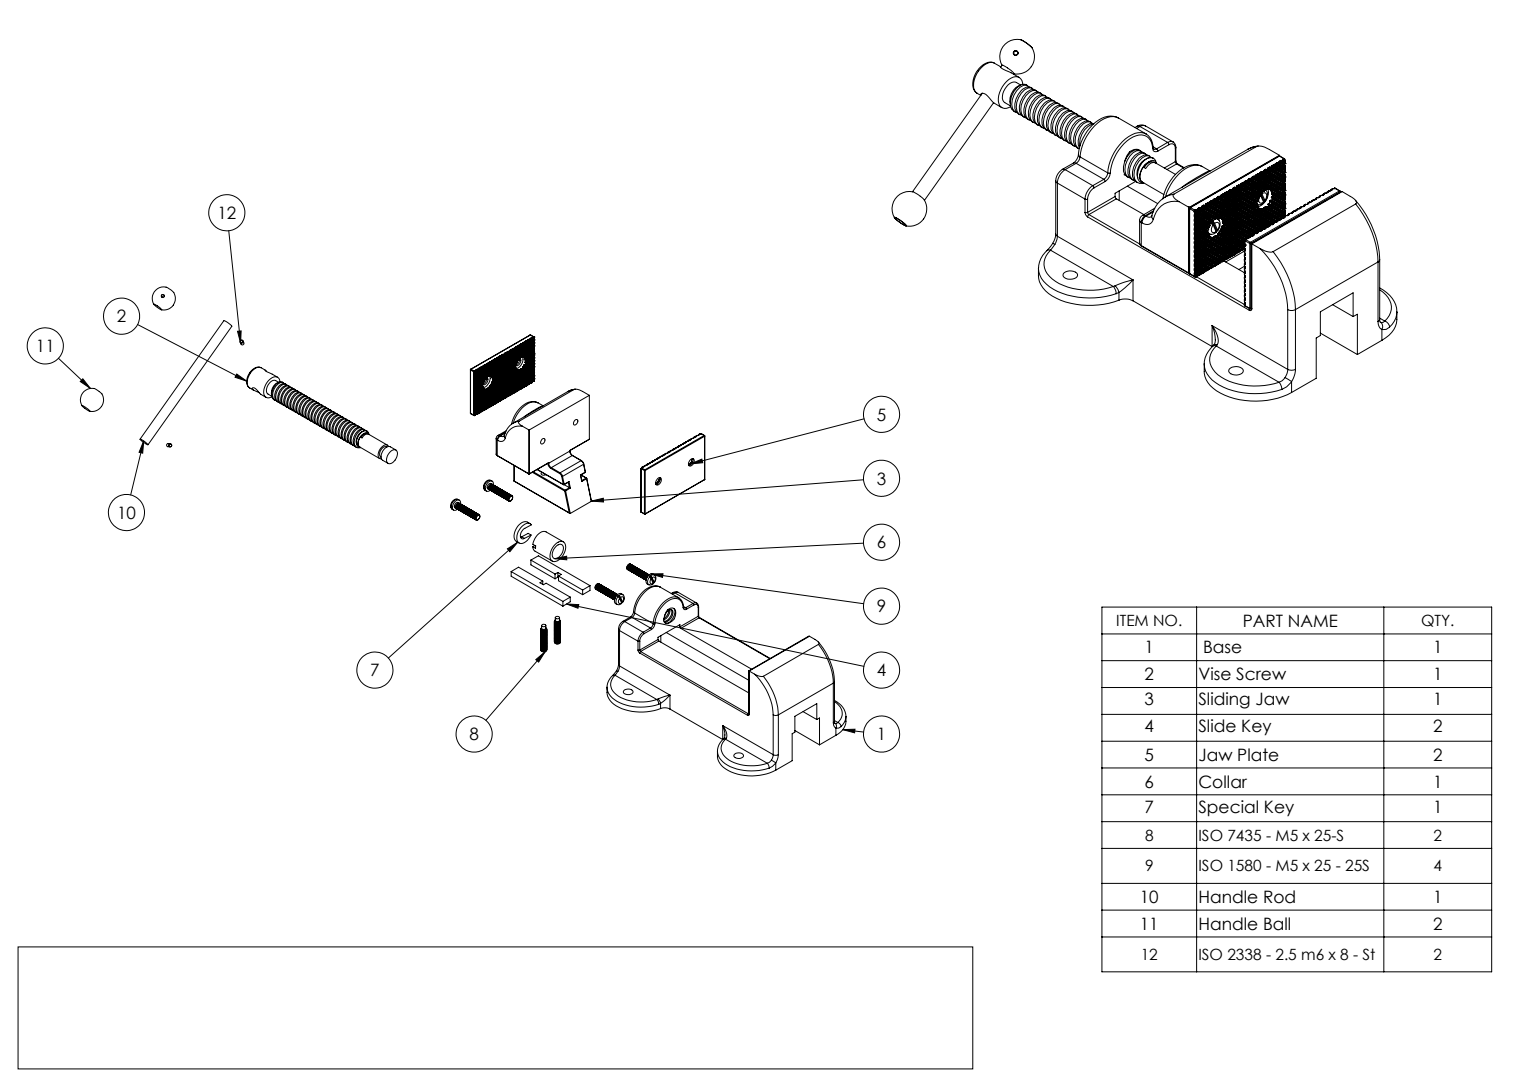
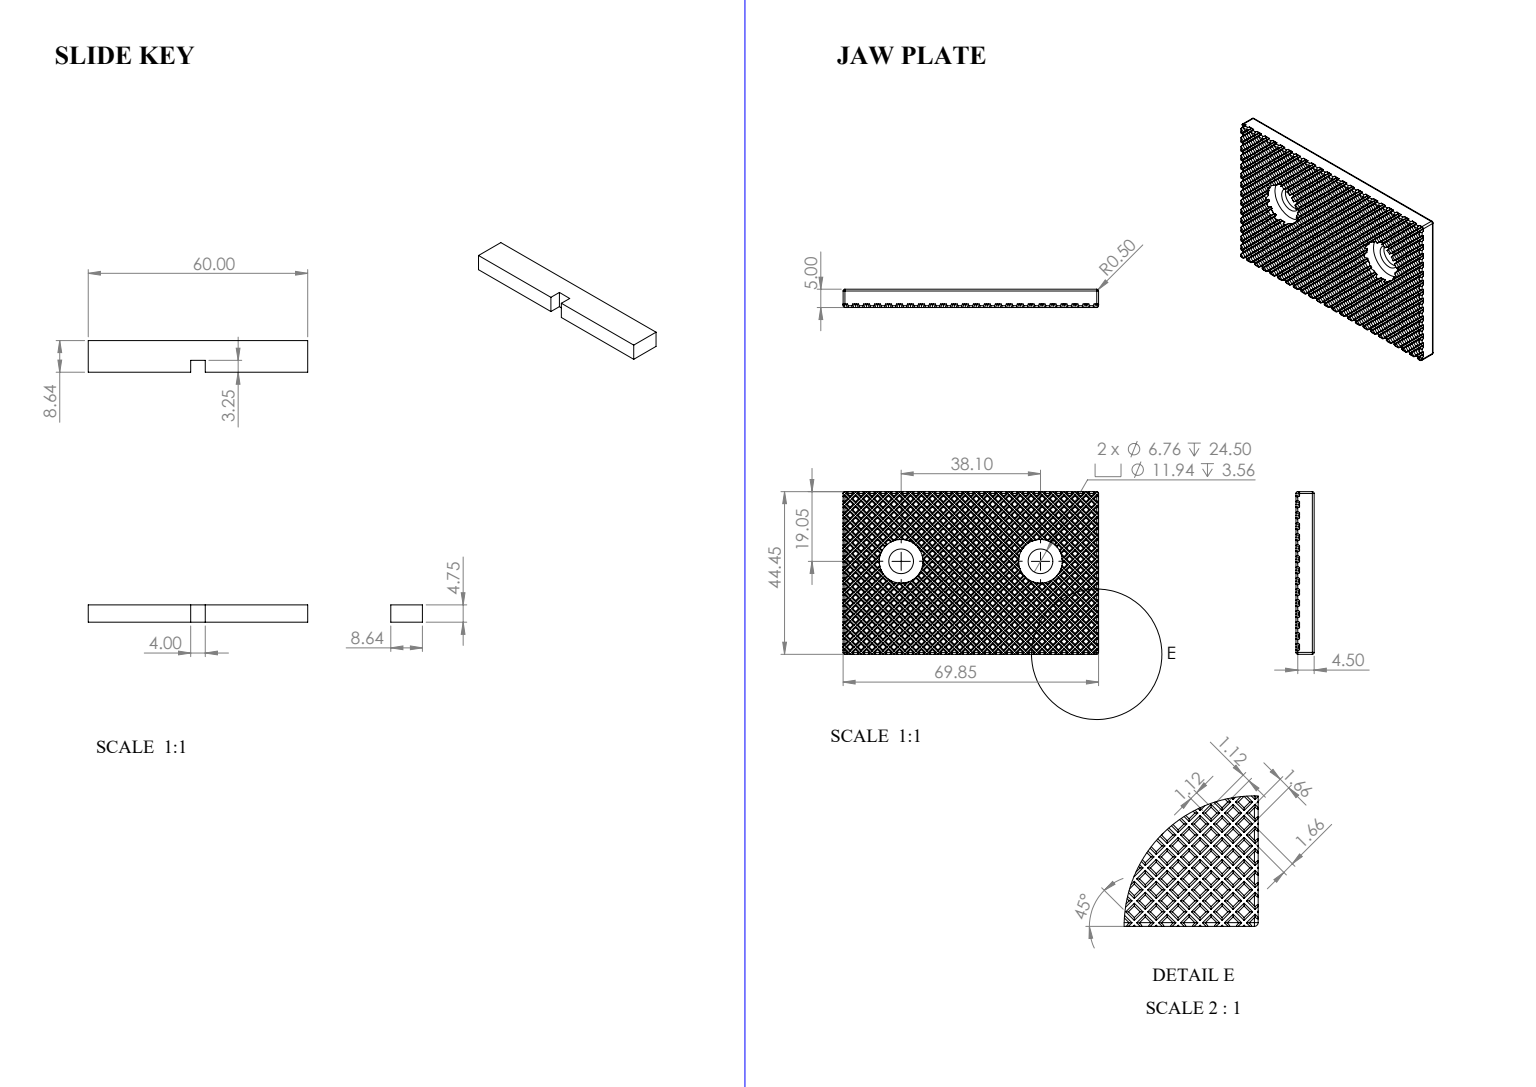
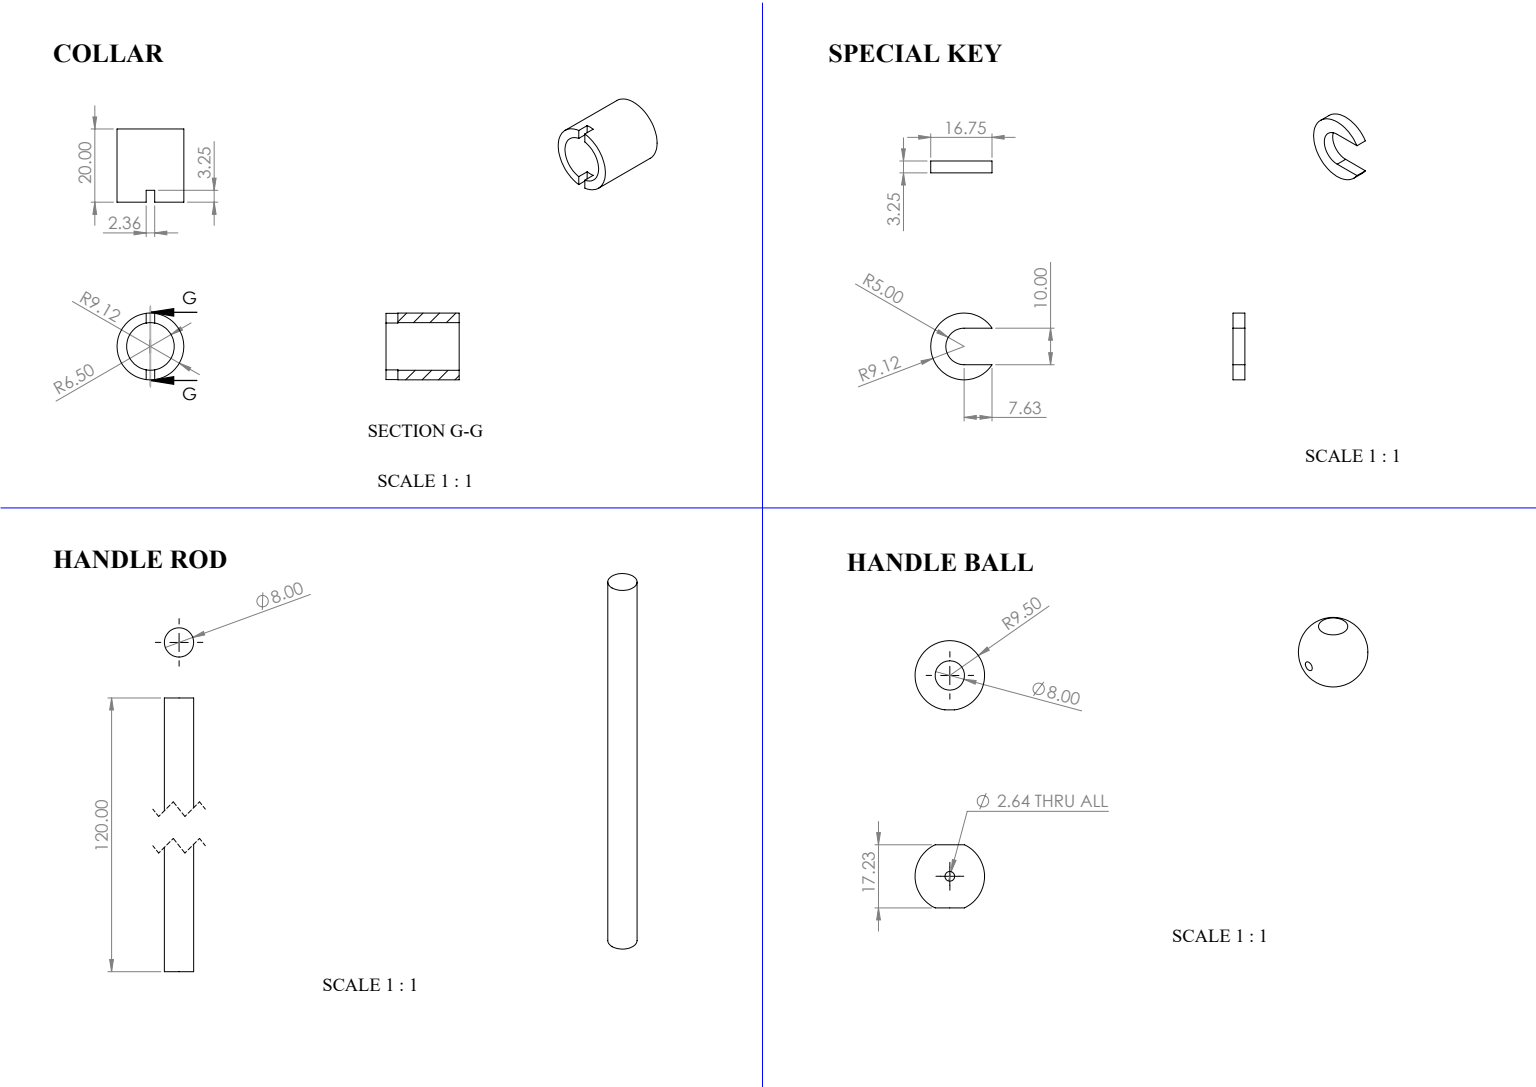
ISO-10303-21;
HEADER;
FILE_DESCRIPTION (('STEP AP214'),
    '1' );
FILE_NAME ('MAS-695',
    '2026-10-06T08:51:13',
    ( '' ),
    ( '' ),
    'SwSTEP 2.0',
    'SolidWorks 2021',
    '' );
FILE_SCHEMA (( 'AUTOMOTIVE_DESIGN' ));
ENDSEC;

DATA;
#1 = DIRECTION ( 'NONE',  ( 0.000000000000000000, 0.000000000000000000, 1.000000000000000000 ) ) ;
#2 = DIRECTION ( 'NONE',  ( 0.000000000000000000, 0.000000000000000000, -1.000000000000000000 ) ) ;
#3 = ADVANCED_FACE ( 'NONE', ( #5101 ), #71138, .F. ) ;
#4 = CARTESIAN_POINT ( 'NONE',  ( 156.1499999999997783, -49.14999999999999147, -40.92499999999998295 ) ) ;
#5 = VECTOR ( 'NONE', #78980, 1000.000000000000227 ) ;
#6 = CARTESIAN_POINT ( 'NONE',  ( 116.7245968585647660, -1.637169565754160949, 6.109999999999997655 ) ) ;
#7 = ORIENTED_EDGE ( 'NONE', *, *, #104399, .F. ) ;
#8 = EDGE_LOOP ( 'NONE', ( #83544, #1856, #131189, #37000 ) ) ;
#9 = FACE_OUTER_BOUND ( 'NONE', #81012, .T. ) ;
#10 = VECTOR ( 'NONE', #93764, 1000.000000000000000 ) ;
#11 = AXIS2_PLACEMENT_3D ( 'NONE', #21199, #109633, #54568 ) ;
#12 = VECTOR ( 'NONE', #112321, 1000.000000000000000 ) ;
#13 =( BOUNDED_CURVE ( )  B_SPLINE_CURVE ( 3, ( #128504, #27742, #103166, #38633 ),
 .UNSPECIFIED., .F., .T. ) 
 B_SPLINE_CURVE_WITH_KNOTS ( ( 4, 4 ),
 ( 5.143245962375963209, 6.645403452391246191 ),
 .UNSPECIFIED. ) 
 CURVE ( )  GEOMETRIC_REPRESENTATION_ITEM ( )  RATIONAL_B_SPLINE_CURVE ( ( 1.000000000000000000, 0.8206354192515237234, 0.8206354192515237234, 1.000000000000000000 ) ) 
 REPRESENTATION_ITEM ( '' )  );
#14 = COLOUR_RGB ( '', 0.08235294, 0.09019608, 0.10196078) ;
#15 = ORIENTED_EDGE ( 'NONE', *, *, #47014, .F. ) ;
#16 = VERTEX_POINT ( 'NONE', #58144 ) ;
#17 = CARTESIAN_POINT ( 'NONE',  ( 37.77126352523144703, 4.472830434245839371, 4.472830434245842035 ) ) ;
#18 = ORIENTED_EDGE ( 'NONE', *, *, #122540, .F. ) ;
#19 = CARTESIAN_POINT ( 'NONE',  ( -20.20710678118640402, -14.24070752338413826, 5.000000000000000000 ) ) ;
#20 = DIRECTION ( 'NONE',  ( -1.000000000000000000, -0.000000000000000000, -0.000000000000000000 ) ) ;
#21 = CYLINDRICAL_SURFACE ( 'NONE', #62371, 5.999999999999998224 ) ;
#22 = AXIS2_PLACEMENT_3D ( 'NONE', #116807, #105905, #95043 ) ;
#23 = CARTESIAN_POINT ( 'NONE',  ( 26.89126352523144092, -4.472830434245839371, -4.472830434245839371 ) ) ;
#24 = ORIENTED_EDGE ( 'NONE', *, *, #19090, .F. ) ;
#25 = LINE ( 'NONE', #44323, #82672 ) ;
#26 = ORIENTED_EDGE ( 'NONE', *, *, #3909, .F. ) ;
#27 = ORIENTED_EDGE ( 'NONE', *, *, #125600, .F. ) ;
#28 = AXIS2_PLACEMENT_3D ( 'NONE', #83260, #28167, #72429 ) ;
#29 = ORIENTED_EDGE ( 'NONE', *, *, #119403, .F. ) ;
#30 = VECTOR ( 'NONE', #87246, 1000.000000000000000 ) ;
#32 = PLANE ( 'NONE',  #68433 ) ;
#31 = VECTOR ( 'NONE', #125646, 1000.000000000000227 ) ;
#33 = CARTESIAN_POINT ( 'NONE',  ( -1.180000000000000604, 10.00000000000000178, 6.750000000000000888 ) ) ;
#34 = ORIENTED_EDGE ( 'NONE', *, *, #95665, .T. ) ;
#35 = FACE_OUTER_BOUND ( 'NONE', #136835, .T. ) ;
#36 = LINE ( 'NONE', #90690, #18133 ) ;
#37 = PLANE ( 'NONE',  #65195 ) ;
#38 = ADVANCED_FACE ( 'NONE', ( #115284 ), #3675, .F. ) ;
#39 = FACE_BOUND ( 'NONE', #50173, .T. ) ;
#40 = ORIENTED_EDGE ( 'NONE', *, *, #20313, .F. ) ;
#41 = CARTESIAN_POINT ( 'NONE',  ( -29.99451991528749417, 28.92564299267958816, 4.000000000000000000 ) ) ;
#42 = EDGE_CURVE ( 'NONE', #25059, #21205, #27594, .T. ) ;
#43 = EDGE_CURVE ( 'NONE', #65963, #18880, #92855, .T. ) ;
#44 = AXIS2_PLACEMENT_3D ( 'NONE', #3347, #93234, #125883 ) ;
#45 = DIRECTION ( 'NONE',  ( 0.3543493200069162685, -0.000000000000000000, -0.9351131265310288487 ) ) ;
#46 = DIRECTION ( 'NONE',  ( 1.000000000000000000, 0.000000000000000000, -0.000000000000000000 ) ) ;
#47 = ORIENTED_EDGE ( 'NONE', *, *, #35015, .F. ) ;
#48 = LINE ( 'NONE', #77678, #78225 ) ;
#49 = EDGE_LOOP ( 'NONE', ( #96646, #108093, #78224, #23588 ) ) ;
#50 = ORIENTED_EDGE ( 'NONE', *, *, #36159, .F. ) ;
#51 = LINE ( 'NONE', #32014, #142062 ) ;
#52 = ORIENTED_EDGE ( 'NONE', *, *, #60548, .T. ) ;
#53 = EDGE_CURVE ( 'NONE', #25081, #19559, #82032, .T. ) ;
#54 = EDGE_CURVE ( 'NONE', #25745, #125467, #104441, .T. ) ;
#55 = CARTESIAN_POINT ( 'NONE',  ( 47.30793019189811588, -6.109999999999998543, 1.637169565754158507 ) ) ;
#56 = ORIENTED_EDGE ( 'NONE', *, *, #91353, .F. ) ;
#57 = AXIS2_PLACEMENT_3D ( 'NONE', #43785, #22010, #66260 ) ;
#58 = DIRECTION ( 'NONE',  ( -0.7071067811865486830, -0.7071067811865464625, 0.000000000000000000 ) ) ;
#59 = CARTESIAN_POINT ( 'NONE',  ( -12.69999999999999929, -60.26999999999998892, -39.50000000000000000 ) ) ;
#60 = ADVANCED_FACE ( 'NONE', ( #80585 ), #50094, .F. ) ;
#61 = CARTESIAN_POINT ( 'NONE',  ( 68.99451991528748351, 28.92564299267986172, 4.000000000000000000 ) ) ;
#62 = EDGE_LOOP ( 'NONE', ( #94258, #115607, #50312, #53192 ) ) ;
#64 = CARTESIAN_POINT ( 'NONE',  ( 34.92499999999998295, -21.72500000000000142, 5.000000000000000000 ) ) ;
#63 = AXIS2_PLACEMENT_3D ( 'NONE', #104309, #85415, #117326 ) ;
#65 = EDGE_CURVE ( 'NONE', #58716, #118828, #49403, .T. ) ;
#66 = FILL_AREA_STYLE ('',( #56690 ) ) ;
#67 = DIRECTION ( 'NONE',  ( -0.7071067811865486830, -0.7071067811865464625, 0.000000000000000000 ) ) ;
#68 = DIRECTION ( 'NONE',  ( 0.000000000000000000, 0.000000000000000000, 1.000000000000000000 ) ) ;
#69 = LINE ( 'NONE', #66808, #128074 ) ;
#70 = DIRECTION ( 'NONE',  ( -0.7071067811865486830, -0.7071067811865464625, 0.000000000000000000 ) ) ;
#71 = ORIENTED_EDGE ( 'NONE', *, *, #64035, .T. ) ;
#72 = ORIENTED_EDGE ( 'NONE', *, *, #68229, .T. ) ;
#73 = VECTOR ( 'NONE', #82018, 1000.000000000000114 ) ;
#74 = EDGE_LOOP ( 'NONE', ( #63334, #111913, #607, #124092 ) ) ;
#75 = FACE_OUTER_BOUND ( 'NONE', #77019, .T. ) ;
#76 = EDGE_CURVE ( 'NONE', #54574, #78177, #14595, .T. ) ;
#77 = DIRECTION ( 'NONE',  ( 0.3543493200069162685, -0.000000000000000000, -0.9351131265310288487 ) ) ;
#78 = ORIENTED_EDGE ( 'NONE', *, *, #62615, .T. ) ;
#79 = ORIENTED_EDGE ( 'NONE', *, *, #43969, .T. ) ;
#80 = CARTESIAN_POINT ( 'NONE',  ( 166.6274442290528555, 26.96999999999994202, -32.76433874914447131 ) ) ;
#81 = DIRECTION ( 'NONE',  ( 1.000000000000000000, 0.000000000000000000, 0.000000000000000000 ) ) ;
#82 = CARTESIAN_POINT ( 'NONE',  ( 0.000000000000000000, 0.000000000000000000, 5.000000000000000000 ) ) ;
#83 = ORIENTED_EDGE ( 'NONE', *, *, #34651, .F. ) ;
#84 = DIRECTION ( 'NONE',  ( 0.3543493200069162685, -0.000000000000000000, -0.9351131265310288487 ) ) ;
#85 = EDGE_CURVE ( 'NONE', #114150, #6491, #116025, .T. ) ;
#86 = VECTOR ( 'NONE', #59606, 1000.000000000000000 ) ;
#87 = CARTESIAN_POINT ( 'NONE',  ( -9.489213562373095101, -27.52281430457062328, 5.000000000000000000 ) ) ;
#88 = CARTESIAN_POINT ( 'NONE',  ( 23.54623647476855552, -7.934999999999990727, 4.858786175617117713E-16 ) ) ;
#89 = CARTESIAN_POINT ( 'NONE',  ( 14.99999999999989519, -2.904428200921294057, -6.989807076074975534 ) ) ;
#90 = ORIENTED_EDGE ( 'NONE', *, *, #118546, .F. ) ;
#91 = CARTESIAN_POINT ( 'NONE',  ( 109.2870968585647944, 3.054999999999997939, 5.291415217122920289 ) ) ;
#92 = CARTESIAN_POINT ( 'NONE',  ( -19.83905809817562016, 22.22500000000000142, 10.71662732872346169 ) ) ;
#93 = EDGE_CURVE ( 'NONE', #95062, #84583, #91456, .T. ) ;
#94 = DIRECTION ( 'NONE',  ( -0.6830127018922180770, -0.6830127018922204085, -0.2588190451025213501 ) ) ;
#96 = ORIENTED_EDGE ( 'NONE', *, *, #90476, .F. ) ;
#95 = CARTESIAN_POINT ( 'NONE',  ( 20.99999999999985079, 12.25461709320622639, -10.07315571508692464 ) ) ;
#97 = DIRECTION ( 'NONE',  ( -0.000000000000000000, 0.000000000000000000, 1.000000000000000000 ) ) ;
#98 = ORIENTED_EDGE ( 'NONE', *, *, #70389, .T. ) ;
#99 = DIRECTION ( 'NONE',  ( -0.7071067811865486830, 0.7071067811865464625, 0.000000000000000000 ) ) ;
#100 = VECTOR ( 'NONE', #124280, 1000.000000000000000 ) ;
#101 = CARTESIAN_POINT ( 'NONE',  ( 3.489213562373097322, -27.52281430457057709, 5.000000000000000000 ) ) ;
#102 = DIRECTION ( 'NONE',  ( 1.201410254241279878E-16, -1.000000000000000000, 8.881784197001252323E-16 ) ) ;
#103 = ORIENTED_EDGE ( 'NONE', *, *, #12795, .T. ) ;
#104 = ADVANCED_FACE ( 'NONE', ( #137820 ), #15976, .T. ) ;
#105 = VECTOR ( 'NONE', #70002, 1000.000000000000227 ) ;
#106 = EDGE_CURVE ( 'NONE', #132598, #105272, #69721, .T. ) ;
#107 = LINE ( 'NONE', #77033, #97406 ) ;
#108 = DIRECTION ( 'NONE',  ( -1.000000000000000000, -1.224606353822377258E-16, -0.000000000000000000 ) ) ;
#109 = ORIENTED_EDGE ( 'NONE', *, *, #66738, .T. ) ;
#110 = AXIS2_PLACEMENT_3D ( 'NONE', #91463, #135678, #48666 ) ;
#111 = VECTOR ( 'NONE', #117132, 999.9999999999998863 ) ;
#112 = MECHANICAL_DESIGN_GEOMETRIC_PRESENTATION_REPRESENTATION (  '', ( #37206 ), #67225 ) ;
#113 = DIRECTION ( 'NONE',  ( -0.7071067811865487940, 0.7071067811865463515, -0.000000000000000000 ) ) ;
#114 = VECTOR ( 'NONE', #50874, 1000.000000000000000 ) ;
#116 = EDGE_CURVE ( 'NONE', #31169, #8752, #138521, .T. ) ;
#115 = LINE ( 'NONE', #86474, #33098 ) ;
#118 = EDGE_LOOP ( 'NONE', ( #114372, #70505, #8992, #113022 ) ) ;
#117 = VECTOR ( 'NONE', #30072, 1000.000000000000000 ) ;
#119 = LINE ( 'NONE', #77741, #60053 ) ;
#121 = VERTEX_POINT ( 'NONE', #68996 ) ;
#120 = DIRECTION ( 'NONE',  ( 0.6830127018922180770, -0.6830127018922204085, -0.2588190451025213501 ) ) ;
#122 = ORIENTED_EDGE ( 'NONE', *, *, #95989, .T. ) ;
#123 = CARTESIAN_POINT ( 'NONE',  ( -13.10742158956126424, 3.736470153597435395, 4.109745541549492565 ) ) ;
#124 = AXIS2_PLACEMENT_3D ( 'NONE', #74766, #9441, #75464 ) ;
#125 = ORIENTED_EDGE ( 'NONE', *, *, #121353, .T. ) ;
#126 = CARTESIAN_POINT ( 'NONE',  ( 25.49999999999982592, -19.53360074219753884, 5.000000000000000000 ) ) ;
#127 = DIRECTION ( 'NONE',  ( -0.7071067811865486830, -0.7071067811865464625, 0.000000000000000000 ) ) ;
#128 = DIRECTION ( 'NONE',  ( -0.7071067811865486830, 0.7071067811865464625, 0.000000000000000000 ) ) ;
#129 = ORIENTED_EDGE ( 'NONE', *, *, #131844, .F. ) ;
#130 = EDGE_CURVE ( 'NONE', #6161, #1058, #58874, .T. ) ;
#131 = LINE ( 'NONE', #142993, #129973 ) ;
#132 = LINE ( 'NONE', #67611, #18945 ) ;
#133 = LINE ( 'NONE', #13167, #47104 ) ;
#134 = AXIS2_PLACEMENT_3D ( 'NONE', #6194, #104832, #5501 ) ;
#135 = LINE ( 'NONE', #42284, #50624 ) ;
#136 = CARTESIAN_POINT ( 'NONE',  ( 29.66209685856477307, -5.291415217122919401, 3.054999999999998384 ) ) ;
#137 = CARTESIAN_POINT ( 'NONE',  ( 2.999999999999988898, 2.966399257802230682, 5.000000000000000000 ) ) ;
#138 = VECTOR ( 'NONE', #55015, 1000.000000000000000 ) ;
#139 = ORIENTED_EDGE ( 'NONE', *, *, #36771, .T. ) ;
#140 = ORIENTED_EDGE ( 'NONE', *, *, #3276, .F. ) ;
#141 =( NAMED_UNIT ( * ) SI_UNIT ( $, .STERADIAN. ) SOLID_ANGLE_UNIT ( ) );
#142 = VECTOR ( 'NONE', #39114, 999.9999999999998863 ) ;
#143 = ORIENTED_EDGE ( 'NONE', *, *, #47317, .T. ) ;
#144 = VECTOR ( 'NONE', #74034, 999.9999999999998863 ) ;
#145 = EDGE_LOOP ( 'NONE', ( #119724, #61454, #57894, #85195 ) ) ;
#146 = CARTESIAN_POINT ( 'NONE',  ( -5.708222910169487463, -15.74070752338411694, 19.73771281079096340 ) ) ;
#147 = DIRECTION ( 'NONE',  ( -0.7071067811865486830, -0.7071067811865464625, 0.000000000000000000 ) ) ;
#148 = VECTOR ( 'NONE', #138557, 1000.000000000000000 ) ;
#149 = ORIENTED_EDGE ( 'NONE', *, *, #38243, .F. ) ;
#150 = DIRECTION ( 'NONE',  ( 0.000000000000000000, -0.9647414015272155474, 0.2631995976047525887 ) ) ;
#151 = FACE_OUTER_BOUND ( 'NONE', #122556, .T. ) ;
#152 = CARTESIAN_POINT ( 'NONE',  ( -7.499999999999947597, -4.796895815301026822, -3.611700055028700174 ) ) ;
#153 = ADVANCED_FACE ( 'NONE', ( #103035 ), #103710, .F. ) ;
#154 = CARTESIAN_POINT ( 'NONE',  ( -12.18398860626900060, 28.73617430169795739, 5.000000000000000000 ) ) ;
#155 = CARTESIAN_POINT ( 'NONE',  ( 124.5420968585647756, 5.291415217122923842, -3.054999999999996163 ) ) ;
#156 = AXIS2_PLACEMENT_3D ( 'NONE', #125719, #134450, #3870 ) ;
#157 = ORIENTED_EDGE ( 'NONE', *, *, #128606, .T. ) ;
#158 = CARTESIAN_POINT ( 'NONE',  ( 5.207106781186502609, -17.24070752338410983, 5.000000000000000000 ) ) ;
#159 = DIRECTION ( 'NONE',  ( 0.7071067811865487940, -0.7071067811865463515, 0.000000000000000000 ) ) ;
#160 = FACE_OUTER_BOUND ( 'NONE', #79460, .T. ) ;
#161 =( NAMED_UNIT ( * ) PLANE_ANGLE_UNIT ( ) SI_UNIT ( $, .RADIAN. ) );
#162 = PLANE ( 'NONE',  #130794 ) ;
#163 = CARTESIAN_POINT ( 'NONE',  ( 19.49999999999985789, 8.319652575858395238, -8.582050562765779489 ) ) ;
#164 = FACE_OUTER_BOUND ( 'NONE', #130185, .T. ) ;
#165 = CARTESIAN_POINT ( 'NONE',  ( 54.62086038379622721, -6.884901960086286188, 3.974999999999997424 ) ) ;
#166 = DIRECTION ( 'NONE',  ( 0.6830127018922181881, 0.6830127018922202975, -0.2588190451025214056 ) ) ;
#167 = EDGE_CURVE ( 'NONE', #60255, #130315, #34540, .T. ) ;
#168 = DIRECTION ( 'NONE',  ( 0.7071067811865486830, -0.7071067811865464625, -0.000000000000000000 ) ) ;
#169 = AXIS2_PLACEMENT_3D ( 'NONE', #60485, #124990, #72084 ) ;
#170 = ORIENTED_EDGE ( 'NONE', *, *, #86072, .F. ) ;
#171 = ORIENTED_EDGE ( 'NONE', *, *, #96108, .T. ) ;
#172 = CARTESIAN_POINT ( 'NONE',  ( 48.25000000000000000, -9.735942053221458872E-16, 7.950000000000000178 ) ) ;
#173 = DIRECTION ( 'NONE',  ( -0.7071067811865486830, -0.7071067811865464625, 0.000000000000000000 ) ) ;
#174 = CARTESIAN_POINT ( 'NONE',  ( 53.99451991528749062, 28.92564299267975869, 4.000000000000000000 ) ) ;
#175 = ORIENTED_EDGE ( 'NONE', *, *, #80806, .F. ) ;
#176 = DIRECTION ( 'NONE',  ( 0.7071067811865487940, 0.7071067811865463515, 0.000000000000000000 ) ) ;
#177 = EDGE_CURVE ( 'NONE', #92630, #88659, #70457, .T. ) ;
#178 = LINE ( 'NONE', #43032, #32998 ) ;
#179 = EDGE_CURVE ( 'NONE', #63680, #108628, #141365, .T. ) ;
#180 = CARTESIAN_POINT ( 'NONE',  ( 41.27126352523144703, 4.472830434245839371, 4.472830434245842035 ) ) ;
#181 = ORIENTED_EDGE ( 'NONE', *, *, #134281, .T. ) ;
#182 = CARTESIAN_POINT ( 'NONE',  ( 0.1600000000000011136, 3.289720434613005118, -7.220939306079887210 ) ) ;
#183 = ORIENTED_EDGE ( 'NONE', *, *, #91628, .T. ) ;
#184 = ORIENTED_EDGE ( 'NONE', *, *, #140711, .F. ) ;
#185 = VECTOR ( 'NONE', #101958, 1000.000000000000227 ) ;
#186 = DIRECTION ( 'NONE',  ( 0.9961946980917455452, 0.000000000000000000, -0.08715574274765836016 ) ) ;
#187 = DIRECTION ( 'NONE',  ( 0.6830127018922181881, 0.6830127018922202975, -0.2588190451025214056 ) ) ;
#188 = CARTESIAN_POINT ( 'NONE',  ( -12.29974487139158512, -27.71228299555214747, 4.000000000000000000 ) ) ;
#189 = PLANE ( 'NONE',  #18575 ) ;
#190 = EDGE_LOOP ( 'NONE', ( #15272, #100026, #80901, #142923 ) ) ;
#191 = EDGE_CURVE ( 'NONE', #72974, #90074, #61695, .T. ) ;
#192 = DIRECTION ( 'NONE',  ( -0.7071067811865487940, 0.7071067811865463515, 0.000000000000000000 ) ) ;
#193 = ORIENTED_EDGE ( 'NONE', *, *, #9062, .T. ) ;
#194 = CARTESIAN_POINT ( 'NONE',  ( 82.25043019189810423, 3.055000000000002824, -5.291415217122919401 ) ) ;
#195 = FACE_OUTER_BOUND ( 'NONE', #108561, .T. ) ;
#196 =( LENGTH_UNIT ( ) NAMED_UNIT ( * ) SI_UNIT ( .MILLI., .METRE. ) );
#197 = CARTESIAN_POINT ( 'NONE',  ( -34.92500000000001137, 6.856123077392376253, 4.000000000000000000 ) ) ;
#198 = PLANE ( 'NONE',  #64849 ) ;
#199 = VECTOR ( 'NONE', #98975, 1000.000000000000000 ) ;
#200 = DIRECTION ( 'NONE',  ( 1.000000000000000000, 0.000000000000000000, 0.000000000000000000 ) ) ;
#201 = ORIENTED_EDGE ( 'NONE', *, *, #80508, .F. ) ;
#202 = DIRECTION ( 'NONE',  ( -0.7071067811865486830, -0.7071067811865464625, -0.000000000000000000 ) ) ;
#203 = CARTESIAN_POINT ( 'NONE',  ( 53.43293019189810167, 1.637169565754156508, 6.110000000000000320 ) ) ;
#204 = FACE_OUTER_BOUND ( 'NONE', #73708, .T. ) ;
#205 = DIRECTION ( 'NONE',  ( 0.7071067811865486830, -0.7071067811865464625, -0.000000000000000000 ) ) ;
#206 = DIRECTION ( 'NONE',  ( -0.000000000000000000, -0.000000000000000000, 1.000000000000000000 ) ) ;
#207 = ORIENTED_EDGE ( 'NONE', *, *, #61881, .T. ) ;
#208 = EDGE_LOOP ( 'NONE', ( #82343, #5888, #63190, #69675 ) ) ;
#209 = FACE_OUTER_BOUND ( 'NONE', #9634, .T. ) ;
#210 = AXIS2_PLACEMENT_3D ( 'NONE', #18854, #51517, #105848 ) ;
#211 = ORIENTED_EDGE ( 'NONE', *, *, #117503, .T. ) ;
#212 = VECTOR ( 'NONE', #88205, 1000.000000000000000 ) ;
#213 = AXIS2_PLACEMENT_3D ( 'NONE', #103469, #123843, #48393 ) ;
#214 = CARTESIAN_POINT ( 'NONE',  ( 0.000000000000000000, 0.000000000000000000, 5.000000000000000000 ) ) ;
#215 = ORIENTED_EDGE ( 'NONE', *, *, #26545, .F. ) ;
#216 = CARTESIAN_POINT ( 'NONE',  ( 12.48921356237309155, -27.52281430457064104, 5.000000000000000000 ) ) ;
#217 = CARTESIAN_POINT ( 'NONE',  ( 29.99999999999979039, -10.77435723561692704, -9.972017380717296930 ) ) ;
#218 = VECTOR ( 'NONE', #139975, 1000.000000000000000 ) ;
#219 = VECTOR ( 'NONE', #138745, 1000.000000000000000 ) ;
#220 = AXIS2_PLACEMENT_3D ( 'NONE', #21758, #55108, #75432 ) ;
#221 = AXIS2_PLACEMENT_3D ( 'NONE', #111679, #101498, #113810 ) ;
#222 = EDGE_CURVE ( 'NONE', #139983, #86102, #20281, .T. ) ;
#223 = AXIS2_PLACEMENT_3D ( 'NONE', #89988, #15261, #133521 ) ;
#224 = FACE_OUTER_BOUND ( 'NONE', #124706, .T. ) ;
#225 = FACE_BOUND ( 'NONE', #102384, .T. ) ;
#226 = ADVANCED_FACE ( 'NONE', ( #51523 ), #94983, .F. ) ;
#227 = CARTESIAN_POINT ( 'NONE',  ( 28.49999999999980460, 16.77039438581781639, 0.4657186855307072215 ) ) ;
#228 = LINE ( 'NONE', #88730, #91900 ) ;
#230 = DIRECTION ( 'NONE',  ( -0.7071067811865486830, -0.7071067811865464625, 0.000000000000000000 ) ) ;
#229 = AXIS2_PLACEMENT_3D ( 'NONE', #59966, #127341, #70166 ) ;
#232 = ORIENTED_EDGE ( 'NONE', *, *, #94046, .F. ) ;
#231 = CARTESIAN_POINT ( 'NONE',  ( 5.343289998337836799, 3.759292476615681888, 13.27625715073266832 ) ) ;
#233 = DIRECTION ( 'NONE',  ( 0.7071067811865487940, -0.7071067811865463515, 0.000000000000000000 ) ) ;
#234 = EDGE_LOOP ( 'NONE', ( #55561, #105143, #26118, #111519 ) ) ;
#235 = EDGE_CURVE ( 'NONE', #55527, #138159, #86292, .T. ) ;
#236 = EDGE_CURVE ( 'NONE', #105061, #6978, #28339, .T. ) ;
#237 = VERTEX_POINT ( 'NONE', #52898 ) ;
#238 = CARTESIAN_POINT ( 'NONE',  ( 79.97459685856478018, 1.637169565754164280, -6.109999999999996767 ) ) ;
#239 = ORIENTED_EDGE ( 'NONE', *, *, #100908, .T. ) ;
#240 = CARTESIAN_POINT ( 'NONE',  ( -34.92500000000001137, -22.22500000000000142, 4.000000000000000000 ) ) ;
#241 = EDGE_CURVE ( 'NONE', #93680, #60629, #40644, .T. ) ;
#242 = VECTOR ( 'NONE', #139566, 1000.000000000000000 ) ;
#243 = CARTESIAN_POINT ( 'NONE',  ( -14.99999999999990230, 11.58746187583913390, 4.000000000000000000 ) ) ;
#244 = B_SPLINE_CURVE_WITH_KNOTS ( 'NONE', 3,
 ( #116047, #19597, #116769, #42097, #141380, #17451, #127667, #74728, #105869, #52917, #50814, #86307 ),
 .UNSPECIFIED., .F., .F.,
 ( 4, 2, 2, 2, 2, 4 ),
 ( 9.813815432834144085E-18, 0.001837441947543535809, 0.003674883895087062077, 0.004593604868858823694, 0.005512325842630587044, 0.007349767790174136298 ),
 .UNSPECIFIED. ) ;
#245 = EDGE_CURVE ( 'NONE', #60766, #87872, #129054, .T. ) ;
#246 = ORIENTED_EDGE ( 'NONE', *, *, #38962, .T. ) ;
#247 = CARTESIAN_POINT ( 'NONE',  ( -57.29974487139158157, -27.71228299555246011, 4.000000000000000000 ) ) ;
#248 = ADVANCED_FACE ( 'NONE', ( #84846 ), #37182, .F. ) ;
#249 = VECTOR ( 'NONE', #124185, 999.9999999999998863 ) ;
#250 = LINE ( 'NONE', #99570, #21719 ) ;
#251 = FACE_OUTER_BOUND ( 'NONE', #30396, .T. ) ;
#252 = EDGE_CURVE ( 'NONE', #89926, #37388, #72601, .T. ) ;
#253 = AXIS2_PLACEMENT_3D ( 'NONE', #31106, #7884, #115919 ) ;
#254 = CARTESIAN_POINT ( 'NONE',  ( 0.000000000000000000, 0.000000000000000000, 5.000000000000000000 ) ) ;
#255 = DIRECTION ( 'NONE',  ( -0.3543493200069163240, 0.000000000000000000, 0.9351131265310288487 ) ) ;
#256 = DIRECTION ( 'NONE',  ( 0.7071067811865487940, -0.7071067811865463515, 0.000000000000000000 ) ) ;
#257 = AXIS2_PLACEMENT_3D ( 'NONE', #43444, #11484, #76815 ) ;
#258 = CARTESIAN_POINT ( 'NONE',  ( -11.51078643762690490, -27.52281430457047406, 5.000000000000000000 ) ) ;
#259 = DIRECTION ( 'NONE',  ( 0.000000000000000000, -1.000000000000000000, 0.000000000000000000 ) ) ;
#260 = ORIENTED_EDGE ( 'NONE', *, *, #110078, .F. ) ;
#261 = PRESENTATION_STYLE_ASSIGNMENT (( #47937 ) ) ;
#262 = ORIENTED_EDGE ( 'NONE', *, *, #76274, .T. ) ;
#263 = VECTOR ( 'NONE', #104295, 1000.000000000000000 ) ;
#264 = CARTESIAN_POINT ( 'NONE',  ( 14.20710678118644665, 6.759292476615645029, 5.000000000000000000 ) ) ;
#265 = EDGE_CURVE ( 'NONE', #60839, #128811, #85538, .T. ) ;
#266 = ORIENTED_EDGE ( 'NONE', *, *, #113885, .F. ) ;
#267 = ORIENTED_EDGE ( 'NONE', *, *, #56927, .F. ) ;
#268 = VECTOR ( 'NONE', #71889, 999.9999999999998863 ) ;
#269 = CARTESIAN_POINT ( 'NONE',  ( 28.58376352523143993, -6.110000000000001208, -3.741295971395164515E-16 ) ) ;
#270 = VERTEX_POINT ( 'NONE', #52214 ) ;
#271 = ADVANCED_FACE ( 'NONE', ( #128367 ), #102071, .T. ) ;
#272 = CARTESIAN_POINT ( 'NONE',  ( 18.32816939922340183, -6.740707523384209310, 4.000000000000000000 ) ) ;
#273 = AXIS2_PLACEMENT_3D ( 'NONE', #107756, #108445, #21491 ) ;
#274 = CARTESIAN_POINT ( 'NONE',  ( -0.2245968585647807325, -2.126176841940958351, -7.934999999999989839 ) ) ;
#275 = CARTESIAN_POINT ( 'NONE',  ( -23.51078643762690490, -27.52281430457038880, 5.000000000000000000 ) ) ;
#276 = ORIENTED_EDGE ( 'NONE', *, *, #16957, .T. ) ;
#277 = LINE ( 'NONE', #122073, #61918 ) ;
#278 = ORIENTED_EDGE ( 'NONE', *, *, #76259, .F. ) ;
#279 = DIRECTION ( 'NONE',  ( -0.000000000000000000, -0.3543493200069152693, 0.9351131265310292928 ) ) ;
#280 = DIRECTION ( 'NONE',  ( -0.6830127018922180770, -0.6830127018922204085, -0.2588190451025213501 ) ) ;
#282 = EDGE_LOOP ( 'NONE', ( #75330, #107556, #58149, #92149 ) ) ;
#281 = DIRECTION ( 'NONE',  ( 0.7071067811865486830, -0.7071067811865464625, -0.000000000000000000 ) ) ;
#283 = VECTOR ( 'NONE', #27809, 1000.000000000000000 ) ;
#284 = ORIENTED_EDGE ( 'NONE', *, *, #109477, .T. ) ;
#285 = FACE_OUTER_BOUND ( 'NONE', #1360, .T. ) ;
#286 = LINE ( 'NONE', #34381, #116352 ) ;
#287 = CARTESIAN_POINT ( 'NONE',  ( 1.171830600776462061, -20.24070752338407786, 4.000000000000000000 ) ) ;
#288 = VERTEX_POINT ( 'NONE', #119584 ) ;
#289 = CARTESIAN_POINT ( 'NONE',  ( -72.48921356237309510, -27.52281430457106026, 5.000000000000000000 ) ) ;
#290 = DIRECTION ( 'NONE',  ( -0.6830127018922180770, -0.6830127018922204085, -0.2588190451025213501 ) ) ;
#291 = ORIENTED_EDGE ( 'NONE', *, *, #84770, .T. ) ;
#292 = VECTOR ( 'NONE', #30348, 1000.000000000000000 ) ;
#293 = EDGE_CURVE ( 'NONE', #72640, #57817, #29041, .T. ) ;
#294 = LINE ( 'NONE', #88788, #58847 ) ;
#295 = LINE ( 'NONE', #101775, #132017 ) ;
#296 = CARTESIAN_POINT ( 'NONE',  ( -15.48921356237309510, -27.52281430457066236, 5.000000000000000000 ) ) ;
#297 = AXIS2_PLACEMENT_3D ( 'NONE', #93929, #83070, #52567 ) ;
#298 = DIRECTION ( 'NONE',  ( -1.000000000000000000, -1.224606353822377258E-16, -0.000000000000000000 ) ) ;
#299 = EDGE_CURVE ( 'NONE', #18521, #55587, #117446, .T. ) ;
#300 = DIRECTION ( 'NONE',  ( -1.000000000000000000, -1.224606353822377258E-16, -0.000000000000000000 ) ) ;
#301 = FACE_OUTER_BOUND ( 'NONE', #7948, .T. ) ;
#302 = LINE ( 'NONE', #112664, #34486 ) ;
#303 = ORIENTED_EDGE ( 'NONE', *, *, #124962, .T. ) ;
#304 = CARTESIAN_POINT ( 'NONE',  ( 97.49586038379624142, -3.974999999999998312, -6.884901960086286188 ) ) ;
#305 = VERTEX_POINT ( 'NONE', #7974 ) ;
#306 = VECTOR ( 'NONE', #44663, 1000.000000000000114 ) ;
#307 = SURFACE_SIDE_STYLE ('',( #35140 ) ) ;
#308 = CARTESIAN_POINT ( 'NONE',  ( 0.000000000000000000, 0.000000000000000000, 7.950000000000000178 ) ) ;
#309 = EDGE_CURVE ( 'NONE', #55336, #42777, #64521, .T. ) ;
#310 = LINE ( 'NONE', #120669, #138798 ) ;
#311 = ORIENTED_EDGE ( 'NONE', *, *, #103224, .T. ) ;
#312 = PLANE ( 'NONE',  #122563 ) ;
#313 = DIRECTION ( 'NONE',  ( -0.3543493200069162685, -0.000000000000000000, -0.9351131265310288487 ) ) ;
#314 = CARTESIAN_POINT ( 'NONE',  ( -21.70710678118638981, 11.25929247661560773, 5.000000000000000000 ) ) ;
#315 = ORIENTED_EDGE ( 'NONE', *, *, #1789, .F. ) ;
#316 = EDGE_CURVE ( 'NONE', #33411, #102047, #58129, .T. ) ;
#317 = LINE ( 'NONE', #143165, #97408 ) ;
#318 = LINE ( 'NONE', #11922, #100246 ) ;
#319 = CARTESIAN_POINT ( 'NONE',  ( 12.48921356237309155, -27.52281430457064104, 5.000000000000000000 ) ) ;
#320 = AXIS2_PLACEMENT_3D ( 'NONE', #30283, #118710, #19405 ) ;
#321 = DIRECTION ( 'NONE',  ( 0.7071067811865486830, -0.7071067811865464625, -0.000000000000000000 ) ) ;
#322 = CARTESIAN_POINT ( 'NONE',  ( 56.34959685856478018, 6.109999999999997655, 1.637169565754163836 ) ) ;
#323 = CARTESIAN_POINT ( 'NONE',  ( 60.48921356237309510, -27.52281430457097500, 5.000000000000000000 ) ) ;
#324 = VECTOR ( 'NONE', #96544, 1000.000000000000000 ) ;
#325 =( BOUNDED_CURVE ( )  B_SPLINE_CURVE ( 3, ( #134781, #78969, #34023, #14395 ),
 .UNSPECIFIED., .F., .T. ) 
 B_SPLINE_CURVE_WITH_KNOTS ( ( 4, 4 ),
 ( 4.350170835173023498, 4.500739107949261353 ),
 .UNSPECIFIED. ) 
 CURVE ( )  GEOMETRIC_REPRESENTATION_ITEM ( )  RATIONAL_B_SPLINE_CURVE ( ( 1.000000000000000000, 0.9981116584018945304, 0.9981116584018945304, 1.000000000000000000 ) ) 
 REPRESENTATION_ITEM ( '' )  );
#326 = AXIS2_PLACEMENT_3D ( 'NONE', #113465, #122938, #69282 ) ;
#327 = DIRECTION ( 'NONE',  ( -1.000000000000000000, -2.891205793294679312E-16, 0.000000000000000000 ) ) ;
#328 = CARTESIAN_POINT ( 'NONE',  ( 32.30836038379622721, 7.949999999999996625, 2.130196079827431088 ) ) ;
#329 = CARTESIAN_POINT ( 'NONE',  ( 83.68750000000000000, -5.819803920172573974, 5.819803920172573086 ) ) ;
#330 = VERTEX_POINT ( 'NONE', #9384 ) ;
#331 =( LENGTH_UNIT ( ) NAMED_UNIT ( * ) SI_UNIT ( .MILLI., .METRE. ) );
#332 = VERTEX_POINT ( 'NONE', #53661 ) ;
#333 = VECTOR ( 'NONE', #70121, 1000.000000000000000 ) ;
#334 = VECTOR ( 'NONE', #77445, 1000.000000000000000 ) ;
#335 = CIRCLE ( 'NONE', #118423, 2.256103126841972895 ) ;
#336 = CARTESIAN_POINT ( 'NONE',  ( 8.816011393731004731, 28.73617430169781173, 5.000000000000000000 ) ) ;
#338 = PLANE ( 'NONE',  #138048 ) ;
#337 = AXIS2_PLACEMENT_3D ( 'NONE', #92579, #128791, #104900 ) ;
#339 = AXIS2_PLACEMENT_3D ( 'NONE', #38488, #104434, #126890 ) ;
#340 = FACE_OUTER_BOUND ( 'NONE', #82107, .T. ) ;
#341 = PLANE ( 'NONE',  #25712 ) ;
#342 = PLANE ( 'NONE',  #141146 ) ;
#343 = EDGE_CURVE ( 'NONE', #92701, #118319, #97869, .T. ) ;
#344 = CARTESIAN_POINT ( 'NONE',  ( -34.42500000000001137, 13.54139925780187603, 5.000000000000000000 ) ) ;
#345 = CARTESIAN_POINT ( 'NONE',  ( -34.42500000000001137, 0.000000000000000000, 4.500000000000000888 ) ) ;
#346 = EDGE_CURVE ( 'NONE', #132444, #99209, #109450, .T. ) ;
#347 = ORIENTED_EDGE ( 'NONE', *, *, #6469, .T. ) ;
#348 = ORIENTED_EDGE ( 'NONE', *, *, #75130, .F. ) ;
#349 = FACE_OUTER_BOUND ( 'NONE', #74753, .T. ) ;
#350 = FACE_OUTER_BOUND ( 'NONE', #24729, .T. ) ;
#351 = VECTOR ( 'NONE', #98125, 1000.000000000000000 ) ;
#352 = CARTESIAN_POINT ( 'NONE',  ( -24.18398860626899705, 28.73617430169804265, 5.000000000000000000 ) ) ;
#353 = DIRECTION ( 'NONE',  ( -0.6830127018922181881, 0.6830127018922202975, -0.2588190451025214056 ) ) ;
#354 = CARTESIAN_POINT ( 'NONE',  ( 81.45419371712955581, 6.884901960086283523, 3.975000000000002753 ) ) ;
#355 = CARTESIAN_POINT ( 'NONE',  ( -11.29289321881337571, 17.25929247661553489, 5.000000000000000000 ) ) ;
#356 = ADVANCED_FACE ( 'NONE', ( #123207 ), #110146, .T. ) ;
#357 = DIRECTION ( 'NONE',  ( -1.000000000000000000, -1.224606353822377258E-16, -0.000000000000000000 ) ) ;
#358 = VERTEX_POINT ( 'NONE', #56560 ) ;
#359 = CARTESIAN_POINT ( 'NONE',  ( 73.62500000000000000, -7.950000000000000178, -4.867971026610729436E-16 ) ) ;
#360 = VECTOR ( 'NONE', #90136, 1000.000000000000000 ) ;
#361 = CARTESIAN_POINT ( 'NONE',  ( 5.999999999999960032, 18.08204922493374411, 0.9627537363044759156 ) ) ;
#362 = DIRECTION ( 'NONE',  ( 0.7071067811865487940, 0.7071067811865463515, 0.000000000000000000 ) ) ;
#363 = ORIENTED_EDGE ( 'NONE', *, *, #24956, .F. ) ;
#364 = EDGE_CURVE ( 'NONE', #108536, #57879, #101424, .T. ) ;
#365 = MECHANICAL_DESIGN_GEOMETRIC_PRESENTATION_REPRESENTATION (  '', ( #53591 ), #69867 ) ;
#366 = DIRECTION ( 'NONE',  ( -0.7071067811865487940, 0.7071067811865463515, -0.000000000000000000 ) ) ;
#367 = ORIENTED_EDGE ( 'NONE', *, *, #20533, .T. ) ;
#368 = AXIS2_PLACEMENT_3D ( 'NONE', #120768, #21477, #143248 ) ;
#369 = EDGE_CURVE ( 'NONE', #137573, #138987, #81190, .T. ) ;
#370 = DIRECTION ( 'NONE',  ( 0.000000000000000000, 0.000000000000000000, 1.000000000000000000 ) ) ;
#371 = CARTESIAN_POINT ( 'NONE',  ( 62.12543019189810423, 5.291415217122919401, 3.055000000000002824 ) ) ;
#372 = CARTESIAN_POINT ( 'NONE',  ( 24.39999999999999858, -5.520864266206504263E-14, 0.000000000000000000 ) ) ;
#373 = VERTEX_POINT ( 'NONE', #76859 ) ;
#374 = VECTOR ( 'NONE', #35742, 1000.000000000000000 ) ;
#375 = CARTESIAN_POINT ( 'NONE',  ( -24.32816939922336275, 14.25929247661557575, 4.000000000000000000 ) ) ;
#376 = DIRECTION ( 'NONE',  ( -0.7071067811865486830, -0.7071067811865464625, 0.000000000000000000 ) ) ;
#377 = SURFACE_STYLE_USAGE ( .BOTH. , #24296 ) ;
#378 = CARTESIAN_POINT ( 'NONE',  ( 0.3281693992235297785, 17.25929247661554200, 4.000000000000000000 ) ) ;
#379 = EDGE_CURVE ( 'NONE', #60214, #42523, #120557, .T. ) ;
#380 = CARTESIAN_POINT ( 'NONE',  ( 10.37159235450332062, -3.851859888774471706E-31, 2.500000000000001332 ) ) ;
#382 = ORIENTED_EDGE ( 'NONE', *, *, #28958, .T. ) ;
#381 = CARTESIAN_POINT ( 'NONE',  ( -2.999999999999975131, -6.033600742197674727, 5.000000000000000000 ) ) ;
#383 = CARTESIAN_POINT ( 'NONE',  ( -2.999999999999976463, -1.068876922607804314, 4.000000000000000000 ) ) ;
#384 = CARTESIAN_POINT ( 'NONE',  ( 2.218373117075048029, 21.74787736706806385, 4.999607392498048419 ) ) ;
#385 = CARTESIAN_POINT ( 'NONE',  ( -23.99451991528749062, 28.92564299267954908, 4.000000000000000000 ) ) ;
#386 = AXIS2_PLACEMENT_3D ( 'NONE', #58460, #98177, #96016 ) ;
#387 =( NAMED_UNIT ( * ) SI_UNIT ( $, .STERADIAN. ) SOLID_ANGLE_UNIT ( ) );
#388 = ORIENTED_EDGE ( 'NONE', *, *, #12820, .F. ) ;
#389 = ORIENTED_EDGE ( 'NONE', *, *, #16681, .T. ) ;
#390 = CARTESIAN_POINT ( 'NONE',  ( 65.91709685856477563, 3.054999999999998828, 5.291415217122922066 ) ) ;
#391 = VERTEX_POINT ( 'NONE', #65987 ) ;
#392 = CARTESIAN_POINT ( 'NONE',  ( -34.92500000000001137, 22.22500000000000142, 4.000000000000000000 ) ) ;
#393 = CARTESIAN_POINT ( 'NONE',  ( -26.29289321881326558, -9.740707523384184441, 5.000000000000000000 ) ) ;
#394 = DIRECTION ( 'NONE',  ( 0.7071067811865487940, 0.7071067811865463515, 0.000000000000000000 ) ) ;
#395 = VECTOR ( 'NONE', #66581, 1000.000000000000114 ) ;
#396 = CARTESIAN_POINT ( 'NONE',  ( -24.98480450340313652, 2.536990198832462351, 5.000000000000000000 ) ) ;
#397 = CARTESIAN_POINT ( 'NONE',  ( 17.29289321881334018, -6.740707523384209310, 5.000000000000000000 ) ) ;
#398 = VERTEX_POINT ( 'NONE', #23880 ) ;
#399 = ORIENTED_EDGE ( 'NONE', *, *, #4654, .T. ) ;
#400 = VECTOR ( 'NONE', #70487, 1000.000000000000000 ) ;
#401 = DIRECTION ( 'NONE',  ( -0.7071067811865486830, -0.7071067811865464625, 0.000000000000000000 ) ) ;
#402 = CARTESIAN_POINT ( 'NONE',  ( -16.92402963342697220, -0.5732982342275830812, -34.79992920313960525 ) ) ;
#403 = ORIENTED_EDGE ( 'NONE', *, *, #107919, .F. ) ;
#404 = LINE ( 'NONE', #133118, #125414 ) ;
#405 = EDGE_CURVE ( 'NONE', #121029, #128151, #88328, .T. ) ;
#406 = FACE_OUTER_BOUND ( 'NONE', #46336, .T. ) ;
#407 = FACE_OUTER_BOUND ( 'NONE', #98667, .T. ) ;
#408 = AXIS2_PLACEMENT_3D ( 'NONE', #118351, #30665, #74896 ) ;
#409 = ORIENTED_EDGE ( 'NONE', *, *, #43363, .T. ) ;
#410 = FACE_BOUND ( 'NONE', #51809, .T. ) ;
#411 = CARTESIAN_POINT ( 'NONE',  ( -3.005480084712505828, 28.92564299267936079, 4.000000000000000000 ) ) ;
#412 = LINE ( 'NONE', #119338, #62884 ) ;
#413 = CARTESIAN_POINT ( 'NONE',  ( -18.29974487139159223, -27.71228299555219010, 4.000000000000000000 ) ) ;
#414 = CARTESIAN_POINT ( 'NONE',  ( -7.499999999999951150, 13.08746187583912146, 4.000000000000000000 ) ) ;
#415 = LINE ( 'NONE', #88909, #141470 ) ;
#416 = ORIENTED_EDGE ( 'NONE', *, *, #6486, .F. ) ;
#417 = EDGE_CURVE ( 'NONE', #27268, #65916, #67404, .T. ) ;
#418 = ORIENTED_EDGE ( 'NONE', *, *, #36030, .F. ) ;
#419 = CARTESIAN_POINT ( 'NONE',  ( 105.7870968585647802, 3.054999999999997495, 5.291415217122919401 ) ) ;
#420 = ORIENTED_EDGE ( 'NONE', *, *, #111228, .F. ) ;
#421 = EDGE_CURVE ( 'NONE', #133840, #42748, #31897, .T. ) ;
#422 = FILL_AREA_STYLE ('',( #141288 ) ) ;
#423 = ORIENTED_EDGE ( 'NONE', *, *, #120728, .F. ) ;
#424 = ADVANCED_FACE ( 'NONE', ( #143502 ), #11532, .F. ) ;
#425 = CARTESIAN_POINT ( 'NONE',  ( 9.707106781186480404, -0.7407075233842735917, 5.000000000000000000 ) ) ;
#426 = VECTOR ( 'NONE', #53827, 1000.000000000000000 ) ;
#427 = EDGE_CURVE ( 'NONE', #3647, #106547, #19837, .T. ) ;
#428 = SHAPE_REPRESENTATION ( 'slotted pan head screw_iso_ISO 1580 - M5 x 25 - 25S', ( #127880 ), #95551 ) ;
#429 = DIRECTION ( 'NONE',  ( -0.3543493200069162685, -0.000000000000000000, -0.9351131265310288487 ) ) ;
#430 = VECTOR ( 'NONE', #23278, 999.9999999999998863 ) ;
#431 = VECTOR ( 'NONE', #87814, 1000.000000000000000 ) ;
#432 = CARTESIAN_POINT ( 'NONE',  ( 39.29974487139159578, -27.71228299555233576, 4.000000000000000000 ) ) ;
#433 = EDGE_LOOP ( 'NONE', ( #100677, #114743, #113008 ) ) ;
#434 = DIRECTION ( 'NONE',  ( 0.7071067811865487940, 0.7071067811865463515, 0.000000000000000000 ) ) ;
#435 = DIRECTION ( 'NONE',  ( -0.7071067811865487940, 0.7071067811865463515, -0.000000000000000000 ) ) ;
#436 = CARTESIAN_POINT ( 'NONE',  ( 8.999999999999943157, 7.552185695429089130, 5.000000000000000000 ) ) ;
#437 = EDGE_CURVE ( 'NONE', #128814, #125503, #6074, .T. ) ;
#438 = LINE ( 'NONE', #139913, #105981 ) ;
#440 = CARTESIAN_POINT ( 'NONE',  ( 59.14169371712955581, -2.130196079827424871, -7.949999999999998401 ) ) ;
#439 = CARTESIAN_POINT ( 'NONE',  ( 54.03752705046288440, -9.735942053221456900E-16, 7.949999999999998401 ) ) ;
#441 = VECTOR ( 'NONE', #51936, 1000.000000000000000 ) ;
#442 = VECTOR ( 'NONE', #49067, 1000.000000000000000 ) ;
#443 = MECHANICAL_DESIGN_GEOMETRIC_PRESENTATION_REPRESENTATION (  '', ( #97739 ), #18987 ) ;
#444 = DIRECTION ( 'NONE',  ( 0.3543493200069162685, -0.000000000000000000, -0.9351131265310288487 ) ) ;
#445 = VERTEX_POINT ( 'NONE', #6784 ) ;
#446 = DIRECTION ( 'NONE',  ( 0.000000000000000000, 1.000000000000000000, 0.000000000000000000 ) ) ;
#447 = DIRECTION ( 'NONE',  ( 0.6830127018922180770, -0.6830127018922204085, -0.2588190451025213501 ) ) ;
#448 = EDGE_CURVE ( 'NONE', #139414, #35675, #74241, .T. ) ;
#449 = ORIENTED_EDGE ( 'NONE', *, *, #79627, .F. ) ;
#450 = EDGE_LOOP ( 'NONE', ( #37770, #449, #12481, #125 ) ) ;
#451 = EDGE_CURVE ( 'NONE', #68140, #73925, #41598, .T. ) ;
#452 = EDGE_LOOP ( 'NONE', ( #21111, #56741, #113242, #114759 ) ) ;
#453 = CARTESIAN_POINT ( 'NONE',  ( 53.81293019189810423, -1.637169565754159617, -6.110000000000001208 ) ) ;
#454 = EDGE_LOOP ( 'NONE', ( #116566, #36964, #17088, #40231, #105946, #55816 ) ) ;
#455 = EDGE_CURVE ( 'NONE', #121396, #35500, #128617, .T. ) ;
#456 = PLANE ( 'NONE',  #41905 ) ;
#457 = CARTESIAN_POINT ( 'NONE',  ( 1.504139616203772789, -3.047499999999994547, 5.278424836066145431 ) ) ;
#458 = CARTESIAN_POINT ( 'NONE',  ( 93.47959685856476142, 6.109999999999999432, 1.637169565754164280 ) ) ;
#459 = CYLINDRICAL_SURFACE ( 'NONE', #21662, 0.5000000000000004441 ) ;
#460 = ORIENTED_EDGE ( 'NONE', *, *, #37283, .F. ) ;
#461 = DIRECTION ( 'NONE',  ( -0.000000000000000000, -0.3543493200069152693, 0.9351131265310292928 ) ) ;
#462 = LINE ( 'NONE', #141906, #37760 ) ;
#463 = ORIENTED_EDGE ( 'NONE', *, *, #82126, .T. ) ;
#464 = DIRECTION ( 'NONE',  ( -1.000000000000000000, -1.224606353822377258E-16, -0.000000000000000000 ) ) ;
#465 = AXIS2_PLACEMENT_3D ( 'NONE', #68774, #78939, #1320 ) ;
#466 = PLANE ( 'NONE',  #66047 ) ;
#467 = VERTEX_POINT ( 'NONE', #51789 ) ;
#468 = AXIS2_PLACEMENT_3D ( 'NONE', #89931, #34153, #23234 ) ;
#469 = DIRECTION ( 'NONE',  ( 1.000000000000000000, 0.000000000000000000, 0.000000000000000000 ) ) ;
#470 = DIRECTION ( 'NONE',  ( -0.7071067811865486830, 0.7071067811865464625, 0.000000000000000000 ) ) ;
#471 = ORIENTED_EDGE ( 'NONE', *, *, #95394, .T. ) ;
#472 = AXIS2_PLACEMENT_3D ( 'NONE', #141340, #42773, #52189 ) ;
#473 = ORIENTED_EDGE ( 'NONE', *, *, #137601, .F. ) ;
#474 = VERTEX_POINT ( 'NONE', #29291 ) ;
#475 = EDGE_CURVE ( 'NONE', #12429, #109431, #7525, .T. ) ;
#476 = CARTESIAN_POINT ( 'NONE',  ( 121.2454301918981230, -5.291415217122918513, -3.055000000000000160 ) ) ;
#477 = VECTOR ( 'NONE', #71928, 1000.000000000000227 ) ;
#478 = LINE ( 'NONE', #33862, #127907 ) ;
#479 = CARTESIAN_POINT ( 'NONE',  ( 34.92499999999998295, 13.70193056682084887, 4.500000000000000888 ) ) ;
#480 = ORIENTED_EDGE ( 'NONE', *, *, #67194, .T. ) ;
#481 = CARTESIAN_POINT ( 'NONE',  ( -16.49999999999988276, -13.53360074219760101, 5.000000000000000000 ) ) ;
#482 = VERTEX_POINT ( 'NONE', #31451 ) ;
#483 = VECTOR ( 'NONE', #57375, 1000.000000000000227 ) ;
#484 = CARTESIAN_POINT ( 'NONE',  ( 10.33290314143522082, -3.967499999999994476, 6.871911579029513106 ) ) ;
#485 = PLANE ( 'NONE',  #101778 ) ;
#486 = DIRECTION ( 'NONE',  ( 0.000000000000000000, 0.000000000000000000, -1.000000000000000000 ) ) ;
#487 = CARTESIAN_POINT ( 'NONE',  ( -12.69999999999998153, -0.3999999999999997446, -2.467792535850613866 ) ) ;
#488 = VERTEX_POINT ( 'NONE', #75673 ) ;
#489 = VERTEX_POINT ( 'NONE', #100278 ) ;
#490 = ADVANCED_FACE ( 'NONE', ( #66231 ), #198, .F. ) ;
#491 = VECTOR ( 'NONE', #127188, 1000.000000000000000 ) ;
#492 = ORIENTED_EDGE ( 'NONE', *, *, #81875, .T. ) ;
#493 = PLANE ( 'NONE',  #37151 ) ;
#494 = CARTESIAN_POINT ( 'NONE',  ( 39.29974487139159578, -27.71228299555233576, 4.000000000000000000 ) ) ;
#495 = VECTOR ( 'NONE', #102903, 1000.000000000000114 ) ;
#496 = DIRECTION ( 'NONE',  ( -1.000000000000000000, 0.000000000000000000, -0.000000000000000000 ) ) ;
#497 = CARTESIAN_POINT ( 'NONE',  ( -23.99999999999983302, 16.93112307739201583, 4.000000000000000000 ) ) ;
#498 = CARTESIAN_POINT ( 'NONE',  ( -14.24890464969599435, -0.3792994071806680689, 4.162343009174984232 ) ) ;
#499 = DIRECTION ( 'NONE',  ( -0.3543493200069162685, -0.000000000000000000, -0.9351131265310288487 ) ) ;
#500 = EDGE_CURVE ( 'NONE', #83224, #56577, #120555, .T. ) ;
#501 = LINE ( 'NONE', #20833, #42091 ) ;
#502 = DIRECTION ( 'NONE',  ( -0.7071067811865486830, 0.7071067811865464625, 0.000000000000000000 ) ) ;
#503 = ORIENTED_EDGE ( 'NONE', *, *, #122198, .F. ) ;
#504 = CARTESIAN_POINT ( 'NONE',  ( -41.99451991528749062, 28.92564299267967343, 4.000000000000000000 ) ) ;
#505 = VECTOR ( 'NONE', #41332, 1000.000000000000000 ) ;
#506 = EDGE_LOOP ( 'NONE', ( #140030, #45972, #39854, #108702 ) ) ;
#507 = CARTESIAN_POINT ( 'NONE',  ( 57.18398860626899705, 28.73617430169827358, 5.000000000000000000 ) ) ;
#508 = ORIENTED_EDGE ( 'NONE', *, *, #48578, .F. ) ;
#509 = CARTESIAN_POINT ( 'NONE',  ( -48.48921356237309510, -27.52281430457089328, 5.000000000000000000 ) ) ;
#511 = ORIENTED_EDGE ( 'NONE', *, *, #137999, .F. ) ;
#510 = CARTESIAN_POINT ( 'NONE',  ( -48.48921356237309510, -27.52281430457089328, 5.000000000000000000 ) ) ;
#512 = EDGE_CURVE ( 'NONE', #80329, #53800, #11805, .T. ) ;
#513 = DIRECTION ( 'NONE',  ( -0.7071067811865487940, 0.7071067811865463515, -0.000000000000000000 ) ) ;
#514 = LINE ( 'NONE', #1914, #14794 ) ;
#515 = ORIENTED_EDGE ( 'NONE', *, *, #127473, .F. ) ;
#516 = CARTESIAN_POINT ( 'NONE',  ( -15.18398860626900237, 28.73617430169797871, 5.000000000000000000 ) ) ;
#518 = ORIENTED_EDGE ( 'NONE', *, *, #141850, .T. ) ;
#517 = AXIS2_PLACEMENT_3D ( 'NONE', #20502, #1596, #109680 ) ;
#519 = DIRECTION ( 'NONE',  ( -0.7071067811865487940, 0.7071067811865463515, -0.000000000000000000 ) ) ;
#520 = ORIENTED_EDGE ( 'NONE', *, *, #112530, .T. ) ;
#521 = LINE ( 'NONE', #89005, #45331 ) ;
#522 = CARTESIAN_POINT ( 'NONE',  ( 111.0583603837961988, -7.949999999999997513, -2.130196079827425759 ) ) ;
#523 = CARTESIAN_POINT ( 'NONE',  ( 0.000000000000000000, -40.42999999999999261, -39.50000000000000000 ) ) ;
#524 =( NAMED_UNIT ( * ) SI_UNIT ( $, .STERADIAN. ) SOLID_ANGLE_UNIT ( ) );
#525 = DIRECTION ( 'NONE',  ( 0.7071067811865487940, 0.7071067811865463515, 0.000000000000000000 ) ) ;
#526 = CARTESIAN_POINT ( 'NONE',  ( 13.92145407031093818, 4.584330080086930965E-16, 0.000000000000000000 ) ) ;
#527 = LINE ( 'NONE', #44069, #11340 ) ;
#528 = CARTESIAN_POINT ( 'NONE',  ( 18.22916666666666785, -6.094999999999989093, 1.633150327867691765 ) ) ;
#529 = DIRECTION ( 'NONE',  ( -0.7071067811865486830, -0.7071067811865464625, 0.000000000000000000 ) ) ;
#530 = VECTOR ( 'NONE', #99105, 999.9999999999998863 ) ;
#531 = VECTOR ( 'NONE', #90557, 1000.000000000000000 ) ;
#533 = CARTESIAN_POINT ( 'NONE',  ( 0.000000000000000000, 0.000000000000000000, 7.950000000000000178 ) ) ;
#532 = VECTOR ( 'NONE', #82631, 1000.000000000000000 ) ;
#534 = LINE ( 'NONE', #75981, #91767 ) ;
#535 = ORIENTED_EDGE ( 'NONE', *, *, #15196, .F. ) ;
#536 = VERTEX_POINT ( 'NONE', #86555 ) ;
#537 = AXIS2_PLACEMENT_3D ( 'NONE', #63476, #8301, #7604 ) ;
#538 = COLOUR_RGB ( '', 0.09019608, 0.27058824, 0.51372549) ;
#539 = CARTESIAN_POINT ( 'NONE',  ( 27.70710678118635073, -12.74070752338415424, 5.000000000000000000 ) ) ;
#540 = VERTEX_POINT ( 'NONE', #130787 ) ;
#541 = ADVANCED_FACE ( 'NONE', ( #99530 ), #56092, .F. ) ;
#542 = CARTESIAN_POINT ( 'NONE',  ( 106.7504301918981184, 3.055000000000002824, -5.291415217122919401 ) ) ;
#543 = LINE ( 'NONE', #123072, #77852 ) ;
#544 = LINE ( 'NONE', #44839, #9237 ) ;
#545 = AXIS2_PLACEMENT_3D ( 'NONE', #123467, #24124, #58230 ) ;
#547 = VECTOR ( 'NONE', #85064, 1000.000000000000000 ) ;
#546 = CARTESIAN_POINT ( 'NONE',  ( -34.49999999999975842, -7.535744391599424219, 4.994342998332167660 ) ) ;
#548 = CARTESIAN_POINT ( 'NONE',  ( 0.000000000000000000, 0.000000000000000000, 5.000000000000000000 ) ) ;
#549 = ORIENTED_EDGE ( 'NONE', *, *, #89231, .T. ) ;
#550 = LINE ( 'NONE', #133943, #31321 ) ;
#551 = DIRECTION ( 'NONE',  ( -0.5735764363510499342, -0.8191520442889891340, 0.000000000000000000 ) ) ;
#552 = CARTESIAN_POINT ( 'NONE',  ( 21.32816939922336985, -15.74070752338412760, 4.000000000000000000 ) ) ;
#553 = EDGE_CURVE ( 'NONE', #52608, #118518, #64800, .T. ) ;
#554 = CARTESIAN_POINT ( 'NONE',  ( 34.49999999999975131, 22.21934299833216642, 4.348028800457638177 ) ) ;
#555 = EDGE_CURVE ( 'NONE', #94937, #79882, #33614, .T. ) ;
#556 = CARTESIAN_POINT ( 'NONE',  ( -24.70710678118637205, 8.259292476615636147, 5.000000000000000000 ) ) ;
#558 = VERTEX_POINT ( 'NONE', #43749 ) ;
#557 = FACE_OUTER_BOUND ( 'NONE', #112855, .T. ) ;
#559 = CYLINDRICAL_SURFACE ( 'NONE', #125629, 9.119999999999999218 ) ;
#560 = CARTESIAN_POINT ( 'NONE',  ( 1.516262732464673579, 3.821174125832445049E-16, 0.000000000000000000 ) ) ;
#561 = SURFACE_STYLE_FILL_AREA ( #32509 ) ;
#562 = CARTESIAN_POINT ( 'NONE',  ( 47.99451991528749062, 28.92564299267971251, 4.000000000000000000 ) ) ;
#563 = CARTESIAN_POINT ( 'NONE',  ( 3.707106781186515487, -15.74070752338412404, 5.000000000000000000 ) ) ;
#564 = ORIENTED_EDGE ( 'NONE', *, *, #87957, .F. ) ;
#565 = ORIENTED_EDGE ( 'NONE', *, *, #54246, .F. ) ;
#566 = VERTEX_POINT ( 'NONE', #32907 ) ;
#567 = CARTESIAN_POINT ( 'NONE',  ( 94.50043019189810423, -3.055000000000002380, 5.291415217122920289 ) ) ;
#568 = ORIENTED_EDGE ( 'NONE', *, *, #120751, .T. ) ;
#569 = DIRECTION ( 'NONE',  ( 0.7071067811865487940, -0.7071067811865463515, 0.000000000000000000 ) ) ;
#570 = CARTESIAN_POINT ( 'NONE',  ( -12.69999999999998153, 0.000000000000000000, 0.000000000000000000 ) ) ;
#571 = CARTESIAN_POINT ( 'NONE',  ( -17.99451991528748351, 28.92564299267950645, 4.000000000000000000 ) ) ;
#572 = CARTESIAN_POINT ( 'NONE',  ( 0.000000000000000000, 0.000000000000000000, 5.000000000000000000 ) ) ;
#573 = ORIENTED_EDGE ( 'NONE', *, *, #143462, .T. ) ;
#574 = EDGE_CURVE ( 'NONE', #120024, #43089, #22666, .T. ) ;
#575 = CARTESIAN_POINT ( 'NONE',  ( 20.99999999999985079, -16.06887692260765377, 4.000000000000000000 ) ) ;
#576 = DIRECTION ( 'NONE',  ( -1.000000000000000000, 0.000000000000000000, -0.000000000000000000 ) ) ;
#577 = AXIS2_PLACEMENT_3D ( 'NONE', #85870, #75032, #8969 ) ;
#578 = CARTESIAN_POINT ( 'NONE',  ( 83.47459685856478018, 1.637169565754164058, -6.109999999999996767 ) ) ;
#579 = ORIENTED_EDGE ( 'NONE', *, *, #10590, .F. ) ;
#580 = VECTOR ( 'NONE', #117247, 1000.000000000000227 ) ;
#581 = LINE ( 'NONE', #108604, #83736 ) ;
#583 = VECTOR ( 'NONE', #73522, 1000.000000000000227 ) ;
#582 = PLANE ( 'NONE',  #88617 ) ;
#584 = AXIS2_PLACEMENT_3D ( 'NONE', #45025, #34830, #21796 ) ;
#585 = EDGE_LOOP ( 'NONE', ( #84587, #117927, #110585, #17558 ) ) ;
#586 = ORIENTED_EDGE ( 'NONE', *, *, #664, .T. ) ;
#587 = ORIENTED_EDGE ( 'NONE', *, *, #53900, .F. ) ;
#588 = FACE_OUTER_BOUND ( 'NONE', #75692, .T. ) ;
#589 = CARTESIAN_POINT ( 'NONE',  ( 5.700255128608413102, -27.71228299555201957, 4.000000000000000000 ) ) ;
#590 = CARTESIAN_POINT ( 'NONE',  ( 18.00456980810188767, 6.871911579029510442, -3.967499999999998916 ) ) ;
#591 = CARTESIAN_POINT ( 'NONE',  ( 6.066782984417857350, 2.500000000000000444, 0.000000000000000000 ) ) ;
#592 = CARTESIAN_POINT ( 'NONE',  ( 166.4267503027637929, 26.96999999999993847, 33.05223327726561422 ) ) ;
#593 = CARTESIAN_POINT ( 'NONE',  ( 26.99999999999980815, 10.21212019023811557, -2.019456568337861135 ) ) ;
#594 = EDGE_CURVE ( 'NONE', #43234, #102340, #12534, .T. ) ;
#595 = LINE ( 'NONE', #67318, #59027 ) ;
#596 = ADVANCED_FACE ( 'NONE', ( #108976 ), #23407, .F. ) ;
#597 = ORIENTED_EDGE ( 'NONE', *, *, #82825, .T. ) ;
#598 = ORIENTED_EDGE ( 'NONE', *, *, #22116, .T. ) ;
#599 = EDGE_CURVE ( 'NONE', #53838, #27206, #43053, .T. ) ;
#600 = CARTESIAN_POINT ( 'NONE',  ( -2.671830600776458287, 5.259292476615669010, 4.000000000000000000 ) ) ;
#601 = ORIENTED_EDGE ( 'NONE', *, *, #119460, .T. ) ;
#602 = ORIENTED_EDGE ( 'NONE', *, *, #80662, .F. ) ;
#603 = AXIS2_PLACEMENT_3D ( 'NONE', #111128, #114010, #68409 ) ;
#604 = EDGE_CURVE ( 'NONE', #29147, #103671, #114246, .T. ) ;
#605 = EDGE_CURVE ( 'NONE', #107763, #100224, #143057, .T. ) ;
#606 = CARTESIAN_POINT ( 'NONE',  ( -9.183988606268997046, 28.73617430169793607, 5.000000000000000000 ) ) ;
#607 = ORIENTED_EDGE ( 'NONE', *, *, #61214, .T. ) ;
#608 = CARTESIAN_POINT ( 'NONE',  ( -11.67183060077639212, -3.740707523384244837, 4.000000000000000000 ) ) ;
#609 = CARTESIAN_POINT ( 'NONE',  ( -4.110173228882081808, -22.22499999999999787, 4.785647885939356527 ) ) ;
#610 = CARTESIAN_POINT ( 'NONE',  ( 34.45011844616451668, -19.48371918836231131, 5.000000000000000888 ) ) ;
#611 = CARTESIAN_POINT ( 'NONE',  ( 0.000000000000000000, 0.000000000000000000, 5.000000000000000000 ) ) ;
#612 = VECTOR ( 'NONE', #14332, 1000.000000000000000 ) ;
#613 = LINE ( 'NONE', #33988, #72153 ) ;
#614 = ORIENTED_EDGE ( 'NONE', *, *, #124518, .T. ) ;
#615 = EDGE_CURVE ( 'NONE', #122922, #20850, #37895, .T. ) ;
#616 = ORIENTED_EDGE ( 'NONE', *, *, #111910, .T. ) ;
#617 = PLANE ( 'NONE',  #31847 ) ;
#618 = ORIENTED_EDGE ( 'NONE', *, *, #37492, .F. ) ;
#619 = LINE ( 'NONE', #111537, #97830 ) ;
#620 = EDGE_CURVE ( 'NONE', #75539, #80902, #91546, .T. ) ;
#621 = ORIENTED_EDGE ( 'NONE', *, *, #448, .T. ) ;
#622 = CARTESIAN_POINT ( 'NONE',  ( 84.18398860626899705, 28.73617430169846187, 5.000000000000000000 ) ) ;
#623 = ORIENTED_EDGE ( 'NONE', *, *, #73535, .T. ) ;
#624 = EDGE_LOOP ( 'NONE', ( #65991, #135134, #38337 ) ) ;
#625 = VECTOR ( 'NONE', #10022, 1000.000000000000000 ) ;
#626 = VERTEX_POINT ( 'NONE', #16070 ) ;
#627 = EDGE_CURVE ( 'NONE', #673, #24426, #48759, .T. ) ;
#628 = DIRECTION ( 'NONE',  ( 0.7071067811865487940, -0.7071067811865463515, 0.000000000000000000 ) ) ;
#629 = DIRECTION ( 'NONE',  ( 0.7071067811865486830, -0.7071067811865464625, -0.000000000000000000 ) ) ;
#630 = CARTESIAN_POINT ( 'NONE',  ( 29.20710678118634718, -5.240707523384230626, 5.000000000000000000 ) ) ;
#631 = CARTESIAN_POINT ( 'NONE',  ( 126.5837635252314612, -6.110000000000001208, -3.741295971395164515E-16 ) ) ;
#632 = CARTESIAN_POINT ( 'NONE',  ( 30.48921356237309510, -27.52281430457076894, 5.000000000000000000 ) ) ;
#633 = CARTESIAN_POINT ( 'NONE',  ( 13.82816939922344091, 6.759292476615649470, 4.000000000000000000 ) ) ;
#634 = CARTESIAN_POINT ( 'NONE',  ( 24.39999999999999858, -16.48000000000005016, 33.92499999999998295 ) ) ;
#635 = EDGE_CURVE ( 'NONE', #24706, #53682, #47379, .T. ) ;
#636 = VECTOR ( 'NONE', #35690, 999.9999999999998863 ) ;
#637 = PLANE ( 'NONE',  #65519 ) ;
#638 = VECTOR ( 'NONE', #31363, 999.9999999999998863 ) ;
#639 = VECTOR ( 'NONE', #108295, 1000.000000000000000 ) ;
#640 = CARTESIAN_POINT ( 'NONE',  ( 19.04500000000000881, 3.130000000000007887, -22.35000000000000142 ) ) ;
#641 = ORIENTED_EDGE ( 'NONE', *, *, #126480, .F. ) ;
#642 = DIRECTION ( 'NONE',  ( -0.7071067811865486830, -0.7071067811865464625, 0.000000000000000000 ) ) ;
#643 = FACE_OUTER_BOUND ( 'NONE', #70966, .T. ) ;
#644 = EDGE_LOOP ( 'NONE', ( #63079, #95765, #122634, #54205, #52507, #92729, #71035, #105923, #46654 ) ) ;
#645 = VERTEX_POINT ( 'NONE', #82129 ) ;
#646 = AXIS2_PLACEMENT_3D ( 'NONE', #17941, #17261, #27404 ) ;
#648 = ORIENTED_EDGE ( 'NONE', *, *, #75395, .F. ) ;
#647 = EDGE_CURVE ( 'NONE', #93537, #97071, #26987, .T. ) ;
#649 = AXIS2_PLACEMENT_3D ( 'NONE', #98295, #41049, #75831 ) ;
#650 = AXIS2_PLACEMENT_3D ( 'NONE', #123682, #2556, #90297 ) ;
#651 = B_SPLINE_CURVE_WITH_KNOTS ( 'NONE', 3,
 ( #139201, #42017, #96340, #72543, #117387, #140584, #118840, #17386, #41274, #9323, #39892, #85482, #18060, #129710, #30417, #19530, #31144, #107932, #8601, #52849, #97044, #141306, #86234, #119521, #53605, #103316, #91068, #114212, #48245, #79507, #101192, #14894, #25050, #57018 ),
 .UNSPECIFIED., .F., .F.,
 ( 4, 2, 2, 2, 2, 2, 2, 2, 2, 2, 2, 2, 2, 2, 2, 2, 4 ),
 ( 0.000000000000000000, 0.002428652292010244872, 0.003642978438015367741, 0.004857304584020490611, 0.006071630730025613480, 0.007285956876030735482, 0.008500283022035860087, 0.009714609168040984691, 0.01032177224104354613, 0.01092893531404610583, 0.01214326146005123043, 0.01335758760605635503, 0.01457191375206147964, 0.01578623989806660424, 0.01700056604407173058, 0.01821489219007685345, 0.01942921833608197632 ),
 .UNSPECIFIED. ) ;
#652 = CARTESIAN_POINT ( 'NONE',  ( 36.18398860626899705, 28.73617430169812437, 5.000000000000000000 ) ) ;
#653 = ORIENTED_EDGE ( 'NONE', *, *, #128854, .T. ) ;
#654 = ORIENTED_EDGE ( 'NONE', *, *, #99886, .F. ) ;
#655 = CARTESIAN_POINT ( 'NONE',  ( -8.050415908692611922, -22.22500000000000142, 15.18378453690488072 ) ) ;
#656 = CARTESIAN_POINT ( 'NONE',  ( 108.1416937171295700, -2.130196079827424871, -7.949999999999998401 ) ) ;
#657 = DIRECTION ( 'NONE',  ( -0.6830127018922181881, 0.6830127018922202975, -0.2588190451025214056 ) ) ;
#658 = CARTESIAN_POINT ( 'NONE',  ( 42.48921356237308800, -27.52281430457085065, 5.000000000000000000 ) ) ;
#659 = EDGE_CURVE ( 'NONE', #13443, #108133, #113272, .T. ) ;
#660 = ORIENTED_EDGE ( 'NONE', *, *, #55307, .T. ) ;
#661 = LINE ( 'NONE', #43469, #58016 ) ;
#662 = ORIENTED_EDGE ( 'NONE', *, *, #138768, .T. ) ;
#663 = FACE_OUTER_BOUND ( 'NONE', #7412, .T. ) ;
#664 = EDGE_CURVE ( 'NONE', #70961, #59222, #36447, .T. ) ;
#665 = CIRCLE ( 'NONE', #130268, 2.500000000000000888 ) ;
#666 = CARTESIAN_POINT ( 'NONE',  ( 16.10873647476855552, -5.808823158059033709, 5.808823158059035485 ) ) ;
#667 = VERTEX_POINT ( 'NONE', #3090 ) ;
#668 = CARTESIAN_POINT ( 'NONE',  ( 87.12043019189812298, 3.055000000000002380, -5.291415217122917625 ) ) ;
#669 = CARTESIAN_POINT ( 'NONE',  ( 8.372623110723612427, -8.651829453956585425, -3.925649932724890157 ) ) ;
#670 = CARTESIAN_POINT ( 'NONE',  ( 99.10002705046288440, 5.819803920172570422, 5.819803920172575751 ) ) ;
#671 = ORIENTED_EDGE ( 'NONE', *, *, #119679, .F. ) ;
#672 = VERTEX_POINT ( 'NONE', #81409 ) ;
#673 = VERTEX_POINT ( 'NONE', #57504 ) ;
#674 = FACE_OUTER_BOUND ( 'NONE', #8826, .T. ) ;
#675 = DIRECTION ( 'NONE',  ( 1.000000000000000000, -1.248002500702738701E-15, 3.404785525682858480E-16 ) ) ;
#676 = PLANE ( 'NONE',  #72895 ) ;
#677 = CARTESIAN_POINT ( 'NONE',  ( 20.99999999999985079, -6.108550654416941228, -3.114665004254919101 ) ) ;
#678 = ORIENTED_EDGE ( 'NONE', *, *, #11186, .F. ) ;
#679 = FILL_AREA_STYLE ('',( #44971 ) ) ;
#680 = LINE ( 'NONE', #44973, #51290 ) ;
#681 = LINE ( 'NONE', #79745, #4821 ) ;
#682 = ORIENTED_EDGE ( 'NONE', *, *, #122898, .T. ) ;
#683 = PLANE ( 'NONE',  #37383 ) ;
#684 = DIRECTION ( 'NONE',  ( 0.7071067811865487940, 0.7071067811865463515, 0.000000000000000000 ) ) ;
#685 = EDGE_LOOP ( 'NONE', ( #90796, #60174, #71280, #138128 ) ) ;
#687 = VERTEX_POINT ( 'NONE', #80678 ) ;
#686 = LINE ( 'NONE', #132693, #50983 ) ;
#688 = ORIENTED_EDGE ( 'NONE', *, *, #99468, .T. ) ;
#689 = CARTESIAN_POINT ( 'NONE',  ( 21.48921356237309155, -27.52281430457070499, 5.000000000000000000 ) ) ;
#690 = LINE ( 'NONE', #131960, #52937 ) ;
#691 = ORIENTED_EDGE ( 'NONE', *, *, #94261, .T. ) ;
#692 = FILL_AREA_STYLE_COLOUR ( '', #111503 ) ;
#693 = VECTOR ( 'NONE', #63519, 1000.000000000000000 ) ;
#694 = CARTESIAN_POINT ( 'NONE',  ( -2.510786437626908008, -27.52281430457053446, 5.000000000000000000 ) ) ;
#695 = CARTESIAN_POINT ( 'NONE',  ( 0.000000000000000000, 0.000000000000000000, 5.000000000000000000 ) ) ;
#696 = CARTESIAN_POINT ( 'NONE',  ( -15.48921356237309510, -27.52281430457066236, 5.000000000000000000 ) ) ;
#697 = CARTESIAN_POINT ( 'NONE',  ( 14.70692117890024697, 3.061616997868383634E-16, -2.500000000000000444 ) ) ;
#698 = DIRECTION ( 'NONE',  ( 0.000000000000000000, 1.000000000000000000, 0.000000000000000000 ) ) ;
#699 = VECTOR ( 'NONE', #102639, 1000.000000000000227 ) ;
#700 = PLANE ( 'NONE',  #109644 ) ;
#701 = LINE ( 'NONE', #44997, #59943 ) ;
#702 = CARTESIAN_POINT ( 'NONE',  ( 20.68706980810189222, -2.126176841940956130, 7.934999999999991616 ) ) ;
#703 = DIRECTION ( 'NONE',  ( -0.000000000000000000, 0.3543493200069152138, -0.9351131265310292928 ) ) ;
#704 = CIRCLE ( 'NONE', #121067, 2.500000000000000444 ) ;
#705 = CARTESIAN_POINT ( 'NONE',  ( 12.18398860626900060, 28.73617430169795739, 5.000000000000000000 ) ) ;
#706 = CARTESIAN_POINT ( 'NONE',  ( 66.18398860626901126, 28.73617430169833753, 5.000000000000000000 ) ) ;
#707 = FACE_OUTER_BOUND ( 'NONE', #88184, .T. ) ;
#708 = EDGE_LOOP ( 'NONE', ( #23324, #103090, #25830, #73276 ) ) ;
#709 = EDGE_LOOP ( 'NONE', ( #127924, #22174, #9037, #2696 ) ) ;
#710 = CARTESIAN_POINT ( 'NONE',  ( 99.29166666666667140, 3.975000000000003642, -6.884901960086285300 ) ) ;
#711 = ORIENTED_EDGE ( 'NONE', *, *, #130086, .T. ) ;
#712 = ORIENTED_EDGE ( 'NONE', *, *, #38638, .T. ) ;
#713 = ORIENTED_EDGE ( 'NONE', *, *, #40905, .F. ) ;
#714 = CARTESIAN_POINT ( 'NONE',  ( -15.18398860626900237, 28.73617430169797871, 5.000000000000000000 ) ) ;
#715 = FACE_OUTER_BOUND ( 'NONE', #19018, .T. ) ;
#716 = VECTOR ( 'NONE', #61353, 1000.000000000000000 ) ;
#717 = ORIENTED_EDGE ( 'NONE', *, *, #51275, .F. ) ;
#718 = DIRECTION ( 'NONE',  ( -0.7071067811865486830, -0.7071067811865464625, -0.000000000000000000 ) ) ;
#719 = LINE ( 'NONE', #121084, #83549 ) ;
#720 = CARTESIAN_POINT ( 'NONE',  ( 22.75000000000000355, -7.464222240803106570E-16, -6.094999999999989981 ) ) ;
#721 = PLANE ( 'NONE',  #7126 ) ;
#722 = ADVANCED_FACE ( 'NONE', ( #69825 ), #13234, .F. ) ;
#723 = ORIENTED_EDGE ( 'NONE', *, *, #4699, .F. ) ;
#724 = ADVANCED_FACE ( 'NONE', ( #2348 ), #25555, .F. ) ;
#726 = CIRCLE ( 'NONE', #7757, 2.500000000000000888 ) ;
#725 = DIRECTION ( 'NONE',  ( -1.000000000000000000, 0.000000000000000000, -0.000000000000000000 ) ) ;
#727 = CARTESIAN_POINT ( 'NONE',  ( -33.18398860626899705, 28.73617430169810305, 5.000000000000000000 ) ) ;
#728 = CARTESIAN_POINT ( 'NONE',  ( 62.99451991528749772, 28.92564299267982264, 4.000000000000000000 ) ) ;
#729 = LINE ( 'NONE', #45023, #17561 ) ;
#730 = DIRECTION ( 'NONE',  ( 0.000000000000000000, 1.000000000000000000, 0.000000000000000000 ) ) ;
#731 = DIRECTION ( 'NONE',  ( -0.7071067811865487940, 0.7071067811865463515, -0.000000000000000000 ) ) ;
#732 = EDGE_LOOP ( 'NONE', ( #19977, #72782, #56165, #112373 ) ) ;
#733 = ORIENTED_EDGE ( 'NONE', *, *, #102361, .F. ) ;
#734 = CARTESIAN_POINT ( 'NONE',  ( 120.8962635252314186, 4.472830434245840259, -4.472830434245839371 ) ) ;
#735 = ORIENTED_EDGE ( 'NONE', *, *, #48279, .T. ) ;
#736 = EDGE_CURVE ( 'NONE', #98842, #15513, #59650, .T. ) ;
#737 = DIRECTION ( 'NONE',  ( 0.7071067811865487940, -0.7071067811865463515, 0.000000000000000000 ) ) ;
#738 = VECTOR ( 'NONE', #29742, 999.9999999999998863 ) ;
#739 = DIRECTION ( 'NONE',  ( 0.3543493200069162685, -0.000000000000000000, -0.9351131265310288487 ) ) ;
#740 = EDGE_CURVE ( 'NONE', #1167, #13678, #45912, .T. ) ;
#741 = DIRECTION ( 'NONE',  ( 0.7071067811865486830, -0.7071067811865464625, -0.000000000000000000 ) ) ;
#742 = AXIS2_PLACEMENT_3D ( 'NONE', #72568, #104411, #5073 ) ;
#743 = CARTESIAN_POINT ( 'NONE',  ( 113.9537635252314516, -6.109999999999998543, -3.741295971395162543E-16 ) ) ;
#744 = ORIENTED_EDGE ( 'NONE', *, *, #46623, .T. ) ;
#745 = VERTEX_POINT ( 'NONE', #106668 ) ;
#746 = VECTOR ( 'NONE', #44314, 1000.000000000000000 ) ;
#747 = PRODUCT_DEFINITION_FORMATION_WITH_SPECIFIED_SOURCE ( 'ANY', '', #32831, .NOT_KNOWN. ) ;
#748 = CARTESIAN_POINT ( 'NONE',  ( -10.49999999999992006, 6.052185695429103340, 5.000000000000000000 ) ) ;
#749 = EDGE_CURVE ( 'NONE', #77643, #28995, #40049, .T. ) ;
#750 = CARTESIAN_POINT ( 'NONE',  ( 97.97916666666667140, -7.950000000000000178, 2.130196079827424427 ) ) ;
#751 = VERTEX_POINT ( 'NONE', #39315 ) ;
#752 = EDGE_LOOP ( 'NONE', ( #20197, #50764, #68012, #107527 ) ) ;
#753 = CARTESIAN_POINT ( 'NONE',  ( 36.16709685856476852, -3.055000000000000160, -5.291415217122921177 ) ) ;
#754 = ORIENTED_EDGE ( 'NONE', *, *, #126186, .F. ) ;
#755 = DIRECTION ( 'NONE',  ( -0.7071067811865486830, -0.7071067811865463515, 0.000000000000000000 ) ) ;
#756 = DIRECTION ( 'NONE',  ( -0.3543493200069162685, -0.000000000000000000, -0.9351131265310288487 ) ) ;
#757 = CARTESIAN_POINT ( 'NONE',  ( -23.99451991528749062, 28.92564299267954908, 4.000000000000000000 ) ) ;
#758 = VECTOR ( 'NONE', #100911, 1000.000000000000227 ) ;
#759 = CARTESIAN_POINT ( 'NONE',  ( 31.41209685856477662, 5.291415217122921177, -3.054999999999994831 ) ) ;
#760 = ORIENTED_EDGE ( 'NONE', *, *, #91607, .F. ) ;
#761 = ADVANCED_FACE ( 'NONE', ( #6610 ), #61111, .F. ) ;
#762 = LINE ( 'NONE', #89924, #117300 ) ;
#763 = ORIENTED_EDGE ( 'NONE', *, *, #55111, .T. ) ;
#764 = VERTEX_POINT ( 'NONE', #93687 ) ;
#765 = EDGE_LOOP ( 'NONE', ( #81631, #28554, #45008 ) ) ;
#766 = VECTOR ( 'NONE', #69328, 1000.000000000000227 ) ;
#767 = ADVANCED_FACE ( 'NONE', ( #62489 ), #137913, .T. ) ;
#768 = EDGE_CURVE ( 'NONE', #109345, #74861, #53227, .T. ) ;
#769 = CARTESIAN_POINT ( 'NONE',  ( 29.99999999999979039, -10.06887692260770528, 4.000000000000000000 ) ) ;
#770 = DIRECTION ( 'NONE',  ( 0.000000000000000000, 0.000000000000000000, 1.000000000000000000 ) ) ;
#771 = VERTEX_POINT ( 'NONE', #72696 ) ;
#772 = AXIS2_PLACEMENT_3D ( 'NONE', #3609, #81964, #5032 ) ;
#773 = PLANE ( 'NONE',  #106202 ) ;
#774 = PLANE ( 'NONE',  #135913 ) ;
#775 = EDGE_CURVE ( 'NONE', #27298, #47459, #36603, .T. ) ;
#776 = CARTESIAN_POINT ( 'NONE',  ( 82.03752705046288440, -9.735942053221456900E-16, 7.949999999999998401 ) ) ;
#777 = VECTOR ( 'NONE', #141746, 1000.000000000000000 ) ;
#778 = FACE_BOUND ( 'NONE', #115100, .T. ) ;
#779 = ADVANCED_FACE ( 'NONE', ( #84941 ), #16834, .F. ) ;
#780 = ORIENTED_EDGE ( 'NONE', *, *, #73508, .T. ) ;
#781 = DIRECTION ( 'NONE',  ( -0.3543493200069162685, -0.000000000000000000, -0.9351131265310288487 ) ) ;
#782 = CARTESIAN_POINT ( 'NONE',  ( 28.49999999999979750, -7.912538124160673370, 4.000000000000000000 ) ) ;
#783 = LINE ( 'NONE', #90696, #25924 ) ;
#784 = LINE ( 'NONE', #11649, #141109 ) ;
#785 = EDGE_CURVE ( 'NONE', #137573, #33799, #105265, .T. ) ;
#786 = VERTEX_POINT ( 'NONE', #82823 ) ;
#787 = CARTESIAN_POINT ( 'NONE',  ( 31.49999999999979039, 16.46639925780209524, 5.000000000000000000 ) ) ;
#788 = ORIENTED_EDGE ( 'NONE', *, *, #120399, .T. ) ;
#789 = ORIENTED_EDGE ( 'NONE', *, *, #98660, .F. ) ;
#790 = ORIENTED_EDGE ( 'NONE', *, *, #83069, .T. ) ;
#791 = VECTOR ( 'NONE', #14177, 1000.000000000000000 ) ;
#792 = CARTESIAN_POINT ( 'NONE',  ( 43.51626352523143737, -4.472830434245838482, 4.472830434245838482 ) ) ;
#793 = EDGE_CURVE ( 'NONE', #54071, #79781, #96490, .T. ) ;
#795 = ORIENTED_EDGE ( 'NONE', *, *, #34836, .F. ) ;
#794 = VECTOR ( 'NONE', #21386, 999.9999999999998863 ) ;
#796 = EDGE_CURVE ( 'NONE', #61200, #46586, #5914, .T. ) ;
#797 = DIRECTION ( 'NONE',  ( 0.000000000000000000, 0.000000000000000000, -1.000000000000000000 ) ) ;
#798 = CARTESIAN_POINT ( 'NONE',  ( 16.44013779566152778, 4.333342374871280669E-31, 2.500000000000000444 ) ) ;
#799 = ORIENTED_EDGE ( 'NONE', *, *, #62263, .F. ) ;
#800 = CARTESIAN_POINT ( 'NONE',  ( 0.000000000000000000, 9.735942053221458872E-16, -7.950000000000000178 ) ) ;
#801 = CARTESIAN_POINT ( 'NONE',  ( 72.29974487139158157, -27.71228299555256669, 4.000000000000000000 ) ) ;
#802 = VECTOR ( 'NONE', #88315, 1000.000000000000000 ) ;
#803 = EDGE_CURVE ( 'NONE', #32716, #98588, #117541, .T. ) ;
#804 = DIRECTION ( 'NONE',  ( -0.000000000000000000, 0.000000000000000000, 1.000000000000000000 ) ) ;
#805 = CARTESIAN_POINT ( 'NONE',  ( 31.04515773336646944, -21.74070752338406365, 21.72585301388592072 ) ) ;
#806 = CARTESIAN_POINT ( 'NONE',  ( 0.000000000000000000, 0.000000000000000000, 0.000000000000000000 ) ) ;
#807 = CARTESIAN_POINT ( 'NONE',  ( -6.489213562373093325, -27.52281430457059841, 5.000000000000000000 ) ) ;
#808 = CARTESIAN_POINT ( 'NONE',  ( 25.00193056682080339, -22.22500000000000142, 4.500000000000000888 ) ) ;
#809 = ORIENTED_EDGE ( 'NONE', *, *, #143170, .T. ) ;
#810 = ORIENTED_EDGE ( 'NONE', *, *, #109263, .F. ) ;
#812 = ORIENTED_EDGE ( 'NONE', *, *, #97962, .T. ) ;
#811 = AXIS2_PLACEMENT_3D ( 'NONE', #14769, #3844, #59046 ) ;
#813 = ORIENTED_EDGE ( 'NONE', *, *, #115141, .F. ) ;
#814 = CARTESIAN_POINT ( 'NONE',  ( 6.328169399223488867, 8.259292476615634371, 4.000000000000000000 ) ) ;
#815 = CARTESIAN_POINT ( 'NONE',  ( 36.24586038379622011, 3.974999999999996980, 6.884901960086287964 ) ) ;
#816 = VERTEX_POINT ( 'NONE', #50189 ) ;
#817 = ORIENTED_EDGE ( 'NONE', *, *, #106172, .F. ) ;
#818 = PRESENTATION_STYLE_ASSIGNMENT (( #100864 ) ) ;
#819 = PLANE ( 'NONE',  #129599 ) ;
#820 = VECTOR ( 'NONE', #75844, 1000.000000000000227 ) ;
#821 = ORIENTED_EDGE ( 'NONE', *, *, #120338, .F. ) ;
#822 = PLANE ( 'NONE',  #97367 ) ;
#823 = EDGE_CURVE ( 'NONE', #46985, #101990, #30576, .T. ) ;
#824 = DIRECTION ( 'NONE',  ( 0.000000000000000000, -1.000000000000000000, 0.000000000000000000 ) ) ;
#825 = EDGE_CURVE ( 'NONE', #56410, #7821, #8066, .T. ) ;
#826 = CARTESIAN_POINT ( 'NONE',  ( 28.21290314143522338, 3.967499999999992699, -6.871911579029513994 ) ) ;
#827 = CIRCLE ( 'NONE', #47185, 2.500000000000000888 ) ;
#828 = CARTESIAN_POINT ( 'NONE',  ( 42.18398860626899705, 28.73617430169816700, 5.000000000000000000 ) ) ;
#829 = ORIENTED_EDGE ( 'NONE', *, *, #138260, .T. ) ;
#830 = CARTESIAN_POINT ( 'NONE',  ( 108.1204301918981230, 3.055000000000002380, -5.291415217122917625 ) ) ;
#831 = DIRECTION ( 'NONE',  ( -0.7071067811865487940, 0.7071067811865463515, -0.000000000000000000 ) ) ;
#832 = DIRECTION ( 'NONE',  ( 0.000000000000000000, 0.000000000000000000, 1.000000000000000000 ) ) ;
#833 = CARTESIAN_POINT ( 'NONE',  ( 19.05000000000000071, 3.174999999999997158, 5.000000000000000000 ) ) ;
#835 = EDGE_LOOP ( 'NONE', ( #4036, #48798, #131663, #1006 ) ) ;
#834 = CARTESIAN_POINT ( 'NONE',  ( 28.49999999999979750, -15.29013452822852237, 0.3645803511611025449 ) ) ;
#836 = PLANE ( 'NONE',  #18546 ) ;
#837 = ORIENTED_EDGE ( 'NONE', *, *, #122262, .F. ) ;
#838 = SURFACE_STYLE_FILL_AREA ( #111022 ) ;
#839 = EDGE_CURVE ( 'NONE', #86454, #58696, #17530, .T. ) ;
#840 = CARTESIAN_POINT ( 'NONE',  ( -34.44665057663196706, 2.259292476615694323, 14.86850063742362416 ) ) ;
#841 = CARTESIAN_POINT ( 'NONE',  ( 121.4583333333333286, 3.974999999999997424, 6.884901960086288852 ) ) ;
#842 = ORIENTED_EDGE ( 'NONE', *, *, #139986, .F. ) ;
#843 = DIRECTION ( 'NONE',  ( 0.3543493200069162685, -0.000000000000000000, -0.9351131265310288487 ) ) ;
#844 = CARTESIAN_POINT ( 'NONE',  ( -6.938893903907228378E-15, 20.58746187583904330, 4.000000000000000000 ) ) ;
#845 = DIRECTION ( 'NONE',  ( 1.000000000000000000, 0.000000000000000000, 0.000000000000000000 ) ) ;
#846 = ORIENTED_EDGE ( 'NONE', *, *, #78356, .T. ) ;
#847 = CARTESIAN_POINT ( 'NONE',  ( 32.99451991528749062, 28.92564299267960948, 4.000000000000000000 ) ) ;
#848 = ORIENTED_EDGE ( 'NONE', *, *, #124268, .F. ) ;
#849 = CARTESIAN_POINT ( 'NONE',  ( 6.540657738503846907, 4.202752102959690472E-16, 0.000000000000000000 ) ) ;
#851 = ORIENTED_EDGE ( 'NONE', *, *, #93238, .F. ) ;
#850 = DIRECTION ( 'NONE',  ( 0.000000000000000000, 1.000000000000000000, 0.000000000000000000 ) ) ;
#852 = ORIENTED_EDGE ( 'NONE', *, *, #6267, .F. ) ;
#853 = CARTESIAN_POINT ( 'NONE',  ( 18.91358171146897860, 2.162374846302510090, -30.33482670853117114 ) ) ;
#854 = CARTESIAN_POINT ( 'NONE',  ( -4.499999999999964473, 15.05218569542901896, 5.000000000000000000 ) ) ;
#855 = AXIS2_PLACEMENT_3D ( 'NONE', #36138, #25231, #66792 ) ;
#856 = EDGE_LOOP ( 'NONE', ( #106789, #129484, #94059, #133606 ) ) ;
#857 = CARTESIAN_POINT ( 'NONE',  ( -9.299744871391588674, -27.71228299555212971, 4.000000000000000000 ) ) ;
#858 = STYLED_ITEM ( 'NONE', ( #106410 ), #103236 ) ;
#859 =( NAMED_UNIT ( * ) SI_UNIT ( $, .STERADIAN. ) SOLID_ANGLE_UNIT ( ) );
#860 = FACE_OUTER_BOUND ( 'NONE', #101516, .T. ) ;
#861 = VERTEX_POINT ( 'NONE', #127749 ) ;
#862 = PLANE ( 'NONE',  #42020 ) ;
#863 = EDGE_CURVE ( 'NONE', #97217, #125896, #73846, .T. ) ;
#864 = CARTESIAN_POINT ( 'NONE',  ( -19.05499999999999972, 3.130000000000007887, -23.88381690219165776 ) ) ;
#865 = DIRECTION ( 'NONE',  ( 0.000000000000000000, 1.000000000000000000, 0.000000000000000000 ) ) ;
#866 = DIRECTION ( 'NONE',  ( 1.000000000000000000, 0.000000000000000000, 0.000000000000000000 ) ) ;
#867 = CARTESIAN_POINT ( 'NONE',  ( 28.78709685856477307, 3.054999999999997939, 5.291415217122920289 ) ) ;
#868 = VECTOR ( 'NONE', #41498, 1000.000000000000000 ) ;
#869 = LINE ( 'NONE', #110344, #72055 ) ;
#870 = ORIENTED_EDGE ( 'NONE', *, *, #140608, .T. ) ;
#871 = VERTEX_POINT ( 'NONE', #73375 ) ;
#872 = FACE_OUTER_BOUND ( 'NONE', #17850, .T. ) ;
#873 = VECTOR ( 'NONE', #62404, 1000.000000000000000 ) ;
#874 = VERTEX_POINT ( 'NONE', #18217 ) ;
#875 = EDGE_LOOP ( 'NONE', ( #85490, #63150, #94760, #112992 ) ) ;
#876 = DIRECTION ( 'NONE',  ( -0.6830127018922180770, -0.6830127018922204085, -0.2588190451025213501 ) ) ;
#877 = DIRECTION ( 'NONE',  ( -0.7071067811865486830, -0.7071067811865464625, 0.000000000000000000 ) ) ;
#878 = VERTEX_POINT ( 'NONE', #7356 ) ;
#879 = LINE ( 'NONE', #98087, #27716 ) ;
#881 = AXIS2_PLACEMENT_3D ( 'NONE', #49592, #61883, #40145 ) ;
#880 = CARTESIAN_POINT ( 'NONE',  ( -24.64327148205084583, 5.259292476615665457, 4.831541298974430632 ) ) ;
#882 = EDGE_CURVE ( 'NONE', #47009, #105119, #51619, .T. ) ;
#883 = CARTESIAN_POINT ( 'NONE',  ( 11.99451991528749417, 28.92564299267946382, 4.000000000000000000 ) ) ;
#884 =( GEOMETRIC_REPRESENTATION_CONTEXT ( 3 ) GLOBAL_UNCERTAINTY_ASSIGNED_CONTEXT ( ( #102893 ) ) GLOBAL_UNIT_ASSIGNED_CONTEXT ( ( #116752, #2986, #47280 ) ) REPRESENTATION_CONTEXT ( 'NONE', 'WORKASPACE' ) );
#885 = PLANE ( 'NONE',  #21022 ) ;
#886 = CARTESIAN_POINT ( 'NONE',  ( 121.9170968585647756, 3.054999999999998828, 5.291415217122922066 ) ) ;
#887 = EDGE_CURVE ( 'NONE', #116708, #16533, #74072, .T. ) ;
#888 = EDGE_LOOP ( 'NONE', ( #37870, #14350, #70171, #3435 ) ) ;
#889 = DIRECTION ( 'NONE',  ( 0.3543493200069162685, -0.000000000000000000, -0.9351131265310288487 ) ) ;
#890 = DIRECTION ( 'NONE',  ( -0.7071067811865487940, 0.7071067811865463515, -0.000000000000000000 ) ) ;
#891 = CARTESIAN_POINT ( 'NONE',  ( 3.328169399223502189, -0.7407075233842770334, 4.000000000000000000 ) ) ;
#892 = CARTESIAN_POINT ( 'NONE',  ( 1.342642840338568844, 0.4167709042101988004, 6.752357159661401376 ) ) ;
#893 = DIRECTION ( 'NONE',  ( -0.7071067811865486830, -0.7071067811865464625, 0.000000000000000000 ) ) ;
#894 = LINE ( 'NONE', #90057, #81597 ) ;
#895 = CARTESIAN_POINT ( 'NONE',  ( 29.99999999999979039, 19.55218569542897100, 5.000000000000000000 ) ) ;
#897 = EDGE_CURVE ( 'NONE', #127404, #117376, #22499, .T. ) ;
#896 = AXIS2_PLACEMENT_3D ( 'NONE', #142068, #78228, #86951 ) ;
#899 = EDGE_CURVE ( 'NONE', #138853, #137586, #132029, .T. ) ;
#898 = CARTESIAN_POINT ( 'NONE',  ( 46.16252705046289151, 7.949999999999998401, 1.460391307983218338E-15 ) ) ;
#900 = LINE ( 'NONE', #79251, #9697 ) ;
#901 = CONICAL_SURFACE ( 'NONE', #118993, 2.500000000000000888, 0.9599310885968822538 ) ;
#902 = DIRECTION ( 'NONE',  ( -0.6830127018922180770, -0.6830127018922204085, -0.2588190451025213501 ) ) ;
#903 = VERTEX_POINT ( 'NONE', #43575 ) ;
#904 = ORIENTED_EDGE ( 'NONE', *, *, #70082, .F. ) ;
#905 = CARTESIAN_POINT ( 'NONE',  ( 46.64583333333332860, 2.130196079827431976, -7.949999999999999289 ) ) ;
#906 = ADVANCED_FACE ( 'NONE', ( #78353 ), #97204, .F. ) ;
#907 = CARTESIAN_POINT ( 'NONE',  ( -4.171830600776438303, 12.75929247661558996, 4.000000000000000000 ) ) ;
#908 = VECTOR ( 'NONE', #57091, 1000.000000000000000 ) ;
#909 = CARTESIAN_POINT ( 'NONE',  ( -53.99451991528749062, 28.92564299267975869, 4.000000000000000000 ) ) ;
#910 = ORIENTED_EDGE ( 'NONE', *, *, #110228, .T. ) ;
#911 = CARTESIAN_POINT ( 'NONE',  ( 24.29974487139158867, -27.71228299555223273, 4.000000000000000000 ) ) ;
#912 = LINE ( 'NONE', #136435, #70053 ) ;
#913 = EDGE_CURVE ( 'NONE', #62294, #141092, #53006, .T. ) ;
#914 = CARTESIAN_POINT ( 'NONE',  ( 37.91709685856477563, 3.054999999999998828, 5.291415217122922066 ) ) ;
#915 = ORIENTED_EDGE ( 'NONE', *, *, #126095, .T. ) ;
#916 = LINE ( 'NONE', #134326, #80419 ) ;
#917 = EDGE_LOOP ( 'NONE', ( #64120, #140955, #26192, #20102 ) ) ;
#918 = ORIENTED_EDGE ( 'NONE', *, *, #46748, .T. ) ;
#919 = VECTOR ( 'NONE', #125330, 1000.000000000000227 ) ;
#920 = DIRECTION ( 'NONE',  ( 0.6830127018922181881, 0.6830127018922202975, -0.2588190451025214056 ) ) ;
#921 = EDGE_CURVE ( 'NONE', #50789, #60934, #87792, .T. ) ;
#922 = CARTESIAN_POINT ( 'NONE',  ( -19.26506670282039480, 12.75929247661558286, 18.34774599283960939 ) ) ;
#923 = LINE ( 'NONE', #188, #18886 ) ;
#924 = LINE ( 'NONE', #11071, #53375 ) ;
#925 = VERTEX_POINT ( 'NONE', #89230 ) ;
#926 = DIRECTION ( 'NONE',  ( 0.7071067811865486830, -0.7071067811865464625, -0.000000000000000000 ) ) ;
#927 = VERTEX_POINT ( 'NONE', #10911 ) ;
#928 = DIRECTION ( 'NONE',  ( 0.3543493200069162685, -0.000000000000000000, -0.9351131265310288487 ) ) ;
#929 = PLANE ( 'NONE',  #64783 ) ;
#930 = SURFACE_STYLE_FILL_AREA ( #10384 ) ;
#931 = ADVANCED_FACE ( 'NONE', ( #33454 ), #110230, .F. ) ;
#932 = DIRECTION ( 'NONE',  ( -0.7071067811865487940, 0.7071067811865463515, 0.000000000000000000 ) ) ;
#933 = CARTESIAN_POINT ( 'NONE',  ( 14.81601139373099585, 28.73617430169776910, 5.000000000000000000 ) ) ;
#934 = ORIENTED_EDGE ( 'NONE', *, *, #89062, .F. ) ;
#935 = VECTOR ( 'NONE', #129209, 1000.000000000000000 ) ;
#936 = CARTESIAN_POINT ( 'NONE',  ( 26.99451991528749417, 28.92564299267956685, 4.000000000000000000 ) ) ;
#937 = CARTESIAN_POINT ( 'NONE',  ( 60.43293019189810877, 1.637169565754156508, 6.110000000000000320 ) ) ;
#938 = DIRECTION ( 'NONE',  ( 1.000000000000000000, 1.224606353822377258E-16, 0.000000000000000000 ) ) ;
#939 = ADVANCED_FACE ( 'NONE', ( #54479 ), #21, .F. ) ;
#940 = PLANE ( 'NONE',  #105606 ) ;
#941 = LINE ( 'NONE', #78536, #36402 ) ;
#942 = VERTEX_POINT ( 'NONE', #42174 ) ;
#943 = DIRECTION ( 'NONE',  ( -1.000000000000000000, -1.224606353822377258E-16, -0.000000000000000000 ) ) ;
#944 = CARTESIAN_POINT ( 'NONE',  ( 0.000000000000000000, 0.000000000000000000, 0.000000000000000000 ) ) ;
#945 = ORIENTED_EDGE ( 'NONE', *, *, #128368, .F. ) ;
#946 = AXIS2_PLACEMENT_3D ( 'NONE', #78392, #9523, #76993 ) ;
#947 = EDGE_CURVE ( 'NONE', #4808, #99520, #20373, .T. ) ;
#948 = CARTESIAN_POINT ( 'NONE',  ( 60.48921356237309510, -27.52281430457097500, 5.000000000000000000 ) ) ;
#950 = ADVANCED_FACE ( 'NONE', ( #53763 ), #142200, .F. ) ;
#949 = VERTEX_POINT ( 'NONE', #75501 ) ;
#951 = CARTESIAN_POINT ( 'NONE',  ( -27.18398860626900060, 28.73617430169806042, 5.000000000000000000 ) ) ;
#952 = CARTESIAN_POINT ( 'NONE',  ( -36.33010218547242687, 17.25929247661553845, 19.83885114516079895 ) ) ;
#953 = PLANE ( 'NONE',  #143468 ) ;
#954 = EDGE_CURVE ( 'NONE', #76142, #77634, #11622, .T. ) ;
#955 = DIRECTION ( 'NONE',  ( -0.7071067811865487940, 0.7071067811865463515, -0.000000000000000000 ) ) ;
#956 = FACE_BOUND ( 'NONE', #109790, .T. ) ;
#957 = CARTESIAN_POINT ( 'NONE',  ( -18.32816939922339472, 17.25929247661555266, 4.000000000000000000 ) ) ;
#958 = CARTESIAN_POINT ( 'NONE',  ( -25.49999999999980815, 19.08746187583905041, 4.000000000000000000 ) ) ;
#959 = DIRECTION ( 'NONE',  ( 0.7071067811865486830, -0.7071067811865464625, -0.000000000000000000 ) ) ;
#960 = LINE ( 'NONE', #45242, #101382 ) ;
#962 = VERTEX_POINT ( 'NONE', #65363 ) ;
#961 = CARTESIAN_POINT ( 'NONE',  ( 32.67183060077624646, -9.740707523384177335, 4.000000000000000000 ) ) ;
#963 = VECTOR ( 'NONE', #101921, 999.9999999999998863 ) ;
#964 = DIRECTION ( 'NONE',  ( 0.000000000000000000, -1.000000000000000000, 0.000000000000000000 ) ) ;
#965 = ORIENTED_EDGE ( 'NONE', *, *, #26029, .T. ) ;
#966 = CIRCLE ( 'NONE', #12566, 2.500000000000000444 ) ;
#967 = VERTEX_POINT ( 'NONE', #46478 ) ;
#968 = CARTESIAN_POINT ( 'NONE',  ( 78.22459685856478018, -1.637169565754160949, 6.109999999999997655 ) ) ;
#969 = ORIENTED_EDGE ( 'NONE', *, *, #96607, .F. ) ;
#970 = EDGE_CURVE ( 'NONE', #139596, #73106, #81223, .T. ) ;
#971 = LINE ( 'NONE', #136494, #120723 ) ;
#972 = AXIS2_PLACEMENT_3D ( 'NONE', #58558, #82405, #14972 ) ;
#973 = ORIENTED_EDGE ( 'NONE', *, *, #18277, .T. ) ;
#974 = CARTESIAN_POINT ( 'NONE',  ( 48.48921356237309510, -27.52281430457089328, 5.000000000000000000 ) ) ;
#975 = ADVANCED_FACE ( 'NONE', ( #25374 ), #2165, .F. ) ;
#976 = CARTESIAN_POINT ( 'NONE',  ( 30.75860074219774631, 21.72500000000000142, 5.000000000000000000 ) ) ;
#977 = DIRECTION ( 'NONE',  ( 0.7071067811865486830, -0.7071067811865464625, -0.000000000000000000 ) ) ;
#978 = CARTESIAN_POINT ( 'NONE',  ( -24.58521188482543707, 5.410383847852841654, 4.279600586820024866 ) ) ;
#979 = AXIS2_PLACEMENT_3D ( 'NONE', #54919, #23698, #67968 ) ;
#980 = PLANE ( 'NONE',  #69093 ) ;
#982 = CARTESIAN_POINT ( 'NONE',  ( -19.05499999999999261, 3.130000000000007887, -22.35000000000000142 ) ) ;
#981 = CARTESIAN_POINT ( 'NONE',  ( 25.17183060077629619, -5.240707523384228850, 4.000000000000000000 ) ) ;
#983 = CARTESIAN_POINT ( 'NONE',  ( 23.48334561358938899, 22.22500000000000142, 4.500000000000000888 ) ) ;
#984 = CARTESIAN_POINT ( 'NONE',  ( -3.793339364578453665, 21.75929247661549581, 4.998822639870701856 ) ) ;
#985 = EDGE_LOOP ( 'NONE', ( #90250, #83405, #138439, #103289, #3325 ) ) ;
#986 = EDGE_LOOP ( 'NONE', ( #37723, #6916, #143545, #49162 ) ) ;
#987 = CARTESIAN_POINT ( 'NONE',  ( 0.000000000000000000, 21.72500000000000142, 4.500000000000000888 ) ) ;
#988 = EDGE_LOOP ( 'NONE', ( #94299, #71, #52780 ) ) ;
#989 = ORIENTED_EDGE ( 'NONE', *, *, #103086, .T. ) ;
#990 = ORIENTED_EDGE ( 'NONE', *, *, #78179, .T. ) ;
#991 = AXIS2_PLACEMENT_3D ( 'NONE', #6512, #50791, #39948 ) ;
#992 = CARTESIAN_POINT ( 'NONE',  ( 29.02126352523143282, -4.472830434245838482, -4.472830434245840259 ) ) ;
#993 = ORIENTED_EDGE ( 'NONE', *, *, #103380, .F. ) ;
#994 = LINE ( 'NONE', #45278, #55610 ) ;
#995 = VECTOR ( 'NONE', #112974, 1000.000000000000000 ) ;
#996 = ADVANCED_FACE ( 'NONE', ( #67502 ), #80504, .F. ) ;
#997 = DIRECTION ( 'NONE',  ( -0.6830127018922181881, 0.6830127018922202975, -0.2588190451025214056 ) ) ;
#998 = CARTESIAN_POINT ( 'NONE',  ( 31.98330628287044064, 6.094999999999991758, 1.633150327867687102 ) ) ;
#999 = AXIS2_PLACEMENT_3D ( 'NONE', #25284, #70964, #126056 ) ;
#1000 = FACE_OUTER_BOUND ( 'NONE', #61432, .T. ) ;
#1001 = EDGE_LOOP ( 'NONE', ( #109061, #123159, #101143, #113750, #111956 ) ) ;
#1002 = LINE ( 'NONE', #133691, #29483 ) ;
#1003 = DIRECTION ( 'NONE',  ( 0.3543493200069162685, -0.000000000000000000, -0.9351131265310288487 ) ) ;
#1004 = LINE ( 'NONE', #111193, #49798 ) ;
#1006 = ORIENTED_EDGE ( 'NONE', *, *, #101122, .T. ) ;
#1005 = LINE ( 'NONE', #89461, #79703 ) ;
#1007 = ORIENTED_EDGE ( 'NONE', *, *, #135968, .F. ) ;
#1008 = CARTESIAN_POINT ( 'NONE',  ( 63.18398860626900415, 28.73617430169831621, 5.000000000000000000 ) ) ;
#1009 = EDGE_CURVE ( 'NONE', #4395, #106598, #120848, .T. ) ;
#1010 = CYLINDRICAL_SURFACE ( 'NONE', #88540, 0.5000000000000004441 ) ;
#1011 = LINE ( 'NONE', #34383, #58711 ) ;
#1012 = EDGE_LOOP ( 'NONE', ( #39573, #92186, #49527, #55324 ) ) ;
#1013 = VECTOR ( 'NONE', #57020, 1000.000000000000000 ) ;
#1014 = DIRECTION ( 'NONE',  ( -0.6830127018922181881, 0.6830127018922202975, -0.2588190451025214056 ) ) ;
#1015 = DIRECTION ( 'NONE',  ( -0.000000000000000000, -0.3543493200069152693, 0.9351131265310292928 ) ) ;
#1016 = VERTEX_POINT ( 'NONE', #25940 ) ;
#1017 = LINE ( 'NONE', #45298, #81912 ) ;
#1018 = CARTESIAN_POINT ( 'NONE',  ( 27.97916666666666430, -7.950000000000000178, 2.130196079827424427 ) ) ;
#1019 = CARTESIAN_POINT ( 'NONE',  ( -63.48921356237309510, -27.52281430457099631, 5.000000000000000000 ) ) ;
#1020 = LINE ( 'NONE', #113357, #141104 ) ;
#1021 = LINE ( 'NONE', #64172, #109457 ) ;
#1022 = CARTESIAN_POINT ( 'NONE',  ( -50.99451991528749062, 28.92564299267973738, 4.000000000000000000 ) ) ;
#1023 = DIRECTION ( 'NONE',  ( -0.000000000000000000, -0.3543493200069152693, 0.9351131265310292928 ) ) ;
#1024 = LINE ( 'NONE', #33702, #103879 ) ;
#1025 = ORIENTED_EDGE ( 'NONE', *, *, #18427, .F. ) ;
#1026 = ORIENTED_EDGE ( 'NONE', *, *, #86562, .F. ) ;
#1027 = CARTESIAN_POINT ( 'NONE',  ( 34.92500000000001847, -3.269999999999991580, -36.39086428169088094 ) ) ;
#1028 = PRESENTATION_STYLE_ASSIGNMENT (( #46764 ) ) ;
#1029 = DIRECTION ( 'NONE',  ( 0.3543493200069163240, 0.000000000000000000, 0.9351131265310288487 ) ) ;
#1030 = ORIENTED_EDGE ( 'NONE', *, *, #40797, .F. ) ;
#1031 = CARTESIAN_POINT ( 'NONE',  ( -20.99999999999985079, 7.007997736742429318, -8.085015511992160953 ) ) ;
#1032 = FACE_OUTER_BOUND ( 'NONE', #54625, .T. ) ;
#1033 = LINE ( 'NONE', #80087, #118514 ) ;
#1034 = ORIENTED_EDGE ( 'NONE', *, *, #129908, .T. ) ;
#1035 = DIRECTION ( 'NONE',  ( -0.000000000000000000, 1.000000000000000000, -0.000000000000000000 ) ) ;
#1036 = CARTESIAN_POINT ( 'NONE',  ( 112.4166666666666714, -6.884901960086287076, -3.975000000000000977 ) ) ;
#1037 = CARTESIAN_POINT ( 'NONE',  ( 7.014532492589830248, 3.821174125832445049E-16, 0.000000000000000000 ) ) ;
#1038 = LINE ( 'NONE', #56212, #15794 ) ;
#1039 = CARTESIAN_POINT ( 'NONE',  ( 54.74543019189812298, -5.291415217122919401, -3.055000000000000604 ) ) ;
#1040 = VECTOR ( 'NONE', #97058, 1000.000000000000227 ) ;
#1041 = DIRECTION ( 'NONE',  ( 0.3543493200069163240, -0.000000000000000000, 0.9351131265310288487 ) ) ;
#1042 = CARTESIAN_POINT ( 'NONE',  ( 3.005480084712505828, 28.92564299267936079, 4.000000000000000000 ) ) ;
#1043 =( NAMED_UNIT ( * ) SI_UNIT ( $, .STERADIAN. ) SOLID_ANGLE_UNIT ( ) );
#1044 = CARTESIAN_POINT ( 'NONE',  ( 19.49999999999987566, -14.94781430457067550, 5.000000000000000000 ) ) ;
#1045 = ORIENTED_EDGE ( 'NONE', *, *, #27467, .F. ) ;
#1046 = CARTESIAN_POINT ( 'NONE',  ( 0.000000000000000000, 60.00000000000000000, 0.000000000000000000 ) ) ;
#1047 = ADVANCED_FACE ( 'NONE', ( #70206 ), #15713, .F. ) ;
#1048 = ORIENTED_EDGE ( 'NONE', *, *, #119704, .T. ) ;
#1049 = LINE ( 'NONE', #80102, #117244 ) ;
#1050 = CARTESIAN_POINT ( 'NONE',  ( -54.29974487139159578, -27.71228299555243879, 4.000000000000000000 ) ) ;
#1051 = LINE ( 'NONE', #135198, #53564 ) ;
#1052 = CARTESIAN_POINT ( 'NONE',  ( 29.99451991528749417, 28.92564299267958816, 4.000000000000000000 ) ) ;
#1053 = CARTESIAN_POINT ( 'NONE',  ( 26.29289321881327623, -12.74070752338415247, 5.000000000000000000 ) ) ;
#1054 = CARTESIAN_POINT ( 'NONE',  ( -16.26506670282041611, 12.75929247661558996, 18.34774599283960228 ) ) ;
#1055 = ADVANCED_FACE ( 'NONE', ( #60005 ), #28802, .F. ) ;
#1056 = ADVANCED_FACE ( 'NONE', ( #50539 ), #4109, .F. ) ;
#1057 = ORIENTED_EDGE ( 'NONE', *, *, #123182, .T. ) ;
#1058 = VERTEX_POINT ( 'NONE', #38245 ) ;
#1059 = FACE_OUTER_BOUND ( 'NONE', #79286, .T. ) ;
#1060 = PLANE ( 'NONE',  #79155 ) ;
#1061 = UNCERTAINTY_MEASURE_WITH_UNIT (LENGTH_MEASURE( 1.000000000000000082E-05 ), #107553, 'distance_accuracy_value', 'NONE');
#1062 = CIRCLE ( 'NONE', #24171, 9.524999999999991473 ) ;
#1063 = CARTESIAN_POINT ( 'NONE',  ( 56.99451991528749062, 28.92564299267978001, 4.000000000000000000 ) ) ;
#1064 = DIRECTION ( 'NONE',  ( -0.7071067811865486830, -0.7071067811865464625, 0.000000000000000000 ) ) ;
#1065 = ADVANCED_FACE ( 'NONE', ( #127376 ), #94729, .F. ) ;
#1067 = ADVANCED_FACE ( 'NONE', ( #115751 ), #138990, .F. ) ;
#1066 = CARTESIAN_POINT ( 'NONE',  ( 71.82919371712957002, -3.975000000000001865, 6.884901960086284411 ) ) ;
#1068 = DIRECTION ( 'NONE',  ( 0.000000000000000000, 0.000000000000000000, 1.000000000000000000 ) ) ;
#1069 = VECTOR ( 'NONE', #17496, 1000.000000000000000 ) ;
#1070 = CARTESIAN_POINT ( 'NONE',  ( 0.000000000000000000, 0.000000000000000000, 5.000000000000000000 ) ) ;
#1071 = ORIENTED_EDGE ( 'NONE', *, *, #45808, .T. ) ;
#1072 = CARTESIAN_POINT ( 'NONE',  ( 77.27083333333332860, -7.949999999999999289, -2.130196079827426203 ) ) ;
#1073 = PLANE ( 'NONE',  #60902 ) ;
#1074 = VECTOR ( 'NONE', #110538, 1000.000000000000000 ) ;
#1075 = ADVANCED_FACE ( 'NONE', ( #137562 ), #126651, .T. ) ;
#1076 = DIRECTION ( 'NONE',  ( -0.6830127018922181881, 0.6830127018922202975, -0.2588190451025214056 ) ) ;
#1077 = PLANE ( 'NONE',  #133101 ) ;
#1078 = EDGE_CURVE ( 'NONE', #140410, #98076, #28075, .T. ) ;
#1079 = ORIENTED_EDGE ( 'NONE', *, *, #104038, .F. ) ;
#1080 = FACE_OUTER_BOUND ( 'NONE', #114828, .T. ) ;
#1081 = ADVANCED_FACE ( 'NONE', ( #116511 ), #71589, .F. ) ;
#1082 = AXIS2_PLACEMENT_3D ( 'NONE', #48681, #26916, #84193 ) ;
#1083 = FACE_OUTER_BOUND ( 'NONE', #126972, .T. ) ;
#1084 = CARTESIAN_POINT ( 'NONE',  ( 66.79209685856477563, -5.291415217122921177, 3.054999999999999272 ) ) ;
#1085 = VERTEX_POINT ( 'NONE', #128116 ) ;
#1086 = VERTEX_POINT ( 'NONE', #17198 ) ;
#1087 = DIRECTION ( 'NONE',  ( 0.6830127018922180770, -0.6830127018922204085, -0.2588190451025213501 ) ) ;
#1088 = CARTESIAN_POINT ( 'NONE',  ( 41.99451991528749062, 28.92564299267967343, 4.000000000000000000 ) ) ;
#1089 = EDGE_CURVE ( 'NONE', #138081, #131497, #61458, .T. ) ;
#1090 = DIRECTION ( 'NONE',  ( -1.000000000000000000, -0.000000000000000000, 0.000000000000000000 ) ) ;
#1091 = CARTESIAN_POINT ( 'NONE',  ( 43.00000000000000000, 0.000000000000000000, -7.950000000000000178 ) ) ;
#1092 = PLANE ( 'NONE',  #99515 ) ;
#1094 = ORIENTED_EDGE ( 'NONE', *, *, #50202, .T. ) ;
#1093 = CARTESIAN_POINT ( 'NONE',  ( 34.49999999999975842, -2.945670655169024155, 4.994342998332159667 ) ) ;
#1095 = DIRECTION ( 'NONE',  ( 0.000000000000000000, 0.000000000000000000, 1.000000000000000000 ) ) ;
#1096 = CARTESIAN_POINT ( 'NONE',  ( 6.160000000000001030, 9.521314400968980422E-16, 0.000000000000000000 ) ) ;
#1097 = DIRECTION ( 'NONE',  ( -0.3543493200069163240, -0.000000000000000000, 0.9351131265310288487 ) ) ;
#1098 = EDGE_CURVE ( 'NONE', #125503, #115328, #46246, .T. ) ;
#1099 = DIRECTION ( 'NONE',  ( 1.000000000000000000, 0.000000000000000000, 0.000000000000000000 ) ) ;
#1100 = ORIENTED_EDGE ( 'NONE', *, *, #136821, .F. ) ;
#1101 = CIRCLE ( 'NONE', #47540, 2.552699999999990865 ) ;
#1102 = ORIENTED_EDGE ( 'NONE', *, *, #130845, .F. ) ;
#1103 = CARTESIAN_POINT ( 'NONE',  ( 68.54209685856477563, 5.291415217122923842, -3.054999999999996163 ) ) ;
#1104 = AXIS2_PLACEMENT_3D ( 'NONE', #64324, #62193, #96206 ) ;
#1105 = ORIENTED_EDGE ( 'NONE', *, *, #121183, .T. ) ;
#1106 = AXIS2_PLACEMENT_3D ( 'NONE', #54858, #8428, #9135 ) ;
#1107 = DIRECTION ( 'NONE',  ( -0.7071067811865486830, -0.7071067811865464625, -0.000000000000000000 ) ) ;
#1108 = FACE_OUTER_BOUND ( 'NONE', #128603, .T. ) ;
#1109 = DIRECTION ( 'NONE',  ( -0.000000000000000000, -0.000000000000000000, 1.000000000000000000 ) ) ;
#1110 = EDGE_CURVE ( 'NONE', #9952, #4761, #29480, .T. ) ;
#1111 = LINE ( 'NONE', #12710, #57346 ) ;
#1112 = DIRECTION ( 'NONE',  ( -0.7071067811865486830, -0.7071067811865464625, 0.000000000000000000 ) ) ;
#1113 = EDGE_LOOP ( 'NONE', ( #101021, #24489, #97914, #30059 ) ) ;
#1114 = ORIENTED_EDGE ( 'NONE', *, *, #50311, .F. ) ;
#1115 = CARTESIAN_POINT ( 'NONE',  ( -63.29974487139158867, -27.71228299555250274, 4.000000000000000000 ) ) ;
#1116 = SURFACE_STYLE_FILL_AREA ( #111312 ) ;
#1117 = ADVANCED_FACE ( 'NONE', ( #106305 ), #51266, .F. ) ;
#1118 = ORIENTED_EDGE ( 'NONE', *, *, #19224, .F. ) ;
#1119 = DIRECTION ( 'NONE',  ( -0.000000000000000000, 1.000000000000000000, -0.000000000000000000 ) ) ;
#1120 = EDGE_CURVE ( 'NONE', #69887, #22434, #79304, .T. ) ;
#1121 = LINE ( 'NONE', #45399, #73463 ) ;
#1122 = DIRECTION ( 'NONE',  ( -0.7071067811865487940, 0.7071067811865463515, -0.000000000000000000 ) ) ;
#1123 = ADVANCED_FACE ( 'NONE', ( #22000 ), #44524, .T. ) ;
#1124 = ORIENTED_EDGE ( 'NONE', *, *, #37881, .T. ) ;
#1125 = ADVANCED_FACE ( 'NONE', ( #66956 ), #107052, .F. ) ;
#1126 = FACE_BOUND ( 'NONE', #89379, .T. ) ;
#1127 = LINE ( 'NONE', #2551, #131276 ) ;
#1128 = LINE ( 'NONE', #134546, #37408 ) ;
#1129 = CARTESIAN_POINT ( 'NONE',  ( 36.53752705046288440, -9.735942053221456900E-16, 7.949999999999998401 ) ) ;
#1130 = DIRECTION ( 'NONE',  ( -0.6830127018922181881, 0.6830127018922202975, -0.2588190451025214056 ) ) ;
#1131 = CARTESIAN_POINT ( 'NONE',  ( -34.82816939922327748, 9.759292476615621936, 4.000000000000000000 ) ) ;
#1132 = DIRECTION ( 'NONE',  ( -1.000000000000000000, 6.798155367234455277E-33, 1.132120292052417344E-48 ) ) ;
#1133 = ORIENTED_EDGE ( 'NONE', *, *, #19224, .T. ) ;
#1134 = ORIENTED_EDGE ( 'NONE', *, *, #138991, .T. ) ;
#1135 = CARTESIAN_POINT ( 'NONE',  ( 101.8495968585647802, 6.109999999999996767, 1.637169565754163836 ) ) ;
#1136 = ORIENTED_EDGE ( 'NONE', *, *, #74828, .F. ) ;
#1137 = EDGE_CURVE ( 'NONE', #131909, #97989, #100301, .T. ) ;
#1138 = DIRECTION ( 'NONE',  ( -0.000000000000000000, 0.000000000000000000, 1.000000000000000000 ) ) ;
#1139 = EDGE_LOOP ( 'NONE', ( #35677, #126554, #84697, #96997 ) ) ;
#1140 = DIRECTION ( 'NONE',  ( -0.7071067811865486830, 0.7071067811865464625, 0.000000000000000000 ) ) ;
#1141 = CARTESIAN_POINT ( 'NONE',  ( 4.420806282870438864, 3.047499999999997655, 5.278424836066143655 ) ) ;
#1142 = CARTESIAN_POINT ( 'NONE',  ( 5.994519915287488843, 28.92564299267942118, 4.000000000000000000 ) ) ;
#1143 = ORIENTED_EDGE ( 'NONE', *, *, #103846, .T. ) ;
#1144 = CARTESIAN_POINT ( 'NONE',  ( -10.49999999999991829, 19.46639925780206326, 5.000000000000000000 ) ) ;
#1145 = CARTESIAN_POINT ( 'NONE',  ( 59.99451991528749772, 28.92564299267980132, 4.000000000000000000 ) ) ;
#1146 = PLANE ( 'NONE',  #66295 ) ;
#1148 = CARTESIAN_POINT ( 'NONE',  ( -24.18398860626899705, 28.73617430169804265, 5.000000000000000000 ) ) ;
#1147 = CARTESIAN_POINT ( 'NONE',  ( 18.18398860626898994, 28.73617430169800002, 5.000000000000000000 ) ) ;
#1149 = CARTESIAN_POINT ( 'NONE',  ( 34.42499999999998295, 22.22500000000000142, 5.000000000000000000 ) ) ;
#1150 = DIRECTION ( 'NONE',  ( -1.000000000000000000, -1.224606353822377258E-16, -0.000000000000000000 ) ) ;
#1151 = ORIENTED_EDGE ( 'NONE', *, *, #3377, .T. ) ;
#1152 = CARTESIAN_POINT ( 'NONE',  ( 18.63425672184678916, 2.500000000000000888, 0.000000000000000000 ) ) ;
#1153 = CARTESIAN_POINT ( 'NONE',  ( 50.99451991528749062, 28.92564299267973738, 4.000000000000000000 ) ) ;
#1154 = ORIENTED_EDGE ( 'NONE', *, *, #33420, .T. ) ;
#1155 = ADVANCED_FACE ( 'NONE', ( #51979 ), #953, .F. ) ;
#1156 = VERTEX_POINT ( 'NONE', #67705 ) ;
#1157 = ORIENTED_EDGE ( 'NONE', *, *, #68554, .T. ) ;
#1158 = CARTESIAN_POINT ( 'NONE',  ( 51.18793019189810423, 6.110000000000002984, -1.637169565754156730 ) ) ;
#1159 = ORIENTED_EDGE ( 'NONE', *, *, #141206, .T. ) ;
#1160 = LINE ( 'NONE', #21523, #62927 ) ;
#1161 = VECTOR ( 'NONE', #121622, 1000.000000000000000 ) ;
#1162 = EDGE_CURVE ( 'NONE', #123801, #89060, #111889, .T. ) ;
#1163 = CARTESIAN_POINT ( 'NONE',  ( 6.462472949537106715, -7.464222240803106570E-16, -6.094999999999989981 ) ) ;
#1164 = CARTESIAN_POINT ( 'NONE',  ( 94.64626352523143282, -4.472830434245840259, 4.472830434245838482 ) ) ;
#1165 = LINE ( 'NONE', #67173, #84196 ) ;
#1166 = EDGE_CURVE ( 'NONE', #128760, #71811, #56834, .T. ) ;
#1167 = VERTEX_POINT ( 'NONE', #45930 ) ;
#1168 = AXIS2_PLACEMENT_3D ( 'NONE', #40012, #29099, #31776 ) ;
#1169 = EDGE_CURVE ( 'NONE', #56720, #4770, #80696, .T. ) ;
#1170 = DIRECTION ( 'NONE',  ( -0.3543493200069162685, -0.000000000000000000, -0.9351131265310288487 ) ) ;
#1171 = ORIENTED_EDGE ( 'NONE', *, *, #136792, .F. ) ;
#1172 = DIRECTION ( 'NONE',  ( -0.6830127018922180770, -0.6830127018922204085, -0.2588190451025213501 ) ) ;
#1173 = CARTESIAN_POINT ( 'NONE',  ( -11.81601139373100651, 28.73617430169779041, 5.000000000000000000 ) ) ;
#1174 = VERTEX_POINT ( 'NONE', #69107 ) ;
#1175 = EDGE_CURVE ( 'NONE', #104818, #11807, #13965, .T. ) ;
#1176 = DIRECTION ( 'NONE',  ( 0.000000000000000000, 0.000000000000000000, 1.000000000000000000 ) ) ;
#1177 = CARTESIAN_POINT ( 'NONE',  ( 2.510786437626908008, -27.52281430457053446, 5.000000000000000000 ) ) ;
#1178 = ORIENTED_EDGE ( 'NONE', *, *, #48064, .F. ) ;
#1179 = EDGE_CURVE ( 'NONE', #76434, #9731, #45604, .T. ) ;
#1180 = DIRECTION ( 'NONE',  ( -1.000000000000000000, -0.000000000000000000, -0.000000000000000000 ) ) ;
#1181 = VECTOR ( 'NONE', #15133, 1000.000000000000000 ) ;
#1182 = EDGE_LOOP ( 'NONE', ( #123591, #125967, #138779, #93583 ) ) ;
#1183 = EDGE_LOOP ( 'NONE', ( #4775, #85337, #276, #105897 ) ) ;
#1184 = ORIENTED_EDGE ( 'NONE', *, *, #18214, .F. ) ;
#1185 = LINE ( 'NONE', #67947, #137352 ) ;
#1186 = CARTESIAN_POINT ( 'NONE',  ( 14.20710678118645376, 12.75929247661558996, 5.000000000000000000 ) ) ;
#1187 = DIRECTION ( 'NONE',  ( 0.000000000000000000, 0.000000000000000000, -1.000000000000000000 ) ) ;
#1188 = EDGE_CURVE ( 'NONE', #127957, #23069, #90867, .T. ) ;
#1189 = LINE ( 'NONE', #89649, #25674 ) ;
#1190 = VERTEX_POINT ( 'NONE', #57524 ) ;
#1191 = DIRECTION ( 'NONE',  ( 0.6830127018922181881, 0.6830127018922202975, -0.2588190451025214056 ) ) ;
#1192 = VECTOR ( 'NONE', #13568, 1000.000000000000000 ) ;
#1193 = AXIS2_PLACEMENT_3D ( 'NONE', #10456, #9746, #32235 ) ;
#1194 = CARTESIAN_POINT ( 'NONE',  ( 17.04123647476855652, 0.000000000000000000, 7.934999999999990727 ) ) ;
#1195 = LINE ( 'NONE', #101964, #87911 ) ;
#1196 = AXIS2_PLACEMENT_3D ( 'NONE', #52105, #133091, #33772 ) ;
#1197 = CARTESIAN_POINT ( 'NONE',  ( -32.00492477221175136, -5.240707523384228850, 12.38332538355503409 ) ) ;
#1198 = VECTOR ( 'NONE', #26699, 1000.000000000000000 ) ;
#1199 = CARTESIAN_POINT ( 'NONE',  ( -39.48921356237310221, -27.52281430457082934, 5.000000000000000000 ) ) ;
#1200 = ORIENTED_EDGE ( 'NONE', *, *, #8875, .T. ) ;
#1201 = ORIENTED_EDGE ( 'NONE', *, *, #73588, .T. ) ;
#1202 = ORIENTED_EDGE ( 'NONE', *, *, #5532, .T. ) ;
#1203 = CARTESIAN_POINT ( 'NONE',  ( 156.1500000000000057, -49.14999999999999147, 49.92499999999997584 ) ) ;
#1204 = CARTESIAN_POINT ( 'NONE',  ( 28.17183060077628198, -2.240707523384254163, 4.000000000000000000 ) ) ;
#1205 = UNCERTAINTY_MEASURE_WITH_UNIT (LENGTH_MEASURE( 1.000000000000000082E-05 ), #112057, 'distance_accuracy_value', 'NONE');
#1206 = LINE ( 'NONE', #98413, #61291 ) ;
#1207 = FACE_OUTER_BOUND ( 'NONE', #10102, .T. ) ;
#1208 = CARTESIAN_POINT ( 'NONE',  ( 7.036110477784782269, 9.049368983927246646, -2.898830007922127638 ) ) ;
#1209 = CARTESIAN_POINT ( 'NONE',  ( -57.18398860626899705, 28.73617430169827358, 5.000000000000000000 ) ) ;
#1210 = CARTESIAN_POINT ( 'NONE',  ( -7.499999999999940492, -1.912538124160739095, 4.000000000000000000 ) ) ;
#1211 = DIRECTION ( 'NONE',  ( 0.7071067811865486830, -0.7071067811865464625, -0.000000000000000000 ) ) ;
#1212 = DIRECTION ( 'NONE',  ( -0.6830127018922181881, 0.6830127018922202975, -0.2588190451025214056 ) ) ;
#1213 = VERTEX_POINT ( 'NONE', #101711 ) ;
#1214 = DIRECTION ( 'NONE',  ( -1.000000000000000000, -0.000000000000000000, -0.000000000000000000 ) ) ;
#1215 = EDGE_LOOP ( 'NONE', ( #133131, #72921, #116682, #12853 ) ) ;
#1216 = CARTESIAN_POINT ( 'NONE',  ( 19.61406247417281890, -0.8217383486644460611, -31.54407713966740090 ) ) ;
#1217 = ORIENTED_EDGE ( 'NONE', *, *, #127215, .T. ) ;
#1218 = LINE ( 'NONE', #1910, #117720 ) ;
#1220 = ORIENTED_EDGE ( 'NONE', *, *, #119260, .F. ) ;
#1219 = CARTESIAN_POINT ( 'NONE',  ( 7.499999999999949374, 6.052185695429103340, 5.000000000000000000 ) ) ;
#1221 =( NAMED_UNIT ( * ) SI_UNIT ( $, .STERADIAN. ) SOLID_ANGLE_UNIT ( ) );
#1222 = DIRECTION ( 'NONE',  ( 0.6830127018922180770, -0.6830127018922204085, -0.2588190451025213501 ) ) ;
#1223 = EDGE_CURVE ( 'NONE', #56577, #75784, #81427, .T. ) ;
#1224 = EDGE_LOOP ( 'NONE', ( #85581, #115658, #42988, #56556 ) ) ;
#1225 = CARTESIAN_POINT ( 'NONE',  ( -72.18398860626899705, 28.73617430169837661, 5.000000000000000000 ) ) ;
#1226 = ORIENTED_EDGE ( 'NONE', *, *, #75166, .F. ) ;
#1227 = DIRECTION ( 'NONE',  ( 1.000000000000000000, 1.224606353822377258E-16, 0.000000000000000000 ) ) ;
#1228 = UNCERTAINTY_MEASURE_WITH_UNIT (LENGTH_MEASURE( 1.000000000000000082E-05 ), #8180, 'distance_accuracy_value', 'NONE');
#1229 = ORIENTED_EDGE ( 'NONE', *, *, #123542, .F. ) ;
#1230 = CARTESIAN_POINT ( 'NONE',  ( -5.292893218813416567, 8.259292476615632594, 5.000000000000000000 ) ) ;
#1232 = EDGE_CURVE ( 'NONE', #106471, #108854, #48777, .T. ) ;
#1231 = CARTESIAN_POINT ( 'NONE',  ( 107.1208603837962272, -6.884901960086286188, 3.974999999999997424 ) ) ;
#1233 = LINE ( 'NONE', #78845, #27718 ) ;
#1235 = EDGE_CURVE ( 'NONE', #89696, #57963, #115397, .T. ) ;
#1234 = ORIENTED_EDGE ( 'NONE', *, *, #47549, .T. ) ;
#1236 = CARTESIAN_POINT ( 'NONE',  ( 17.06332250466817158, 4.584330080086930965E-16, 0.000000000000000000 ) ) ;
#1237 = LINE ( 'NONE', #66535, #7897 ) ;
#1238 = EDGE_CURVE ( 'NONE', #142920, #91253, #19690, .T. ) ;
#1239 = DIRECTION ( 'NONE',  ( 0.6830127018922180770, -0.6830127018922204085, -0.2588190451025213501 ) ) ;
#1240 = CARTESIAN_POINT ( 'NONE',  ( 15.60416666666666430, -1.633150327867691987, -6.094999999999989093 ) ) ;
#1241 = LINE ( 'NONE', #102737, #56051 ) ;
#1242 = CARTESIAN_POINT ( 'NONE',  ( 65.99451991528749772, 28.92564299267984396, 4.000000000000000000 ) ) ;
#1244 = EDGE_CURVE ( 'NONE', #24821, #66605, #107417, .T. ) ;
#1243 = CARTESIAN_POINT ( 'NONE',  ( 29.20710678118634007, -8.240707523384203981, 5.000000000000000000 ) ) ;
#1245 = VERTEX_POINT ( 'NONE', #5930 ) ;
#1246 = EDGE_LOOP ( 'NONE', ( #48610, #109261, #97300, #61995 ) ) ;
#1247 = CARTESIAN_POINT ( 'NONE',  ( 14.27159235450332098, -5.777789833161707559E-31, 2.500000000000001332 ) ) ;
#1249 = EDGE_LOOP ( 'NONE', ( #141134, #120202, #46022, #17961 ) ) ;
#1248 = EDGE_CURVE ( 'NONE', #52184, #99523, #50206, .T. ) ;
#1250 = EDGE_CURVE ( 'NONE', #59483, #94981, #53019, .T. ) ;
#1251 = CARTESIAN_POINT ( 'NONE',  ( 93.33376352523144703, 6.110000000000001208, 1.122388791418549305E-15 ) ) ;
#1252 = CARTESIAN_POINT ( 'NONE',  ( -8.531356016368066619, 22.22500000000000142, 15.00153835162133475 ) ) ;
#1253 = DIRECTION ( 'NONE',  ( -1.000000000000000000, -0.000000000000000000, -0.000000000000000000 ) ) ;
#1254 = DIRECTION ( 'NONE',  ( -0.000000000000000000, -0.3543493200069152693, 0.9351131265310292928 ) ) ;
#1255 = ORIENTED_EDGE ( 'NONE', *, *, #118819, .F. ) ;
#1256 = PLANE ( 'NONE',  #10391 ) ;
#1257 = CARTESIAN_POINT ( 'NONE',  ( -6.316579611327855837, -6.740707523384212863, 11.88629033278125746 ) ) ;
#1258 = ADVANCED_FACE ( 'NONE', ( #7373 ), #95826, .F. ) ;
#1259 = LINE ( 'NONE', #102031, #106730 ) ;
#1260 = EDGE_CURVE ( 'NONE', #50292, #107270, #121139, .T. ) ;
#1261 = LINE ( 'NONE', #45545, #141113 ) ;
#1262 = DIRECTION ( 'NONE',  ( -1.000000000000000000, -1.224606353822377258E-16, -0.000000000000000000 ) ) ;
#1264 = ORIENTED_EDGE ( 'NONE', *, *, #33892, .F. ) ;
#1263 = DIRECTION ( 'NONE',  ( 0.6830127018922181881, 0.6830127018922202975, -0.2588190451025214056 ) ) ;
#1265 = CARTESIAN_POINT ( 'NONE',  ( 156.1499999999997783, -52.14999999999999147, 34.92500000000004690 ) ) ;
#1266 = DIRECTION ( 'NONE',  ( -0.7071067811865487940, 0.7071067811865463515, -0.000000000000000000 ) ) ;
#1267 = DIRECTION ( 'NONE',  ( -0.7071067811865486830, -0.7071067811865464625, -0.000000000000000000 ) ) ;
#1268 = CARTESIAN_POINT ( 'NONE',  ( 184.1499999999998067, -3.180000000000061444, 31.92499999999998295 ) ) ;
#1269 = EDGE_CURVE ( 'NONE', #63821, #131899, #101132, .T. ) ;
#1270 = CARTESIAN_POINT ( 'NONE',  ( 0.000000000000000000, 0.000000000000000000, -1.142820323027524232 ) ) ;
#1271 = ORIENTED_EDGE ( 'NONE', *, *, #28429, .T. ) ;
#1272 = VECTOR ( 'NONE', #142529, 999.9999999999998863 ) ;
#1273 = ORIENTED_EDGE ( 'NONE', *, *, #42125, .T. ) ;
#1274 = VERTEX_POINT ( 'NONE', #76228 ) ;
#1275 = CARTESIAN_POINT ( 'NONE',  ( 87.93793019189809002, -6.110000000000001208, 1.637169565754158951 ) ) ;
#1276 = ORIENTED_EDGE ( 'NONE', *, *, #52310, .T. ) ;
#1277 = VECTOR ( 'NONE', #51961, 1000.000000000000227 ) ;
#1278 = CARTESIAN_POINT ( 'NONE',  ( 32.99999999999977973, -6.412538124160687580, 4.000000000000000000 ) ) ;
#1279 = CARTESIAN_POINT ( 'NONE',  ( 14.97558742549547794, -1.187250289053316088, 4.247958624336164668 ) ) ;
#1280 = DIRECTION ( 'NONE',  ( 0.7071067811865487940, -0.7071067811865463515, 0.000000000000000000 ) ) ;
#1281 = LINE ( 'NONE', #13581, #24591 ) ;
#1282 = ORIENTED_EDGE ( 'NONE', *, *, #97105, .T. ) ;
#1283 = DIRECTION ( 'NONE',  ( -0.7071067811865486830, -0.7071067811865464625, 0.000000000000000000 ) ) ;
#1285 =( BOUNDED_CURVE ( )  B_SPLINE_CURVE ( 3, ( #10003, #133935, #89708, #110022 ),
 .UNSPECIFIED., .F., .F. ) 
 B_SPLINE_CURVE_WITH_KNOTS ( ( 4, 4 ),
 ( 5.106027341939277875, 6.645403452391244414 ),
 .UNSPECIFIED. ) 
 CURVE ( )  GEOMETRIC_REPRESENTATION_ITEM ( )  RATIONAL_B_SPLINE_CURVE ( ( 1.000000000000000000, 0.8120851936182275077, 0.8120851936182275077, 1.000000000000000000 ) ) 
 REPRESENTATION_ITEM ( '' )  );
#1284 = FACE_OUTER_BOUND ( 'NONE', #26117, .T. ) ;
#1286 = CARTESIAN_POINT ( 'NONE',  ( 57.29974487139158157, -27.71228299555246011, 4.000000000000000000 ) ) ;
#1287 = CARTESIAN_POINT ( 'NONE',  ( 85.22459685856478018, -1.637169565754160949, 6.109999999999997655 ) ) ;
#1288 = VECTOR ( 'NONE', #116450, 1000.000000000000000 ) ;
#1289 = ORIENTED_EDGE ( 'NONE', *, *, #44710, .F. ) ;
#1290 = DIRECTION ( 'NONE',  ( 0.7071067811865487940, 0.7071067811865463515, 0.000000000000000000 ) ) ;
#1291 = EDGE_CURVE ( 'NONE', #86454, #32049, #43589, .T. ) ;
#1292 = CARTESIAN_POINT ( 'NONE',  ( 27.48921356237309155, -27.52281430457074762, 5.000000000000000000 ) ) ;
#1293 = ORIENTED_EDGE ( 'NONE', *, *, #77447, .F. ) ;
#1294 = VERTEX_POINT ( 'NONE', #23239 ) ;
#1295 = LINE ( 'NONE', #14338, #102420 ) ;
#1296 = LINE ( 'NONE', #12894, #36184 ) ;
#1297 = CARTESIAN_POINT ( 'NONE',  ( 24.85873647476855552, 5.808823158059031044, -5.808823158059037262 ) ) ;
#1298 = LINE ( 'NONE', #36117, #81309 ) ;
#1299 = DIRECTION ( 'NONE',  ( 0.7071067811865487940, 0.7071067811865463515, -0.000000000000000000 ) ) ;
#1300 = EDGE_CURVE ( 'NONE', #106183, #141363, #142217, .T. ) ;
#1301 = AXIS2_PLACEMENT_3D ( 'NONE', #51952, #96133, #42518 ) ;
#1302 = CARTESIAN_POINT ( 'NONE',  ( -33.18398860626899705, 28.73617430169810305, 5.000000000000000000 ) ) ;
#1303 = CYLINDRICAL_SURFACE ( 'NONE', #112184, 2.500000000000000000 ) ;
#1304 =( NAMED_UNIT ( * ) SI_UNIT ( $, .STERADIAN. ) SOLID_ANGLE_UNIT ( ) );
#1305 = VECTOR ( 'NONE', #138783, 1000.000000000000114 ) ;
#1306 = ORIENTED_EDGE ( 'NONE', *, *, #112485, .F. ) ;
#1308 = ORIENTED_EDGE ( 'NONE', *, *, #103071, .F. ) ;
#1307 = AXIS2_PLACEMENT_3D ( 'NONE', #122764, #67720, #32944 ) ;
#1309 = LINE ( 'NONE', #85131, #64250 ) ;
#1311 = VERTEX_POINT ( 'NONE', #20387 ) ;
#1310 = ADVANCED_FACE ( 'NONE', ( #132047 ), #119686, .F. ) ;
#1312 = ORIENTED_EDGE ( 'NONE', *, *, #63406, .T. ) ;
#1313 = AXIS2_PLACEMENT_3D ( 'NONE', #138192, #72269, #83097 ) ;
#1314 = CARTESIAN_POINT ( 'NONE',  ( 16.61159235450331906, 9.902892378096218942E-16, 0.000000000000000000 ) ) ;
#1315 = VERTEX_POINT ( 'NONE', #76971 ) ;
#1316 = CARTESIAN_POINT ( 'NONE',  ( 57.39169371712954160, 2.130196079827421762, 7.950000000000000178 ) ) ;
#1317 = DIRECTION ( 'NONE',  ( -0.3543493200069162685, -0.000000000000000000, -0.9351131265310288487 ) ) ;
#1318 = ADVANCED_FACE ( 'NONE', ( #130632 ), #75517, .F. ) ;
#1319 = CARTESIAN_POINT ( 'NONE',  ( 0.000000000000000000, 0.000000000000000000, 5.000000000000000000 ) ) ;
#1320 = DIRECTION ( 'NONE',  ( 0.7071067811865487940, 0.7071067811865463515, 0.000000000000000000 ) ) ;
#1321 = ORIENTED_EDGE ( 'NONE', *, *, #26511, .T. ) ;
#1322 = CARTESIAN_POINT ( 'NONE',  ( 25.39999999999999858, 0.000000000000000000, 0.000000000000000000 ) ) ;
#1323 = ORIENTED_EDGE ( 'NONE', *, *, #90940, .F. ) ;
#1325 = ADVANCED_FACE ( 'NONE', ( #66780 ), #774, .T. ) ;
#1324 = DIRECTION ( 'NONE',  ( 0.6830127018922181881, 0.6830127018922202975, -0.2588190451025214056 ) ) ;
#1326 = EDGE_LOOP ( 'NONE', ( #260, #7384, #48856, #127940 ) ) ;
#1327 = SURFACE_STYLE_FILL_AREA ( #56502 ) ;
#1328 = ORIENTED_EDGE ( 'NONE', *, *, #99413, .F. ) ;
#1329 = PLANE ( 'NONE',  #140790 ) ;
#1330 = ORIENTED_EDGE ( 'NONE', *, *, #53151, .T. ) ;
#1331 = ORIENTED_EDGE ( 'NONE', *, *, #70841, .T. ) ;
#1332 = ORIENTED_EDGE ( 'NONE', *, *, #26827, .F. ) ;
#1333 = FACE_OUTER_BOUND ( 'NONE', #102147, .T. ) ;
#1334 = CARTESIAN_POINT ( 'NONE',  ( -8.700255128608413102, -27.71228299555199825, 4.000000000000000000 ) ) ;
#1335 = CARTESIAN_POINT ( 'NONE',  ( -12.69999999999998153, 0.000000000000000000, 0.000000000000000000 ) ) ;
#1336 = LINE ( 'NONE', #112283, #107401 ) ;
#1337 = CARTESIAN_POINT ( 'NONE',  ( 121.0420968585647756, 5.291415217122923842, -3.054999999999996163 ) ) ;
#1338 = DIRECTION ( 'NONE',  ( 0.000000000000000000, 0.000000000000000000, 1.000000000000000000 ) ) ;
#1339 = DIRECTION ( 'NONE',  ( 0.7071067811865487940, 0.7071067811865463515, 0.000000000000000000 ) ) ;
#1340 = CARTESIAN_POINT ( 'NONE',  ( 15.48921356237309510, -27.52281430457066236, 5.000000000000000000 ) ) ;
#1341 = CARTESIAN_POINT ( 'NONE',  ( -9.722814304570524868, -21.72500000000000497, 5.000000000000000000 ) ) ;
#1342 = FACE_OUTER_BOUND ( 'NONE', #53273, .T. ) ;
#1343 = VERTEX_POINT ( 'NONE', #45069 ) ;
#1344 = EDGE_CURVE ( 'NONE', #48060, #114516, #12378, .T. ) ;
#1345 = CARTESIAN_POINT ( 'NONE',  ( 17.57538274164440040, -2.608983483842240325, 5.000000000000000000 ) ) ;
#1346 = DIRECTION ( 'NONE',  ( 0.7071067811865487940, 0.7071067811865463515, 0.000000000000000000 ) ) ;
#1347 = DIRECTION ( 'NONE',  ( -0.7071067811865486830, -0.7071067811865464625, 0.000000000000000000 ) ) ;
#1348 = EDGE_LOOP ( 'NONE', ( #40969, #4224, #128380, #788, #67686, #50092, #101673, #38774, #62214, #112247, #107375, #138463, #133997, #65653, #92971, #39749, #60305, #21777, #3018, #81975, #44225, #99062, #121351, #87831, #27165, #142601, #12354, #79618, #22556, #95417, #98165, #72518, #24293, #107396, #1773, #20521, #129040, #59526 ) ) ;
#1349 = VERTEX_POINT ( 'NONE', #11640 ) ;
#1350 = DIRECTION ( 'NONE',  ( -0.6830127018922181881, 0.6830127018922202975, -0.2588190451025214056 ) ) ;
#1351 = ORIENTED_EDGE ( 'NONE', *, *, #98474, .F. ) ;
#1352 = ORIENTED_EDGE ( 'NONE', *, *, #9974, .T. ) ;
#1353 = CARTESIAN_POINT ( 'NONE',  ( 57.29974487139158157, -27.71228299555246011, 4.000000000000000000 ) ) ;
#1354 = CARTESIAN_POINT ( 'NONE',  ( 13.75413961620377457, 3.047499999999993214, -5.278424836066146320 ) ) ;
#1355 = CARTESIAN_POINT ( 'NONE',  ( -1.637538124160967001, 22.22500000000000142, 4.000000000000000000 ) ) ;
#1356 = EDGE_CURVE ( 'NONE', #76633, #89639, #55919, .T. ) ;
#1357 = DIRECTION ( 'NONE',  ( 0.000000000000000000, 0.000000000000000000, 1.000000000000000000 ) ) ;
#1358 = ORIENTED_EDGE ( 'NONE', *, *, #129245, .F. ) ;
#1359 = PLANE ( 'NONE',  #139009 ) ;
#1360 = EDGE_LOOP ( 'NONE', ( #126214, #64444, #65547, #24000 ) ) ;
#1361 = DIRECTION ( 'NONE',  ( -1.000000000000000000, -1.224606353822377258E-16, -0.000000000000000000 ) ) ;
#1362 = VECTOR ( 'NONE', #6419, 1000.000000000000000 ) ;
#1363 = CARTESIAN_POINT ( 'NONE',  ( 22.08790314143522338, 6.871911579029515771, 3.967499999999989146 ) ) ;
#1364 = ORIENTED_EDGE ( 'NONE', *, *, #130588, .F. ) ;
#1365 = CARTESIAN_POINT ( 'NONE',  ( 85.80793019189810877, -6.109999999999999432, 1.637169565754158507 ) ) ;
#1366 = CARTESIAN_POINT ( 'NONE',  ( 31.49999999999977973, -11.56887692260769285, 4.000000000000000000 ) ) ;
#1367 = AXIS2_PLACEMENT_3D ( 'NONE', #27872, #61279, #19142 ) ;
#1368 = DIRECTION ( 'NONE',  ( 0.7071067811865487940, 0.7071067811865463515, 0.000000000000000000 ) ) ;
#1369 = ORIENTED_EDGE ( 'NONE', *, *, #69640, .T. ) ;
#1370 = VERTEX_POINT ( 'NONE', #34156 ) ;
#1371 = ORIENTED_EDGE ( 'NONE', *, *, #53949, .F. ) ;
#1372 = LINE ( 'NONE', #95894, #109803 ) ;
#1373 = CARTESIAN_POINT ( 'NONE',  ( 14.08373646989360317, 3.821174125832445049E-16, 0.000000000000000000 ) ) ;
#1374 = FACE_OUTER_BOUND ( 'NONE', #130641, .T. ) ;
#1375 = DIRECTION ( 'NONE',  ( 0.7071067811865487940, -0.7071067811865463515, 0.000000000000000000 ) ) ;
#1376 = EDGE_CURVE ( 'NONE', #85512, #4593, #1479, .T. ) ;
#1377 = ORIENTED_EDGE ( 'NONE', *, *, #98353, .T. ) ;
#1378 = CARTESIAN_POINT ( 'NONE',  ( -34.42500000000001137, -21.72500000000000142, 4.500000000000000888 ) ) ;
#1379 = VECTOR ( 'NONE', #78654, 999.9999999999998863 ) ;
#1380 = DIRECTION ( 'NONE',  ( -0.7071067811865486830, -0.7071067811865464625, 0.000000000000000000 ) ) ;
#1381 = DIRECTION ( 'NONE',  ( -1.000000000000000000, -1.224606353822377258E-16, -0.000000000000000000 ) ) ;
#1382 = EDGE_LOOP ( 'NONE', ( #65288, #6857, #101636, #67565 ) ) ;
#1383 = CARTESIAN_POINT ( 'NONE',  ( -19.05000000000000071, 3.174999999999997158, 5.000000000000000000 ) ) ;
#1384 = CARTESIAN_POINT ( 'NONE',  ( 34.42499999999998295, 0.000000000000000000, 4.500000000000000888 ) ) ;
#1385 = ORIENTED_EDGE ( 'NONE', *, *, #44170, .T. ) ;
#1387 = ORIENTED_EDGE ( 'NONE', *, *, #16307, .T. ) ;
#1386 = CARTESIAN_POINT ( 'NONE',  ( 11.62000000000000099, 9.521314400968980422E-16, 0.000000000000000000 ) ) ;
#1388 = ORIENTED_EDGE ( 'NONE', *, *, #111799, .T. ) ;
#1389 = CARTESIAN_POINT ( 'NONE',  ( 34.92499999999998295, -7.487538124160447950, 4.000000000000000000 ) ) ;
#1390 = CARTESIAN_POINT ( 'NONE',  ( 13.60986171580761805, 2.055000000000001048, 0.000000000000000000 ) ) ;
#1391 = ORIENTED_EDGE ( 'NONE', *, *, #140476, .F. ) ;
#1392 = SURFACE_SIDE_STYLE ('',( #100744 ) ) ;
#1393 = UNCERTAINTY_MEASURE_WITH_UNIT (LENGTH_MEASURE( 1.000000000000000082E-05 ), #82010, 'distance_accuracy_value', 'NONE');
#1394 = AXIS2_PLACEMENT_3D ( 'NONE', #92961, #114694, #58248 ) ;
#1395 = CARTESIAN_POINT ( 'NONE',  ( -32.20710678118631876, -2.240707523384264377, 5.000000000000000000 ) ) ;
#1396 = LINE ( 'NONE', #81149, #117940 ) ;
#1398 = EDGE_CURVE ( 'NONE', #6574, #114790, #31302, .T. ) ;
#1397 = AXIS2_PLACEMENT_3D ( 'NONE', #38406, #114520, #71053 ) ;
#1399 = CARTESIAN_POINT ( 'NONE',  ( 27.18398860626900060, 28.73617430169806042, 5.000000000000000000 ) ) ;
#1400 = LINE ( 'NONE', #113761, #82996 ) ;
#1401 = EDGE_CURVE ( 'NONE', #91522, #20875, #13079, .T. ) ;
#1402 = DIRECTION ( 'NONE',  ( -0.7071067811865486830, 0.7071067811865464625, 0.000000000000000000 ) ) ;
#1403 = CARTESIAN_POINT ( 'NONE',  ( 0.7928932188134476533, -2.240707523384262601, 5.000000000000000000 ) ) ;
#1404 = CARTESIAN_POINT ( 'NONE',  ( 39.48921356237310221, -27.52281430457082934, 5.000000000000000000 ) ) ;
#1405 = ADVANCED_FACE ( 'NONE', ( #114545 ), #136301, .F. ) ;
#1406 = DIRECTION ( 'NONE',  ( -0.3543493200069162685, -0.000000000000000000, -0.9351131265310288487 ) ) ;
#1407 = CARTESIAN_POINT ( 'NONE',  ( 21.85373647476855297, -5.808823158059035485, -5.808823158059033709 ) ) ;
#1408 = CARTESIAN_POINT ( 'NONE',  ( 0.7079031414352193741, -6.871911579029513106, -3.967499999999993587 ) ) ;
#1409 = PLANE ( 'NONE',  #92278 ) ;
#1410 = VECTOR ( 'NONE', #48517, 1000.000000000000000 ) ;
#1411 = CARTESIAN_POINT ( 'NONE',  ( 109.7916666666666572, 3.975000000000003642, -6.884901960086285300 ) ) ;
#1413 = EDGE_CURVE ( 'NONE', #39017, #37842, #16246, .T. ) ;
#1412 = CARTESIAN_POINT ( 'NONE',  ( 0.000000000000000000, 0.000000000000000000, 5.000000000000000000 ) ) ;
#1414 = VERTEX_POINT ( 'NONE', #92074 ) ;
#1415 = ORIENTED_EDGE ( 'NONE', *, *, #40573, .F. ) ;
#1416 = CARTESIAN_POINT ( 'NONE',  ( 106.1458333333333144, 2.130196079827431976, -7.949999999999999289 ) ) ;
#1417 = EDGE_LOOP ( 'NONE', ( #107064, #64039, #40241, #73848 ) ) ;
#1418 = VERTEX_POINT ( 'NONE', #124719 ) ;
#1419 = ORIENTED_EDGE ( 'NONE', *, *, #126471, .F. ) ;
#1420 = CARTESIAN_POINT ( 'NONE',  ( -20.99999999999985789, -16.44781430457065952, 5.000000000000000000 ) ) ;
#1421 = CARTESIAN_POINT ( 'NONE',  ( 14.47120107780393461, 9.396302691346770430, -1.425124364721372938 ) ) ;
#1422 = ORIENTED_EDGE ( 'NONE', *, *, #49308, .T. ) ;
#1423 = CARTESIAN_POINT ( 'NONE',  ( 19.93618820137057668, -0.2700000000508058218, -40.00000000000000000 ) ) ;
#1424 = CARTESIAN_POINT ( 'NONE',  ( 18.18398860626898994, 28.73617430169800002, 5.000000000000000000 ) ) ;
#1425 = ADVANCED_FACE ( 'NONE', ( #123322 ), #115223, .F. ) ;
#1426 = DIRECTION ( 'NONE',  ( -1.000000000000000000, -1.224606353822377258E-16, -0.000000000000000000 ) ) ;
#1427 = CARTESIAN_POINT ( 'NONE',  ( 5.510786437626906675, -27.52281430457051314, 5.000000000000000000 ) ) ;
#1428 = EDGE_LOOP ( 'NONE', ( #35076, #122709, #134803, #121004 ) ) ;
#1429 = EDGE_CURVE ( 'NONE', #132789, #47888, #104377, .T. ) ;
#1430 = CARTESIAN_POINT ( 'NONE',  ( 128.6829301918981230, -1.637169565754158951, -6.109999999999998543 ) ) ;
#1431 = DIRECTION ( 'NONE',  ( -0.7071067811865487940, 0.7071067811865463515, 0.000000000000000000 ) ) ;
#1432 = LINE ( 'NONE', #55142, #137712 ) ;
#1433 = CARTESIAN_POINT ( 'NONE',  ( 34.49999999999975842, 15.05432934483078888, 4.994342998332163219 ) ) ;
#1434 = LINE ( 'NONE', #102930, #31347 ) ;
#1435 = CARTESIAN_POINT ( 'NONE',  ( 9.591592354503321260, 9.902892378096218942E-16, 0.000000000000000000 ) ) ;
#1436 = CARTESIAN_POINT ( 'NONE',  ( 34.42499999999998295, -7.458600742197882383, 5.000000000000000000 ) ) ;
#1437 = CARTESIAN_POINT ( 'NONE',  ( 87.14169371712955581, -2.130196079827424871, -7.949999999999998401 ) ) ;
#1438 = EDGE_CURVE ( 'NONE', #81104, #49860, #2180, .T. ) ;
#1439 = CARTESIAN_POINT ( 'NONE',  ( 34.92499999999998295, 7.067865804795108176, 10.74360474999299342 ) ) ;
#1440 = ORIENTED_EDGE ( 'NONE', *, *, #89087, .F. ) ;
#1441 = VERTEX_POINT ( 'NONE', #95646 ) ;
#1442 = CARTESIAN_POINT ( 'NONE',  ( 119.8754301918981184, -5.291415217122920289, -3.055000000000001492 ) ) ;
#1443 =( BOUNDED_CURVE ( )  B_SPLINE_CURVE ( 3, ( #73077, #117229, #93369, #106347 ),
 .UNSPECIFIED., .F., .T. ) 
 B_SPLINE_CURVE_WITH_KNOTS ( ( 4, 4 ),
 ( 1.964434688349483871, 3.503810798801452187 ),
 .UNSPECIFIED. ) 
 CURVE ( )  GEOMETRIC_REPRESENTATION_ITEM ( )  RATIONAL_B_SPLINE_CURVE ( ( 1.000000000000000000, 0.8120851936182270636, 0.8120851936182270636, 1.000000000000000000 ) ) 
 REPRESENTATION_ITEM ( '' )  );
#1444 = ORIENTED_EDGE ( 'NONE', *, *, #135572, .F. ) ;
#1445 = CARTESIAN_POINT ( 'NONE',  ( -2.999999999999981792, 4.931123077392134846, 4.000000000000000000 ) ) ;
#1446 = ADVANCED_FACE ( 'NONE', ( #40583 ), #127578, .T. ) ;
#1447 = TOROIDAL_SURFACE ( 'NONE', #52377, 16.45000000000002061, 1.000000000000000000 ) ;
#1448 = DIRECTION ( 'NONE',  ( 0.7071067811865487940, 0.7071067811865463515, -0.000000000000000000 ) ) ;
#1449 = DIRECTION ( 'NONE',  ( 0.000000000000000000, -1.000000000000000000, 0.000000000000000000 ) ) ;
#1450 = PLANE ( 'NONE',  #127662 ) ;
#1451 = CARTESIAN_POINT ( 'NONE',  ( 113.2245968585647944, -1.637169565754160949, 6.109999999999997655 ) ) ;
#1452 = ORIENTED_EDGE ( 'NONE', *, *, #25871, .T. ) ;
#1453 = VERTEX_POINT ( 'NONE', #115958 ) ;
#1454 = EDGE_CURVE ( 'NONE', #23170, #56532, #105103, .T. ) ;
#1455 = VECTOR ( 'NONE', #16197, 1000.000000000000000 ) ;
#1456 = DIRECTION ( 'NONE',  ( 0.7071067811865487940, 0.7071067811865463515, -0.000000000000000000 ) ) ;
#1457 = EDGE_LOOP ( 'NONE', ( #117782, #72152, #105613, #133932 ) ) ;
#1458 = ORIENTED_EDGE ( 'NONE', *, *, #52172, .F. ) ;
#1459 = CARTESIAN_POINT ( 'NONE',  ( 37.18793019189810423, 6.110000000000002984, -1.637169565754156730 ) ) ;
#1460 = VERTEX_POINT ( 'NONE', #38433 ) ;
#1461 = LINE ( 'NONE', #6429, #42184 ) ;
#1462 = DIRECTION ( 'NONE',  ( -0.000000000000000000, 1.000000000000000000, 0.000000000000000000 ) ) ;
#1463 =( BOUNDED_CURVE ( )  B_SPLINE_CURVE ( 3, ( #123074, #133940, #90430, #546 ),
 .UNSPECIFIED., .F., .T. ) 
 B_SPLINE_CURVE_WITH_KNOTS ( ( 4, 4 ),
 ( 5.920967161967927161, 7.341195215986644484 ),
 .UNSPECIFIED. ) 
 CURVE ( )  GEOMETRIC_REPRESENTATION_ITEM ( )  RATIONAL_B_SPLINE_CURVE ( ( 1.000000000000000000, 0.8388583629366599403, 0.8388583629366599403, 1.000000000000000000 ) ) 
 REPRESENTATION_ITEM ( '' )  );
#1464 = EDGE_CURVE ( 'NONE', #114304, #124605, #49338, .T. ) ;
#1465 = VECTOR ( 'NONE', #113483, 1000.000000000000000 ) ;
#1466 = LINE ( 'NONE', #79103, #133371 ) ;
#1467 = VERTEX_POINT ( 'NONE', #116695 ) ;
#1468 = VECTOR ( 'NONE', #7725, 1000.000000000000227 ) ;
#1469 = FACE_OUTER_BOUND ( 'NONE', #87679, .T. ) ;
#1470 = ORIENTED_EDGE ( 'NONE', *, *, #91967, .T. ) ;
#1471 = ORIENTED_EDGE ( 'NONE', *, *, #26179, .F. ) ;
#1472 = VERTEX_POINT ( 'NONE', #84783 ) ;
#1473 = DIRECTION ( 'NONE',  ( 0.6830127018922181881, 0.6830127018922202975, -0.2588190451025214056 ) ) ;
#1474 = CARTESIAN_POINT ( 'NONE',  ( 29.99999999999979039, 1.931123077392167264, 4.000000000000000000 ) ) ;
#1475 = ORIENTED_EDGE ( 'NONE', *, *, #5643, .F. ) ;
#1476 = DIRECTION ( 'NONE',  ( 0.6830127018922180770, -0.6830127018922204085, -0.2588190451025213501 ) ) ;
#1477 = STYLED_ITEM ( 'NONE', ( #106319 ), #33707 ) ;
#1478 = EDGE_CURVE ( 'NONE', #60822, #110777, #93522, .T. ) ;
#1479 = LINE ( 'NONE', #111709, #50245 ) ;
#1480 = CARTESIAN_POINT ( 'NONE',  ( 24.39999999999999858, -7.600000000000061817, 28.92499999999998650 ) ) ;
#1481 = CARTESIAN_POINT ( 'NONE',  ( -75.29974487139158157, -27.71228299555258445, 4.000000000000000000 ) ) ;
#1483 = FACE_BOUND ( 'NONE', #94642, .T. ) ;
#1482 = COLOUR_RGB ( '', 0.66274510, 0.83137255, 0.94901961) ;
#1484 = ORIENTED_EDGE ( 'NONE', *, *, #38988, .F. ) ;
#1485 = DIRECTION ( 'NONE',  ( 0.3543493200069162685, -0.000000000000000000, -0.9351131265310288487 ) ) ;
#1487 = EDGE_CURVE ( 'NONE', #89682, #91342, #71787, .T. ) ;
#1486 = DIRECTION ( 'NONE',  ( -0.5735764363510501562, 0.8191520442889890230, 1.003171929053521419E-16 ) ) ;
#1488 = DIRECTION ( 'NONE',  ( 0.6830127018922180770, -0.6830127018922204085, -0.2588190451025213501 ) ) ;
#1489 = FACE_OUTER_BOUND ( 'NONE', #13573, .T. ) ;
#1490 = VERTEX_POINT ( 'NONE', #96331 ) ;
#1491 = DIRECTION ( 'NONE',  ( -0.7071067811865486830, 0.7071067811865464625, 0.000000000000000000 ) ) ;
#1492 = EDGE_LOOP ( 'NONE', ( #55613, #119762, #135155, #110848 ) ) ;
#1493 = ORIENTED_EDGE ( 'NONE', *, *, #59045, .F. ) ;
#1494 = VECTOR ( 'NONE', #70882, 1000.000000000000000 ) ;
#1495 = ORIENTED_EDGE ( 'NONE', *, *, #87274, .F. ) ;
#1496 = VECTOR ( 'NONE', #118446, 999.9999999999998863 ) ;
#1497 = AXIS2_PLACEMENT_3D ( 'NONE', #89913, #79094, #11614 ) ;
#1498 = CARTESIAN_POINT ( 'NONE',  ( 50.07876352523145158, -7.482591942790325086E-16, 6.109999999999998543 ) ) ;
#1499 = ORIENTED_EDGE ( 'NONE', *, *, #12379, .F. ) ;
#1500 = DIRECTION ( 'NONE',  ( 0.000000000000000000, -1.000000000000000000, 0.000000000000000000 ) ) ;
#1501 = DIRECTION ( 'NONE',  ( -0.7071067811865486830, -0.7071067811865464625, 0.000000000000000000 ) ) ;
#1502 = EDGE_LOOP ( 'NONE', ( #118836, #140359, #24138, #67306, #53247, #41866 ) ) ;
#1503 = CARTESIAN_POINT ( 'NONE',  ( 0.7933393645784738712, 21.75929247661549937, 4.998822639870705409 ) ) ;
#1504 = DIRECTION ( 'NONE',  ( -0.7071067811865486830, -0.7071067811865464625, 0.000000000000000000 ) ) ;
#1505 = VECTOR ( 'NONE', #40511, 1000.000000000000227 ) ;
#1506 = CARTESIAN_POINT ( 'NONE',  ( 34.17183060077623225, 6.759292476615649470, 4.000000000000000000 ) ) ;
#1507 = DIRECTION ( 'NONE',  ( -0.7071067811865487940, 0.7071067811865463515, -0.000000000000000000 ) ) ;
#1508 = EDGE_CURVE ( 'NONE', #97600, #63490, #117360, .T. ) ;
#1509 = CARTESIAN_POINT ( 'NONE',  ( -8.206660635421469507, 21.75929247661548516, 4.998822639870715179 ) ) ;
#1510 = ORIENTED_EDGE ( 'NONE', *, *, #84750, .T. ) ;
#1511 = VERTEX_POINT ( 'NONE', #60945 ) ;
#1512 = ORIENTED_EDGE ( 'NONE', *, *, #137577, .F. ) ;
#1513 = ORIENTED_EDGE ( 'NONE', *, *, #78402, .F. ) ;
#1514 = DIRECTION ( 'NONE',  ( 0.7071067811865487940, 0.7071067811865463515, 0.000000000000000000 ) ) ;
#1515 = DIRECTION ( 'NONE',  ( -0.7071067811865487940, 0.7071067811865463515, -0.000000000000000000 ) ) ;
#1516 = EDGE_LOOP ( 'NONE', ( #43037, #113889, #1371, #10256 ) ) ;
#1517 = ORIENTED_EDGE ( 'NONE', *, *, #98319, .F. ) ;
#1518 = CARTESIAN_POINT ( 'NONE',  ( 34.49999999999976552, -20.56887692260760758, 4.000000000000000000 ) ) ;
#1519 = EDGE_CURVE ( 'NONE', #132460, #13150, #118831, .T. ) ;
#1520 = EDGE_CURVE ( 'NONE', #95429, #71113, #90370, .T. ) ;
#1521 = CARTESIAN_POINT ( 'NONE',  ( 8.031592354503320763, 9.902892378096218942E-16, 0.000000000000000000 ) ) ;
#1522 = ORIENTED_EDGE ( 'NONE', *, *, #12001, .F. ) ;
#1523 = DIRECTION ( 'NONE',  ( -0.7071067811865486830, -0.7071067811865464625, 0.000000000000000000 ) ) ;
#1524 = CARTESIAN_POINT ( 'NONE',  ( 0.2569208697893812232, 0.4000000000000001332, -2.015694669338588429 ) ) ;
#1525 = CARTESIAN_POINT ( 'NONE',  ( 23.98373647476855197, -5.808823158059035485, -5.808823158059033709 ) ) ;
#1526 = AXIS2_PLACEMENT_3D ( 'NONE', #100709, #35484, #34032 ) ;
#1527 = CARTESIAN_POINT ( 'NONE',  ( 18.29974487139159223, -27.71228299555219010, 4.000000000000000000 ) ) ;
#1528 = ORIENTED_EDGE ( 'NONE', *, *, #23028, .T. ) ;
#1529 = CARTESIAN_POINT ( 'NONE',  ( 108.2662635252314374, 4.472830434245839371, -4.472830434245839371 ) ) ;
#1530 = ADVANCED_FACE ( 'NONE', ( #39883 ), #5765, .F. ) ;
#1531 = CARTESIAN_POINT ( 'NONE',  ( -19.82816939922339117, -20.24070752338407075, 4.000000000000000000 ) ) ;
#1532 = CARTESIAN_POINT ( 'NONE',  ( -22.49999999999984368, -17.56887692260762535, 4.000000000000000000 ) ) ;
#1533 = CARTESIAN_POINT ( 'NONE',  ( -20.29289321881331887, 20.25929247661551713, 5.000000000000000000 ) ) ;
#1535 = VERTEX_POINT ( 'NONE', #126840 ) ;
#1534 = CARTESIAN_POINT ( 'NONE',  ( 22.22840764549667725, 2.499999999999998224, 3.061616997868380183E-16 ) ) ;
#1536 = VECTOR ( 'NONE', #139144, 1000.000000000000000 ) ;
#1537 = DIRECTION ( 'NONE',  ( -1.000000000000000000, -1.224606353822377258E-16, -0.000000000000000000 ) ) ;
#1538 = ORIENTED_EDGE ( 'NONE', *, *, #91976, .F. ) ;
#1539 = CARTESIAN_POINT ( 'NONE',  ( 0.000000000000000000, 0.000000000000000000, 5.000000000000000000 ) ) ;
#1540 = CARTESIAN_POINT ( 'NONE',  ( 120.7291666666666572, 7.950000000000001954, -2.130196079827421762 ) ) ;
#1541 = EDGE_CURVE ( 'NONE', #41257, #28318, #118084, .T. ) ;
#1542 = ORIENTED_EDGE ( 'NONE', *, *, #29424, .T. ) ;
#1543 = CARTESIAN_POINT ( 'NONE',  ( 54.29974487139159578, -27.71228299555243879, 4.000000000000000000 ) ) ;
#1544 = FACE_OUTER_BOUND ( 'NONE', #84083, .T. ) ;
#1545 = VECTOR ( 'NONE', #129995, 999.9999999999998863 ) ;
#1546 = ORIENTED_EDGE ( 'NONE', *, *, #130615, .T. ) ;
#1547 = CARTESIAN_POINT ( 'NONE',  ( 75.29974487139158157, -27.71228299555258445, 4.000000000000000000 ) ) ;
#1548 = ORIENTED_EDGE ( 'NONE', *, *, #13366, .F. ) ;
#1549 = LINE ( 'NONE', #133543, #97033 ) ;
#1551 = ORIENTED_EDGE ( 'NONE', *, *, #11047, .F. ) ;
#1550 = LINE ( 'NONE', #67599, #127337 ) ;
#1552 = ORIENTED_EDGE ( 'NONE', *, *, #115524, .T. ) ;
#1553 = LINE ( 'NONE', #66865, #24099 ) ;
#1554 = LINE ( 'NONE', #134264, #113081 ) ;
#1555 = ORIENTED_EDGE ( 'NONE', *, *, #87944, .T. ) ;
#1556 = CIRCLE ( 'NONE', #98752, 3.000000000000003109 ) ;
#1557 = CARTESIAN_POINT ( 'NONE',  ( -15.48921356237309510, -27.52281430457066236, 5.000000000000000000 ) ) ;
#1558 = EDGE_CURVE ( 'NONE', #44425, #11674, #7911, .T. ) ;
#1559 = EDGE_CURVE ( 'NONE', #80500, #142230, #138460, .T. ) ;
#1560 = FILL_AREA_STYLE_COLOUR ( '', #46155 ) ;
#1561 = PLANE ( 'NONE',  #90822 ) ;
#1562 = AXIS2_PLACEMENT_3D ( 'NONE', #30778, #9700, #19164 ) ;
#1563 = ORIENTED_EDGE ( 'NONE', *, *, #9139, .F. ) ;
#1564 = EDGE_CURVE ( 'NONE', #110396, #16938, #6452, .T. ) ;
#1565 = CARTESIAN_POINT ( 'NONE',  ( 47.99451991528749062, 28.92564299267971251, 4.000000000000000000 ) ) ;
#1566 = DIRECTION ( 'NONE',  ( -1.000000000000000000, 0.000000000000000000, 0.000000000000000000 ) ) ;
#1567 = FACE_OUTER_BOUND ( 'NONE', #2043, .T. ) ;
#1568 = DIRECTION ( 'NONE',  ( 0.000000000000000000, 5.075120898959323014E-15, 1.000000000000000000 ) ) ;
#1569 = CARTESIAN_POINT ( 'NONE',  ( 0.000000000000000000, 0.000000000000000000, 5.000000000000000000 ) ) ;
#1570 = DIRECTION ( 'NONE',  ( -0.7071067811865486830, -0.7071067811865464625, -0.000000000000000000 ) ) ;
#1571 = EDGE_CURVE ( 'NONE', #118176, #99074, #74643, .T. ) ;
#1573 = EDGE_CURVE ( 'NONE', #20152, #38617, #18052, .T. ) ;
#1572 = ORIENTED_EDGE ( 'NONE', *, *, #136943, .T. ) ;
#1574 = ORIENTED_EDGE ( 'NONE', *, *, #63399, .T. ) ;
#1575 = ORIENTED_EDGE ( 'NONE', *, *, #68045, .F. ) ;
#1576 = CARTESIAN_POINT ( 'NONE',  ( -23.29289321881329400, -15.74070752338412049, 5.000000000000000000 ) ) ;
#1577 = ORIENTED_EDGE ( 'NONE', *, *, #16284, .T. ) ;
#1578 = ORIENTED_EDGE ( 'NONE', *, *, #55938, .F. ) ;
#1579 = ORIENTED_EDGE ( 'NONE', *, *, #33468, .F. ) ;
#1580 = DIRECTION ( 'NONE',  ( 0.3543493200069163240, 0.000000000000000000, -0.9351131265310288487 ) ) ;
#1581 = LINE ( 'NONE', #45167, #37017 ) ;
#1582 = ORIENTED_EDGE ( 'NONE', *, *, #59458, .T. ) ;
#1583 = DIRECTION ( 'NONE',  ( 1.000000000000000000, 0.000000000000000000, 0.000000000000000000 ) ) ;
#1584 = DIRECTION ( 'NONE',  ( -0.000000000000000000, -0.000000000000000000, -1.000000000000000000 ) ) ;
#1585 = CARTESIAN_POINT ( 'NONE',  ( -9.489213562373095101, -27.52281430457062328, 5.000000000000000000 ) ) ;
#1586 = VECTOR ( 'NONE', #105774, 999.9999999999998863 ) ;
#1587 = ADVANCED_FACE ( 'NONE', ( #120969 ), #132611, .F. ) ;
#1588 = CARTESIAN_POINT ( 'NONE',  ( 34.49999999999976552, 7.087461875839180081, 4.000000000000000000 ) ) ;
#1589 = CARTESIAN_POINT ( 'NONE',  ( 118.7087635252314328, -7.482591942790329030E-16, 6.110000000000001208 ) ) ;
#1590 = ORIENTED_EDGE ( 'NONE', *, *, #135957, .F. ) ;
#1591 = ADVANCED_FACE ( 'NONE', ( #44148 ), #120223, .F. ) ;
#1592 = PLANE ( 'NONE',  #46502 ) ;
#1593 = CARTESIAN_POINT ( 'NONE',  ( 48.29974487139158867, -27.71228299555239971, 4.000000000000000000 ) ) ;
#1594 = CARTESIAN_POINT ( 'NONE',  ( -27.65671000166196336, 3.759292476615681888, 13.27625715073259194 ) ) ;
#1595 = DIRECTION ( 'NONE',  ( -0.7071067811865486830, 0.7071067811865464625, 0.000000000000000000 ) ) ;
#1596 = DIRECTION ( 'NONE',  ( -0.6830127018922180770, -0.6830127018922204085, -0.2588190451025213501 ) ) ;
#1597 = DIRECTION ( 'NONE',  ( 0.000000000000000000, -0.000000000000000000, -1.000000000000000000 ) ) ;
#1598 = AXIS2_PLACEMENT_3D ( 'NONE', #139895, #16649, #118072 ) ;
#1599 = CARTESIAN_POINT ( 'NONE',  ( 47.62086038379622011, -6.884901960086286188, 3.974999999999997424 ) ) ;
#1600 = CARTESIAN_POINT ( 'NONE',  ( 5.994519915287488843, 28.92564299267942118, 4.000000000000000000 ) ) ;
#1601 = AXIS2_PLACEMENT_3D ( 'NONE', #26769, #94857, #16595 ) ;
#1602 = DIRECTION ( 'NONE',  ( 0.000000000000000000, 0.000000000000000000, 1.000000000000000000 ) ) ;
#1603 = ORIENTED_EDGE ( 'NONE', *, *, #31102, .T. ) ;
#1604 = ORIENTED_EDGE ( 'NONE', *, *, #23536, .T. ) ;
#1605 = CARTESIAN_POINT ( 'NONE',  ( 49.70833333333332860, -3.974999999999999201, -6.884901960086287964 ) ) ;
#1606 = EDGE_CURVE ( 'NONE', #101542, #107149, #122389, .T. ) ;
#1607 = PLANE ( 'NONE',  #55491 ) ;
#1608 = VECTOR ( 'NONE', #22294, 1000.000000000000000 ) ;
#1609 = VERTEX_POINT ( 'NONE', #53599 ) ;
#1610 = EDGE_CURVE ( 'NONE', #23253, #53228, #142047, .T. ) ;
#1611 = DIRECTION ( 'NONE',  ( -0.000000000000000000, 0.3543493200069153248, 0.9351131265310292928 ) ) ;
#1612 = DIRECTION ( 'NONE',  ( 0.6830127018922181881, 0.6830127018922202975, -0.2588190451025214056 ) ) ;
#1613 = CARTESIAN_POINT ( 'NONE',  ( 34.41709685856476852, 3.054999999999998828, 5.291415217122922066 ) ) ;
#1614 = EDGE_LOOP ( 'NONE', ( #29287, #108877, #10108, #69457 ) ) ;
#1615 = ORIENTED_EDGE ( 'NONE', *, *, #82787, .F. ) ;
#1616 = EDGE_CURVE ( 'NONE', #82699, #69434, #59662, .T. ) ;
#1617 = DIRECTION ( 'NONE',  ( -0.000000000000000000, 0.3543493200069153248, 0.9351131265310291818 ) ) ;
#1618 = CARTESIAN_POINT ( 'NONE',  ( 152.4000000000000057, 26.55578643762684266, -34.51078643762689069 ) ) ;
#1619 = CARTESIAN_POINT ( 'NONE',  ( 0.000000000000000000, 0.000000000000000000, 0.000000000000000000 ) ) ;
#1620 = CARTESIAN_POINT ( 'NONE',  ( 8.510786437626906675, -27.52281430457049183, 5.000000000000000000 ) ) ;
#1621 = ORIENTED_EDGE ( 'NONE', *, *, #24503, .F. ) ;
#1622 = CARTESIAN_POINT ( 'NONE',  ( 0.000000000000000000, 0.000000000000000000, 5.000000000000000000 ) ) ;
#1623 = EDGE_LOOP ( 'NONE', ( #19991, #131981, #32246, #39871 ) ) ;
#1624 = CARTESIAN_POINT ( 'NONE',  ( -21.70679250724060694, 20.25929247661551358, 20.83292124670819945 ) ) ;
#1625 = CARTESIAN_POINT ( 'NONE',  ( -17.99451991528748351, 28.92564299267950645, 4.000000000000000000 ) ) ;
#1626 = CARTESIAN_POINT ( 'NONE',  ( 14.99999999999989875, 12.83542986846998524, -1.025386466790403794 ) ) ;
#1627 =( LENGTH_UNIT ( ) NAMED_UNIT ( * ) SI_UNIT ( .MILLI., .METRE. ) );
#1629 = ADVANCED_FACE ( 'NONE', ( #78207 ), #99948, .F. ) ;
#1628 = VECTOR ( 'NONE', #36666, 1000.000000000000000 ) ;
#1630 = DIRECTION ( 'NONE',  ( -0.000000000000000000, 0.3543493200069153248, 0.9351131265310292928 ) ) ;
#1631 = CARTESIAN_POINT ( 'NONE',  ( -14.27718569542929572, -21.72500000000000142, 5.000000000000000000 ) ) ;
#1632 = EDGE_CURVE ( 'NONE', #89964, #137620, #86935, .T. ) ;
#1633 = ORIENTED_EDGE ( 'NONE', *, *, #32152, .F. ) ;
#1634 = AXIS2_PLACEMENT_3D ( 'NONE', #4478, #124902, #27010 ) ;
#1635 = DIRECTION ( 'NONE',  ( 1.000000000000000000, 0.000000000000000000, 0.000000000000000000 ) ) ;
#1636 = CARTESIAN_POINT ( 'NONE',  ( 61.89126352523144448, -4.472830434245839371, -4.472830434245839371 ) ) ;
#1637 = FACE_OUTER_BOUND ( 'NONE', #32238, .T. ) ;
#1638 = LINE ( 'NONE', #33623, #110266 ) ;
#1639 = CARTESIAN_POINT ( 'NONE',  ( 26.75159235450331963, 9.902892378096218942E-16, 0.000000000000000000 ) ) ;
#1640 = ORIENTED_EDGE ( 'NONE', *, *, #64059, .T. ) ;
#1641 = VECTOR ( 'NONE', #73871, 1000.000000000000000 ) ;
#1642 = FACE_OUTER_BOUND ( 'NONE', #17218, .T. ) ;
#1643 = EDGE_CURVE ( 'NONE', #48159, #126178, #54335, .T. ) ;
#1644 = ORIENTED_EDGE ( 'NONE', *, *, #29808, .T. ) ;
#1645 = DIRECTION ( 'NONE',  ( -0.000000000000000000, -1.000000000000000000, 0.000000000000000000 ) ) ;
#1646 = VERTEX_POINT ( 'NONE', #108636 ) ;
#1647 = CARTESIAN_POINT ( 'NONE',  ( -10.49999999999993250, 9.431123077392092213, 4.000000000000000000 ) ) ;
#1648 = CARTESIAN_POINT ( 'NONE',  ( -22.17183060077631396, -20.24070752338407786, 4.000000000000000000 ) ) ;
#1649 = AXIS2_PLACEMENT_3D ( 'NONE', #62270, #141227, #120158 ) ;
#1650 = DIRECTION ( 'NONE',  ( -0.000000000000000000, 0.3543493200069153248, 0.9351131265310292928 ) ) ;
#1651 = DIRECTION ( 'NONE',  ( 0.3543493200069162685, -0.000000000000000000, -0.9351131265310288487 ) ) ;
#1652 = FACE_BOUND ( 'NONE', #21354, .T. ) ;
#1653 = CARTESIAN_POINT ( 'NONE',  ( 34.92499999999998295, 3.006123077391939624, 4.000000000000000000 ) ) ;
#1654 = CARTESIAN_POINT ( 'NONE',  ( 17.99999999999987566, -11.35517001088070366, -1.126524801160067479 ) ) ;
#1655 = CARTESIAN_POINT ( 'NONE',  ( -0.7071067811865415775, 14.25929247661557397, 5.000000000000000000 ) ) ;
#1657 = ORIENTED_EDGE ( 'NONE', *, *, #84019, .T. ) ;
#1656 = LINE ( 'NONE', #111143, #4130 ) ;
#1658 = DIRECTION ( 'NONE',  ( 0.6830127018922181881, 0.6830127018922202975, -0.2588190451025214056 ) ) ;
#1659 = VERTEX_POINT ( 'NONE', #97039 ) ;
#1660 = VERTEX_POINT ( 'NONE', #44906 ) ;
#1661 = CARTESIAN_POINT ( 'NONE',  ( 77.05793019189812298, 6.110000000000000320, -1.637169565754156064 ) ) ;
#1662 = ORIENTED_EDGE ( 'NONE', *, *, #90642, .F. ) ;
#1663 = DIRECTION ( 'NONE',  ( 0.7071067811865487940, 0.7071067811865463515, 0.000000000000000000 ) ) ;
#1664 = EDGE_CURVE ( 'NONE', #55674, #57540, #75352, .T. ) ;
#1665 = ORIENTED_EDGE ( 'NONE', *, *, #13788, .F. ) ;
#1666 = DIRECTION ( 'NONE',  ( 0.7071067811865487940, 0.7071067811865463515, 0.000000000000000000 ) ) ;
#1667 = DIRECTION ( 'NONE',  ( 0.7071067811865487940, -0.7071067811865463515, 0.000000000000000000 ) ) ;
#1668 = CARTESIAN_POINT ( 'NONE',  ( 17.53719725875415847, -2.055000000000000160, 2.789133085058097101E-16 ) ) ;
#1670 = CARTESIAN_POINT ( 'NONE',  ( 57.18398860626899705, 28.73617430169827358, 5.000000000000000000 ) ) ;
#1669 = LINE ( 'NONE', #80037, #29651 ) ;
#1671 = DIRECTION ( 'NONE',  ( 0.5735764363510448272, -0.8191520442889927978, 1.003171929053526103E-16 ) ) ;
#1672 = CARTESIAN_POINT ( 'NONE',  ( 28.99999999999999645, 0.000000000000000000, -7.950000000000000178 ) ) ;
#1673 = VERTEX_POINT ( 'NONE', #141295 ) ;
#1674 = VERTEX_POINT ( 'NONE', #20936 ) ;
#1675 = CARTESIAN_POINT ( 'NONE',  ( -6.183988606268994381, 28.73617430169791476, 5.000000000000000000 ) ) ;
#1676 = CARTESIAN_POINT ( 'NONE',  ( 16.49999999999988276, -19.53360074219753884, 5.000000000000000000 ) ) ;
#1677 = ORIENTED_EDGE ( 'NONE', *, *, #96020, .T. ) ;
#1678 = ORIENTED_EDGE ( 'NONE', *, *, #119738, .T. ) ;
#1680 = ORIENTED_EDGE ( 'NONE', *, *, #101176, .T. ) ;
#1679 = VECTOR ( 'NONE', #128806, 999.9999999999998863 ) ;
#1681 = ADVANCED_FACE ( 'NONE', ( #99196 ), #119515, .F. ) ;
#1682 = EDGE_CURVE ( 'NONE', #98221, #131683, #65923, .T. ) ;
#1683 = LINE ( 'NONE', #88030, #104022 ) ;
#1684 = ORIENTED_EDGE ( 'NONE', *, *, #62219, .F. ) ;
#1685 = DIRECTION ( 'NONE',  ( -0.3543493200069162685, -0.000000000000000000, -0.9351131265310288487 ) ) ;
#1687 = EDGE_CURVE ( 'NONE', #77069, #96033, #119634, .T. ) ;
#1686 = VECTOR ( 'NONE', #62693, 1000.000000000000000 ) ;
#1688 = CARTESIAN_POINT ( 'NONE',  ( 43.39169371712955581, 2.130196079827421762, 7.950000000000000178 ) ) ;
#1689 = VECTOR ( 'NONE', #126123, 1000.000000000000227 ) ;
#1690 = CARTESIAN_POINT ( 'NONE',  ( -1.245430191898114103, -6.871911579029512218, 3.967499999999996252 ) ) ;
#1691 = CARTESIAN_POINT ( 'NONE',  ( 18.18398860626898994, 28.73617430169800002, 5.000000000000000000 ) ) ;
#1692 = ORIENTED_EDGE ( 'NONE', *, *, #17914, .F. ) ;
#1693 = EDGE_CURVE ( 'NONE', #52394, #129216, #31831, .T. ) ;
#1694 = DIRECTION ( 'NONE',  ( -1.000000000000000000, 0.000000000000000000, 0.000000000000000000 ) ) ;
#1695 = VECTOR ( 'NONE', #83896, 1000.000000000000000 ) ;
#1696 = CYLINDRICAL_SURFACE ( 'NONE', #100786, 0.5000000000000004441 ) ;
#1698 = ORIENTED_EDGE ( 'NONE', *, *, #97815, .F. ) ;
#1697 = CARTESIAN_POINT ( 'NONE',  ( -34.92500000000001137, 22.22500000000000142, 4.000000000000000000 ) ) ;
#1699 = ORIENTED_EDGE ( 'NONE', *, *, #53805, .T. ) ;
#1700 = CARTESIAN_POINT ( 'NONE',  ( 26.99999999999981526, -4.068876922607768343, 4.000000000000000000 ) ) ;
#1701 = DIRECTION ( 'NONE',  ( -1.000000000000000000, -1.224606353822377258E-16, -0.000000000000000000 ) ) ;
#1702 = EDGE_CURVE ( 'NONE', #79902, #3869, #143436, .T. ) ;
#1703 = ORIENTED_EDGE ( 'NONE', *, *, #44316, .T. ) ;
#1704 = CARTESIAN_POINT ( 'NONE',  ( 0.000000000000000000, 0.000000000000000000, 5.000000000000000000 ) ) ;
#1705 = CARTESIAN_POINT ( 'NONE',  ( 33.18398860626899705, 28.73617430169810305, 5.000000000000000000 ) ) ;
#1706 = CARTESIAN_POINT ( 'NONE',  ( -32.99999999999977263, 16.55218569542899587, 5.000000000000000000 ) ) ;
#1707 = CARTESIAN_POINT ( 'NONE',  ( 30.29974487139158867, -27.71228299555227537, 4.000000000000000000 ) ) ;
#1708 = DIRECTION ( 'NONE',  ( -0.7071067811865486830, -0.7071067811865464625, 0.000000000000000000 ) ) ;
#1709 = EDGE_CURVE ( 'NONE', #103522, #39262, #65203, .T. ) ;
#1710 = DIRECTION ( 'NONE',  ( -0.000000000000000000, -0.3543493200069152693, 0.9351131265310292928 ) ) ;
#1711 = LINE ( 'NONE', #46005, #139612 ) ;
#1712 =( BOUNDED_CURVE ( )  B_SPLINE_CURVE ( 3, ( #120647, #21366, #129390, #65627 ),
 .UNSPECIFIED., .F., .T. ) 
 B_SPLINE_CURVE_WITH_KNOTS ( ( 4, 4 ),
 ( 5.106027341939290309, 6.645403452391245303 ),
 .UNSPECIFIED. ) 
 CURVE ( )  GEOMETRIC_REPRESENTATION_ITEM ( )  RATIONAL_B_SPLINE_CURVE ( ( 1.000000000000000000, 0.8120851936182301722, 0.8120851936182301722, 1.000000000000000000 ) ) 
 REPRESENTATION_ITEM ( '' )  );
#1713 = CARTESIAN_POINT ( 'NONE',  ( -29.99451991528749417, 28.92564299267958816, 4.000000000000000000 ) ) ;
#1714 = LINE ( 'NONE', #24927, #21617 ) ;
#1715 = LINE ( 'NONE', #124964, #73800 ) ;
#1716 = ORIENTED_EDGE ( 'NONE', *, *, #58492, .T. ) ;
#1717 = ORIENTED_EDGE ( 'NONE', *, *, #28800, .T. ) ;
#1718 = VECTOR ( 'NONE', #35110, 1000.000000000000000 ) ;
#1719 = ADVANCED_FACE ( 'NONE', ( #55742 ), #133309, .F. ) ;
#1720 = PLANE ( 'NONE',  #131344 ) ;
#1721 = CYLINDRICAL_SURFACE ( 'NONE', #111874, 2.500000000000000444 ) ;
#1722 = SURFACE_SIDE_STYLE ('',( #57606 ) ) ;
#1723 = VECTOR ( 'NONE', #137650, 1000.000000000000000 ) ;
#1724 = ORIENTED_EDGE ( 'NONE', *, *, #60406, .F. ) ;
#1725 = DIRECTION ( 'NONE',  ( -0.7071067811865486830, -0.7071067811865464625, 0.000000000000000000 ) ) ;
#1726 = CARTESIAN_POINT ( 'NONE',  ( -3.489213562373097322, -27.52281430457057709, 5.000000000000000000 ) ) ;
#1727 = CARTESIAN_POINT ( 'NONE',  ( 13.11547925347946908, 3.815643823912585386, 4.000000000000000000 ) ) ;
#1728 = ORIENTED_EDGE ( 'NONE', *, *, #127304, .F. ) ;
#1729 = EDGE_CURVE ( 'NONE', #126528, #115378, #92612, .T. ) ;
#1730 = CARTESIAN_POINT ( 'NONE',  ( 25.49999999999982236, 11.52377502935405040, -1.522421517564144677 ) ) ;
#1731 = CARTESIAN_POINT ( 'NONE',  ( -17.99999999999986855, -12.03360074219761700, 5.000000000000000000 ) ) ;
#1732 = CARTESIAN_POINT ( 'NONE',  ( 0.000000000000000000, -43.14999999999996305, -31.92499999999998295 ) ) ;
#1733 =( LENGTH_UNIT ( ) NAMED_UNIT ( * ) SI_UNIT ( .MILLI., .METRE. ) );
#1734 = CARTESIAN_POINT ( 'NONE',  ( 57.37043019189810877, -3.055000000000001936, 5.291415217122918513 ) ) ;
#1735 = FACE_OUTER_BOUND ( 'NONE', #37412, .T. ) ;
#1736 = EDGE_CURVE ( 'NONE', #13171, #91632, #91912, .T. ) ;
#1737 = EDGE_CURVE ( 'NONE', #29835, #121898, #14362, .T. ) ;
#1738 = DIRECTION ( 'NONE',  ( 0.000000000000000000, 1.000000000000000000, 0.000000000000000000 ) ) ;
#1739 = ORIENTED_EDGE ( 'NONE', *, *, #63831, .T. ) ;
#1740 = LINE ( 'NONE', #88821, #118233 ) ;
#1741 = ORIENTED_EDGE ( 'NONE', *, *, #83327, .T. ) ;
#1742 = CARTESIAN_POINT ( 'NONE',  ( 9.773048296453090700, -22.22500000000000142, -11.93776140031427602 ) ) ;
#1743 = ADVANCED_FACE ( 'NONE', ( #47745 ), #12913, .T. ) ;
#1744 = CARTESIAN_POINT ( 'NONE',  ( 0.000000000000000000, 0.000000000000000000, 0.000000000000000000 ) ) ;
#1745 = DIRECTION ( 'NONE',  ( -0.7071067811865486830, -0.7071067811865464625, 0.000000000000000000 ) ) ;
#1746 = DIRECTION ( 'NONE',  ( 0.7071067811865487940, -0.7071067811865463515, 0.000000000000000000 ) ) ;
#1747 = EDGE_CURVE ( 'NONE', #65901, #96557, #134750, .T. ) ;
#1748 = CARTESIAN_POINT ( 'NONE',  ( 17.20666063542140733, 21.75929247661550292, 4.998822639870701856 ) ) ;
#1749 = CARTESIAN_POINT ( 'NONE',  ( -34.92500000000001137, 16.70193056682083821, 4.500000000000000888 ) ) ;
#1750 = EDGE_LOOP ( 'NONE', ( #22599, #112914, #20807, #113972 ) ) ;
#1751 = ORIENTED_EDGE ( 'NONE', *, *, #15487, .T. ) ;
#1752 = LINE ( 'NONE', #24960, #2657 ) ;
#1753 = CARTESIAN_POINT ( 'NONE',  ( -30.70710678118632231, 2.259292476615694323, 5.000000000000000000 ) ) ;
#1754 = CARTESIAN_POINT ( 'NONE',  ( -21.32816939922336985, -6.740707523384218192, 4.000000000000000000 ) ) ;
#1755 = LINE ( 'NONE', #143198, #115332 ) ;
#1756 = CARTESIAN_POINT ( 'NONE',  ( 79.41252705046289861, -7.949999999999998401, -4.867971026610728450E-16 ) ) ;
#1757 = CARTESIAN_POINT ( 'NONE',  ( -1.499999999999977129, 4.087461875839200509, 4.000000000000000000 ) ) ;
#1758 = CARTESIAN_POINT ( 'NONE',  ( 7.940000000000001279, -35.14999999999999858, -10.00000000000000178 ) ) ;
#1759 = ORIENTED_EDGE ( 'NONE', *, *, #15923, .F. ) ;
#1760 = VECTOR ( 'NONE', #139576, 1000.000000000000000 ) ;
#1761 = CARTESIAN_POINT ( 'NONE',  ( 71.58333333333332860, 6.884901960086290629, -3.974999999999994316 ) ) ;
#1762 = EDGE_CURVE ( 'NONE', #28277, #97071, #2761, .T. ) ;
#1763 = FACE_OUTER_BOUND ( 'NONE', #86238, .T. ) ;
#1764 = CARTESIAN_POINT ( 'NONE',  ( -48.48921356237309510, -27.52281430457089328, 5.000000000000000000 ) ) ;
#1765 = LINE ( 'NONE', #89536, #119185 ) ;
#1766 = EDGE_LOOP ( 'NONE', ( #106955, #105624, #92568, #12610 ) ) ;
#1767 = EDGE_CURVE ( 'NONE', #9326, #100143, #125539, .T. ) ;
#1768 = CARTESIAN_POINT ( 'NONE',  ( -30.70710678118633652, -6.740707523384211086, 5.000000000000000000 ) ) ;
#1769 = VECTOR ( 'NONE', #10352, 999.9999999999998863 ) ;
#1770 = CARTESIAN_POINT ( 'NONE',  ( -19.05000000000000071, 3.174999999999997158, 4.000000000000000000 ) ) ;
#1771 = CARTESIAN_POINT ( 'NONE',  ( 69.41709685856477563, 3.054999999999998828, 5.291415217122922066 ) ) ;
#1772 = ORIENTED_EDGE ( 'NONE', *, *, #17406, .T. ) ;
#1773 = ORIENTED_EDGE ( 'NONE', *, *, #82459, .T. ) ;
#1774 = VECTOR ( 'NONE', #115632, 1000.000000000000000 ) ;
#1775 = CARTESIAN_POINT ( 'NONE',  ( 12.19999999999999574, -25.83999999999997499, -40.00000000000000711 ) ) ;
#1776 = CARTESIAN_POINT ( 'NONE',  ( 6.156123077392376963, -22.22500000000000142, 4.000000000000000000 ) ) ;
#1777 = VECTOR ( 'NONE', #117043, 999.9999999999998863 ) ;
#1778 = CARTESIAN_POINT ( 'NONE',  ( 8.683420388672054457, -6.740707523384212863, 11.88629033278122371 ) ) ;
#1779 = DIRECTION ( 'NONE',  ( 0.6830127018922180770, -0.6830127018922204085, -0.2588190451025213501 ) ) ;
#1781 = EDGE_LOOP ( 'NONE', ( #23977, #96409, #94986, #23094, #121520 ) ) ;
#1780 = CARTESIAN_POINT ( 'NONE',  ( 3.299744871391591339, -27.71228299555208352, 4.000000000000000000 ) ) ;
#1782 = DIRECTION ( 'NONE',  ( -1.000000000000000000, -1.224606353822377258E-16, -0.000000000000000000 ) ) ;
#1783 = CARTESIAN_POINT ( 'NONE',  ( -21.48921356237309155, -27.52281430457070499, 5.000000000000000000 ) ) ;
#1784 = LINE ( 'NONE', #385, #98027 ) ;
#1785 = AXIS2_PLACEMENT_3D ( 'NONE', #35089, #112621, #3130 ) ;
#1786 = PLANE ( 'NONE',  #115501 ) ;
#1787 = VECTOR ( 'NONE', #44345, 1000.000000000000000 ) ;
#1788 = VERTEX_POINT ( 'NONE', #47059 ) ;
#1789 = EDGE_CURVE ( 'NONE', #98679, #119012, #89647, .T. ) ;
#1790 = EDGE_LOOP ( 'NONE', ( #29145, #85466, #31293, #139892 ) ) ;
#1791 = CARTESIAN_POINT ( 'NONE',  ( 54.83376352523143282, 6.110000000000001208, 1.122388791418549305E-15 ) ) ;
#1792 = VERTEX_POINT ( 'NONE', #126670 ) ;
#1793 = FACE_OUTER_BOUND ( 'NONE', #42063, .T. ) ;
#1794 = ADVANCED_FACE ( 'NONE', ( #106327 ), #93350, .F. ) ;
#1795 = CARTESIAN_POINT ( 'NONE',  ( 33.18398860626899705, 28.73617430169810305, 5.000000000000000000 ) ) ;
#1796 = DIRECTION ( 'NONE',  ( 1.000000000000000000, 1.224606353822377258E-16, 0.000000000000000000 ) ) ;
#1797 = DIRECTION ( 'NONE',  ( -0.7071067811865486830, -0.7071067811865464625, -0.000000000000000000 ) ) ;
#1798 = CARTESIAN_POINT ( 'NONE',  ( 32.29289321881323360, 14.25929247661557397, 5.000000000000000000 ) ) ;
#1799 = VERTEX_POINT ( 'NONE', #51288 ) ;
#1800 = VERTEX_POINT ( 'NONE', #105620 ) ;
#1801 = CARTESIAN_POINT ( 'NONE',  ( -9.183988606268997046, 28.73617430169793607, 5.000000000000000000 ) ) ;
#1802 = CARTESIAN_POINT ( 'NONE',  ( -17.54957349249705345, -3.270000000000005347, -36.39086428169088094 ) ) ;
#1803 = VERTEX_POINT ( 'NONE', #51995 ) ;
#1804 = CARTESIAN_POINT ( 'NONE',  ( -35.99451991528749772, 28.92564299267963079, 4.000000000000000000 ) ) ;
#1805 = CARTESIAN_POINT ( 'NONE',  ( 112.6625270504628986, 7.949999999999998401, 1.460391307983218338E-15 ) ) ;
#1806 = PLANE ( 'NONE',  #118803 ) ;
#1807 = EDGE_LOOP ( 'NONE', ( #12046, #120511, #128816, #44564 ) ) ;
#1808 = FACE_BOUND ( 'NONE', #103518, .T. ) ;
#1809 = CARTESIAN_POINT ( 'NONE',  ( 23.67183060077630685, -18.74070752338408852, 4.000000000000000000 ) ) ;
#1810 = CARTESIAN_POINT ( 'NONE',  ( 0.000000000000000000, 21.72500000000000142, 4.500000000000000888 ) ) ;
#1811 = LINE ( 'NONE', #78723, #89881 ) ;
#1812 = VECTOR ( 'NONE', #141508, 1000.000000000000000 ) ;
#1813 = DIRECTION ( 'NONE',  ( -0.000000000000000000, 0.000000000000000000, 1.000000000000000000 ) ) ;
#1814 = DIRECTION ( 'NONE',  ( -0.7071067811865486830, -0.7071067811865464625, 0.000000000000000000 ) ) ;
#1815 = DIRECTION ( 'NONE',  ( 0.2920961682182654506, 0.000000000000000000, 0.9563889525251777490 ) ) ;
#1816 = ORIENTED_EDGE ( 'NONE', *, *, #24259, .T. ) ;
#1817 = ORIENTED_EDGE ( 'NONE', *, *, #37742, .T. ) ;
#1818 = CARTESIAN_POINT ( 'NONE',  ( 105.2037635252314516, 6.109999999999998543, 1.122388791418548911E-15 ) ) ;
#1819 =( BOUNDED_SURFACE ( )  B_SPLINE_SURFACE ( 3, 2, ( 
 ( #75238, #141164, #5640 ),
 ( #30275, #8477, #72404 ),
 ( #73785, #50607, #62935 ),
 ( #52728, #28860, #94792 ),
 ( #40465, #19397, #96921 ),
 ( #63650, #52038, #84666 ),
 ( #117253, #128868, #116573 ),
 ( #7786, #119399, #17258 ),
 ( #20093, #61519, #96217 ),
 ( #7051, #139052, #62213 ),
 ( #106368, #104975, #29544 ),
 ( #140459, #41150, #118705 ) ),
 .UNSPECIFIED., .F., .F., .F. ) 
 B_SPLINE_SURFACE_WITH_KNOTS ( ( 4, 2, 2, 2, 2, 4 ),
 ( 3, 3 ),
 ( 0.000000000000000000, 0.001647923167088021293, 0.002471884750632031939, 0.003295846334176042586, 0.004943769501264063879, 0.006591692668352085172 ),
 ( 0.000000000000000000, 1.000000000000000000 ),
 .UNSPECIFIED. ) 
 GEOMETRIC_REPRESENTATION_ITEM ( )  RATIONAL_B_SPLINE_SURFACE ( (
 ( 1.000000000000000000, 0.7071067811865475727, 1.000000000000000000),
 ( 1.000000000000000000, 0.7122033721489959834, 1.000000000000000000),
 ( 1.000000000000000000, 0.7158366153114920083, 1.000000000000000000),
 ( 1.000000000000000000, 0.7192720032935927543, 1.000000000000000000),
 ( 1.000000000000000000, 0.7200809050419634261, 1.000000000000000000),
 ( 1.000000000000000000, 0.7210491446662590231, 1.000000000000000000),
 ( 1.000000000000000000, 0.7212054070301950892, 1.000000000000000000),
 ( 1.000000000000000000, 0.7207522793911053105, 1.000000000000000000),
 ( 1.000000000000000000, 0.7192424821648278899, 1.000000000000000000),
 ( 1.000000000000000000, 0.7143802006615703748, 1.000000000000000000),
 ( 1.000000000000000000, 0.7109884861396060796, 1.000000000000000000),
 ( 1.000000000000000000, 0.7071067811865475727, 1.000000000000000000) ) ) 
 REPRESENTATION_ITEM ( '' )  SURFACE ( )  );
#1820 = ORIENTED_EDGE ( 'NONE', *, *, #126955, .F. ) ;
#1821 = DIRECTION ( 'NONE',  ( -0.6830127018922180770, -0.6830127018922204085, -0.2588190451025213501 ) ) ;
#1822 = ORIENTED_EDGE ( 'NONE', *, *, #97515, .F. ) ;
#1823 = DIRECTION ( 'NONE',  ( -1.000000000000000000, 0.000000000000000000, 0.000000000000000000 ) ) ;
#1824 = CARTESIAN_POINT ( 'NONE',  ( 3.108306282870440640, 1.633150327867692431, -6.094999999999989093 ) ) ;
#1825 = AXIS2_PLACEMENT_3D ( 'NONE', #125722, #80092, #24940 ) ;
#1826 = CARTESIAN_POINT ( 'NONE',  ( -5.149948714589728915, -8.240707523384200428, 17.25253755692238045 ) ) ;
#1827 = ORIENTED_EDGE ( 'NONE', *, *, #5420, .T. ) ;
#1828 = DIRECTION ( 'NONE',  ( -1.000000000000000000, -1.224606353822377258E-16, -0.000000000000000000 ) ) ;
#1829 = LINE ( 'NONE', #33134, #132951 ) ;
#1830 = CARTESIAN_POINT ( 'NONE',  ( -24.48921356237309510, -27.52281430457072631, 5.000000000000000000 ) ) ;
#1832 = CARTESIAN_POINT ( 'NONE',  ( 27.18398860626900060, 28.73617430169806042, 5.000000000000000000 ) ) ;
#1831 = CARTESIAN_POINT ( 'NONE',  ( 68.52083333333334281, 7.949999999999998401, 2.130196079827431532 ) ) ;
#1833 = CARTESIAN_POINT ( 'NONE',  ( -9.183988606268997046, 28.73617430169793607, 5.000000000000000000 ) ) ;
#1834 = LINE ( 'NONE', #2580, #127794 ) ;
#1835 = ORIENTED_EDGE ( 'NONE', *, *, #137418, .F. ) ;
#1836 = CARTESIAN_POINT ( 'NONE',  ( -6.328169399223481761, -21.74070752338406365, 4.000000000000000000 ) ) ;
#1837 = LINE ( 'NONE', #33829, #212 ) ;
#1838 = EDGE_CURVE ( 'NONE', #135322, #113494, #38966, .T. ) ;
#1839 = VERTEX_POINT ( 'NONE', #82484 ) ;
#1840 = EDGE_LOOP ( 'NONE', ( #96030, #136405, #78599, #23348 ) ) ;
#1841 = EDGE_CURVE ( 'NONE', #106517, #37184, #29500, .T. ) ;
#1842 = ADVANCED_FACE ( 'NONE', ( #41108 ), #139007, .F. ) ;
#1843 = ORIENTED_EDGE ( 'NONE', *, *, #82528, .F. ) ;
#1844 = CARTESIAN_POINT ( 'NONE',  ( 50.60459685856477563, 1.637169565754164946, -6.109999999999999432 ) ) ;
#1845 = ORIENTED_EDGE ( 'NONE', *, *, #72695, .F. ) ;
#1846 = EDGE_CURVE ( 'NONE', #16129, #113816, #38263, .T. ) ;
#1847 = EDGE_CURVE ( 'NONE', #93168, #108750, #28817, .T. ) ;
#1848 = DIRECTION ( 'NONE',  ( -0.7071067811865486830, 0.7071067811865464625, 0.000000000000000000 ) ) ;
#1849 = CARTESIAN_POINT ( 'NONE',  ( 3.545806282870439308, 5.278424836066143655, -3.047499999999997655 ) ) ;
#1850 = AXIS2_PLACEMENT_3D ( 'NONE', #129361, #43799, #119892 ) ;
#1851 = CARTESIAN_POINT ( 'NONE',  ( 91.87543019189811844, -5.291415217122920289, -3.055000000000001492 ) ) ;
#1852 = CARTESIAN_POINT ( 'NONE',  ( -78.48921356237309510, -27.52281430457109934, 5.000000000000000000 ) ) ;
#1853 = EDGE_LOOP ( 'NONE', ( #108366, #141116, #110679, #48056 ) ) ;
#1854 = EDGE_CURVE ( 'NONE', #75714, #41182, #129526, .T. ) ;
#1855 = CARTESIAN_POINT ( 'NONE',  ( -32.20710678118631876, 0.7592924766157104211, 5.000000000000000000 ) ) ;
#1856 = ORIENTED_EDGE ( 'NONE', *, *, #134942, .T. ) ;
#1857 = CARTESIAN_POINT ( 'NONE',  ( 156.1500000000000057, -49.14999999999999147, -49.92499999999968452 ) ) ;
#1858 = CARTESIAN_POINT ( 'NONE',  ( 51.48921356237309510, -27.52281430457091460, 5.000000000000000000 ) ) ;
#1859 = VERTEX_POINT ( 'NONE', #40419 ) ;
#1860 = PLANE ( 'NONE',  #34474 ) ;
#1861 = DIRECTION ( 'NONE',  ( 1.000000000000000000, 0.000000000000000000, 0.000000000000000000 ) ) ;
#1862 = EDGE_CURVE ( 'NONE', #55140, #78905, #60023, .T. ) ;
#1863 = ORIENTED_EDGE ( 'NONE', *, *, #76673, .F. ) ;
#1864 = DIRECTION ( 'NONE',  ( -0.7071067811865487940, 0.7071067811865463515, -0.000000000000000000 ) ) ;
#1865 = ORIENTED_EDGE ( 'NONE', *, *, #43373, .F. ) ;
#1866 = ORIENTED_EDGE ( 'NONE', *, *, #71450, .T. ) ;
#1867 = ORIENTED_EDGE ( 'NONE', *, *, #125021, .T. ) ;
#1868 = EDGE_CURVE ( 'NONE', #22900, #79079, #30247, .T. ) ;
#1869 = VECTOR ( 'NONE', #52045, 1000.000000000000000 ) ;
#1870 = VECTOR ( 'NONE', #61137, 1000.000000000000000 ) ;
#1871 = DIRECTION ( 'NONE',  ( 0.7071067811865487940, 0.7071067811865463515, 0.000000000000000000 ) ) ;
#1872 = LINE ( 'NONE', #124421, #106488 ) ;
#1873 = DIRECTION ( 'NONE',  ( 0.6830127018922180770, -0.6830127018922204085, -0.2588190451025213501 ) ) ;
#1874 = ORIENTED_EDGE ( 'NONE', *, *, #45875, .T. ) ;
#1875 = EDGE_CURVE ( 'NONE', #30242, #132436, #7743, .T. ) ;
#1876 = EDGE_CURVE ( 'NONE', #109399, #16896, #4856, .T. ) ;
#1877 = AXIS2_PLACEMENT_3D ( 'NONE', #42932, #55954, #120423 ) ;
#1878 = AXIS2_PLACEMENT_3D ( 'NONE', #106341, #115778, #17899 ) ;
#1879 = DIRECTION ( 'NONE',  ( -0.000000000000000000, 0.000000000000000000, 1.000000000000000000 ) ) ;
#1880 =( BOUNDED_CURVE ( )  B_SPLINE_CURVE ( 3, ( #114115, #125727, #59759, #80096 ),
 .UNSPECIFIED., .F., .T. ) 
 B_SPLINE_CURVE_WITH_KNOTS ( ( 4, 4 ),
 ( 2.779374508378134045, 4.199602562396838934 ),
 .UNSPECIFIED. ) 
 CURVE ( )  GEOMETRIC_REPRESENTATION_ITEM ( )  RATIONAL_B_SPLINE_CURVE ( ( 1.000000000000000000, 0.8388583629366626049, 0.8388583629366626049, 1.000000000000000000 ) ) 
 REPRESENTATION_ITEM ( '' )  );
#1881 = CARTESIAN_POINT ( 'NONE',  ( 23.74956980810188867, 3.967499999999998916, 6.871911579029510442 ) ) ;
#1882 = CARTESIAN_POINT ( 'NONE',  ( 14.99999999999989342, -13.97847968911258931, -0.1324546996126444443 ) ) ;
#1883 = DIRECTION ( 'NONE',  ( 0.3543493200069162685, -0.000000000000000000, -0.9351131265310288487 ) ) ;
#1884 = CARTESIAN_POINT ( 'NONE',  ( -32.59703385998916758, 22.27000000000000668, -14.57157165008255006 ) ) ;
#1885 = VERTEX_POINT ( 'NONE', #137576 ) ;
#1886 = VERTEX_POINT ( 'NONE', #83192 ) ;
#1888 = ORIENTED_EDGE ( 'NONE', *, *, #141103, .F. ) ;
#1887 = EDGE_CURVE ( 'NONE', #57582, #134641, #71607, .T. ) ;
#1889 = FILL_AREA_STYLE ('',( #136727 ) ) ;
#1890 = CARTESIAN_POINT ( 'NONE',  ( 0.000000000000000000, 0.000000000000000000, 0.000000000000000000 ) ) ;
#1891 = AXIS2_PLACEMENT_3D ( 'NONE', #6712, #50996, #37990 ) ;
#1892 = FACE_OUTER_BOUND ( 'NONE', #24783, .T. ) ;
#1893 = SURFACE_SIDE_STYLE ('',( #93240 ) ) ;
#1894 = CARTESIAN_POINT ( 'NONE',  ( 0.000000000000000000, 0.000000000000000000, 5.000000000000000000 ) ) ;
#1895 = ADVANCED_FACE ( 'NONE', ( #16470 ), #60770, .F. ) ;
#1897 = CARTESIAN_POINT ( 'NONE',  ( 9.005480084712511157, 28.92564299267931816, 4.000000000000000000 ) ) ;
#1896 = VECTOR ( 'NONE', #89011, 1000.000000000000000 ) ;
#1898 = DIRECTION ( 'NONE',  ( 0.000000000000000000, 0.000000000000000000, 1.000000000000000000 ) ) ;
#1899 = DIRECTION ( 'NONE',  ( -1.000000000000000000, -0.000000000000000000, -0.000000000000000000 ) ) ;
#1900 = CARTESIAN_POINT ( 'NONE',  ( -24.48921356237309510, -27.52281430457072631, 5.000000000000000000 ) ) ;
#1901 = ADVANCED_FACE ( 'NONE', ( #28093 ), #72360, .F. ) ;
#1902 = LINE ( 'NONE', #504, #115948 ) ;
#1903 = ORIENTED_EDGE ( 'NONE', *, *, #103057, .F. ) ;
#1904 = VECTOR ( 'NONE', #36226, 1000.000000000000227 ) ;
#1905 =( NAMED_UNIT ( * ) SI_UNIT ( $, .STERADIAN. ) SOLID_ANGLE_UNIT ( ) );
#1906 = ORIENTED_EDGE ( 'NONE', *, *, #19958, .T. ) ;
#1908 = EDGE_CURVE ( 'NONE', #51825, #93361, #134880, .T. ) ;
#1907 = COLOUR_RGB ( '', 0.31764706, 0.68627451, 0.89019608) ;
#1909 = CIRCLE ( 'NONE', #85349, 1.000000000000000888 ) ;
#1910 = CARTESIAN_POINT ( 'NONE',  ( 8.510786437626906675, -27.52281430457049183, 5.000000000000000000 ) ) ;
#1912 = EDGE_LOOP ( 'NONE', ( #110003, #108495, #107348, #26014 ) ) ;
#1911 = DIRECTION ( 'NONE',  ( 0.7071067811865486830, -0.7071067811865464625, -0.000000000000000000 ) ) ;
#1913 = SURFACE_STYLE_USAGE ( .BOTH. , #78832 ) ;
#1914 = CARTESIAN_POINT ( 'NONE',  ( 7.499999999999951150, -6.839392718269120763, -8.480912228396103814 ) ) ;
#1915 = ORIENTED_EDGE ( 'NONE', *, *, #99339, .T. ) ;
#1916 = LINE ( 'NONE', #34603, #4461 ) ;
#1917 = ORIENTED_EDGE ( 'NONE', *, *, #129818, .F. ) ;
#1918 = CARTESIAN_POINT ( 'NONE',  ( -3.489213562373097322, -27.52281430457057709, 5.000000000000000000 ) ) ;
#1919 = ORIENTED_EDGE ( 'NONE', *, *, #78418, .T. ) ;
#1920 = EDGE_CURVE ( 'NONE', #135518, #143125, #124680, .T. ) ;
#1921 = DIRECTION ( 'NONE',  ( 0.000000000000000000, -1.000000000000000000, 0.000000000000000000 ) ) ;
#1922 = CARTESIAN_POINT ( 'NONE',  ( 101.1416937171295558, -2.130196079827424871, -7.949999999999999289 ) ) ;
#1923 = FACE_OUTER_BOUND ( 'NONE', #35629, .T. ) ;
#1924 = CARTESIAN_POINT ( 'NONE',  ( 19.49999999999986144, 9.127013188829479873, 4.802533355213541633 ) ) ;
#1925 = ORIENTED_EDGE ( 'NONE', *, *, #126778, .F. ) ;
#1926 = EDGE_CURVE ( 'NONE', #16100, #41563, #54172, .T. ) ;
#1927 = DIRECTION ( 'NONE',  ( -0.7071067811865486830, -0.7071067811865464625, 0.000000000000000000 ) ) ;
#1928 = CARTESIAN_POINT ( 'NONE',  ( -19.21498419724177609, -3.740707523384238176, 15.76143240460119443 ) ) ;
#1929 = CARTESIAN_POINT ( 'NONE',  ( -2.510786437626908008, -27.52281430457053446, 5.000000000000000000 ) ) ;
#1930 = CARTESIAN_POINT ( 'NONE',  ( 9.625000000000001776, 6.094999999999989981, -1.119633336120465690E-15 ) ) ;
#1931 = CARTESIAN_POINT ( 'NONE',  ( 23.02040314143522082, 7.934999999999988951, -2.126176841940961904 ) ) ;
#1932 = VECTOR ( 'NONE', #59352, 1000.000000000000000 ) ;
#1933 = DIRECTION ( 'NONE',  ( -0.7071067811865486830, -0.7071067811865464625, 0.000000000000000000 ) ) ;
#1934 = CARTESIAN_POINT ( 'NONE',  ( -29.27718569542920335, -21.72500000000000142, 5.000000000000000000 ) ) ;
#1935 = ORIENTED_EDGE ( 'NONE', *, *, #50749, .T. ) ;
#1936 = VECTOR ( 'NONE', #30691, 1000.000000000000000 ) ;
#1937 = PLANE ( 'NONE',  #136965 ) ;
#1938 = ORIENTED_EDGE ( 'NONE', *, *, #80746, .T. ) ;
#1939 = CARTESIAN_POINT ( 'NONE',  ( 98.72959685856478984, -6.110000000000000320, -1.637169565754161393 ) ) ;
#1940 = DIRECTION ( 'NONE',  ( 0.7071067811865487940, -0.7071067811865463515, 0.000000000000000000 ) ) ;
#1941 = CYLINDRICAL_SURFACE ( 'NONE', #89996, 6.094999999999989093 ) ;
#1942 = DIRECTION ( 'NONE',  ( -0.6830127018922180770, -0.6830127018922204085, -0.2588190451025213501 ) ) ;
#1943 = CARTESIAN_POINT ( 'NONE',  ( 126.2665610010987649, -48.52444309369079178, -36.09967824800681768 ) ) ;
#1944 = ORIENTED_EDGE ( 'NONE', *, *, #142379, .T. ) ;
#1945 = FACE_OUTER_BOUND ( 'NONE', #78347, .T. ) ;
#1946 = CARTESIAN_POINT ( 'NONE',  ( -19.49999999999985789, -13.91253812416061386, 4.000000000000000000 ) ) ;
#1947 = DIRECTION ( 'NONE',  ( 0.7071067811865486830, -0.7071067811865464625, -0.000000000000000000 ) ) ;
#1948 = ORIENTED_EDGE ( 'NONE', *, *, #3075, .T. ) ;
#1949 = DIRECTION ( 'NONE',  ( -0.7071067811865486830, -0.7071067811865464625, 0.000000000000000000 ) ) ;
#1950 = LINE ( 'NONE', #112210, #88812 ) ;
#1952 = VERTEX_POINT ( 'NONE', #19358 ) ;
#1951 = DIRECTION ( 'NONE',  ( 0.7071067811865486830, -0.7071067811865464625, -0.000000000000000000 ) ) ;
#1953 = CARTESIAN_POINT ( 'NONE',  ( 22.49999999999985079, -5.947814304570765209, 5.000000000000000000 ) ) ;
#1954 = LINE ( 'NONE', #24469, #134998 ) ;
#1955 = LINE ( 'NONE', #13570, #50294 ) ;
#1956 = DIRECTION ( 'NONE',  ( 1.000000000000000000, 1.224606353822377258E-16, 0.000000000000000000 ) ) ;
#1957 = EDGE_LOOP ( 'NONE', ( #112942, #63873, #141474, #33566 ) ) ;
#1958 = ADVANCED_FACE ( 'NONE', ( #54864 ), #20773, .F. ) ;
#1959 = ORIENTED_EDGE ( 'NONE', *, *, #8760, .F. ) ;
#1960 = ORIENTED_EDGE ( 'NONE', *, *, #30041, .F. ) ;
#1961 = CARTESIAN_POINT ( 'NONE',  ( 86.33376352523144703, 6.110000000000001208, 1.122388791418549305E-15 ) ) ;
#1962 = ORIENTED_EDGE ( 'NONE', *, *, #10892, .T. ) ;
#1963 = FACE_OUTER_BOUND ( 'NONE', #11789, .T. ) ;
#1964 = LINE ( 'NONE', #124513, #103480 ) ;
#1965 = DIRECTION ( 'NONE',  ( -0.000000000000000000, 0.000000000000000000, 1.000000000000000000 ) ) ;
#1966 = CARTESIAN_POINT ( 'NONE',  ( 2.999999999999988010, -12.41253812416062985, 4.000000000000000000 ) ) ;
#1967 = ORIENTED_EDGE ( 'NONE', *, *, #36055, .T. ) ;
#1968 = CARTESIAN_POINT ( 'NONE',  ( -3.489213562373097322, -27.52281430457057709, 5.000000000000000000 ) ) ;
#1970 = EDGE_CURVE ( 'NONE', #119435, #81122, #129068, .T. ) ;
#1969 = CARTESIAN_POINT ( 'NONE',  ( -48.48921356237309510, -27.52281430457089328, 5.000000000000000000 ) ) ;
#1971 = CARTESIAN_POINT ( 'NONE',  ( -29.20710678118634007, -17.24070752338410273, 5.000000000000000000 ) ) ;
#1972 = CARTESIAN_POINT ( 'NONE',  ( 87.70376352523146579, 6.109999999999998543, 1.122388791418548911E-15 ) ) ;
#1973 = ADVANCED_FACE ( 'NONE', ( #75889 ), #143273, .T. ) ;
#1974 = VERTEX_POINT ( 'NONE', #32388 ) ;
#1975 = CARTESIAN_POINT ( 'NONE',  ( 24.79333936457830134, 21.75929247661549226, 4.998822639870711626 ) ) ;
#1976 = DIRECTION ( 'NONE',  ( 1.000000000000000000, 0.000000000000000000, 0.000000000000000000 ) ) ;
#1977 = AXIS2_PLACEMENT_3D ( 'NONE', #134005, #102092, #34698 ) ;
#1978 = AXIS2_PLACEMENT_3D ( 'NONE', #41884, #44027, #131034 ) ;
#1979 = VECTOR ( 'NONE', #137755, 1000.000000000000000 ) ;
#1980 = ORIENTED_EDGE ( 'NONE', *, *, #31379, .F. ) ;
#1981 = EDGE_LOOP ( 'NONE', ( #66680, #62829, #38339, #82103 ) ) ;
#1982 = VECTOR ( 'NONE', #125447, 1000.000000000000000 ) ;
#1983 = PLANE ( 'NONE',  #40026 ) ;
#1984 = EDGE_CURVE ( 'NONE', #49245, #71694, #131696, .T. ) ;
#1985 = DIRECTION ( 'NONE',  ( -1.000000000000000000, -0.000000000000000000, -0.000000000000000000 ) ) ;
#1986 = CARTESIAN_POINT ( 'NONE',  ( 25.34729149122530245, 7.934999999999992504, 0.7443565279215664798 ) ) ;
#1987 = CARTESIAN_POINT ( 'NONE',  ( 7.499999999999944045, -14.70932175296476352, -11.46312253303839057 ) ) ;
#1988 = MECHANICAL_DESIGN_GEOMETRIC_PRESENTATION_REPRESENTATION (  '', ( #117493 ), #76141 ) ;
#1989 = AXIS2_PLACEMENT_3D ( 'NONE', #93068, #48864, #122843 ) ;
#1990 = CARTESIAN_POINT ( 'NONE',  ( 122.6835989386367345, -49.14999999999999147, 40.92499999999998295 ) ) ;
#1991 = DIRECTION ( 'NONE',  ( 0.000000000000000000, -1.000000000000000000, 0.000000000000000000 ) ) ;
#1992 = CARTESIAN_POINT ( 'NONE',  ( 25.39999999999999858, -7.600000000000055600, -34.92499999999998295 ) ) ;
#1993 = SHAPE_REPRESENTATION_RELATIONSHIP ( 'NONE' , 'NONE' ,  #108808, #122638 ) ;
#1994 = EDGE_LOOP ( 'NONE', ( #80199, #136333, #15968, #43619 ) ) ;
#1995 = ORIENTED_EDGE ( 'NONE', *, *, #47752, .F. ) ;
#1996 = FACE_OUTER_BOUND ( 'NONE', #10193, .T. ) ;
#1997 = ORIENTED_EDGE ( 'NONE', *, *, #45424, .F. ) ;
#1998 = VERTEX_POINT ( 'NONE', #64296 ) ;
#1999 = CIRCLE ( 'NONE', #120081, 2.500000000000000444 ) ;
#2000 = MECHANICAL_DESIGN_GEOMETRIC_PRESENTATION_REPRESENTATION (  '', ( #32175 ), #101598 ) ;
#2001 = DIRECTION ( 'NONE',  ( 0.7071067811865486830, -0.7071067811865464625, -0.000000000000000000 ) ) ;
#2002 = EDGE_LOOP ( 'NONE', ( #24135, #30818, #116626, #50545 ) ) ;
#2003 = CARTESIAN_POINT ( 'NONE',  ( -15.18398860626900237, 28.73617430169797871, 5.000000000000000000 ) ) ;
#2004 = DIRECTION ( 'NONE',  ( 0.7071067811865487940, 0.7071067811865463515, 0.000000000000000000 ) ) ;
#2005 = DIRECTION ( 'NONE',  ( 0.000000000000000000, 0.000000000000000000, -1.000000000000000000 ) ) ;
#2006 = CARTESIAN_POINT ( 'NONE',  ( 22.85159235450332105, 2.500000000000001332, 0.000000000000000000 ) ) ;
#2007 = VECTOR ( 'NONE', #69761, 1000.000000000000227 ) ;
#2008 = AXIS2_PLACEMENT_3D ( 'NONE', #68547, #79451, #113432 ) ;
#2009 = CARTESIAN_POINT ( 'NONE',  ( 10.49999999999992184, 21.43112307739196609, 4.000000000000000000 ) ) ;
#2010 = ORIENTED_EDGE ( 'NONE', *, *, #87769, .F. ) ;
#2012 = ADVANCED_FACE ( 'NONE', ( #20050 ), #43978, .F. ) ;
#2011 = VECTOR ( 'NONE', #48325, 1000.000000000000000 ) ;
#2013 = LINE ( 'NONE', #134755, #58046 ) ;
#2014 = ORIENTED_EDGE ( 'NONE', *, *, #119442, .T. ) ;
#2015 = DIRECTION ( 'NONE',  ( -0.000000000000000000, 0.3543493200069153248, 0.9351131265310292928 ) ) ;
#2016 = ORIENTED_EDGE ( 'NONE', *, *, #129111, .T. ) ;
#2017 = CARTESIAN_POINT ( 'NONE',  ( 116.6000270504628844, 5.819803920172570422, 5.819803920172575751 ) ) ;
#2019 = ORIENTED_EDGE ( 'NONE', *, *, #9909, .T. ) ;
#2018 = ADVANCED_FACE ( 'NONE', ( #77352 ), #141119, .F. ) ;
#2020 = DIRECTION ( 'NONE',  ( -0.6830127018922181881, 0.6830127018922202975, -0.2588190451025214056 ) ) ;
#2021 = ORIENTED_EDGE ( 'NONE', *, *, #76077, .T. ) ;
#2022 = VERTEX_POINT ( 'NONE', #53411 ) ;
#2023 = VECTOR ( 'NONE', #133398, 1000.000000000000000 ) ;
#2024 = ORIENTED_EDGE ( 'NONE', *, *, #88951, .T. ) ;
#2025 = VECTOR ( 'NONE', #59194, 1000.000000000000114 ) ;
#2026 = EDGE_CURVE ( 'NONE', #86181, #127621, #31671, .T. ) ;
#2027 = EDGE_CURVE ( 'NONE', #136233, #94607, #74475, .T. ) ;
#2028 = CARTESIAN_POINT ( 'NONE',  ( 93.89583333333331439, -2.130196079827427091, 7.949999999999998401 ) ) ;
#2029 = CARTESIAN_POINT ( 'NONE',  ( -1.828169399223512848, -5.240707523384230626, 4.000000000000000000 ) ) ;
#2030 = DIRECTION ( 'NONE',  ( -1.000000000000000000, -0.000000000000000000, -0.000000000000000000 ) ) ;
#2032 = EDGE_CURVE ( 'NONE', #32915, #53582, #120054, .T. ) ;
#2031 = DIRECTION ( 'NONE',  ( 0.7071067811865487940, -0.7071067811865463515, 0.000000000000000000 ) ) ;
#2033 = CARTESIAN_POINT ( 'NONE',  ( 122.0629301918980900, 1.637169565754157174, 6.110000000000002984 ) ) ;
#2034 = PLANE ( 'NONE',  #79866 ) ;
#2035 = EDGE_CURVE ( 'NONE', #89687, #67143, #85183, .T. ) ;
#2036 = CARTESIAN_POINT ( 'NONE',  ( -21.18398860626899349, 28.73617430169802134, 5.000000000000000000 ) ) ;
#2037 = LINE ( 'NONE', #49180, #69913 ) ;
#2038 = CIRCLE ( 'NONE', #87666, 9.119999999999999218 ) ;
#2039 = EDGE_CURVE ( 'NONE', #87384, #40271, #22888, .T. ) ;
#2040 = CARTESIAN_POINT ( 'NONE',  ( -17.47599861414538580, 22.03583458319438293, 4.979811245910086726 ) ) ;
#2041 = DIRECTION ( 'NONE',  ( -1.000000000000000000, -1.224606353822377258E-16, -0.000000000000000000 ) ) ;
#2042 = ADVANCED_FACE ( 'NONE', ( #89606 ), #114214, .F. ) ;
#2043 = EDGE_LOOP ( 'NONE', ( #18243, #54537, #90165, #14547 ) ) ;
#2044 = FACE_OUTER_BOUND ( 'NONE', #129847, .T. ) ;
#2045 = LINE ( 'NONE', #124583, #121563 ) ;
#2046 = DIRECTION ( 'NONE',  ( -0.7071067811865487940, -0.7071067811865463515, -0.000000000000000000 ) ) ;
#2047 = VERTEX_POINT ( 'NONE', #59169 ) ;
#2048 = EDGE_LOOP ( 'NONE', ( #59310, #107009, #82025, #89378 ) ) ;
#2049 = DIRECTION ( 'NONE',  ( -1.000000000000000000, -0.000000000000000000, -0.000000000000000000 ) ) ;
#2050 = ORIENTED_EDGE ( 'NONE', *, *, #77073, .T. ) ;
#2051 = LINE ( 'NONE', #77546, #93119 ) ;
#2052 = FACE_OUTER_BOUND ( 'NONE', #89709, .T. ) ;
#2054 = EDGE_CURVE ( 'NONE', #51885, #72728, #124382, .T. ) ;
#2053 = DIRECTION ( 'NONE',  ( -0.7071067811865487940, 0.7071067811865463515, -0.000000000000000000 ) ) ;
#2055 = CARTESIAN_POINT ( 'NONE',  ( 60.18398860626900415, 28.73617430169829490, 5.000000000000000000 ) ) ;
#2056 = CARTESIAN_POINT ( 'NONE',  ( -19.42650926608379436, -2.782569431601979559, 4.369986656771231104 ) ) ;
#2057 = ORIENTED_EDGE ( 'NONE', *, *, #35021, .F. ) ;
#2058 = DIRECTION ( 'NONE',  ( 0.000000000000000000, 0.000000000000000000, 1.000000000000000000 ) ) ;
#2059 = ORIENTED_EDGE ( 'NONE', *, *, #52310, .F. ) ;
#2060 = EDGE_CURVE ( 'NONE', #104452, #81393, #3968, .T. ) ;
#2061 = CARTESIAN_POINT ( 'NONE',  ( 51.48921356237309510, -27.52281430457091460, 5.000000000000000000 ) ) ;
#2062 = B_SPLINE_CURVE_WITH_KNOTS ( 'NONE', 3,
 ( #100924, #13179, #111820, #90042, #23356, #101638, #45166, #79231, #89342, #135028, #47329, #123436, #2291, #46612, #58919, #35722, #91500, #12482, #113220, #122669, #79942, #135712, #56764, #113949, #124113, #69039, #24790, #36396 ),
 .UNSPECIFIED., .F., .F.,
 ( 4, 2, 2, 2, 2, 2, 2, 2, 2, 2, 2, 2, 2, 4 ),
 ( 0.002830889048686786869, 0.003748869865235868355, 0.004666850681784949842, 0.005584831498334031329, 0.006502812314883112815, 0.008338773947981275789, 0.009256754764530356408, 0.01017473558107943703, 0.01109271639762851765, 0.01201069721417759653, 0.01292867803072667542, 0.01384665884727575430, 0.01568262048037391554, 0.01751858211347207331 ),
 .UNSPECIFIED. ) ;
#2063 = CARTESIAN_POINT ( 'NONE',  ( 16.40040314143521982, -7.934999999999989839, 2.126176841940957907 ) ) ;
#2064 = ORIENTED_EDGE ( 'NONE', *, *, #98737, .F. ) ;
#2065 = CARTESIAN_POINT ( 'NONE',  ( 80.99543019189810877, 5.291415217122917625, 3.055000000000002380 ) ) ;
#2066 = FACE_OUTER_BOUND ( 'NONE', #85403, .T. ) ;
#2067 = PLANE ( 'NONE',  #76647 ) ;
#2068 = ORIENTED_EDGE ( 'NONE', *, *, #96696, .T. ) ;
#2069 = ORIENTED_EDGE ( 'NONE', *, *, #32465, .F. ) ;
#2070 = ORIENTED_EDGE ( 'NONE', *, *, #46056, .T. ) ;
#2071 = CARTESIAN_POINT ( 'NONE',  ( 6.707106781186497280, 14.25929247661557575, 5.000000000000000000 ) ) ;
#2072 = CARTESIAN_POINT ( 'NONE',  ( -33.29974487139158867, -27.71228299555229313, 4.000000000000000000 ) ) ;
#2073 = DIRECTION ( 'NONE',  ( -0.000000000000000000, 0.3543493200069153248, 0.9351131265310292928 ) ) ;
#2074 = DIRECTION ( 'NONE',  ( 0.7071067811865486830, -0.7071067811865464625, -0.000000000000000000 ) ) ;
#2075 = ORIENTED_EDGE ( 'NONE', *, *, #99314, .T. ) ;
#2076 = SURFACE_STYLE_USAGE ( .BOTH. , #123925 ) ;
#2077 = DIRECTION ( 'NONE',  ( -0.000000000000000000, 0.000000000000000000, 1.000000000000000000 ) ) ;
#2078 = EDGE_CURVE ( 'NONE', #116493, #30958, #12037, .T. ) ;
#2079 = VERTEX_POINT ( 'NONE', #112098 ) ;
#2080 = VECTOR ( 'NONE', #49503, 1000.000000000000227 ) ;
#2081 = AXIS2_PLACEMENT_3D ( 'NONE', #88011, #55400, #54686 ) ;
#2082 = CIRCLE ( 'NONE', #101676, 2.337593264352433753 ) ;
#2083 = VECTOR ( 'NONE', #122169, 1000.000000000000000 ) ;
#2084 = LINE ( 'NONE', #58715, #40119 ) ;
#2085 = ORIENTED_EDGE ( 'NONE', *, *, #60241, .T. ) ;
#2086 = ADVANCED_FACE ( 'NONE', ( #12745 ), #13448, .F. ) ;
#2087 = ORIENTED_EDGE ( 'NONE', *, *, #73669, .T. ) ;
#2088 = ORIENTED_EDGE ( 'NONE', *, *, #37606, .F. ) ;
#2089 = DIRECTION ( 'NONE',  ( -0.3543493200069162685, -0.000000000000000000, -0.9351131265310288487 ) ) ;
#2090 = CARTESIAN_POINT ( 'NONE',  ( -21.32816939922337340, -3.740707523384238176, 4.000000000000000000 ) ) ;
#2091 = ORIENTED_EDGE ( 'NONE', *, *, #9525, .F. ) ;
#2092 = SURFACE_SIDE_STYLE ('',( #68167 ) ) ;
#2093 = AXIS2_PLACEMENT_3D ( 'NONE', #101620, #135004, #2272 ) ;
#2094 = ORIENTED_EDGE ( 'NONE', *, *, #29552, .T. ) ;
#2095 = DIRECTION ( 'NONE',  ( -0.3543493200069162685, -0.000000000000000000, -0.9351131265310288487 ) ) ;
#2096 = CARTESIAN_POINT ( 'NONE',  ( 34.92499999999998295, 22.22500000000000142, 4.000000000000000000 ) ) ;
#2097 = CARTESIAN_POINT ( 'NONE',  ( 15.18398860626900237, 28.73617430169797871, 5.000000000000000000 ) ) ;
#2098 = CARTESIAN_POINT ( 'NONE',  ( 48.64169371712955581, -2.130196079827424871, -7.949999999999998401 ) ) ;
#2099 = CARTESIAN_POINT ( 'NONE',  ( 15.65494483745372811, 5.259292476615665457, 12.77922209995897518 ) ) ;
#2100 = EDGE_CURVE ( 'NONE', #105207, #47204, #122961, .T. ) ;
#2101 = CARTESIAN_POINT ( 'NONE',  ( -15.70710678118642711, -3.740707523384238176, 5.000000000000000000 ) ) ;
#2102 = LINE ( 'NONE', #46416, #125914 ) ;
#2103 = CARTESIAN_POINT ( 'NONE',  ( 16.76840764549667639, 9.139736423841732040E-16, 0.000000000000000000 ) ) ;
#2104 = CARTESIAN_POINT ( 'NONE',  ( 23.16623647476855652, 7.934999999999990727, -1.457635852685135314E-15 ) ) ;
#2106 = VECTOR ( 'NONE', #67234, 1000.000000000000000 ) ;
#2105 = FACE_OUTER_BOUND ( 'NONE', #89123, .T. ) ;
#2107 = LINE ( 'NONE', #705, #29778 ) ;
#2108 = AXIS2_PLACEMENT_3D ( 'NONE', #116991, #80996, #28582 ) ;
#2109 = CARTESIAN_POINT ( 'NONE',  ( 24.87999999999999901, 9.521314400968980422E-16, 0.000000000000000000 ) ) ;
#2110 = FACE_OUTER_BOUND ( 'NONE', #138548, .T. ) ;
#2111 = ORIENTED_EDGE ( 'NONE', *, *, #119507, .F. ) ;
#2112 =( BOUNDED_CURVE ( )  B_SPLINE_CURVE ( 3, ( #39492, #128628, #6795, #17692 ),
 .UNSPECIFIED., .F., .F. ) 
 B_SPLINE_CURVE_WITH_KNOTS ( ( 4, 4 ),
 ( 5.043186909253424055, 5.074607125596347856 ),
 .UNSPECIFIED. ) 
 CURVE ( )  GEOMETRIC_REPRESENTATION_ITEM ( )  RATIONAL_B_SPLINE_CURVE ( ( 1.000000000000000000, 0.9999177325257868620, 0.9999177325257868620, 1.000000000000000000 ) ) 
 REPRESENTATION_ITEM ( '' )  );
#2113 = ORIENTED_EDGE ( 'NONE', *, *, #128807, .F. ) ;
#2114 = CARTESIAN_POINT ( 'NONE',  ( 96.81250000000000000, 5.819803920172571310, 5.819803920172575751 ) ) ;
#2115 = ORIENTED_EDGE ( 'NONE', *, *, #36511, .F. ) ;
#2116 = ORIENTED_EDGE ( 'NONE', *, *, #54667, .F. ) ;
#2117 = ORIENTED_EDGE ( 'NONE', *, *, #27601, .F. ) ;
#2118 = DIRECTION ( 'NONE',  ( -0.3543493200069162685, -0.000000000000000000, -0.9351131265310288487 ) ) ;
#2119 = DIRECTION ( 'NONE',  ( -0.6830127018922180770, -0.6830127018922204085, -0.2588190451025213501 ) ) ;
#2120 = FACE_OUTER_BOUND ( 'NONE', #143010, .T. ) ;
#2121 = EDGE_LOOP ( 'NONE', ( #45640, #4604, #130584, #5417 ) ) ;
#2122 = AXIS2_PLACEMENT_3D ( 'NONE', #122165, #33778, #1095 ) ;
#2123 = DIRECTION ( 'NONE',  ( -0.6830127018922181881, 0.6830127018922202975, -0.2588190451025214056 ) ) ;
#2124 = VECTOR ( 'NONE', #105539, 1000.000000000000227 ) ;
#2125 = LINE ( 'NONE', #46438, #16321 ) ;
#2126 = VECTOR ( 'NONE', #74739, 1000.000000000000000 ) ;
#2127 = CARTESIAN_POINT ( 'NONE',  ( -39.48921356237310221, -27.52281430457082934, 5.000000000000000000 ) ) ;
#2128 = CARTESIAN_POINT ( 'NONE',  ( 5.999999999999963585, -9.412538124160663600, 4.000000000000000000 ) ) ;
#2129 = EDGE_CURVE ( 'NONE', #38121, #134952, #101194, .T. ) ;
#2130 = PLANE ( 'NONE',  #97323 ) ;
#2131 = VECTOR ( 'NONE', #120363, 999.9999999999998863 ) ;
#2132 = CARTESIAN_POINT ( 'NONE',  ( 24.48921356237309510, -27.52281430457072631, 5.000000000000000000 ) ) ;
#2133 = CARTESIAN_POINT ( 'NONE',  ( 13.49159235450332162, 2.500000000000001332, 0.000000000000000000 ) ) ;
#2134 = CARTESIAN_POINT ( 'NONE',  ( 34.42499999999998295, 22.22500000000000142, 5.000000000000000000 ) ) ;
#2135 = VECTOR ( 'NONE', #53514, 1000.000000000000000 ) ;
#2136 = CARTESIAN_POINT ( 'NONE',  ( 34.47516574401890921, 22.22311076525683760, 4.292435211492992231 ) ) ;
#2137 = CARTESIAN_POINT ( 'NONE',  ( -12.70710678118644843, -15.74070752338412404, 5.000000000000000000 ) ) ;
#2138 = DIRECTION ( 'NONE',  ( 0.7071067811865487940, 0.7071067811865463515, -0.000000000000000000 ) ) ;
#2139 = CIRCLE ( 'NONE', #83211, 9.000000000000001776 ) ;
#2140 = CARTESIAN_POINT ( 'NONE',  ( 26.51360224591381254, -6.350000000000003197, -3.888253587292850026E-16 ) ) ;
#2141 = DIRECTION ( 'NONE',  ( 0.000000000000000000, -1.000000000000000000, 0.000000000000000000 ) ) ;
#2142 = ORIENTED_EDGE ( 'NONE', *, *, #125053, .F. ) ;
#2143 = VERTEX_POINT ( 'NONE', #101914 ) ;
#2144 = CARTESIAN_POINT ( 'NONE',  ( 121.1879301918980900, 6.110000000000002984, -1.637169565754156730 ) ) ;
#2145 = ORIENTED_EDGE ( 'NONE', *, *, #59090, .T. ) ;
#2146 = EDGE_CURVE ( 'NONE', #142117, #54589, #2577, .T. ) ;
#2147 = DIRECTION ( 'NONE',  ( 0.6830127018922180770, -0.6830127018922204085, -0.2588190451025213501 ) ) ;
#2148 = CONICAL_SURFACE ( 'NONE', #101736, 2.055000000000000604, 0.9599310885968764806 ) ;
#2149 = CARTESIAN_POINT ( 'NONE',  ( 19.49999999999986500, -5.947814304570768762, 5.000000000000000000 ) ) ;
#2150 = ADVANCED_FACE ( 'NONE', ( #26501 ), #16299, .F. ) ;
#2151 = DIRECTION ( 'NONE',  ( 0.3543493200069162685, -0.000000000000000000, -0.9351131265310288487 ) ) ;
#2153 = EDGE_CURVE ( 'NONE', #103874, #56532, #135388, .T. ) ;
#2152 = CARTESIAN_POINT ( 'NONE',  ( 11.51078643762690490, -27.52281430457047406, 5.000000000000000000 ) ) ;
#2154 = CARTESIAN_POINT ( 'NONE',  ( 110.8912635252314658, -4.472830434245839371, -4.472830434245839371 ) ) ;
#2155 = EDGE_CURVE ( 'NONE', #8822, #119805, #59852, .T. ) ;
#2156 = ORIENTED_EDGE ( 'NONE', *, *, #4066, .F. ) ;
#2157 = VERTEX_POINT ( 'NONE', #114893 ) ;
#2158 = CARTESIAN_POINT ( 'NONE',  ( 8.649972949537106715, -4.461849672132299105, 4.461849672132299993 ) ) ;
#2159 = DIRECTION ( 'NONE',  ( -0.000000000000000000, 0.000000000000000000, 1.000000000000000000 ) ) ;
#2160 = ORIENTED_EDGE ( 'NONE', *, *, #20603, .F. ) ;
#2161 = ORIENTED_EDGE ( 'NONE', *, *, #131259, .F. ) ;
#2162 = ORIENTED_EDGE ( 'NONE', *, *, #106738, .F. ) ;
#2163 = DIRECTION ( 'NONE',  ( 0.7071067811865487940, 0.7071067811865463515, 0.000000000000000000 ) ) ;
#2164 = ADVANCED_FACE ( 'NONE', ( #83028 ), #127218, .F. ) ;
#2165 = PLANE ( 'NONE',  #97069 ) ;
#2166 = CARTESIAN_POINT ( 'NONE',  ( 21.65295664585917379, -22.22500000000000142, 26.43950276819876422 ) ) ;
#2167 = ORIENTED_EDGE ( 'NONE', *, *, #33107, .T. ) ;
#2168 = ORIENTED_EDGE ( 'NONE', *, *, #2569, .T. ) ;
#2169 = CARTESIAN_POINT ( 'NONE',  ( 24.48921356237309510, -27.52281430457072631, 5.000000000000000000 ) ) ;
#2170 = EDGE_LOOP ( 'NONE', ( #48629, #11800, #111564, #134897, #33238 ) ) ;
#2171 = VERTEX_POINT ( 'NONE', #104767 ) ;
#2172 = ORIENTED_EDGE ( 'NONE', *, *, #61266, .T. ) ;
#2173 = CARTESIAN_POINT ( 'NONE',  ( 0.000000000000000000, -18.03360074219755660, 5.000000000000000000 ) ) ;
#2174 = LINE ( 'NONE', #122554, #93845 ) ;
#2175 = CARTESIAN_POINT ( 'NONE',  ( -34.42500000000001137, -21.72500000000000142, 0.000000000000000000 ) ) ;
#2176 = ORIENTED_EDGE ( 'NONE', *, *, #117095, .T. ) ;
#2177 = CARTESIAN_POINT ( 'NONE',  ( -5.816011393731002066, 28.73617430169783304, 5.000000000000000000 ) ) ;
#2178 = EDGE_CURVE ( 'NONE', #89522, #15253, #138841, .T. ) ;
#2179 = VECTOR ( 'NONE', #55374, 1000.000000000000000 ) ;
#2180 = LINE ( 'NONE', #107924, #75697 ) ;
#2181 = LINE ( 'NONE', #67519, #140887 ) ;
#2182 = CIRCLE ( 'NONE', #43947, 2.500000000000000888 ) ;
#2183 = VECTOR ( 'NONE', #132936, 1000.000000000000000 ) ;
#2184 = DIRECTION ( 'NONE',  ( 0.6830127018922180770, -0.6830127018922204085, -0.2588190451025213501 ) ) ;
#2185 = VECTOR ( 'NONE', #103169, 1000.000000000000000 ) ;
#2186 = FACE_BOUND ( 'NONE', #38740, .T. ) ;
#2187 = VERTEX_POINT ( 'NONE', #7575 ) ;
#2188 = PLANE ( 'NONE',  #6299 ) ;
#2189 = CARTESIAN_POINT ( 'NONE',  ( -34.92500000000001137, -11.29530194282805233, 17.70209546082494256 ) ) ;
#2190 = DIRECTION ( 'NONE',  ( -0.7071067811865486830, 0.7071067811865464625, 0.000000000000000000 ) ) ;
#2191 = LINE ( 'NONE', #133477, #46278 ) ;
#2192 = VERTEX_POINT ( 'NONE', #106897 ) ;
#2193 = EDGE_LOOP ( 'NONE', ( #133761, #14164, #62737, #84970 ) ) ;
#2194 = EDGE_LOOP ( 'NONE', ( #107474, #1633, #57374, #39206 ) ) ;
#2195 = VECTOR ( 'NONE', #91323, 1000.000000000000000 ) ;
#2196 = ORIENTED_EDGE ( 'NONE', *, *, #93811, .F. ) ;
#2197 = EDGE_CURVE ( 'NONE', #142484, #128301, #81620, .T. ) ;
#2198 = CARTESIAN_POINT ( 'NONE',  ( 45.70376352523145158, 6.109999999999998543, 1.122388791418548911E-15 ) ) ;
#2199 = VERTEX_POINT ( 'NONE', #125826 ) ;
#2200 = VECTOR ( 'NONE', #10305, 1000.000000000000000 ) ;
#2201 = CARTESIAN_POINT ( 'NONE',  ( -18.70710678118640757, 11.25929247661560417, 5.000000000000000000 ) ) ;
#2202 = EDGE_CURVE ( 'NONE', #73650, #141344, #10329, .T. ) ;
#2203 = EDGE_CURVE ( 'NONE', #120482, #92375, #117057, .T. ) ;
#2204 = PLANE ( 'NONE',  #10363 ) ;
#2205 = ORIENTED_EDGE ( 'NONE', *, *, #38294, .F. ) ;
#2206 = ADVANCED_FACE ( 'NONE', ( #28659 ), #73578, .F. ) ;
#2207 =( NAMED_UNIT ( * ) SI_UNIT ( $, .STERADIAN. ) SOLID_ANGLE_UNIT ( ) );
#2208 = LINE ( 'NONE', #46528, #106041 ) ;
#2209 = AXIS2_PLACEMENT_3D ( 'NONE', #126261, #115333, #72643 ) ;
#2210 = VECTOR ( 'NONE', #32746, 999.9999999999998863 ) ;
#2211 = EDGE_CURVE ( 'NONE', #139208, #22203, #126504, .T. ) ;
#2212 = VECTOR ( 'NONE', #62111, 1000.000000000000000 ) ;
#2213 = CARTESIAN_POINT ( 'NONE',  ( -22.36246187583885359, 22.22500000000000853, 4.000000000000000000 ) ) ;
#2214 = FACE_OUTER_BOUND ( 'NONE', #130362, .T. ) ;
#2215 = CARTESIAN_POINT ( 'NONE',  ( 0.000000000000000000, 0.000000000000000000, 5.000000000000000000 ) ) ;
#2216 = CARTESIAN_POINT ( 'NONE',  ( -18.48921356237309510, -27.52281430457068367, 5.000000000000000000 ) ) ;
#2217 = ADVANCED_FACE ( 'NONE', ( #115591 ), #62714, .F. ) ;
#2218 = ORIENTED_EDGE ( 'NONE', *, *, #24523, .F. ) ;
#2219 = ORIENTED_EDGE ( 'NONE', *, *, #107714, .F. ) ;
#2220 = ORIENTED_EDGE ( 'NONE', *, *, #140856, .T. ) ;
#2221 = VERTEX_POINT ( 'NONE', #49708 ) ;
#2222 = VECTOR ( 'NONE', #11802, 999.9999999999998863 ) ;
#2223 = LINE ( 'NONE', #12414, #79795 ) ;
#2224 = ORIENTED_EDGE ( 'NONE', *, *, #34832, .T. ) ;
#2225 = VECTOR ( 'NONE', #93640, 999.9999999999998863 ) ;
#2226 = VECTOR ( 'NONE', #69394, 999.9999999999998863 ) ;
#2227 = ORIENTED_EDGE ( 'NONE', *, *, #117221, .T. ) ;
#2228 = CARTESIAN_POINT ( 'NONE',  ( 2.206660635421510808, 21.75929247661549937, 4.998822639870701856 ) ) ;
#2229 = ADVANCED_FACE ( 'NONE', ( #93885 ), #72192, .T. ) ;
#2230 = ADVANCED_FACE ( 'NONE', ( #50402 ), #83767, .F. ) ;
#2231 = VECTOR ( 'NONE', #8494, 1000.000000000000000 ) ;
#2232 = CARTESIAN_POINT ( 'NONE',  ( -8.816011393731004731, 28.73617430169781173, 5.000000000000000000 ) ) ;
#2233 = ORIENTED_EDGE ( 'NONE', *, *, #108014, .T. ) ;
#2234 = VECTOR ( 'NONE', #63374, 999.9999999999998863 ) ;
#2235 = CARTESIAN_POINT ( 'NONE',  ( 25.49999999999983658, 16.46639925780209879, 5.000000000000000000 ) ) ;
#2236 = ADVANCED_FACE ( 'NONE', ( #30046 ), #130103, .F. ) ;
#2237 = PLANE ( 'NONE',  #116146 ) ;
#2238 = CARTESIAN_POINT ( 'NONE',  ( 24.27540314143521982, -2.126176841940958351, -7.934999999999989839 ) ) ;
#2239 = DIRECTION ( 'NONE',  ( 0.000000000000000000, -1.000000000000000000, 0.000000000000000000 ) ) ;
#2240 = ORIENTED_EDGE ( 'NONE', *, *, #46303, .T. ) ;
#2242 = LINE ( 'NONE', #124066, #103157 ) ;
#2241 = CARTESIAN_POINT ( 'NONE',  ( 113.5162635252314516, -4.472830434245839371, 4.472830434245839371 ) ) ;
#2243 = LINE ( 'NONE', #45814, #111387 ) ;
#2244 = CARTESIAN_POINT ( 'NONE',  ( 0.000000000000000000, -9.500000000000000000, 0.000000000000000000 ) ) ;
#2245 = ORIENTED_EDGE ( 'NONE', *, *, #101650, .F. ) ;
#2246 = CARTESIAN_POINT ( 'NONE',  ( 25.39999999999999858, 1.194621026894847171, -17.40906030209848510 ) ) ;
#2247 = VECTOR ( 'NONE', #39055, 1000.000000000000000 ) ;
#2249 = VERTEX_POINT ( 'NONE', #130835 ) ;
#2248 = CARTESIAN_POINT ( 'NONE',  ( 75.48921356237309510, -27.52281430457107803, 5.000000000000000000 ) ) ;
#2250 = LINE ( 'NONE', #18116, #81105 ) ;
#2251 = ORIENTED_EDGE ( 'NONE', *, *, #133996, .T. ) ;
#2252 = DIRECTION ( 'NONE',  ( 0.6830127018922180770, -0.6830127018922204085, -0.2588190451025213501 ) ) ;
#2253 = CARTESIAN_POINT ( 'NONE',  ( 31.77149322861315994, 20.25929247661551003, 7.808871592221842128 ) ) ;
#2254 = CARTESIAN_POINT ( 'NONE',  ( -36.48921356237310221, -27.52281430457080802, 5.000000000000000000 ) ) ;
#2255 = VERTEX_POINT ( 'NONE', #75720 ) ;
#2256 = CARTESIAN_POINT ( 'NONE',  ( -6.640000000000001457, -40.42999999999999261, -40.00000000000000000 ) ) ;
#2257 = DIRECTION ( 'NONE',  ( -0.7071067811865486830, -0.7071067811865464625, 0.000000000000000000 ) ) ;
#2258 = EDGE_CURVE ( 'NONE', #69590, #123136, #53990, .T. ) ;
#2259 = ORIENTED_EDGE ( 'NONE', *, *, #121085, .F. ) ;
#2260 = AXIS2_PLACEMENT_3D ( 'NONE', #100342, #58316, #77187 ) ;
#2261 = CARTESIAN_POINT ( 'NONE',  ( -17.99999999999987210, -16.06887692260766087, 4.000000000000000000 ) ) ;
#2262 = VERTEX_POINT ( 'NONE', #10434 ) ;
#2263 = DIRECTION ( 'NONE',  ( -1.000000000000000000, 0.000000000000000000, 0.000000000000000000 ) ) ;
#2265 = VERTEX_POINT ( 'NONE', #131523 ) ;
#2264 = DIRECTION ( 'NONE',  ( 0.7071067811865487940, 0.7071067811865463515, 0.000000000000000000 ) ) ;
#2266 = ORIENTED_EDGE ( 'NONE', *, *, #58497, .T. ) ;
#2267 = CARTESIAN_POINT ( 'NONE',  ( 12.56294698093633500, 9.782926692783094680, -27.04452493197952734 ) ) ;
#2268 = CARTESIAN_POINT ( 'NONE',  ( -26.99999999999981526, 13.93112307739204425, 4.000000000000000000 ) ) ;
#2269 = ORIENTED_EDGE ( 'NONE', *, *, #83811, .F. ) ;
#2270 = EDGE_CURVE ( 'NONE', #47602, #60604, #19188, .T. ) ;
#2271 = LINE ( 'NONE', #115133, #96914 ) ;
#2272 = DIRECTION ( 'NONE',  ( 0.000000000000000000, -1.000000000000000000, 0.000000000000000000 ) ) ;
#2273 = ORIENTED_EDGE ( 'NONE', *, *, #3238, .F. ) ;
#2274 = CARTESIAN_POINT ( 'NONE',  ( -0.3281693992235245605, -12.74070752338415424, 4.000000000000000000 ) ) ;
#2275 = ADVANCED_FACE ( 'NONE', ( #85148 ), #118488, .T. ) ;
#2276 = LINE ( 'NONE', #100910, #93038 ) ;
#2277 = LINE ( 'NONE', #11738, #84123 ) ;
#2278 = LINE ( 'NONE', #124814, #21647 ) ;
#2279 = DIRECTION ( 'NONE',  ( -1.000000000000000000, 0.000000000000000000, 0.000000000000000000 ) ) ;
#2280 = DIRECTION ( 'NONE',  ( -0.000000000000000000, 0.000000000000000000, 1.000000000000000000 ) ) ;
#2281 = ORIENTED_EDGE ( 'NONE', *, *, #4826, .T. ) ;
#2282 = EDGE_LOOP ( 'NONE', ( #51623, #89592, #38507, #68224 ) ) ;
#2283 = ORIENTED_EDGE ( 'NONE', *, *, #74281, .T. ) ;
#2284 = CARTESIAN_POINT ( 'NONE',  ( 115.7708333333333428, -7.949999999999999289, -2.130196079827426203 ) ) ;
#2285 = VECTOR ( 'NONE', #134611, 999.9999999999998863 ) ;
#2286 = EDGE_LOOP ( 'NONE', ( #137657, #83804, #58420, #112384 ) ) ;
#2287 = EDGE_LOOP ( 'NONE', ( #43419, #11730, #83774, #11348 ) ) ;
#2288 = EDGE_CURVE ( 'NONE', #127030, #77873, #120613, .T. ) ;
#2289 = ORIENTED_EDGE ( 'NONE', *, *, #659, .T. ) ;
#2290 = VECTOR ( 'NONE', #11080, 1000.000000000000000 ) ;
#2291 = CARTESIAN_POINT ( 'NONE',  ( 1.000065336733412913, -5.551087553957981591, -4.428894815882122415 ) ) ;
#2292 = LINE ( 'NONE', #45867, #136560 ) ;
#2293 = VECTOR ( 'NONE', #82016, 1000.000000000000227 ) ;
#2294 = AXIS2_PLACEMENT_3D ( 'NONE', #108004, #40656, #97118 ) ;
#2295 = AXIS2_PLACEMENT_3D ( 'NONE', #9383, #118893, #30472 ) ;
#2296 = VERTEX_POINT ( 'NONE', #54689 ) ;
#2297 = CARTESIAN_POINT ( 'NONE',  ( 25.49999999999981881, -8.568876922607733704, 4.000000000000000000 ) ) ;
#2298 = DIRECTION ( 'NONE',  ( -0.7071067811865487940, 0.7071067811865463515, -0.000000000000000000 ) ) ;
#2299 = CIRCLE ( 'NONE', #106395, 2.500000000000000888 ) ;
#2300 = CARTESIAN_POINT ( 'NONE',  ( 31.82816939922330235, -11.24070752338417201, 4.000000000000000000 ) ) ;
#2301 = CARTESIAN_POINT ( 'NONE',  ( -48.29974487139158867, -27.71228299555239971, 4.000000000000000000 ) ) ;
#2302 = CARTESIAN_POINT ( 'NONE',  ( 121.4795968585647614, 6.109999999999999432, 1.637169565754164280 ) ) ;
#2303 = ADVANCED_FACE ( 'NONE', ( #19883 ), #8273, .F. ) ;
#2304 = ORIENTED_EDGE ( 'NONE', *, *, #24463, .F. ) ;
#2305 = CARTESIAN_POINT ( 'NONE',  ( -22.49999999999984013, 1.030536316426494681, -5.498701923753746001 ) ) ;
#2306 = DIRECTION ( 'NONE',  ( 0.7071067811865487940, 0.7071067811865463515, 0.000000000000000000 ) ) ;
#2307 = CARTESIAN_POINT ( 'NONE',  ( -60.18398860626900415, 28.73617430169829490, 5.000000000000000000 ) ) ;
#2308 = VECTOR ( 'NONE', #136055, 1000.000000000000227 ) ;
#2309 = DIRECTION ( 'NONE',  ( -1.000000000000000000, -1.224606353822377258E-16, -0.000000000000000000 ) ) ;
#2310 = PLANE ( 'NONE',  #119253 ) ;
#2311 =( BOUNDED_CURVE ( )  B_SPLINE_CURVE ( 2, ( #39603, #115666, #105528, #93242, #94650, #136027, #27256, #59233, #25841, #92508, #83089, #81688, #71504 ),
 .UNSPECIFIED., .F., .T. ) 
 B_SPLINE_CURVE_WITH_KNOTS ( ( 3, 2, 2, 2, 2, 2, 3 ),
 ( 0.4333333333333334592, 0.4361111111111112271, 0.4388888888888889950, 0.4416666666666667629, 0.4444444444444445308, 0.4472222222222223542, 0.4500000000000001221 ),
 .UNSPECIFIED. ) 
 CURVE ( )  GEOMETRIC_REPRESENTATION_ITEM ( )  RATIONAL_B_SPLINE_CURVE ( ( 0.9999999999999986677, 0.9659258262890696445, 1.000000000000000000, 0.9659258262890683122, 1.000000000000000000, 0.9659258262890683122, 1.000000000000000000, 0.9659258262890683122, 1.000000000000000000, 0.9659258262890683122, 1.000000000000000000, 0.9659258262890669799, 1.000000000000001332 ) ) 
 REPRESENTATION_ITEM ( '' )  );
#2312 = DIRECTION ( 'NONE',  ( -1.000000000000000000, -1.224606353822377258E-16, -0.000000000000000000 ) ) ;
#2313 = CARTESIAN_POINT ( 'NONE',  ( 7.499999999999947597, 8.900465351122155866, -2.516491619111531186 ) ) ;
#2314 = CARTESIAN_POINT ( 'NONE',  ( 49.51669371712955581, 7.950000000000001066, -2.130196079827421318 ) ) ;
#2315 = DIRECTION ( 'NONE',  ( -0.7071067811865486830, -0.7071067811865464625, 0.000000000000000000 ) ) ;
#2316 = LINE ( 'NONE', #99495, #108601 ) ;
#2317 = ORIENTED_EDGE ( 'NONE', *, *, #64119, .F. ) ;
#2318 = VERTEX_POINT ( 'NONE', #30800 ) ;
#2319 = CARTESIAN_POINT ( 'NONE',  ( 44.75000000000000000, -9.735942053221458872E-16, 7.950000000000000178 ) ) ;
#2320 = ORIENTED_EDGE ( 'NONE', *, *, #17735, .T. ) ;
#2321 = FACE_OUTER_BOUND ( 'NONE', #6003, .T. ) ;
#2322 = VECTOR ( 'NONE', #61577, 1000.000000000000000 ) ;
#2323 = ORIENTED_EDGE ( 'NONE', *, *, #40337, .F. ) ;
#2324 = DIRECTION ( 'NONE',  ( 0.7071067811865487940, 0.7071067811865463515, 0.000000000000000000 ) ) ;
#2326 = EDGE_CURVE ( 'NONE', #90786, #77143, #116725, .T. ) ;
#2325 = CARTESIAN_POINT ( 'NONE',  ( -34.92500000000001137, 9.662461875838888048, 4.000000000000000000 ) ) ;
#2327 = AXIS2_PLACEMENT_3D ( 'NONE', #38047, #27143, #138787 ) ;
#2328 = CARTESIAN_POINT ( 'NONE',  ( 39.37543019189809712, -5.291415217122920289, -3.055000000000001492 ) ) ;
#2329 = EDGE_CURVE ( 'NONE', #73005, #76116, #75028, .T. ) ;
#2330 = ORIENTED_EDGE ( 'NONE', *, *, #12806, .F. ) ;
#2331 = VECTOR ( 'NONE', #30888, 1000.000000000000000 ) ;
#2332 = CARTESIAN_POINT ( 'NONE',  ( 18.29974487139159223, -27.71228299555219010, 4.000000000000000000 ) ) ;
#2333 = ORIENTED_EDGE ( 'NONE', *, *, #39966, .F. ) ;
#2334 = CARTESIAN_POINT ( 'NONE',  ( 4.499999999999976019, -1.912538124160739095, 4.000000000000000000 ) ) ;
#2335 = AXIS2_PLACEMENT_3D ( 'NONE', #45709, #2123, #90624 ) ;
#2336 = CARTESIAN_POINT ( 'NONE',  ( 59.99451991528749772, 28.92564299267980132, 4.000000000000000000 ) ) ;
#2337 = LINE ( 'NONE', #43735, #60646 ) ;
#2338 = PLANE ( 'NONE',  #113590 ) ;
#2340 = ADVANCED_FACE ( 'NONE', ( #64128 ), #108293, .F. ) ;
#2339 = ORIENTED_EDGE ( 'NONE', *, *, #116323, .T. ) ;
#2341 = LINE ( 'NONE', #12526, #72047 ) ;
#2342 = EDGE_LOOP ( 'NONE', ( #132806, #114622, #99029, #81008 ) ) ;
#2343 = VECTOR ( 'NONE', #117115, 1000.000000000000227 ) ;
#2344 = LINE ( 'NONE', #89388, #121115 ) ;
#2345 = EDGE_CURVE ( 'NONE', #63317, #74837, #43800, .T. ) ;
#2346 = CARTESIAN_POINT ( 'NONE',  ( -27.29974487139158512, -27.71228299555225405, 4.000000000000000000 ) ) ;
#2347 = FACE_BOUND ( 'NONE', #104330, .T. ) ;
#2348 = FACE_OUTER_BOUND ( 'NONE', #113078, .T. ) ;
#2349 = CARTESIAN_POINT ( 'NONE',  ( 21.48921356237309155, -27.52281430457070499, 5.000000000000000000 ) ) ;
#2350 = AXIS2_PLACEMENT_3D ( 'NONE', #72169, #81599, #114193 ) ;
#2351 = CARTESIAN_POINT ( 'NONE',  ( 25.34840764549667469, 9.139736423841732040E-16, 0.000000000000000000 ) ) ;
#2352 = CARTESIAN_POINT ( 'NONE',  ( 56.78709685856478728, 3.054999999999997495, 5.291415217122919401 ) ) ;
#2353 = FACE_OUTER_BOUND ( 'NONE', #96288, .T. ) ;
#2354 = FACE_OUTER_BOUND ( 'NONE', #128403, .T. ) ;
#2356 = ORIENTED_EDGE ( 'NONE', *, *, #58952, .F. ) ;
#2355 = CARTESIAN_POINT ( 'NONE',  ( 34.45011844616453800, 7.516280811637427561, 5.000000000000001776 ) ) ;
#2357 = ORIENTED_EDGE ( 'NONE', *, *, #102896, .T. ) ;
#2358 = AXIS2_PLACEMENT_3D ( 'NONE', #52422, #95217, #41545 ) ;
#2359 = DIRECTION ( 'NONE',  ( 0.000000000000000000, 0.000000000000000000, 1.000000000000000000 ) ) ;
#2360 = ORIENTED_EDGE ( 'NONE', *, *, #25504, .T. ) ;
#2361 = EDGE_CURVE ( 'NONE', #22428, #43234, #56862, .T. ) ;
#2362 = CARTESIAN_POINT ( 'NONE',  ( 33.16642969376915318, 22.27000000000001023, -14.18759795118478806 ) ) ;
#2363 = VERTEX_POINT ( 'NONE', #102482 ) ;
#2364 = CARTESIAN_POINT ( 'NONE',  ( 34.92499999999998295, 7.701930566820908375, 4.500000000000000888 ) ) ;
#2365 = VECTOR ( 'NONE', #142092, 1000.000000000000000 ) ;
#2366 = DIRECTION ( 'NONE',  ( 0.7071067811865487940, 0.7071067811865463515, 0.000000000000000000 ) ) ;
#2367 = FACE_BOUND ( 'NONE', #6822, .T. ) ;
#2368 = CARTESIAN_POINT ( 'NONE',  ( -2.999999999999978240, -10.06887692260771416, 4.000000000000000000 ) ) ;
#2369 = DIRECTION ( 'NONE',  ( -0.6830127018922180770, -0.6830127018922204085, -0.2588190451025213501 ) ) ;
#2370 = DIRECTION ( 'NONE',  ( -0.3543493200069162685, -0.000000000000000000, -0.9351131265310288487 ) ) ;
#2372 = ORIENTED_EDGE ( 'NONE', *, *, #50186, .F. ) ;
#2371 = DIRECTION ( 'NONE',  ( -1.000000000000000000, -1.224606353822377258E-16, -0.000000000000000000 ) ) ;
#2373 = VECTOR ( 'NONE', #127306, 999.9999999999998863 ) ;
#2374 = ORIENTED_EDGE ( 'NONE', *, *, #73069, .F. ) ;
#2375 = CARTESIAN_POINT ( 'NONE',  ( -54.18398860626899705, 28.73617430169825226, 5.000000000000000000 ) ) ;
#2376 = ORIENTED_EDGE ( 'NONE', *, *, #4143, .T. ) ;
#2377 = ADVANCED_FACE ( 'NONE', ( #3131 ), #91585, .F. ) ;
#2379 = ORIENTED_EDGE ( 'NONE', *, *, #58155, .T. ) ;
#2378 = ADVANCED_FACE ( 'NONE', ( #44553 ), #77858, .F. ) ;
#2380 = CARTESIAN_POINT ( 'NONE',  ( 75.16209685856478018, -5.291415217122919401, 3.054999999999997939 ) ) ;
#2381 = ORIENTED_EDGE ( 'NONE', *, *, #99244, .F. ) ;
#2382 = DIRECTION ( 'NONE',  ( 0.7071067811865486830, -0.7071067811865464625, -0.000000000000000000 ) ) ;
#2383 = ADVANCED_FACE ( 'NONE', ( #22714 ), #26494, .F. ) ;
#2384 = EDGE_LOOP ( 'NONE', ( #79358, #5147, #58635, #32402 ) ) ;
#2385 = DIRECTION ( 'NONE',  ( 0.7071067811865487940, -0.7071067811865463515, 0.000000000000000000 ) ) ;
#2386 = VECTOR ( 'NONE', #76252, 1000.000000000000000 ) ;
#2387 = EDGE_CURVE ( 'NONE', #133793, #49119, #123531, .T. ) ;
#2388 = ADVANCED_FACE ( 'NONE', ( #35812 ), #24194, .F. ) ;
#2389 = LINE ( 'NONE', #135801, #12501 ) ;
#2390 = VECTOR ( 'NONE', #68776, 1000.000000000000227 ) ;
#2391 = AXIS2_PLACEMENT_3D ( 'NONE', #101695, #56819, #113278 ) ;
#2392 = PLANE ( 'NONE',  #80277 ) ;
#2393 = CARTESIAN_POINT ( 'NONE',  ( -34.49999999999975842, 10.46425560840038038, 4.994342998332163219 ) ) ;
#2395 =( NAMED_UNIT ( * ) SI_UNIT ( $, .STERADIAN. ) SOLID_ANGLE_UNIT ( ) );
#2394 = DIRECTION ( 'NONE',  ( 0.000000000000000000, 0.000000000000000000, 1.000000000000000000 ) ) ;
#2396 = CARTESIAN_POINT ( 'NONE',  ( 1.828169399223514624, -2.240707523384266153, 4.000000000000000000 ) ) ;
#2397 = DIRECTION ( 'NONE',  ( 0.6830127018922180770, -0.6830127018922204085, -0.2588190451025213501 ) ) ;
#2398 = VERTEX_POINT ( 'NONE', #111923 ) ;
#2399 = VECTOR ( 'NONE', #22392, 1000.000000000000227 ) ;
#2400 = AXIS2_PLACEMENT_3D ( 'NONE', #73798, #54226, #31026 ) ;
#2401 = VERTEX_POINT ( 'NONE', #112622 ) ;
#2402 = VECTOR ( 'NONE', #87077, 1000.000000000000227 ) ;
#2403 = LINE ( 'NONE', #34357, #102928 ) ;
#2404 = CARTESIAN_POINT ( 'NONE',  ( 20.28242261357419096, -21.73023691814493930, 5.000000000000000888 ) ) ;
#2405 = ORIENTED_EDGE ( 'NONE', *, *, #73426, .F. ) ;
#2406 = AXIS2_PLACEMENT_3D ( 'NONE', #126695, #45099, #5621 ) ;
#2407 = ORIENTED_EDGE ( 'NONE', *, *, #53785, .T. ) ;
#2408 = ORIENTED_EDGE ( 'NONE', *, *, #48236, .T. ) ;
#2410 = EDGE_CURVE ( 'NONE', #8692, #92047, #6079, .T. ) ;
#2409 = LINE ( 'NONE', #137251, #24402 ) ;
#2411 = ADVANCED_FACE ( 'NONE', ( #69137 ), #41291, .F. ) ;
#2412 = CARTESIAN_POINT ( 'NONE',  ( 29.45876352523143993, 0.000000000000000000, -6.110000000000001208 ) ) ;
#2413 = EDGE_LOOP ( 'NONE', ( #115330, #84092, #137165, #81660, #115388 ) ) ;
#2414 = AXIS2_PLACEMENT_3D ( 'NONE', #81917, #4980, #106434 ) ;
#2415 = CARTESIAN_POINT ( 'NONE',  ( -16.49999999999988631, -12.66682484999667757, -0.6294897503864330668 ) ) ;
#2416 = EDGE_CURVE ( 'NONE', #77035, #1792, #73239, .T. ) ;
#2417 = CARTESIAN_POINT ( 'NONE',  ( 3.858736474768553304, 5.808823158059031044, -5.808823158059038150 ) ) ;
#2418 = CARTESIAN_POINT ( 'NONE',  ( -7.940000000000001279, -35.14999999999999147, -11.89864999999999640 ) ) ;
#2419 = ORIENTED_EDGE ( 'NONE', *, *, #68952, .T. ) ;
#2420 = DIRECTION ( 'NONE',  ( -0.7071067811865486830, -0.7071067811865464625, 0.000000000000000000 ) ) ;
#2421 = CARTESIAN_POINT ( 'NONE',  ( 119.6625270504628986, 7.949999999999998401, 1.460391307983218338E-15 ) ) ;
#2422 = VECTOR ( 'NONE', #64920, 1000.000000000000000 ) ;
#2423 = CARTESIAN_POINT ( 'NONE',  ( -77.99451991528749772, 28.92564299267992567, 4.000000000000000000 ) ) ;
#2424 = EDGE_CURVE ( 'NONE', #31384, #17080, #17401, .T. ) ;
#2426 = EDGE_LOOP ( 'NONE', ( #135710, #51906, #114340, #8829, #67737 ) ) ;
#2425 = LINE ( 'NONE', #91610, #7713 ) ;
#2427 = VERTEX_POINT ( 'NONE', #84810 ) ;
#2428 = DIRECTION ( 'NONE',  ( -0.7071067811865486830, -0.7071067811865464625, 0.000000000000000000 ) ) ;
#2429 = CARTESIAN_POINT ( 'NONE',  ( 17.99999999999986855, -22.22500000000000142, 4.412002311790053533 ) ) ;
#2430 = DIRECTION ( 'NONE',  ( -0.6830127018922181881, 0.6830127018922202975, -0.2588190451025214056 ) ) ;
#2431 = ORIENTED_EDGE ( 'NONE', *, *, #21887, .T. ) ;
#2432 = VECTOR ( 'NONE', #42719, 1000.000000000000227 ) ;
#2433 = PLANE ( 'NONE',  #73651 ) ;
#2434 = LINE ( 'NONE', #80068, #52573 ) ;
#2435 = VECTOR ( 'NONE', #64655, 1000.000000000000227 ) ;
#2437 = LINE ( 'NONE', #47455, #42573 ) ;
#2436 = AXIS2_PLACEMENT_3D ( 'NONE', #34265, #48017, #79241 ) ;
#2438 = CARTESIAN_POINT ( 'NONE',  ( 39.48921356237310221, -27.52281430457082934, 5.000000000000000000 ) ) ;
#2439 = DIRECTION ( 'NONE',  ( -0.3543493200069162685, -0.000000000000000000, -0.9351131265310288487 ) ) ;
#2440 = ADVANCED_FACE ( 'NONE', ( #5787 ), #100695, .F. ) ;
#2441 = CARTESIAN_POINT ( 'NONE',  ( -34.92500000000001137, 22.22500000000000142, 4.000000000000000000 ) ) ;
#2442 = VECTOR ( 'NONE', #53297, 1000.000000000000000 ) ;
#2443 = LINE ( 'NONE', #24925, #33137 ) ;
#2444 = CARTESIAN_POINT ( 'NONE',  ( 21.19163961620376924, 6.094999999999988205, -1.633150327867694651 ) ) ;
#2445 = DIRECTION ( 'NONE',  ( 0.7071067811865486830, -0.7071067811865464625, -0.000000000000000000 ) ) ;
#2446 = CARTESIAN_POINT ( 'NONE',  ( -2.999999999999981792, 1.761378380278681099, -6.096875308897261370 ) ) ;
#2447 = ORIENTED_EDGE ( 'NONE', *, *, #78535, .T. ) ;
#2448 = AXIS2_PLACEMENT_3D ( 'NONE', #64910, #54750, #119948 ) ;
#2449 = EDGE_CURVE ( 'NONE', #21837, #31597, #130626, .T. ) ;
#2450 = ORIENTED_EDGE ( 'NONE', *, *, #137199, .T. ) ;
#2451 = EDGE_CURVE ( 'NONE', #142117, #1085, #9341, .T. ) ;
#2452 = CARTESIAN_POINT ( 'NONE',  ( 72.48921356237309510, -27.52281430457106026, 5.000000000000000000 ) ) ;
#2453 = CARTESIAN_POINT ( 'NONE',  ( -20.99451991528748707, 28.92564299267952777, 4.000000000000000000 ) ) ;
#2454 = ADVANCED_FACE ( 'NONE', ( #123170 ), #106896, .T. ) ;
#2455 = CARTESIAN_POINT ( 'NONE',  ( 0.2704031414352194296, -7.934999999999989839, 2.126176841940957907 ) ) ;
#2456 = DIRECTION ( 'NONE',  ( 0.3543493200069162685, -0.000000000000000000, -0.9351131265310288487 ) ) ;
#2457 = CARTESIAN_POINT ( 'NONE',  ( -9.183988606268997046, 28.73617430169793607, 5.000000000000000000 ) ) ;
#2458 = DIRECTION ( 'NONE',  ( 0.7071067811865487940, 0.7071067811865463515, -0.000000000000000000 ) ) ;
#2459 = VERTEX_POINT ( 'NONE', #26691 ) ;
#2460 = CARTESIAN_POINT ( 'NONE',  ( -14.70025512860841133, -27.71228299555195917, 4.000000000000000000 ) ) ;
#2461 = UNCERTAINTY_MEASURE_WITH_UNIT (LENGTH_MEASURE( 1.000000000000000082E-05 ), #59794, 'distance_accuracy_value', 'NONE');
#2462 = AXIS2_PLACEMENT_3D ( 'NONE', #6569, #71916, #105215 ) ;
#2463 = DIRECTION ( 'NONE',  ( 0.7071067811865487940, 0.7071067811865463515, 0.000000000000000000 ) ) ;
#2464 = CARTESIAN_POINT ( 'NONE',  ( 18.18398860626898994, 28.73617430169800002, 5.000000000000000000 ) ) ;
#2465 = CARTESIAN_POINT ( 'NONE',  ( 58.09959685856477307, -6.109999999999998543, -1.637169565754160727 ) ) ;
#2466 = CARTESIAN_POINT ( 'NONE',  ( 156.1500000000000057, -49.14999999999999147, 45.92499999999998295 ) ) ;
#2467 = DIRECTION ( 'NONE',  ( -0.7071067811865486830, 0.7071067811865463515, 0.000000000000000000 ) ) ;
#2468 = LINE ( 'NONE', #116785, #78926 ) ;
#2469 = ORIENTED_EDGE ( 'NONE', *, *, #5476, .T. ) ;
#2470 = DIRECTION ( 'NONE',  ( -0.000000000000000000, -1.000000000000000000, -0.000000000000000000 ) ) ;
#2471 = ORIENTED_EDGE ( 'NONE', *, *, #87263, .F. ) ;
#2472 = DIRECTION ( 'NONE',  ( -0.7071067811865486830, -0.7071067811865464625, -0.000000000000000000 ) ) ;
#2473 = CARTESIAN_POINT ( 'NONE',  ( 26.40000000000000568, -17.48000000000005016, 12.69999999999954454 ) ) ;
#2474 = DIRECTION ( 'NONE',  ( -0.000000000000000000, -0.3543493200069152693, 0.9351131265310292928 ) ) ;
#2475 = PLANE ( 'NONE',  #37052 ) ;
#2476 = CARTESIAN_POINT ( 'NONE',  ( 17.24139925780192328, 21.72500000000000142, 5.000000000000000000 ) ) ;
#2477 = DIRECTION ( 'NONE',  ( -0.7071067811865487940, 0.7071067811865463515, 0.000000000000000000 ) ) ;
#2478 = VERTEX_POINT ( 'NONE', #34723 ) ;
#2479 = ORIENTED_EDGE ( 'NONE', *, *, #17002, .F. ) ;
#2480 = CARTESIAN_POINT ( 'NONE',  ( -8.999999999999944933, -13.39766691384885000, -10.96608748226463703 ) ) ;
#2481 = CARTESIAN_POINT ( 'NONE',  ( 26.90113084065429305, -4.940037651924031437, -4.143603795564325232 ) ) ;
#2482 = UNCERTAINTY_MEASURE_WITH_UNIT (LENGTH_MEASURE( 1.000000000000000082E-05 ), #112838, 'distance_accuracy_value', 'NONE');
#2483 = AXIS2_PLACEMENT_3D ( 'NONE', #94497, #59080, #82936 ) ;
#2484 = DIRECTION ( 'NONE',  ( -1.000000000000000000, -0.000000000000000000, 0.000000000000000000 ) ) ;
#2485 = CARTESIAN_POINT ( 'NONE',  ( -3.183988606268992161, 28.73617430169789699, 5.000000000000000000 ) ) ;
#2486 = CARTESIAN_POINT ( 'NONE',  ( 75.03752705046288440, -9.735942053221456900E-16, 7.949999999999998401 ) ) ;
#2487 = DIRECTION ( 'NONE',  ( -0.000000000000000000, 0.3543493200069153248, 0.9351131265310292928 ) ) ;
#2488 = CARTESIAN_POINT ( 'NONE',  ( -48.29974487139158867, -27.71228299555239971, 4.000000000000000000 ) ) ;
#2489 = ORIENTED_EDGE ( 'NONE', *, *, #103276, .T. ) ;
#2490 = CARTESIAN_POINT ( 'NONE',  ( 72.31250000000001421, 5.819803920172571310, 5.819803920172575751 ) ) ;
#2491 = DIRECTION ( 'NONE',  ( -0.7071067811865487940, 0.7071067811865463515, -0.000000000000000000 ) ) ;
#2492 = DIRECTION ( 'NONE',  ( 0.7071067811865486830, -0.7071067811865464625, -0.000000000000000000 ) ) ;
#2493 = ADVANCED_FACE ( 'NONE', ( #112288 ), #12937, .F. ) ;
#2494 = CARTESIAN_POINT ( 'NONE',  ( 25.49999999999982236, -6.839392718269110105, -8.480912228396146446 ) ) ;
#2495 = ORIENTED_EDGE ( 'NONE', *, *, #54161, .T. ) ;
#2496 = AXIS2_PLACEMENT_3D ( 'NONE', #131929, #20996, #21729 ) ;
#2497 = FACE_OUTER_BOUND ( 'NONE', #13532, .T. ) ;
#2498 = AXIS2_PLACEMENT_3D ( 'NONE', #85312, #108468, #119361 ) ;
#2499 = CONICAL_SURFACE ( 'NONE', #21043, 2.500000000000000444, 0.9599310885968830309 ) ;
#2500 = DIRECTION ( 'NONE',  ( -1.000000000000000000, -0.000000000000000000, -0.000000000000000000 ) ) ;
#2501 = CARTESIAN_POINT ( 'NONE',  ( 70.29209685856477563, -5.291415217122921177, 3.054999999999999272 ) ) ;
#2502 = CARTESIAN_POINT ( 'NONE',  ( 22.49999999999984013, -13.91253812416061031, 4.000000000000000000 ) ) ;
#2503 = ORIENTED_EDGE ( 'NONE', *, *, #8740, .T. ) ;
#2505 = ORIENTED_EDGE ( 'NONE', *, *, #68906, .F. ) ;
#2504 = AXIS2_PLACEMENT_3D ( 'NONE', #42971, #19052, #8827 ) ;
#2506 = VECTOR ( 'NONE', #105374, 1000.000000000000000 ) ;
#2507 = AXIS2_PLACEMENT_3D ( 'NONE', #72961, #96077, #117116 ) ;
#2509 = CARTESIAN_POINT ( 'NONE',  ( -23.99999999999982592, -0.4125381241607464222, 4.000000000000000000 ) ) ;
#2508 = VECTOR ( 'NONE', #461, 1000.000000000000000 ) ;
#2510 = DIRECTION ( 'NONE',  ( -0.6830127018922181881, 0.6830127018922202975, -0.2588190451025214056 ) ) ;
#2511 = CARTESIAN_POINT ( 'NONE',  ( -13.08638746355377158, 2.894607053745204883, 4.324337194087686242 ) ) ;
#2512 = EDGE_CURVE ( 'NONE', #77572, #132198, #50582, .T. ) ;
#2513 = DIRECTION ( 'NONE',  ( -0.6830127018922181881, 0.6830127018922202975, -0.2588190451025214056 ) ) ;
#2515 = EDGE_LOOP ( 'NONE', ( #29956, #713, #35393, #126362 ) ) ;
#2514 = CARTESIAN_POINT ( 'NONE',  ( 85.43750000000001421, 5.819803920172574863, -5.819803920172573086 ) ) ;
#2516 = EDGE_CURVE ( 'NONE', #110269, #57315, #124577, .T. ) ;
#2517 = LINE ( 'NONE', #48199, #108607 ) ;
#2518 = DIRECTION ( 'NONE',  ( 0.5735764363510453823, -0.8191520442889923537, 1.003171929053525486E-16 ) ) ;
#2519 = DIRECTION ( 'NONE',  ( 0.6830127018922180770, -0.6830127018922204085, -0.2588190451025213501 ) ) ;
#2520 = CIRCLE ( 'NONE', #229, 9.500000000000001776 ) ;
#2521 = DIRECTION ( 'NONE',  ( 0.3543493200069162685, -0.000000000000000000, -0.9351131265310288487 ) ) ;
#2522 = ORIENTED_EDGE ( 'NONE', *, *, #75026, .T. ) ;
#2523 = ORIENTED_EDGE ( 'NONE', *, *, #142075, .F. ) ;
#2524 = CARTESIAN_POINT ( 'NONE',  ( 53.22959685856475431, -6.110000000000000320, -1.637169565754161393 ) ) ;
#2525 = ORIENTED_EDGE ( 'NONE', *, *, #62158, .T. ) ;
#2526 = EDGE_CURVE ( 'NONE', #91761, #87588, #2037, .T. ) ;
#2527 = VECTOR ( 'NONE', #35963, 999.9999999999998863 ) ;
#2528 = CARTESIAN_POINT ( 'NONE',  ( 27.70710678118635784, -15.74070752338411694, 5.000000000000000000 ) ) ;
#2529 = CARTESIAN_POINT ( 'NONE',  ( -26.99451991528749417, 28.92564299267956685, 4.000000000000000000 ) ) ;
#2530 = CARTESIAN_POINT ( 'NONE',  ( 44.99451991528749772, 28.92564299267969474, 4.000000000000000000 ) ) ;
#2531 = AXIS2_PLACEMENT_3D ( 'NONE', #1046, #89511, #78644 ) ;
#2532 = CARTESIAN_POINT ( 'NONE',  ( 19.83957586139685247, 9.091547215995101183, 4.000000000000000000 ) ) ;
#2533 = DIRECTION ( 'NONE',  ( -0.000000000000000000, 0.3543493200069153248, 0.9351131265310292928 ) ) ;
#2534 = ORIENTED_EDGE ( 'NONE', *, *, #72740, .F. ) ;
#2535 = ORIENTED_EDGE ( 'NONE', *, *, #137252, .T. ) ;
#2536 = DIRECTION ( 'NONE',  ( 0.7071067811865487940, -0.7071067811865463515, 0.000000000000000000 ) ) ;
#2537 = CARTESIAN_POINT ( 'NONE',  ( -17.15351703751440482, -1.296283446796709926, -31.89465879581624819 ) ) ;
#2538 = EDGE_CURVE ( 'NONE', #133870, #105072, #90532, .T. ) ;
#2539 = PRESENTATION_LAYER_ASSIGNMENT (  '', '', ( #113699 ) ) ;
#2540 = ORIENTED_EDGE ( 'NONE', *, *, #52332, .T. ) ;
#2541 = VECTOR ( 'NONE', #87249, 1000.000000000000000 ) ;
#2542 = LINE ( 'NONE', #14864, #102349 ) ;
#2543 = CIRCLE ( 'NONE', #78972, 2.500000000000000444 ) ;
#2544 = CARTESIAN_POINT ( 'NONE',  ( 113.1000270504628986, 5.819803920172570422, 5.819803920172575751 ) ) ;
#2545 = DIRECTION ( 'NONE',  ( 1.000000000000000000, 0.000000000000000000, 0.000000000000000000 ) ) ;
#2546 = EDGE_CURVE ( 'NONE', #109916, #119711, #4149, .T. ) ;
#2547 = CIRCLE ( 'NONE', #139195, 25.00000000000002842 ) ;
#2548 = EDGE_LOOP ( 'NONE', ( #1662, #92443, #50337, #60677 ) ) ;
#2549 = FACE_BOUND ( 'NONE', #124058, .T. ) ;
#2550 = AXIS2_PLACEMENT_3D ( 'NONE', #133394, #68175, #134839 ) ;
#2551 = CARTESIAN_POINT ( 'NONE',  ( -5.816011393731002066, 28.73617430169783304, 5.000000000000000000 ) ) ;
#2552 = PLANE ( 'NONE',  #55951 ) ;
#2553 = CARTESIAN_POINT ( 'NONE',  ( 37.99586038379622011, -3.974999999999998312, -6.884901960086286188 ) ) ;
#2554 = CARTESIAN_POINT ( 'NONE',  ( 5.691592354503320905, 9.902892378096218942E-16, 0.000000000000000000 ) ) ;
#2555 = PLANE ( 'NONE',  #35011 ) ;
#2556 = DIRECTION ( 'NONE',  ( 1.000000000000000000, 2.039446610170337267E-32, -1.224646799147353207E-16 ) ) ;
#2557 = ORIENTED_EDGE ( 'NONE', *, *, #30106, .F. ) ;
#2558 =( GEOMETRIC_REPRESENTATION_CONTEXT ( 3 ) GLOBAL_UNCERTAINTY_ASSIGNED_CONTEXT ( ( #139093 ) ) GLOBAL_UNIT_ASSIGNED_CONTEXT ( ( #79225, #54587, #141 ) ) REPRESENTATION_CONTEXT ( 'NONE', 'WORKASPACE' ) );
#2559 = VERTEX_POINT ( 'NONE', #70932 ) ;
#2560 = CARTESIAN_POINT ( 'NONE',  ( 103.5995968585647802, -6.109999999999997655, -1.637169565754160283 ) ) ;
#2561 = ORIENTED_EDGE ( 'NONE', *, *, #49898, .T. ) ;
#2562 = PLANE ( 'NONE',  #120600 ) ;
#2563 = EDGE_LOOP ( 'NONE', ( #129844, #42649, #110459, #102078 ) ) ;
#2564 = ADVANCED_FACE ( 'NONE', ( #115083 ), #37583, .F. ) ;
#2565 = VECTOR ( 'NONE', #11236, 1000.000000000000000 ) ;
#2566 = LINE ( 'NONE', #35254, #47052 ) ;
#2567 = VECTOR ( 'NONE', #109992, 1000.000000000000227 ) ;
#2568 = LINE ( 'NONE', #101185, #98768 ) ;
#2569 = EDGE_CURVE ( 'NONE', #119600, #105140, #15754, .T. ) ;
#2570 = EDGE_CURVE ( 'NONE', #58171, #58911, #81089, .T. ) ;
#2571 = DIRECTION ( 'NONE',  ( -0.7071067811865486830, 0.7071067811865464625, 0.000000000000000000 ) ) ;
#2572 = ORIENTED_EDGE ( 'NONE', *, *, #62327, .T. ) ;
#2573 = DIRECTION ( 'NONE',  ( -0.000000000000000000, 0.3543493200069153248, 0.9351131265310292928 ) ) ;
#2574 = CARTESIAN_POINT ( 'NONE',  ( -6.489213562373093325, -27.52281430457059841, 5.000000000000000000 ) ) ;
#2575 = CARTESIAN_POINT ( 'NONE',  ( 27.18398860626900060, 28.73617430169806042, 5.000000000000000000 ) ) ;
#2577 = LINE ( 'NONE', #15571, #54362 ) ;
#2576 = DIRECTION ( 'NONE',  ( 0.7071067811865487940, 0.7071067811865463515, 0.000000000000000000 ) ) ;
#2578 = CARTESIAN_POINT ( 'NONE',  ( 17.11087965568911073, 8.820243421702873121, 4.000000000000000000 ) ) ;
#2579 = VECTOR ( 'NONE', #72608, 999.9999999999998863 ) ;
#2580 = CARTESIAN_POINT ( 'NONE',  ( 19.98012225071440895, -17.24070752338409562, 20.23474786156473826 ) ) ;
#2581 = VERTEX_POINT ( 'NONE', #136876 ) ;
#2582 = ADVANCED_FACE ( 'NONE', ( #48442 ), #132418, .T. ) ;
#2583 = CARTESIAN_POINT ( 'NONE',  ( 15.29974487139158867, -27.71228299555216879, 4.000000000000000000 ) ) ;
#2584 =( BOUNDED_CURVE ( )  B_SPLINE_CURVE ( 3, ( #9499, #75515, #30595, #76227 ),
 .UNSPECIFIED., .F., .T. ) 
 B_SPLINE_CURVE_WITH_KNOTS ( ( 4, 4 ),
 ( 4.350170835173025274, 4.500739107949216056 ),
 .UNSPECIFIED. ) 
 CURVE ( )  GEOMETRIC_REPRESENTATION_ITEM ( )  RATIONAL_B_SPLINE_CURVE ( ( 1.000000000000000000, 0.9981116584018956406, 0.9981116584018956406, 1.000000000000000000 ) ) 
 REPRESENTATION_ITEM ( '' )  );
#2585 = FACE_OUTER_BOUND ( 'NONE', #26863, .T. ) ;
#2586 = ORIENTED_EDGE ( 'NONE', *, *, #79397, .F. ) ;
#2587 = VERTEX_POINT ( 'NONE', #92637 ) ;
#2588 = ADVANCED_FACE ( 'NONE', ( #60051 ), #4884, .F. ) ;
#2590 = ORIENTED_EDGE ( 'NONE', *, *, #71794, .T. ) ;
#2589 = EDGE_CURVE ( 'NONE', #29676, #23874, #102839, .T. ) ;
#2591 = CARTESIAN_POINT ( 'NONE',  ( 57.75043019189809712, 3.055000000000002824, -5.291415217122919401 ) ) ;
#2592 = VECTOR ( 'NONE', #112371, 1000.000000000000114 ) ;
#2593 = ORIENTED_EDGE ( 'NONE', *, *, #55401, .T. ) ;
#2594 = CARTESIAN_POINT ( 'NONE',  ( 8.212472949537106715, 0.000000000000000000, 6.094999999999989981 ) ) ;
#2595 = CARTESIAN_POINT ( 'NONE',  ( 89.68793019189810423, 6.110000000000002984, -1.637169565754156730 ) ) ;
#2596 = LINE ( 'NONE', #44752, #65693 ) ;
#2597 = ADVANCED_FACE ( 'NONE', ( #39733 ), #73761, .F. ) ;
#2598 = ORIENTED_EDGE ( 'NONE', *, *, #29243, .F. ) ;
#2599 = CARTESIAN_POINT ( 'NONE',  ( 2.000000000000000000, 2.375000000000000000, 1.069999999999998508 ) ) ;
#2600 = ORIENTED_EDGE ( 'NONE', *, *, #59293, .F. ) ;
#2601 = LINE ( 'NONE', #35994, #58058 ) ;
#2603 = ADVANCED_FACE ( 'NONE', ( #8454 ), #71635, .F. ) ;
#2602 = VECTOR ( 'NONE', #38318, 1000.000000000000227 ) ;
#2604 = FACE_OUTER_BOUND ( 'NONE', #55083, .T. ) ;
#2605 = ORIENTED_EDGE ( 'NONE', *, *, #23899, .T. ) ;
#2606 = SURFACE_STYLE_FILL_AREA ( #78778 ) ;
#2607 = DIRECTION ( 'NONE',  ( 0.6830127018922181881, 0.6830127018922202975, -0.2588190451025214056 ) ) ;
#2609 = CARTESIAN_POINT ( 'NONE',  ( 126.0579301918981230, 6.110000000000001208, -1.637169565754156286 ) ) ;
#2608 = AXIS2_PLACEMENT_3D ( 'NONE', #21342, #132276, #123538 ) ;
#2611 = ORIENTED_EDGE ( 'NONE', *, *, #44892, .T. ) ;
#2610 = AXIS2_PLACEMENT_3D ( 'NONE', #62691, #37360, #72166 ) ;
#2612 = CARTESIAN_POINT ( 'NONE',  ( -14.99451991528749595, 28.92564299267948513, 4.000000000000000000 ) ) ;
#2613 = VERTEX_POINT ( 'NONE', #63634 ) ;
#2614 = ORIENTED_EDGE ( 'NONE', *, *, #58952, .T. ) ;
#2615 = ORIENTED_EDGE ( 'NONE', *, *, #20892, .F. ) ;
#2616 = LINE ( 'NONE', #58509, #63282 ) ;
#2617 = AXIS2_PLACEMENT_3D ( 'NONE', #3517, #16545, #83257 ) ;
#2618 = VECTOR ( 'NONE', #104119, 1000.000000000000000 ) ;
#2619 = VECTOR ( 'NONE', #15874, 1000.000000000000000 ) ;
#2620 = CIRCLE ( 'NONE', #223, 5.968999999999998529 ) ;
#2621 =( LENGTH_UNIT ( ) NAMED_UNIT ( * ) SI_UNIT ( .MILLI., .METRE. ) );
#2622 = CARTESIAN_POINT ( 'NONE',  ( 7.499999999999951150, -2.947814304570795851, 5.000000000000000000 ) ) ;
#2623 = LINE ( 'NONE', #62757, #83360 ) ;
#2624 = LINE ( 'NONE', #25821, #185 ) ;
#2626 = ORIENTED_EDGE ( 'NONE', *, *, #1398, .T. ) ;
#2625 = CIRCLE ( 'NONE', #116051, 2.500000000000000888 ) ;
#2627 =( NAMED_UNIT ( * ) PLANE_ANGLE_UNIT ( ) SI_UNIT ( $, .RADIAN. ) );
#2628 = EDGE_CURVE ( 'NONE', #100474, #12218, #16500, .T. ) ;
#2629 = ADVANCED_FACE ( 'NONE', ( #49896 ), #94071, .T. ) ;
#2630 = CARTESIAN_POINT ( 'NONE',  ( 19.66623647476855297, 7.934999999999990727, -1.457635852685135314E-15 ) ) ;
#2631 = LINE ( 'NONE', #80942, #120257 ) ;
#2632 = CARTESIAN_POINT ( 'NONE',  ( -23.54739889332687497, 7.099584588756134629, 5.000000000000000000 ) ) ;
#2633 = VECTOR ( 'NONE', #118826, 1000.000000000000000 ) ;
#2634 = CARTESIAN_POINT ( 'NONE',  ( -28.49999999999980105, 6.277155672890246230, -3.510561720658876173 ) ) ;
#2635 = VERTEX_POINT ( 'NONE', #117937 ) ;
#2636 = ORIENTED_EDGE ( 'NONE', *, *, #130554, .T. ) ;
#2637 = ORIENTED_EDGE ( 'NONE', *, *, #76318, .T. ) ;
#2638 = CARTESIAN_POINT ( 'NONE',  ( 34.49999999999975842, -20.53675388469227769, 2.352720554255973706 ) ) ;
#2639 = CARTESIAN_POINT ( 'NONE',  ( -32.99999999999976552, -15.03360074219758502, 5.000000000000000000 ) ) ;
#2640 = CARTESIAN_POINT ( 'NONE',  ( -9.119999999999999218, 0.000000000000000000, 10.00000000000000000 ) ) ;
#2641 = CARTESIAN_POINT ( 'NONE',  ( 42.29974487139158157, -27.71228299555235708, 4.000000000000000000 ) ) ;
#2642 = CARTESIAN_POINT ( 'NONE',  ( 6.853232476907147763, 9.118190832583858096, -2.677290879925327882 ) ) ;
#2643 = VECTOR ( 'NONE', #79119, 1000.000000000000000 ) ;
#2644 = VECTOR ( 'NONE', #53378, 1000.000000000000000 ) ;
#2645 = DIRECTION ( 'NONE',  ( -0.000000000000000000, 0.3543493200069153248, 0.9351131265310292928 ) ) ;
#2646 = CARTESIAN_POINT ( 'NONE',  ( 14.39532882439692862, 4.202752102959690472E-16, 0.000000000000000000 ) ) ;
#2647 = LINE ( 'NONE', #103384, #90379 ) ;
#2648 = LINE ( 'NONE', #84369, #69805 ) ;
#2649 = CARTESIAN_POINT ( 'NONE',  ( -45.29974487139158867, -27.71228299555237840, 4.000000000000000000 ) ) ;
#2650 = ORIENTED_EDGE ( 'NONE', *, *, #46020, .F. ) ;
#2652 = AXIS2_PLACEMENT_3D ( 'NONE', #81164, #113040, #71008 ) ;
#2651 =( NAMED_UNIT ( * ) PLANE_ANGLE_UNIT ( ) SI_UNIT ( $, .RADIAN. ) );
#2653 = VERTEX_POINT ( 'NONE', #72384 ) ;
#2654 = CARTESIAN_POINT ( 'NONE',  ( -25.39999999999996305, 0.000000000000000000, 2.500000000000000000 ) ) ;
#2656 = ORIENTED_EDGE ( 'NONE', *, *, #78074, .F. ) ;
#2655 = CARTESIAN_POINT ( 'NONE',  ( -8.999999999999932498, 20.96639925780204905, 5.000000000000000000 ) ) ;
#2657 = VECTOR ( 'NONE', #90231, 1000.000000000000000 ) ;
#2658 = DIRECTION ( 'NONE',  ( 0.7071067811865487940, 0.7071067811865463515, 0.000000000000000000 ) ) ;
#2659 = FACE_OUTER_BOUND ( 'NONE', #107936, .T. ) ;
#2660 = ORIENTED_EDGE ( 'NONE', *, *, #41190, .F. ) ;
#2661 = DIRECTION ( 'NONE',  ( -0.6830127018922181881, 0.6830127018922202975, -0.2588190451025214056 ) ) ;
#2662 = ORIENTED_EDGE ( 'NONE', *, *, #20725, .F. ) ;
#2663 = DIRECTION ( 'NONE',  ( -0.7071067811865486830, -0.7071067811865464625, 0.000000000000000000 ) ) ;
#2664 = UNCERTAINTY_MEASURE_WITH_UNIT (LENGTH_MEASURE( 1.000000000000000082E-05 ), #86950, 'distance_accuracy_value', 'NONE');
#2665 = ORIENTED_EDGE ( 'NONE', *, *, #125044, .F. ) ;
#2666 = LINE ( 'NONE', #132531, #89269 ) ;
#2667 = CARTESIAN_POINT ( 'NONE',  ( 101.5791937171295558, 3.975000000000002753, -6.884901960086283523 ) ) ;
#2668 = DIRECTION ( 'NONE',  ( -0.000000000000000000, -0.3543493200069152693, 0.9351131265310292928 ) ) ;
#2669 = CARTESIAN_POINT ( 'NONE',  ( 19.40370036533107978, 9.134293891043357760, 4.529189151624862575 ) ) ;
#2670 = ORIENTED_EDGE ( 'NONE', *, *, #114502, .T. ) ;
#2671 = PLANE ( 'NONE',  #39985 ) ;
#2672 = CARTESIAN_POINT ( 'NONE',  ( -20.22995720542193254, 21.73644205237998506, 5.000000000000000888 ) ) ;
#2673 = EDGE_CURVE ( 'NONE', #36919, #28815, #19379, .T. ) ;
#2674 = DIRECTION ( 'NONE',  ( -0.7071067811865487940, 0.7071067811865463515, 0.000000000000000000 ) ) ;
#2676 = VECTOR ( 'NONE', #9465, 1000.000000000000000 ) ;
#2675 = CARTESIAN_POINT ( 'NONE',  ( 17.50000000000000000, 0.000000000000000000, 6.094999999999989981 ) ) ;
#2677 = CARTESIAN_POINT ( 'NONE',  ( 24.18706980810188867, -2.126176841940956130, 7.934999999999990727 ) ) ;
#2679 = VECTOR ( 'NONE', #24777, 1000.000000000000227 ) ;
#2678 = DIRECTION ( 'NONE',  ( 0.7071067811865487940, 0.7071067811865463515, 0.000000000000000000 ) ) ;
#2680 = CARTESIAN_POINT ( 'NONE',  ( -29.29298673570674794, -21.74070752338405299, 4.999753212805210012 ) ) ;
#2681 = ORIENTED_EDGE ( 'NONE', *, *, #68927, .T. ) ;
#2682 = CARTESIAN_POINT ( 'NONE',  ( -21.29974487139158512, -27.71228299555221142, 4.000000000000000000 ) ) ;
#2683 = ORIENTED_EDGE ( 'NONE', *, *, #129377, .F. ) ;
#2686 = EDGE_CURVE ( 'NONE', #22961, #80080, #128162, .T. ) ;
#2685 = VECTOR ( 'NONE', #69507, 999.9999999999998863 ) ;
#2684 = CARTESIAN_POINT ( 'NONE',  ( 91.87543019189811844, -5.291415217122920289, -3.055000000000001492 ) ) ;
#2687 = DIRECTION ( 'NONE',  ( -0.7071067811865486830, -0.7071067811865464625, -0.000000000000000000 ) ) ;
#2688 = CARTESIAN_POINT ( 'NONE',  ( 19.02964696762728636, -22.22500000000000142, 25.44543266665133885 ) ) ;
#2690 = VECTOR ( 'NONE', #78443, 999.9999999999998863 ) ;
#2689 = DIRECTION ( 'NONE',  ( -0.7071067811865486830, 0.7071067811865464625, 0.000000000000000000 ) ) ;
#2691 = CARTESIAN_POINT ( 'NONE',  ( 124.0768256643040388, -45.23984008851422089, -35.04755940937664604 ) ) ;
#2692 = ORIENTED_EDGE ( 'NONE', *, *, #103610, .T. ) ;
#2693 = DIRECTION ( 'NONE',  ( 0.000000000000000000, 0.000000000000000000, 1.000000000000000000 ) ) ;
#2694 = ADVANCED_FACE ( 'NONE', ( #61499 ), #128846, .F. ) ;
#2695 = FACE_OUTER_BOUND ( 'NONE', #133482, .T. ) ;
#2696 = ORIENTED_EDGE ( 'NONE', *, *, #27152, .T. ) ;
#2697 = CARTESIAN_POINT ( 'NONE',  ( -21.48921356237309155, -27.52281430457070499, 5.000000000000000000 ) ) ;
#2698 = ADVANCED_FACE ( 'NONE', ( #29522 ), #94775, .F. ) ;
#2699 = EDGE_CURVE ( 'NONE', #121977, #75295, #129555, .T. ) ;
#2700 = DIRECTION ( 'NONE',  ( -0.7071067811865486830, -0.7071067811865464625, 0.000000000000000000 ) ) ;
#2702 = ORIENTED_EDGE ( 'NONE', *, *, #17294, .T. ) ;
#2701 = CARTESIAN_POINT ( 'NONE',  ( 23.99451991528749062, 28.92564299267954908, 4.000000000000000000 ) ) ;
#2703 = CARTESIAN_POINT ( 'NONE',  ( 5.999999999999970690, 20.96639925780204905, 5.000000000000000000 ) ) ;
#2704 = DIRECTION ( 'NONE',  ( -1.000000000000000000, -0.000000000000000000, -0.000000000000000000 ) ) ;
#2705 = VECTOR ( 'NONE', #46814, 999.9999999999998863 ) ;
#2706 = DIRECTION ( 'NONE',  ( -0.000000000000000000, 0.000000000000000000, 1.000000000000000000 ) ) ;
#2707 = FACE_OUTER_BOUND ( 'NONE', #18162, .T. ) ;
#2708 = FACE_OUTER_BOUND ( 'NONE', #125792, .T. ) ;
#2709 = EDGE_CURVE ( 'NONE', #42434, #39115, #139763, .T. ) ;
#2711 = VERTEX_POINT ( 'NONE', #9166 ) ;
#2710 = EDGE_CURVE ( 'NONE', #89978, #101438, #87498, .T. ) ;
#2712 = EDGE_LOOP ( 'NONE', ( #25102, #63841, #133635, #9677 ) ) ;
#2713 = VERTEX_POINT ( 'NONE', #32411 ) ;
#2714 = CARTESIAN_POINT ( 'NONE',  ( 79.04209685856477563, 5.291415217122923842, -3.054999999999996163 ) ) ;
#2715 = EDGE_LOOP ( 'NONE', ( #11447, #78910, #72154, #63725 ) ) ;
#2716 = EDGE_CURVE ( 'NONE', #26708, #80820, #130306, .T. ) ;
#2717 = DIRECTION ( 'NONE',  ( -0.7071067811865486830, -0.7071067811865464625, 0.000000000000000000 ) ) ;
#2718 = CARTESIAN_POINT ( 'NONE',  ( -23.99999999999983658, 2.342191155542430181, -5.001666872980029765 ) ) ;
#2719 = DIRECTION ( 'NONE',  ( 0.000000000000000000, -1.000000000000000000, 0.000000000000000000 ) ) ;
#2720 = CARTESIAN_POINT ( 'NONE',  ( 1.499999999999987566, 22.22500000000000142, 4.362957392718795901 ) ) ;
#2721 = EDGE_LOOP ( 'NONE', ( #3345, #136037, #40475 ) ) ;
#2722 = VECTOR ( 'NONE', #94099, 999.9999999999998863 ) ;
#2723 = MECHANICAL_DESIGN_GEOMETRIC_PRESENTATION_REPRESENTATION (  '', ( #65265 ), #107034 ) ;
#2724 = LINE ( 'NONE', #4823, #130093 ) ;
#2725 = CARTESIAN_POINT ( 'NONE',  ( -78.29974487139158157, -27.71228299555260577, 4.000000000000000000 ) ) ;
#2726 = CIRCLE ( 'NONE', #21261, 2.500000000000000444 ) ;
#2727 = EDGE_CURVE ( 'NONE', #109693, #12547, #75219, .T. ) ;
#2729 = AXIS2_PLACEMENT_3D ( 'NONE', #76239, #142911, #128482 ) ;
#2728 = CARTESIAN_POINT ( 'NONE',  ( 33.32816939922329880, 20.25929247661551003, 4.000000000000000000 ) ) ;
#2730 = CARTESIAN_POINT ( 'NONE',  ( 80.84959685856478018, 6.109999999999996767, 1.637169565754163836 ) ) ;
#2731 = ORIENTED_EDGE ( 'NONE', *, *, #32007, .F. ) ;
#2732 = CARTESIAN_POINT ( 'NONE',  ( 24.52400138585431577, 22.03583458319438293, 4.979811245910089390 ) ) ;
#2733 = AXIS2_PLACEMENT_3D ( 'NONE', #15507, #102583, #123634 ) ;
#2734 = DIRECTION ( 'NONE',  ( -0.7071067811865486830, -0.7071067811865464625, 0.000000000000000000 ) ) ;
#2735 = EDGE_CURVE ( 'NONE', #128291, #39409, #98380, .T. ) ;
#2736 = ORIENTED_EDGE ( 'NONE', *, *, #17084, .F. ) ;
#2737 = ORIENTED_EDGE ( 'NONE', *, *, #52281, .F. ) ;
#2738 = PLANE ( 'NONE',  #130244 ) ;
#2739 = FACE_OUTER_BOUND ( 'NONE', #96191, .T. ) ;
#2740 = CARTESIAN_POINT ( 'NONE',  ( 25.15040314143521627, 7.934999999999988951, -2.126176841940961904 ) ) ;
#2741 = LINE ( 'NONE', #81048, #99795 ) ;
#2742 = EDGE_CURVE ( 'NONE', #110817, #65645, #131012, .T. ) ;
#2743 = CARTESIAN_POINT ( 'NONE',  ( -5.700255128608413102, -27.71228299555201957, 4.000000000000000000 ) ) ;
#2744 = DIRECTION ( 'NONE',  ( 0.7071067811865486830, -0.7071067811865464625, -0.000000000000000000 ) ) ;
#2745 = DIRECTION ( 'NONE',  ( -0.7071067811865486830, -0.7071067811865464625, 0.000000000000000000 ) ) ;
#2746 = VERTEX_POINT ( 'NONE', #54192 ) ;
#2747 = ORIENTED_EDGE ( 'NONE', *, *, #44337, .T. ) ;
#2748 = DIRECTION ( 'NONE',  ( 0.3543493200069162685, -0.000000000000000000, -0.9351131265310288487 ) ) ;
#2749 = VERTEX_POINT ( 'NONE', #97646 ) ;
#2750 = ORIENTED_EDGE ( 'NONE', *, *, #14849, .F. ) ;
#2751 = EDGE_CURVE ( 'NONE', #125118, #3555, #86071, .T. ) ;
#2752 = VECTOR ( 'NONE', #25053, 1000.000000000000000 ) ;
#2753 = EDGE_CURVE ( 'NONE', #89590, #131877, #7216, .T. ) ;
#2754 = VECTOR ( 'NONE', #63417, 1000.000000000000000 ) ;
#2755 = DIRECTION ( 'NONE',  ( -0.6830127018922181881, 0.6830127018922202975, -0.2588190451025214056 ) ) ;
#2756 = VERTEX_POINT ( 'NONE', #31688 ) ;
#2757 = CARTESIAN_POINT ( 'NONE',  ( 18.18398860626898994, 28.73617430169800002, 5.000000000000000000 ) ) ;
#2758 = DIRECTION ( 'NONE',  ( -0.7071067811865486830, -0.7071067811865464625, 0.000000000000000000 ) ) ;
#2759 = EDGE_CURVE ( 'NONE', #9115, #102939, #20071, .T. ) ;
#2760 = VECTOR ( 'NONE', #89125, 1000.000000000000227 ) ;
#2761 = LINE ( 'NONE', #13621, #66489 ) ;
#2762 = DIRECTION ( 'NONE',  ( 0.6830127018922180770, -0.6830127018922204085, -0.2588190451025213501 ) ) ;
#2763 = VECTOR ( 'NONE', #80647, 1000.000000000000000 ) ;
#2764 = PLANE ( 'NONE',  #102347 ) ;
#2765 = VERTEX_POINT ( 'NONE', #20885 ) ;
#2766 = ADVANCED_FACE ( 'NONE', ( #76000 ), #76741, .T. ) ;
#2767 = SURFACE_STYLE_FILL_AREA ( #121850 ) ;
#2768 = VERTEX_POINT ( 'NONE', #120923 ) ;
#2769 = FACE_OUTER_BOUND ( 'NONE', #114331, .T. ) ;
#2770 = ORIENTED_EDGE ( 'NONE', *, *, #28694, .T. ) ;
#2771 = DIRECTION ( 'NONE',  ( 0.3543493200069162685, -0.000000000000000000, -0.9351131265310288487 ) ) ;
#2772 = VERTEX_POINT ( 'NONE', #41953 ) ;
#2773 = CARTESIAN_POINT ( 'NONE',  ( -12.48921356237309155, -27.52281430457064104, 5.000000000000000000 ) ) ;
#2774 = ORIENTED_EDGE ( 'NONE', *, *, #41427, .T. ) ;
#2775 = VERTEX_POINT ( 'NONE', #74591 ) ;
#2776 = VECTOR ( 'NONE', #87300, 1000.000000000000000 ) ;
#2777 = VERTEX_POINT ( 'NONE', #129650 ) ;
#2778 = CARTESIAN_POINT ( 'NONE',  ( 93.75000000000000000, -9.735942053221458872E-16, 7.950000000000000178 ) ) ;
#2779 = LINE ( 'NONE', #24538, #995 ) ;
#2780 = CARTESIAN_POINT ( 'NONE',  ( 120.0212635252314328, -4.472830434245838482, -4.472830434245840259 ) ) ;
#2781 = FACE_OUTER_BOUND ( 'NONE', #60982, .T. ) ;
#2782 = EDGE_CURVE ( 'NONE', #18419, #6978, #87589, .T. ) ;
#2783 = DIRECTION ( 'NONE',  ( 0.000000000000000000, 1.000000000000000000, 0.000000000000000000 ) ) ;
#2785 = CARTESIAN_POINT ( 'NONE',  ( 14.70692117890024697, 4.584330080086930965E-16, 0.000000000000000000 ) ) ;
#2784 = VECTOR ( 'NONE', #73875, 1000.000000000000000 ) ;
#2786 = STYLED_ITEM ( 'NONE', ( #120887 ), #31273 ) ;
#2787 = ADVANCED_FACE ( 'NONE', ( #51407 ), #139856, .T. ) ;
#2788 = LINE ( 'NONE', #102842, #97873 ) ;
#2789 = FACE_OUTER_BOUND ( 'NONE', #119368, .T. ) ;
#2790 = ORIENTED_EDGE ( 'NONE', *, *, #91009, .T. ) ;
#2791 = FACE_OUTER_BOUND ( 'NONE', #134953, .T. ) ;
#2792 = DIRECTION ( 'NONE',  ( -0.7071067811865486830, -0.7071067811865464625, 0.000000000000000000 ) ) ;
#2793 = ORIENTED_EDGE ( 'NONE', *, *, #85, .F. ) ;
#2794 = ORIENTED_EDGE ( 'NONE', *, *, #45649, .F. ) ;
#2795 = VECTOR ( 'NONE', #136920, 1000.000000000000000 ) ;
#2796 = DIRECTION ( 'NONE',  ( -0.7071067811865486830, 0.7071067811865464625, 0.000000000000000000 ) ) ;
#2797 = ORIENTED_EDGE ( 'NONE', *, *, #44201, .T. ) ;
#2798 = PLANE ( 'NONE',  #5109 ) ;
#2799 = CARTESIAN_POINT ( 'NONE',  ( 14.33747294953710494, 6.094999999999989981, -1.119633336120465690E-15 ) ) ;
#2800 = CARTESIAN_POINT ( 'NONE',  ( -23.99999999999982592, -19.44781430457063465, 5.000000000000000000 ) ) ;
#2801 = LINE ( 'NONE', #135491, #95034 ) ;
#2802 = EDGE_CURVE ( 'NONE', #127404, #44686, #54284, .T. ) ;
#2803 = ORIENTED_EDGE ( 'NONE', *, *, #81886, .T. ) ;
#2804 = CARTESIAN_POINT ( 'NONE',  ( 18.48921356237309510, -27.52281430457068367, 5.000000000000000000 ) ) ;
#2805 = AXIS2_PLACEMENT_3D ( 'NONE', #43712, #131445, #88664 ) ;
#2806 = VERTEX_POINT ( 'NONE', #65149 ) ;
#2807 = CARTESIAN_POINT ( 'NONE',  ( -20.99451991528748707, 28.92564299267952777, 4.000000000000000000 ) ) ;
#2808 = CARTESIAN_POINT ( 'NONE',  ( 30.69206980810189123, -7.934999999999991616, -2.126176841940955242 ) ) ;
#2809 = VERTEX_POINT ( 'NONE', #40531 ) ;
#2810 = PLANE ( 'NONE',  #73735 ) ;
#2811 = DIRECTION ( 'NONE',  ( -0.000000000000000000, 0.000000000000000000, 1.000000000000000000 ) ) ;
#2812 = ORIENTED_EDGE ( 'NONE', *, *, #34720, .F. ) ;
#2813 = EDGE_LOOP ( 'NONE', ( #97197, #71112, #82582, #1452 ) ) ;
#2814 = ORIENTED_EDGE ( 'NONE', *, *, #736, .F. ) ;
#2815 = DIRECTION ( 'NONE',  ( 0.7071067811865487940, 0.7071067811865463515, 0.000000000000000000 ) ) ;
#2816 = DIRECTION ( 'NONE',  ( -0.6830127018922180770, -0.6830127018922204085, -0.2588190451025213501 ) ) ;
#2817 = VECTOR ( 'NONE', #133730, 1000.000000000000114 ) ;
#2819 = CARTESIAN_POINT ( 'NONE',  ( 18.18268087362628194, -22.22500000000000142, 25.12448555237915926 ) ) ;
#2818 = VECTOR ( 'NONE', #46373, 1000.000000000000000 ) ;
#2820 = AXIS2_PLACEMENT_3D ( 'NONE', #39865, #84086, #60177 ) ;
#2821 = EDGE_LOOP ( 'NONE', ( #114591, #67792, #81456, #68040 ) ) ;
#2822 = CARTESIAN_POINT ( 'NONE',  ( 30.18398860626900060, 28.73617430169808173, 5.000000000000000000 ) ) ;
#2823 = AXIS2_PLACEMENT_3D ( 'NONE', #138707, #69164, #116223 ) ;
#2824 = CARTESIAN_POINT ( 'NONE',  ( 32.20710678118632586, 6.759292476615653023, 5.000000000000000000 ) ) ;
#2825 = AXIS2_PLACEMENT_3D ( 'NONE', #33316, #33994, #45608 ) ;
#2826 = EDGE_CURVE ( 'NONE', #124530, #3810, #118032, .T. ) ;
#2827 = CARTESIAN_POINT ( 'NONE',  ( 5.999999999999960032, 8.966399257802164513, 5.000000000000000000 ) ) ;
#2828 = FACE_OUTER_BOUND ( 'NONE', #81836, .T. ) ;
#2829 = ORIENTED_EDGE ( 'NONE', *, *, #112687, .T. ) ;
#2830 = AXIS2_PLACEMENT_3D ( 'NONE', #71216, #40028, #4429 ) ;
#2831 = STYLED_ITEM ( 'NONE', ( #89354 ), #66228 ) ;
#2832 = AXIS2_PLACEMENT_3D ( 'NONE', #48944, #83731, #105431 ) ;
#2833 = PLANE ( 'NONE',  #35466 ) ;
#2834 = ORIENTED_EDGE ( 'NONE', *, *, #102929, .F. ) ;
#2836 = VERTEX_POINT ( 'NONE', #130394 ) ;
#2835 = CARTESIAN_POINT ( 'NONE',  ( 60.76962477605442814, -44.19516442797058886, -34.92499999999998295 ) ) ;
#2837 = ORIENTED_EDGE ( 'NONE', *, *, #60531, .F. ) ;
#2838 = EDGE_CURVE ( 'NONE', #108536, #77576, #96281, .T. ) ;
#2839 = CARTESIAN_POINT ( 'NONE',  ( 32.67183060077624646, -15.74070752338412049, 4.000000000000000000 ) ) ;
#2840 = CARTESIAN_POINT ( 'NONE',  ( 104.5416666666666714, -3.975000000000002753, 6.884901960086286188 ) ) ;
#2841 = ORIENTED_EDGE ( 'NONE', *, *, #48314, .F. ) ;
#2842 = UNCERTAINTY_MEASURE_WITH_UNIT (LENGTH_MEASURE( 1.000000000000000082E-05 ), #105526, 'distance_accuracy_value', 'NONE');
#2843 = ORIENTED_EDGE ( 'NONE', *, *, #19754, .F. ) ;
#2844 = LINE ( 'NONE', #13701, #63738 ) ;
#2845 = DIRECTION ( 'NONE',  ( 0.7071067811865487940, 0.7071067811865463515, 0.000000000000000000 ) ) ;
#2846 = PLANE ( 'NONE',  #127235 ) ;
#2847 = CARTESIAN_POINT ( 'NONE',  ( -32.99999999999976552, -6.108550654416993630, -3.114665004255040781 ) ) ;
#2848 = CARTESIAN_POINT ( 'NONE',  ( -10.49999999999992539, -9.462702396501018853, -9.474982329943488324 ) ) ;
#2849 = LINE ( 'NONE', #100752, #30657 ) ;
#2850 = DIRECTION ( 'NONE',  ( -0.5735764363510499342, -0.8191520442889891340, 0.000000000000000000 ) ) ;
#2851 = DIRECTION ( 'NONE',  ( -0.7071067811865486830, -0.7071067811865464625, 0.000000000000000000 ) ) ;
#2852 = CARTESIAN_POINT ( 'NONE',  ( 23.31206980810188512, 7.934999999999993392, 2.126176841940951689 ) ) ;
#2853 = CARTESIAN_POINT ( 'NONE',  ( 13.92145407031093818, 4.584330080086930965E-16, 0.000000000000000000 ) ) ;
#2854 = LINE ( 'NONE', #69587, #48219 ) ;
#2855 = CARTESIAN_POINT ( 'NONE',  ( 14.20666063542142687, 21.75929247661549937, 4.998822639870700080 ) ) ;
#2856 = PLANE ( 'NONE',  #110182 ) ;
#2857 = EDGE_LOOP ( 'NONE', ( #25330, #20229, #67010, #104199, #27651 ) ) ;
#2858 = ORIENTED_EDGE ( 'NONE', *, *, #35205, .F. ) ;
#2859 = CARTESIAN_POINT ( 'NONE',  ( 88.79166666666665719, 3.975000000000003642, -6.884901960086285300 ) ) ;
#2860 = VERTEX_POINT ( 'NONE', #119469 ) ;
#2861 = VERTEX_POINT ( 'NONE', #31084 ) ;
#2862 = B_SPLINE_CURVE_WITH_KNOTS ( 'NONE', 3,
 ( #57172, #101347, #46299, #18589, #127377, #96156, #83174, #116512, #70891, #16449, #94730, #40400, #51980, #60754 ),
 .UNSPECIFIED., .F., .F.,
 ( 4, 2, 2, 2, 2, 2, 4 ),
 ( 0.000000000000000000, 0.001506850370412668103, 0.002260275555619002154, 0.003013700740825336205, 0.003767125926031670256, 0.004520551111238004308, 0.006027401481650672410 ),
 .UNSPECIFIED. ) ;
#2863 = VECTOR ( 'NONE', #65070, 1000.000000000000000 ) ;
#2864 = ORIENTED_EDGE ( 'NONE', *, *, #129952, .F. ) ;
#2865 = ADVANCED_FACE ( 'NONE', ( #10020 ), #29616, .T. ) ;
#2866 = CARTESIAN_POINT ( 'NONE',  ( -32.99999999999977263, 4.384688058510537445, -7.090945410444762231 ) ) ;
#2867 = CARTESIAN_POINT ( 'NONE',  ( -29.99999999999978328, -12.41253812416062985, 4.000000000000000000 ) ) ;
#2868 = VECTOR ( 'NONE', #133428, 1000.000000000000000 ) ;
#2869 = CARTESIAN_POINT ( 'NONE',  ( 12.99795884586121630, 8.843280219809532383, 3.474951431101239052 ) ) ;
#2870 = ORIENTED_EDGE ( 'NONE', *, *, #102075, .F. ) ;
#2871 = LINE ( 'NONE', #125389, #48633 ) ;
#2872 = DIRECTION ( 'NONE',  ( -0.7071067811865487940, 0.7071067811865463515, 0.000000000000000000 ) ) ;
#2873 = CARTESIAN_POINT ( 'NONE',  ( 0.000000000000000000, 0.000000000000000000, 5.000000000000000000 ) ) ;
#2874 = DIRECTION ( 'NONE',  ( 0.000000000000000000, 0.000000000000000000, 1.000000000000000000 ) ) ;
#2875 = EDGE_CURVE ( 'NONE', #141302, #134952, #43378, .T. ) ;
#2876 = EDGE_CURVE ( 'NONE', #29769, #74867, #20924, .T. ) ;
#2877 = PLANE ( 'NONE',  #129740 ) ;
#2878 = CARTESIAN_POINT ( 'NONE',  ( 34.42499999999998295, 10.54139925780192932, 5.000000000000000000 ) ) ;
#2879 = CARTESIAN_POINT ( 'NONE',  ( 26.40000000000000568, -16.48000000000005016, 34.92499999999998295 ) ) ;
#2880 = CARTESIAN_POINT ( 'NONE',  ( 39.29974487139159578, -27.71228299555233576, 4.000000000000000000 ) ) ;
#2881 = CARTESIAN_POINT ( 'NONE',  ( 15.29974487139158867, -27.71228299555216879, 4.000000000000000000 ) ) ;
#2882 = CARTESIAN_POINT ( 'NONE',  ( 15.71757738642556568, -21.73023691814493219, 5.000000000000000000 ) ) ;
#2883 = CARTESIAN_POINT ( 'NONE',  ( 7.362461875838964609, 22.22500000000000142, 4.000000000000000000 ) ) ;
#2884 = EDGE_CURVE ( 'NONE', #90006, #117097, #141240, .T. ) ;
#2885 = EDGE_CURVE ( 'NONE', #20632, #105661, #141994, .T. ) ;
#2886 = EDGE_LOOP ( 'NONE', ( #3608, #78834, #90700, #136857 ) ) ;
#2887 = EDGE_LOOP ( 'NONE', ( #80635, #96807, #108926, #14800 ) ) ;
#2888 = CARTESIAN_POINT ( 'NONE',  ( 110.6879301918981184, 6.110000000000002984, -1.637169565754156730 ) ) ;
#2889 = EDGE_CURVE ( 'NONE', #3378, #79257, #26439, .T. ) ;
#2890 = EDGE_LOOP ( 'NONE', ( #38959, #26343, #102466, #10380 ) ) ;
#2891 = EDGE_CURVE ( 'NONE', #22488, #17542, #102172, .T. ) ;
#2892 = AXIS2_PLACEMENT_3D ( 'NONE', #8924, #19852, #75686 ) ;
#2893 = DIRECTION ( 'NONE',  ( -2.781805975412905890E-17, 0.3543493200069152693, 0.9351131265310292928 ) ) ;
#2894 = ADVANCED_FACE ( 'NONE', ( #55693 ), #66561, .F. ) ;
#2895 = CARTESIAN_POINT ( 'NONE',  ( -2.994519915287485734, 28.92564299267940342, 4.000000000000000000 ) ) ;
#2896 = CARTESIAN_POINT ( 'NONE',  ( 6.046588136295404148, 14.25929247661557042, 18.84478104361326345 ) ) ;
#2897 = CARTESIAN_POINT ( 'NONE',  ( -12.18398860626900060, 28.73617430169795739, 5.000000000000000000 ) ) ;
#2898 = ADVANCED_FACE ( 'NONE', ( #99890 ), #70689, .F. ) ;
#2899 = CARTESIAN_POINT ( 'NONE',  ( 100.2454301918981230, -5.291415217122918513, -3.055000000000000160 ) ) ;
#2900 = ORIENTED_EDGE ( 'NONE', *, *, #6554, .T. ) ;
#2901 = ORIENTED_EDGE ( 'NONE', *, *, #13968, .F. ) ;
#2902 = LINE ( 'NONE', #3594, #63916 ) ;
#2903 = CARTESIAN_POINT ( 'NONE',  ( 97.25000000000000000, -9.735942053221458872E-16, 7.950000000000000178 ) ) ;
#2904 = EDGE_CURVE ( 'NONE', #98425, #96060, #77461, .T. ) ;
#2905 = ORIENTED_EDGE ( 'NONE', *, *, #11671, .F. ) ;
#2906 = VERTEX_POINT ( 'NONE', #71377 ) ;
#2907 = VERTEX_POINT ( 'NONE', #4607 ) ;
#2908 = PLANE ( 'NONE',  #12026 ) ;
#2909 = CARTESIAN_POINT ( 'NONE',  ( 1.233736474768552860, 5.808823158059035485, 5.808823158059032821 ) ) ;
#2910 = VECTOR ( 'NONE', #24639, 1000.000000000000000 ) ;
#2911 = EDGE_CURVE ( 'NONE', #6460, #22107, #114837, .T. ) ;
#2912 = CARTESIAN_POINT ( 'NONE',  ( 33.16209685856478018, -5.291415217122919401, 3.054999999999997939 ) ) ;
#2913 = ORIENTED_EDGE ( 'NONE', *, *, #75065, .T. ) ;
#2914 = ORIENTED_EDGE ( 'NONE', *, *, #100813, .F. ) ;
#2915 = DIRECTION ( 'NONE',  ( 0.3543493200069162685, -0.000000000000000000, -0.9351131265310288487 ) ) ;
#2916 = ORIENTED_EDGE ( 'NONE', *, *, #44396, .T. ) ;
#2917 = EDGE_LOOP ( 'NONE', ( #136745, #86290, #53238, #52829 ) ) ;
#2918 = VECTOR ( 'NONE', #102357, 1000.000000000000000 ) ;
#2919 = EDGE_LOOP ( 'NONE', ( #55155, #101299, #91850, #128345, #50723 ) ) ;
#2920 = AXIS2_PLACEMENT_3D ( 'NONE', #66953, #42365, #100299 ) ;
#2921 = VECTOR ( 'NONE', #68999, 1000.000000000000000 ) ;
#2922 = CYLINDRICAL_SURFACE ( 'NONE', #121136, 7.950000000000000178 ) ;
#2923 = AXIS2_PLACEMENT_3D ( 'NONE', #51660, #9534, #110280 ) ;
#2924 = EDGE_CURVE ( 'NONE', #50248, #142882, #143391, .T. ) ;
#2925 = DIRECTION ( 'NONE',  ( 2.781805975412905890E-17, -0.3543493200069152693, 0.9351131265310292928 ) ) ;
#2926 = DIRECTION ( 'NONE',  ( -0.7071067811865487940, 0.7071067811865463515, -0.000000000000000000 ) ) ;
#2927 = VERTEX_POINT ( 'NONE', #103266 ) ;
#2928 = CARTESIAN_POINT ( 'NONE',  ( -26.99999999999980815, -12.03360074219761700, 5.000000000000000000 ) ) ;
#2929 = ADVANCED_FACE ( 'NONE', ( #78879 ), #559, .T. ) ;
#2930 = AXIS2_PLACEMENT_3D ( 'NONE', #104612, #49559, #93741 ) ;
#2931 = VECTOR ( 'NONE', #119304, 1000.000000000000000 ) ;
#2932 = LINE ( 'NONE', #93523, #27469 ) ;
#2933 = ADVANCED_FACE ( 'NONE', ( #92376 ), #37674, .T. ) ;
#2934 = FACE_OUTER_BOUND ( 'NONE', #131274, .T. ) ;
#2935 = FACE_BOUND ( 'NONE', #8113, .T. ) ;
#2936 = ORIENTED_EDGE ( 'NONE', *, *, #19255, .F. ) ;
#2937 = LINE ( 'NONE', #47231, #41126 ) ;
#2938 = CARTESIAN_POINT ( 'NONE',  ( -13.21498419724181517, -3.740707523384244837, 15.76143240460121220 ) ) ;
#2939 = DIRECTION ( 'NONE',  ( 0.7071067811865487940, 0.7071067811865463515, 0.000000000000000000 ) ) ;
#2940 = ORIENTED_EDGE ( 'NONE', *, *, #46505, .T. ) ;
#2941 = DIRECTION ( 'NONE',  ( 0.7071067811865486830, -0.7071067811865464625, -0.000000000000000000 ) ) ;
#2942 = ORIENTED_EDGE ( 'NONE', *, *, #124276, .T. ) ;
#2943 = VERTEX_POINT ( 'NONE', #111475 ) ;
#2944 = ORIENTED_EDGE ( 'NONE', *, *, #92942, .F. ) ;
#2945 = CARTESIAN_POINT ( 'NONE',  ( 39.28709685856478018, 3.054999999999997495, 5.291415217122919401 ) ) ;
#2946 = VERTEX_POINT ( 'NONE', #56443 ) ;
#2947 = VECTOR ( 'NONE', #92331, 1000.000000000000000 ) ;
#2948 = CARTESIAN_POINT ( 'NONE',  ( -33.29974487139158867, -27.71228299555229313, 4.000000000000000000 ) ) ;
#2949 = LINE ( 'NONE', #113860, #3317 ) ;
#2950 = EDGE_CURVE ( 'NONE', #94849, #25409, #23005, .T. ) ;
#2951 = EDGE_LOOP ( 'NONE', ( #106972, #86066, #39161, #121826 ) ) ;
#2952 = CARTESIAN_POINT ( 'NONE',  ( 30.32816939922331656, 2.259292476615694323, 4.000000000000000000 ) ) ;
#2954 = DIRECTION ( 'NONE',  ( 0.6830127018922181881, 0.6830127018922202975, -0.2588190451025214056 ) ) ;
#2953 = VECTOR ( 'NONE', #9343, 1000.000000000000000 ) ;
#2955 = DIRECTION ( 'NONE',  ( 1.055184596092948005E-16, -1.000000000000000000, 0.000000000000000000 ) ) ;
#2957 = ADVANCED_FACE ( 'NONE', ( #89724 ), #33255, .T. ) ;
#2956 = CARTESIAN_POINT ( 'NONE',  ( -14.60438740478481989, -0.8081507193758268315, 4.000000000000000000 ) ) ;
#2958 = AXIS2_PLACEMENT_3D ( 'NONE', #137286, #26379, #90187 ) ;
#2959 = DIRECTION ( 'NONE',  ( 0.7071067811865486830, -0.7071067811865464625, -0.000000000000000000 ) ) ;
#2960 = ORIENTED_EDGE ( 'NONE', *, *, #2258, .F. ) ;
#2961 = ORIENTED_EDGE ( 'NONE', *, *, #74069, .T. ) ;
#2962 = ORIENTED_EDGE ( 'NONE', *, *, #137949, .T. ) ;
#2963 = ORIENTED_EDGE ( 'NONE', *, *, #13092, .T. ) ;
#2964 = AXIS2_PLACEMENT_3D ( 'NONE', #136803, #81749, #16423 ) ;
#2965 = CARTESIAN_POINT ( 'NONE',  ( -2.999999999999981792, -5.527737879153195699, -7.983877177622365373 ) ) ;
#2966 = ORIENTED_EDGE ( 'NONE', *, *, #113345, .F. ) ;
#2967 = ORIENTED_EDGE ( 'NONE', *, *, #16620, .F. ) ;
#2968 = DIRECTION ( 'NONE',  ( 0.3543493200069163240, 0.000000000000000000, -0.9351131265310288487 ) ) ;
#2969 = EDGE_CURVE ( 'NONE', #86443, #123774, #30739, .T. ) ;
#2970 = CARTESIAN_POINT ( 'NONE',  ( 2.999999999999981792, 7.588810512006216591, -3.013526669885234099 ) ) ;
#2971 = ADVANCED_FACE ( 'NONE', ( #138056 ), #85092, .F. ) ;
#2972 = ORIENTED_EDGE ( 'NONE', *, *, #112737, .T. ) ;
#2973 = DIRECTION ( 'NONE',  ( 0.6830127018922181881, 0.6830127018922202975, -0.2588190451025214056 ) ) ;
#2974 = VERTEX_POINT ( 'NONE', #40886 ) ;
#2976 = AXIS2_PLACEMENT_3D ( 'NONE', #93608, #126917, #50109 ) ;
#2975 = CARTESIAN_POINT ( 'NONE',  ( 23.67183060077630330, -15.74070752338411339, 4.000000000000000000 ) ) ;
#2977 = EDGE_CURVE ( 'NONE', #47310, #141344, #83707, .T. ) ;
#2978 = CARTESIAN_POINT ( 'NONE',  ( 29.52540314143522338, 2.126176841940962348, 7.934999999999989839 ) ) ;
#2979 = CARTESIAN_POINT ( 'NONE',  ( 0.6504031414352192675, 7.934999999999989839, -2.126176841940961904 ) ) ;
#2980 = ORIENTED_EDGE ( 'NONE', *, *, #81699, .F. ) ;
#2981 = CARTESIAN_POINT ( 'NONE',  ( 107.9745968585647660, 1.637169565754164280, -6.109999999999997655 ) ) ;
#2982 = DIRECTION ( 'NONE',  ( 1.000000000000000000, 0.000000000000000000, 0.000000000000000000 ) ) ;
#2983 = DIRECTION ( 'NONE',  ( 0.7071067811865486830, -0.7071067811865464625, -0.000000000000000000 ) ) ;
#2984 = AXIS2_PLACEMENT_3D ( 'NONE', #16080, #37905, #93694 ) ;
#2985 = ORIENTED_EDGE ( 'NONE', *, *, #121994, .F. ) ;
#2986 =( NAMED_UNIT ( * ) PLANE_ANGLE_UNIT ( ) SI_UNIT ( $, .RADIAN. ) );
#2988 = ORIENTED_EDGE ( 'NONE', *, *, #21911, .T. ) ;
#2987 = CARTESIAN_POINT ( 'NONE',  ( 29.99999999999979750, -18.41253812416056235, 4.000000000000000000 ) ) ;
#2990 = VECTOR ( 'NONE', #1431, 1000.000000000000000 ) ;
#2989 = LINE ( 'NONE', #25450, #117983 ) ;
#2991 = DIRECTION ( 'NONE',  ( -0.7071067811865487940, 0.7071067811865463515, 0.000000000000000000 ) ) ;
#2992 = LINE ( 'NONE', #91457, #8039 ) ;
#2993 = CARTESIAN_POINT ( 'NONE',  ( 15.79289321881335439, -5.240707523384221744, 5.000000000000000000 ) ) ;
#2994 = LINE ( 'NONE', #135674, #77317 ) ;
#2997 = EDGE_CURVE ( 'NONE', #139608, #43233, #7516, .T. ) ;
#2996 = ORIENTED_EDGE ( 'NONE', *, *, #16515, .T. ) ;
#2995 =( BOUNDED_CURVE ( )  B_SPLINE_CURVE ( 3, ( #45291, #122811, #13312, #46743 ),
 .UNSPECIFIED., .F., .F. ) 
 B_SPLINE_CURVE_WITH_KNOTS ( ( 4, 4 ),
 ( 5.043186909253415173, 5.074607125596370949 ),
 .UNSPECIFIED. ) 
 CURVE ( )  GEOMETRIC_REPRESENTATION_ITEM ( )  RATIONAL_B_SPLINE_CURVE ( ( 1.000000000000000000, 0.9999177325257868620, 0.9999177325257868620, 1.000000000000000000 ) ) 
 REPRESENTATION_ITEM ( '' )  );
#2998 = CARTESIAN_POINT ( 'NONE',  ( 0.000000000000000000, 0.000000000000000000, 5.000000000000000000 ) ) ;
#2999 = EDGE_CURVE ( 'NONE', #38388, #85885, #19125, .T. ) ;
#3000 = CARTESIAN_POINT ( 'NONE',  ( 12.19999999999999574, -34.51840020119763608, 17.97447928118983640 ) ) ;
#3001 = FACE_OUTER_BOUND ( 'NONE', #125880, .T. ) ;
#3002 = ORIENTED_EDGE ( 'NONE', *, *, #39321, .T. ) ;
#3003 = CARTESIAN_POINT ( 'NONE',  ( -34.92499999999999005, -3.270000000000013340, -37.00000000000000000 ) ) ;
#3004 = VECTOR ( 'NONE', #133806, 1000.000000000000000 ) ;
#3005 =( BOUNDED_CURVE ( )  B_SPLINE_CURVE ( 3, ( #103964, #48192, #122896, #4608 ),
 .UNSPECIFIED., .F., .F. ) 
 B_SPLINE_CURVE_WITH_KNOTS ( ( 4, 4 ),
 ( 1.901594255663603183, 1.933014472006550966 ),
 .UNSPECIFIED. ) 
 CURVE ( )  GEOMETRIC_REPRESENTATION_ITEM ( )  RATIONAL_B_SPLINE_CURVE ( ( 1.000000000000000000, 0.9999177325257868620, 0.9999177325257868620, 1.000000000000000000 ) ) 
 REPRESENTATION_ITEM ( '' )  );
#3006 = LINE ( 'NONE', #47979, #74788 ) ;
#3007 = ORIENTED_EDGE ( 'NONE', *, *, #14711, .T. ) ;
#3009 = VERTEX_POINT ( 'NONE', #40203 ) ;
#3008 = DIRECTION ( 'NONE',  ( -0.7071067811865487940, 0.7071067811865463515, 0.000000000000000000 ) ) ;
#3010 = EDGE_CURVE ( 'NONE', #9331, #58595, #93214, .T. ) ;
#3011 = ORIENTED_EDGE ( 'NONE', *, *, #104011, .T. ) ;
#3012 = VECTOR ( 'NONE', #15009, 1000.000000000000000 ) ;
#3013 = DIRECTION ( 'NONE',  ( -0.7071067811865486830, -0.7071067811865464625, 0.000000000000000000 ) ) ;
#3014 = CARTESIAN_POINT ( 'NONE',  ( -20.99999999999985789, -10.77435723561697145, -9.972017380717186796 ) ) ;
#3015 = VERTEX_POINT ( 'NONE', #29987 ) ;
#3016 = SURFACE_STYLE_USAGE ( .BOTH. , #22088 ) ;
#3017 = DIRECTION ( 'NONE',  ( 0.6830127018922180770, -0.6830127018922204085, -0.2588190451025213501 ) ) ;
#3018 = ORIENTED_EDGE ( 'NONE', *, *, #80098, .F. ) ;
#3019 = CARTESIAN_POINT ( 'NONE',  ( 22.25000000000000000, 2.143131898507868051E-16, -1.749999999999999778 ) ) ;
#3020 = CARTESIAN_POINT ( 'NONE',  ( -15.79289321881334196, -17.24070752338410628, 5.000000000000000000 ) ) ;
#3021 = DIRECTION ( 'NONE',  ( 0.3543493200069162685, -0.000000000000000000, -0.9351131265310288487 ) ) ;
#3022 = AXIS2_PLACEMENT_3D ( 'NONE', #120297, #10833, #42094 ) ;
#3023 = DIRECTION ( 'NONE',  ( -0.7071067811865487940, 0.7071067811865463515, 0.000000000000000000 ) ) ;
#3024 = CARTESIAN_POINT ( 'NONE',  ( 126.2740448710917320, -7.159498723440732348, 0.5736663686628497016 ) ) ;
#3025 = LINE ( 'NONE', #37086, #65102 ) ;
#3026 = DIRECTION ( 'NONE',  ( -0.000000000000000000, 0.000000000000000000, 1.000000000000000000 ) ) ;
#3027 = ORIENTED_EDGE ( 'NONE', *, *, #61422, .T. ) ;
#3028 = AXIS2_PLACEMENT_3D ( 'NONE', #48625, #60233, #136331 ) ;
#3029 = VERTEX_POINT ( 'NONE', #28593 ) ;
#3030 = VERTEX_POINT ( 'NONE', #30740 ) ;
#3031 = CARTESIAN_POINT ( 'NONE',  ( 120.4374999999999858, 5.819803920172573974, -5.819803920172572198 ) ) ;
#3032 = ORIENTED_EDGE ( 'NONE', *, *, #74849, .F. ) ;
#3033 = EDGE_LOOP ( 'NONE', ( #122028, #131656, #46271 ) ) ;
#3034 = ORIENTED_EDGE ( 'NONE', *, *, #43142, .T. ) ;
#3035 = AXIS2_PLACEMENT_3D ( 'NONE', #94451, #114758, #70619 ) ;
#3036 = DIRECTION ( 'NONE',  ( -0.6830127018922181881, 0.6830127018922202975, -0.2588190451025214056 ) ) ;
#3037 = ORIENTED_EDGE ( 'NONE', *, *, #70665, .F. ) ;
#3038 = DIRECTION ( 'NONE',  ( 0.7071067811865487940, -0.7071067811865463515, 0.000000000000000000 ) ) ;
#3039 = DIRECTION ( 'NONE',  ( 0.7071067811865486830, -0.7071067811865464625, -0.000000000000000000 ) ) ;
#3040 = PLANE ( 'NONE',  #81060 ) ;
#3041 = CARTESIAN_POINT ( 'NONE',  ( -17.99999999999987210, 12.83542986846995504, -1.025386466790330076 ) ) ;
#3042 = CARTESIAN_POINT ( 'NONE',  ( 108.9379301918981042, -6.110000000000001208, 1.637169565754158951 ) ) ;
#3043 = ORIENTED_EDGE ( 'NONE', *, *, #27290, .F. ) ;
#3044 = ADVANCED_FACE ( 'NONE', ( #72850 ), #17672, .T. ) ;
#3045 = DIRECTION ( 'NONE',  ( -2.781805975412905890E-17, 0.3543493200069152693, 0.9351131265310292928 ) ) ;
#3046 = DIRECTION ( 'NONE',  ( -0.3543493200069162685, -0.000000000000000000, -0.9351131265310288487 ) ) ;
#3047 = CIRCLE ( 'NONE', #37746, 2.055000000000000604 ) ;
#3048 = LINE ( 'NONE', #137878, #142172 ) ;
#3049 = DIRECTION ( 'NONE',  ( -0.7071067811865487940, 0.7071067811865463515, -0.000000000000000000 ) ) ;
#3050 = CARTESIAN_POINT ( 'NONE',  ( -2.999999999999968026, 11.96639925780214675, 5.000000000000000000 ) ) ;
#3051 = LINE ( 'NONE', #25515, #107019 ) ;
#3052 = DIRECTION ( 'NONE',  ( -0.000000000000000000, -0.3543493200069152693, 0.9351131265310292928 ) ) ;
#3053 = CARTESIAN_POINT ( 'NONE',  ( 43.10002705046289861, 5.819803920172570422, 5.819803920172574863 ) ) ;
#3054 = CARTESIAN_POINT ( 'NONE',  ( 2.207106781186528810, 9.759292476615625489, 5.000000000000000000 ) ) ;
#3055 = EDGE_CURVE ( 'NONE', #136825, #90110, #115538, .T. ) ;
#3057 = CARTESIAN_POINT ( 'NONE',  ( -31.17183060077625356, -5.240707523384225297, 4.000000000000000000 ) ) ;
#3056 = VECTOR ( 'NONE', #44435, 1000.000000000000000 ) ;
#3058 = EDGE_LOOP ( 'NONE', ( #17079, #6653, #115395, #37668 ) ) ;
#3059 = ORIENTED_EDGE ( 'NONE', *, *, #103222, .T. ) ;
#3060 = CARTESIAN_POINT ( 'NONE',  ( 37.60416666666666430, 2.130196079827422206, 7.950000000000001954 ) ) ;
#3061 = ADVANCED_FACE ( 'NONE', ( #61945 ), #106095, .F. ) ;
#3062 = VERTEX_POINT ( 'NONE', #85801 ) ;
#3063 = VERTEX_POINT ( 'NONE', #51773 ) ;
#3064 = DIRECTION ( 'NONE',  ( 0.7071067811865487940, 0.7071067811865463515, 0.000000000000000000 ) ) ;
#3065 = ADVANCED_FACE ( 'NONE', ( #128605 ), #116295, .F. ) ;
#3066 = CARTESIAN_POINT ( 'NONE',  ( -26.70025512860841488, -27.71228299555187391, 4.000000000000000000 ) ) ;
#3067 = ORIENTED_EDGE ( 'NONE', *, *, #120246, .F. ) ;
#3068 = EDGE_CURVE ( 'NONE', #90489, #14841, #61261, .T. ) ;
#3069 = CARTESIAN_POINT ( 'NONE',  ( -47.99451991528749062, 28.92564299267971251, 4.000000000000000000 ) ) ;
#3070 = VECTOR ( 'NONE', #281, 1000.000000000000000 ) ;
#3071 = CARTESIAN_POINT ( 'NONE',  ( -23.27718569542924243, -21.72500000000000142, 5.000000000000000000 ) ) ;
#3072 = CARTESIAN_POINT ( 'NONE',  ( 42.72959685856476142, -6.110000000000000320, -1.637169565754161393 ) ) ;
#3073 = VECTOR ( 'NONE', #82646, 1000.000000000000000 ) ;
#3075 = EDGE_CURVE ( 'NONE', #101812, #82012, #134955, .T. ) ;
#3074 = VERTEX_POINT ( 'NONE', #29279 ) ;
#3076 = DIRECTION ( 'NONE',  ( 0.7071067811865486830, -0.7071067811865464625, -0.000000000000000000 ) ) ;
#3077 = ORIENTED_EDGE ( 'NONE', *, *, #6967, .T. ) ;
#3078 = CARTESIAN_POINT ( 'NONE',  ( -1.320799999999990870, 0.000000000000000000, 0.000000000000000000 ) ) ;
#3079 = CARTESIAN_POINT ( 'NONE',  ( -13.49999999999990408, -20.53675388469232033, 2.352720554255862684 ) ) ;
#3080 = CARTESIAN_POINT ( 'NONE',  ( 42.18398860626899705, 28.73617430169816700, 5.000000000000000000 ) ) ;
#3081 = AXIS2_PLACEMENT_3D ( 'NONE', #58344, #80078, #59053 ) ;
#3082 = ADVANCED_FACE ( 'NONE', ( #117682 ), #107552, .F. ) ;
#3083 = DIRECTION ( 'NONE',  ( -0.7071067811865486830, -0.7071067811865464625, 0.000000000000000000 ) ) ;
#3084 = VERTEX_POINT ( 'NONE', #127160 ) ;
#3085 = ADVANCED_FACE ( 'NONE', ( #41580 ), #105406, .F. ) ;
#3086 = ORIENTED_EDGE ( 'NONE', *, *, #89982, .F. ) ;
#3087 = CARTESIAN_POINT ( 'NONE',  ( -39.48921356237310221, -27.52281430457082934, 5.000000000000000000 ) ) ;
#3088 = CARTESIAN_POINT ( 'NONE',  ( 72.18398860626899705, 28.73617430169837661, 5.000000000000000000 ) ) ;
#3089 = CARTESIAN_POINT ( 'NONE',  ( 3.792893218813435663, -14.24070752338414003, 5.000000000000000000 ) ) ;
#3090 = CARTESIAN_POINT ( 'NONE',  ( 21.70710678118639692, 14.25929247661557042, 5.000000000000000000 ) ) ;
#3091 = DIRECTION ( 'NONE',  ( 0.6830127018922181881, 0.6830127018922202975, -0.2588190451025214056 ) ) ;
#3092 = EDGE_CURVE ( 'NONE', #11574, #83476, #76372, .T. ) ;
#3093 = VECTOR ( 'NONE', #41639, 1000.000000000000114 ) ;
#3094 = VECTOR ( 'NONE', #128024, 1000.000000000000000 ) ;
#3095 = CARTESIAN_POINT ( 'NONE',  ( 59.99543019189810877, 5.291415217122916737, 3.055000000000001936 ) ) ;
#3096 = LINE ( 'NONE', #49509, #132227 ) ;
#3097 = DIRECTION ( 'NONE',  ( 0.7071067811865487940, -0.7071067811865463515, -0.000000000000000000 ) ) ;
#3098 = ORIENTED_EDGE ( 'NONE', *, *, #41692, .T. ) ;
#3099 = ORIENTED_EDGE ( 'NONE', *, *, #84317, .F. ) ;
#3100 = VECTOR ( 'NONE', #123808, 1000.000000000000000 ) ;
#3101 = FACE_OUTER_BOUND ( 'NONE', #121817, .T. ) ;
#3102 = EDGE_LOOP ( 'NONE', ( #88999, #8435, #140131, #20316 ) ) ;
#3103 = PLANE ( 'NONE',  #60435 ) ;
#3104 = ORIENTED_EDGE ( 'NONE', *, *, #100168, .T. ) ;
#3105 = FILL_AREA_STYLE ('',( #68415 ) ) ;
#3106 = EDGE_CURVE ( 'NONE', #123367, #121372, #119141, .T. ) ;
#3107 = AXIS2_PLACEMENT_3D ( 'NONE', #35709, #113207, #26225 ) ;
#3108 = DIRECTION ( 'NONE',  ( 0.7071067811865487940, -0.7071067811865463515, 0.000000000000000000 ) ) ;
#3109 = FACE_BOUND ( 'NONE', #51793, .T. ) ;
#3110 = CARTESIAN_POINT ( 'NONE',  ( 3.707106781186521705, 8.259292476615639700, 5.000000000000000000 ) ) ;
#3111 = FACE_OUTER_BOUND ( 'NONE', #14633, .T. ) ;
#3113 = VERTEX_POINT ( 'NONE', #43039 ) ;
#3112 = DIRECTION ( 'NONE',  ( -0.7071067811865486830, -0.7071067811865464625, -0.000000000000000000 ) ) ;
#3114 = CARTESIAN_POINT ( 'NONE',  ( 28.49999999999980460, 11.52377502935405751, -1.522421517564149118 ) ) ;
#3115 = ADVANCED_FACE ( 'NONE', ( #21970 ), #10371, .F. ) ;
#3116 = ORIENTED_EDGE ( 'NONE', *, *, #117463, .F. ) ;
#3117 = ORIENTED_EDGE ( 'NONE', *, *, #101106, .T. ) ;
#3118 = CARTESIAN_POINT ( 'NONE',  ( 69.62043019189812298, 3.055000000000001936, -5.291415217122916737 ) ) ;
#3120 = EDGE_LOOP ( 'NONE', ( #42000, #40558, #71469, #78975 ) ) ;
#3119 = VECTOR ( 'NONE', #99052, 999.9999999999998863 ) ;
#3121 = CARTESIAN_POINT ( 'NONE',  ( -11.67183060077638679, 17.25929247661554200, 4.000000000000000000 ) ) ;
#3122 = EDGE_CURVE ( 'NONE', #72171, #12168, #11067, .T. ) ;
#3123 = ORIENTED_EDGE ( 'NONE', *, *, #75155, .T. ) ;
#3124 = FILL_AREA_STYLE_COLOUR ( '', #104610 ) ;
#3125 = VECTOR ( 'NONE', #100669, 1000.000000000000000 ) ;
#3126 = CARTESIAN_POINT ( 'NONE',  ( 17.99999999999987566, -8.151047557385048492, -8.977947279169839589 ) ) ;
#3127 = DIRECTION ( 'NONE',  ( -0.7071067811865487940, 0.7071067811865463515, -0.000000000000000000 ) ) ;
#3128 = ADVANCED_FACE ( 'NONE', ( #120541 ), #11793, .F. ) ;
#3129 = CARTESIAN_POINT ( 'NONE',  ( -22.94330788408294808, -22.22500000000000142, 9.540311041892492128 ) ) ;
#3131 = FACE_OUTER_BOUND ( 'NONE', #101997, .T. ) ;
#3130 = DIRECTION ( 'NONE',  ( 1.000000000000000000, 0.000000000000000000, 0.000000000000000000 ) ) ;
#3132 = CARTESIAN_POINT ( 'NONE',  ( 69.18398860626899705, 28.73617430169835529, 5.000000000000000000 ) ) ;
#3133 = DIRECTION ( 'NONE',  ( -0.7071067811865487940, 0.7071067811865463515, 0.000000000000000000 ) ) ;
#3134 = ORIENTED_EDGE ( 'NONE', *, *, #12577, .T. ) ;
#3135 = EDGE_CURVE ( 'NONE', #62769, #84933, #96668, .T. ) ;
#3136 = ORIENTED_EDGE ( 'NONE', *, *, #80394, .F. ) ;
#3137 = LINE ( 'NONE', #16888, #91358 ) ;
#3138 = PLANE ( 'NONE',  #60625 ) ;
#3139 = ORIENTED_EDGE ( 'NONE', *, *, #95939, .F. ) ;
#3140 = VERTEX_POINT ( 'NONE', #21270 ) ;
#3141 = ORIENTED_EDGE ( 'NONE', *, *, #77429, .T. ) ;
#3142 = ADVANCED_FACE ( 'NONE', ( #130772 ), #65529, .F. ) ;
#3143 =( REPRESENTATION_RELATIONSHIP ('NONE','NONE', #69070, #64389 ) REPRESENTATION_RELATIONSHIP_WITH_TRANSFORMATION ( #66261 )SHAPE_REPRESENTATION_RELATIONSHIP( ) );
#3144 = DIRECTION ( 'NONE',  ( 0.7071067811865486830, -0.7071067811865464625, -0.000000000000000000 ) ) ;
#3145 = ORIENTED_EDGE ( 'NONE', *, *, #127067, .F. ) ;
#3146 = AXIS2_PLACEMENT_3D ( 'NONE', #70913, #83197, #103489 ) ;
#3147 = FACE_OUTER_BOUND ( 'NONE', #18353, .T. ) ;
#3148 = VECTOR ( 'NONE', #94137, 999.9999999999998863 ) ;
#3149 = CARTESIAN_POINT ( 'NONE',  ( -1.099596858564781066, -7.934999999999989839, 2.126176841940957907 ) ) ;
#3150 = CARTESIAN_POINT ( 'NONE',  ( 14.92996780037367799, 4.193323835446171266, -32.27671736793806900 ) ) ;
#3151 = EDGE_LOOP ( 'NONE', ( #4845, #49636, #132721, #119062 ) ) ;
#3152 = DIRECTION ( 'NONE',  ( 1.000000000000000000, 0.000000000000000000, 0.000000000000000000 ) ) ;
#3153 = DIRECTION ( 'NONE',  ( -0.7071067811865486830, -0.7071067811865464625, 0.000000000000000000 ) ) ;
#3154 = CARTESIAN_POINT ( 'NONE',  ( -21.48921356237309155, -27.52281430457070499, 5.000000000000000000 ) ) ;
#3156 = ORIENTED_EDGE ( 'NONE', *, *, #1709, .T. ) ;
#3155 = DIRECTION ( 'NONE',  ( 0.7071067811865487940, -0.7071067811865463515, 0.000000000000000000 ) ) ;
#3157 = VERTEX_POINT ( 'NONE', #53163 ) ;
#3158 = DIRECTION ( 'NONE',  ( 0.7071067811865486830, -0.7071067811865464625, -0.000000000000000000 ) ) ;
#3159 = DIRECTION ( 'NONE',  ( 1.000000000000000000, 0.000000000000000000, 0.000000000000000000 ) ) ;
#3160 = CONICAL_SURFACE ( 'NONE', #86601, 2.500000000000000888, 0.9599310885968822538 ) ;
#3161 = DIRECTION ( 'NONE',  ( 1.000000000000000000, 0.000000000000000000, 0.000000000000000000 ) ) ;
#3162 = ORIENTED_EDGE ( 'NONE', *, *, #15930, .F. ) ;
#3163 = CARTESIAN_POINT ( 'NONE',  ( 20.87852683662840292, -20.24070752338407075, 7.412974875817742948 ) ) ;
#3164 = DIRECTION ( 'NONE',  ( 0.7071067811865486830, -0.7071067811865464625, -0.000000000000000000 ) ) ;
#3165 = EDGE_CURVE ( 'NONE', #134283, #95889, #109703, .T. ) ;
#3166 = AXIS2_PLACEMENT_3D ( 'NONE', #120457, #31364, #65444 ) ;
#3167 = CARTESIAN_POINT ( 'NONE',  ( -29.99999999999979039, -6.412538124160687580, 4.000000000000000000 ) ) ;
#3168 = CARTESIAN_POINT ( 'NONE',  ( 48.48921356237309510, -27.52281430457089328, 5.000000000000000000 ) ) ;
#3169 = ORIENTED_EDGE ( 'NONE', *, *, #56125, .F. ) ;
#3170 = LINE ( 'NONE', #103201, #143489 ) ;
#3171 = CARTESIAN_POINT ( 'NONE',  ( -23.48334561358938899, 22.22500000000000142, 4.500000000000000888 ) ) ;
#3173 = VECTOR ( 'NONE', #18312, 1000.000000000000227 ) ;
#3172 = CARTESIAN_POINT ( 'NONE',  ( 20.60830628287044419, 1.633150327867706864, -6.094999999999981100 ) ) ;
#3175 = ADVANCED_FACE ( 'NONE', ( #66218 ), #121986, .F. ) ;
#3174 = CARTESIAN_POINT ( 'NONE',  ( -5.994519915287488843, 28.92564299267942118, 4.000000000000000000 ) ) ;
#3176 = DIRECTION ( 'NONE',  ( 0.7071067811865487940, 0.7071067811865463515, -0.000000000000000000 ) ) ;
#3177 = ORIENTED_EDGE ( 'NONE', *, *, #116429, .F. ) ;
#3178 = ADVANCED_FACE ( 'NONE', ( #43730 ), #99514, .F. ) ;
#3179 = VERTEX_POINT ( 'NONE', #77112 ) ;
#3180 = DIRECTION ( 'NONE',  ( -1.000000000000000000, -0.000000000000000000, -0.000000000000000000 ) ) ;
#3181 = AXIS2_PLACEMENT_3D ( 'NONE', #78101, #67216, #1898 ) ;
#3182 = CARTESIAN_POINT ( 'NONE',  ( -12.69999999999998153, 0.000000000000000000, 0.000000000000000000 ) ) ;
#3183 =( BOUNDED_CURVE ( )  B_SPLINE_CURVE ( 3, ( #109716, #43750, #21982, #85814 ),
 .UNSPECIFIED., .F., .T. ) 
 B_SPLINE_CURVE_WITH_KNOTS ( ( 4, 4 ),
 ( 2.779374508378132713, 4.199602562396792749 ),
 .UNSPECIFIED. ) 
 CURVE ( )  GEOMETRIC_REPRESENTATION_ITEM ( )  RATIONAL_B_SPLINE_CURVE ( ( 1.000000000000000000, 0.8388583629366723748, 0.8388583629366723748, 1.000000000000000000 ) ) 
 REPRESENTATION_ITEM ( '' )  );
#3184 = AXIS2_PLACEMENT_3D ( 'NONE', #101386, #134032, #2031 ) ;
#3185 = DIRECTION ( 'NONE',  ( -0.000000000000000000, 0.000000000000000000, 1.000000000000000000 ) ) ;
#3186 = LINE ( 'NONE', #91639, #110683 ) ;
#3187 = VECTOR ( 'NONE', #115094, 1000.000000000000000 ) ;
#3188 = DIRECTION ( 'NONE',  ( -0.000000000000000000, 0.3543493200069153248, 0.9351131265310292928 ) ) ;
#3189 = LINE ( 'NONE', #13341, #101572 ) ;
#3190 = FACE_OUTER_BOUND ( 'NONE', #26742, .T. ) ;
#3191 = EDGE_LOOP ( 'NONE', ( #81785, #13339, #15057, #105868 ) ) ;
#3192 = FILL_AREA_STYLE ('',( #26399 ) ) ;
#3193 = CARTESIAN_POINT ( 'NONE',  ( 3.299744871391591339, -27.71228299555208352, 4.000000000000000000 ) ) ;
#3194 = VECTOR ( 'NONE', #44596, 1000.000000000000000 ) ;
#3195 = DIRECTION ( 'NONE',  ( -0.6830127018922180770, -0.6830127018922204085, -0.2588190451025213501 ) ) ;
#3196 = CARTESIAN_POINT ( 'NONE',  ( 55.91209685856478018, 5.291415217122922066, -3.054999999999995275 ) ) ;
#3197 = ADVANCED_FACE ( 'NONE', ( #121288 ), #88688, .T. ) ;
#3198 = FACE_OUTER_BOUND ( 'NONE', #17576, .T. ) ;
#3199 = ORIENTED_EDGE ( 'NONE', *, *, #34344, .T. ) ;
#3200 = CARTESIAN_POINT ( 'NONE',  ( -20.99999999999985079, -18.03360074219755660, 5.000000000000000000 ) ) ;
#3201 = ORIENTED_EDGE ( 'NONE', *, *, #79876, .F. ) ;
#3202 = AXIS2_PLACEMENT_3D ( 'NONE', #95350, #15606, #27230 ) ;
#3203 = FACE_OUTER_BOUND ( 'NONE', #60981, .T. ) ;
#3204 = DIRECTION ( 'NONE',  ( 0.7071067811865487940, -0.7071067811865463515, 0.000000000000000000 ) ) ;
#3205 = CARTESIAN_POINT ( 'NONE',  ( -11.20710678118646797, 15.75929247661555976, 5.000000000000000000 ) ) ;
#3206 = CARTESIAN_POINT ( 'NONE',  ( 24.39999999999999858, -16.48000000000005016, 34.92499999999998295 ) ) ;
#3207 = CARTESIAN_POINT ( 'NONE',  ( -21.18398860626899349, 28.73617430169802134, 5.000000000000000000 ) ) ;
#3208 = CARTESIAN_POINT ( 'NONE',  ( -11.99999999999991473, -0.03360074219773377668, 5.000000000000000000 ) ) ;
#3209 = EDGE_LOOP ( 'NONE', ( #31867, #53769, #7795, #72141 ) ) ;
#3210 = VERTEX_POINT ( 'NONE', #56080 ) ;
#3211 = DIRECTION ( 'NONE',  ( -0.7071067811865486830, -0.7071067811865464625, 0.000000000000000000 ) ) ;
#3212 = PLANE ( 'NONE',  #58477 ) ;
#3213 = CARTESIAN_POINT ( 'NONE',  ( 1.371765549556144048, -8.240707523384196875, 11.38925528200752169 ) ) ;
#3214 = CARTESIAN_POINT ( 'NONE',  ( 117.9583333333333286, 3.974999999999997424, 6.884901960086288852 ) ) ;
#3215 = CARTESIAN_POINT ( 'NONE',  ( 76.49586038379621300, -3.974999999999998312, -6.884901960086286188 ) ) ;
#3216 = PLANE ( 'NONE',  #78724 ) ;
#3217 = EDGE_CURVE ( 'NONE', #3234, #139953, #116694, .T. ) ;
#3218 = VECTOR ( 'NONE', #79720, 1000.000000000000000 ) ;
#3219 = CARTESIAN_POINT ( 'NONE',  ( 69.48921356237309510, -27.52281430457103895, 5.000000000000000000 ) ) ;
#3220 = ORIENTED_EDGE ( 'NONE', *, *, #10733, .T. ) ;
#3221 = CARTESIAN_POINT ( 'NONE',  ( 63.27083333333332860, -7.949999999999999289, -2.130196079827426203 ) ) ;
#3222 = DIRECTION ( 'NONE',  ( 1.000000000000000000, 1.224606353822377258E-16, 0.000000000000000000 ) ) ;
#3223 = EDGE_CURVE ( 'NONE', #134670, #143282, #108231, .T. ) ;
#3224 = DIRECTION ( 'NONE',  ( 0.7071067811865487940, 0.7071067811865463515, 0.000000000000000000 ) ) ;
#3225 = FACE_OUTER_BOUND ( 'NONE', #76005, .T. ) ;
#3226 = ORIENTED_EDGE ( 'NONE', *, *, #79951, .T. ) ;
#3227 = EDGE_CURVE ( 'NONE', #53161, #86656, #8895, .T. ) ;
#3228 = ADVANCED_FACE ( 'NONE', ( #20523 ), #64782, .F. ) ;
#3229 = VECTOR ( 'NONE', #53043, 1000.000000000000000 ) ;
#3230 = LINE ( 'NONE', #57660, #83808 ) ;
#3231 = DIRECTION ( 'NONE',  ( -0.000000000000000000, 0.000000000000000000, 1.000000000000000000 ) ) ;
#3232 = CARTESIAN_POINT ( 'NONE',  ( 64.60459685856477563, 1.637169565754164946, -6.109999999999999432 ) ) ;
#3233 = LINE ( 'NONE', #102586, #32160 ) ;
#3234 = VERTEX_POINT ( 'NONE', #142352 ) ;
#3235 = VERTEX_POINT ( 'NONE', #68382 ) ;
#3236 = DIRECTION ( 'NONE',  ( -0.7071067811865486830, 0.7071067811865464625, 0.000000000000000000 ) ) ;
#3237 = DIRECTION ( 'NONE',  ( 0.6830127018922180770, -0.6830127018922204085, -0.2588190451025213501 ) ) ;
#3238 = EDGE_CURVE ( 'NONE', #120537, #2401, #79273, .T. ) ;
#3239 = DIRECTION ( 'NONE',  ( 0.000000000000000000, -1.000000000000000000, 0.000000000000000000 ) ) ;
#3240 = EDGE_CURVE ( 'NONE', #23652, #32623, #78510, .T. ) ;
#3241 = CARTESIAN_POINT ( 'NONE',  ( 15.65467068707222076, 3.821174125832445049E-16, 0.000000000000000000 ) ) ;
#3243 = VERTEX_POINT ( 'NONE', #24834 ) ;
#3242 = DIRECTION ( 'NONE',  ( -1.000000000000000000, -0.000000000000000000, -0.000000000000000000 ) ) ;
#3244 = CARTESIAN_POINT ( 'NONE',  ( 16.49999999999988276, 22.22500000000000142, 4.362957392718795901 ) ) ;
#3245 = FACE_OUTER_BOUND ( 'NONE', #85822, .T. ) ;
#3246 = DIRECTION ( 'NONE',  ( 0.000000000000000000, 0.000000000000000000, -1.000000000000000000 ) ) ;
#3247 = VECTOR ( 'NONE', #43984, 1000.000000000000000 ) ;
#3248 = DIRECTION ( 'NONE',  ( -1.000000000000000000, 1.451651444332056451E-15, 0.000000000000000000 ) ) ;
#3249 = VERTEX_POINT ( 'NONE', #13221 ) ;
#3250 = EDGE_CURVE ( 'NONE', #59344, #57263, #10207, .T. ) ;
#3251 = VERTEX_POINT ( 'NONE', #124863 ) ;
#3252 = VECTOR ( 'NONE', #101289, 1000.000000000000227 ) ;
#3253 = EDGE_LOOP ( 'NONE', ( #29575, #123693, #89337 ) ) ;
#3254 = LINE ( 'NONE', #114853, #52206 ) ;
#3255 = LINE ( 'NONE', #124340, #36458 ) ;
#3256 = LINE ( 'NONE', #11260, #31794 ) ;
#3257 = CARTESIAN_POINT ( 'NONE',  ( 8.897059064271770623, 2.055000000000001048, 2.516649172247811554E-16 ) ) ;
#3258 = CARTESIAN_POINT ( 'NONE',  ( 16.49999999999988276, -12.66682484999664737, -0.6294897503863559063 ) ) ;
#3259 = VERTEX_POINT ( 'NONE', #36434 ) ;
#3261 = EDGE_CURVE ( 'NONE', #110799, #32452, #4435, .T. ) ;
#3260 = ORIENTED_EDGE ( 'NONE', *, *, #43213, .T. ) ;
#3262 = DIRECTION ( 'NONE',  ( 0.6830127018922180770, -0.6830127018922204085, -0.2588190451025213501 ) ) ;
#3263 = CARTESIAN_POINT ( 'NONE',  ( -16.45742106731621845, 0.9613713492673543470, -33.49048331797055766 ) ) ;
#3264 = ORIENTED_EDGE ( 'NONE', *, *, #77395, .F. ) ;
#3265 = AXIS2_PLACEMENT_3D ( 'NONE', #68836, #122454, #44969 ) ;
#3266 = ORIENTED_EDGE ( 'NONE', *, *, #70615, .F. ) ;
#3267 = DIRECTION ( 'NONE',  ( 0.3543493200069162685, -0.000000000000000000, -0.9351131265310288487 ) ) ;
#3268 = EDGE_CURVE ( 'NONE', #72134, #23963, #48043, .T. ) ;
#3269 = CARTESIAN_POINT ( 'NONE',  ( 25.49999999999983658, -5.947814304570765209, 5.000000000000000000 ) ) ;
#3270 = ORIENTED_EDGE ( 'NONE', *, *, #30413, .F. ) ;
#3271 = VECTOR ( 'NONE', #122625, 1000.000000000000000 ) ;
#3272 = FACE_BOUND ( 'NONE', #53399, .T. ) ;
#3273 = LINE ( 'NONE', #69280, #13162 ) ;
#3274 = DIRECTION ( 'NONE',  ( -0.000000000000000000, 0.000000000000000000, 1.000000000000000000 ) ) ;
#3275 = FACE_OUTER_BOUND ( 'NONE', #110605, .T. ) ;
#3276 = EDGE_CURVE ( 'NONE', #6439, #25909, #5535, .T. ) ;
#3277 = PLANE ( 'NONE',  #108171 ) ;
#3278 =( LENGTH_UNIT ( ) NAMED_UNIT ( * ) SI_UNIT ( .MILLI., .METRE. ) );
#3280 = ADVANCED_FACE ( 'NONE', ( #59640 ), #67673, .T. ) ;
#3279 =( LENGTH_UNIT ( ) NAMED_UNIT ( * ) SI_UNIT ( .MILLI., .METRE. ) );
#3281 = VERTEX_POINT ( 'NONE', #92216 ) ;
#3282 = AXIS2_PLACEMENT_3D ( 'NONE', #1008, #45290, #89464 ) ;
#3283 = VERTEX_POINT ( 'NONE', #13936 ) ;
#3284 = CARTESIAN_POINT ( 'NONE',  ( 106.6620968585647802, -5.291415217122919401, 3.054999999999997939 ) ) ;
#3285 = EDGE_LOOP ( 'NONE', ( #15701, #137223, #112251, #40560 ) ) ;
#3286 = DIRECTION ( 'NONE',  ( -0.7071067811865486830, 0.7071067811865464625, 0.000000000000000000 ) ) ;
#3287 = ORIENTED_EDGE ( 'NONE', *, *, #137131, .F. ) ;
#3288 = DIRECTION ( 'NONE',  ( 0.6830127018922180770, -0.6830127018922204085, -0.2588190451025213501 ) ) ;
#3289 = CARTESIAN_POINT ( 'NONE',  ( -24.48921356237309510, -27.52281430457072631, 5.000000000000000000 ) ) ;
#3290 = FACE_OUTER_BOUND ( 'NONE', #61967, .T. ) ;
#3291 = ORIENTED_EDGE ( 'NONE', *, *, #108340, .T. ) ;
#3292 = FACE_OUTER_BOUND ( 'NONE', #19326, .T. ) ;
#3293 = AXIS2_PLACEMENT_3D ( 'NONE', #63467, #17073, #117074 ) ;
#3294 = DIRECTION ( 'NONE',  ( -1.000000000000000000, -1.224606353822377258E-16, -0.000000000000000000 ) ) ;
#3295 = EDGE_CURVE ( 'NONE', #119191, #73062, #101674, .T. ) ;
#3296 = DIRECTION ( 'NONE',  ( 0.3543493200069162685, -0.000000000000000000, -0.9351131265310288487 ) ) ;
#3297 = DIRECTION ( 'NONE',  ( -0.7071067811865486830, -0.7071067811865464625, 0.000000000000000000 ) ) ;
#3298 = DIRECTION ( 'NONE',  ( -0.000000000000000000, -0.3543493200069152693, 0.9351131265310292928 ) ) ;
#3299 = ORIENTED_EDGE ( 'NONE', *, *, #7862, .T. ) ;
#3300 = LINE ( 'NONE', #93892, #79047 ) ;
#3301 = ORIENTED_EDGE ( 'NONE', *, *, #50801, .F. ) ;
#3302 = ORIENTED_EDGE ( 'NONE', *, *, #33053, .T. ) ;
#3303 = EDGE_CURVE ( 'NONE', #85379, #44481, #134328, .T. ) ;
#3304 = VERTEX_POINT ( 'NONE', #2334 ) ;
#3305 = CARTESIAN_POINT ( 'NONE',  ( 50.31293019189809712, -1.637169565754159617, -6.110000000000001208 ) ) ;
#3306 = ORIENTED_EDGE ( 'NONE', *, *, #28430, .F. ) ;
#3307 = CARTESIAN_POINT ( 'NONE',  ( 2.087472949537105826, -6.094999999999989981, 3.732111120401553285E-16 ) ) ;
#3308 = DIRECTION ( 'NONE',  ( -0.7071067811865486830, -0.7071067811865464625, -0.000000000000000000 ) ) ;
#3309 = EDGE_LOOP ( 'NONE', ( #37255, #9683, #53883, #38811, #9565 ) ) ;
#3310 = DIRECTION ( 'NONE',  ( 0.7071067811865486830, -0.7071067811865464625, -0.000000000000000000 ) ) ;
#3311 = VERTEX_POINT ( 'NONE', #35029 ) ;
#3312 = CARTESIAN_POINT ( 'NONE',  ( -7.940000000000001279, -33.26999999999999602, -8.101350000000008933 ) ) ;
#3313 = ADVANCED_FACE ( 'NONE', ( #114685 ), #48748, .F. ) ;
#3315 = ORIENTED_EDGE ( 'NONE', *, *, #23637, .F. ) ;
#3314 = DIRECTION ( 'NONE',  ( -0.6830127018922180770, -0.6830127018922204085, -0.2588190451025213501 ) ) ;
#3316 = ORIENTED_EDGE ( 'NONE', *, *, #62044, .F. ) ;
#3317 = VECTOR ( 'NONE', #14555, 999.9999999999998863 ) ;
#3318 = CARTESIAN_POINT ( 'NONE',  ( -45.18398860626900415, 28.73617430169818832, 5.000000000000000000 ) ) ;
#3319 = CARTESIAN_POINT ( 'NONE',  ( -14.99999999999988454, -13.44781430457069149, 5.000000000000000000 ) ) ;
#3320 = CARTESIAN_POINT ( 'NONE',  ( 128.5370968585647802, -3.054999999999999272, -5.291415217122919401 ) ) ;
#3321 = VERTEX_POINT ( 'NONE', #47369 ) ;
#3322 = PLANE ( 'NONE',  #115201 ) ;
#3324 = ORIENTED_EDGE ( 'NONE', *, *, #105654, .T. ) ;
#3323 = EDGE_CURVE ( 'NONE', #119026, #83338, #100961, .T. ) ;
#3325 = ORIENTED_EDGE ( 'NONE', *, *, #89367, .F. ) ;
#3326 = VERTEX_POINT ( 'NONE', #112561 ) ;
#3327 = CARTESIAN_POINT ( 'NONE',  ( -33.29974487139158867, -27.71228299555229313, 4.000000000000000000 ) ) ;
#3328 =( NAMED_UNIT ( * ) SI_UNIT ( $, .STERADIAN. ) SOLID_ANGLE_UNIT ( ) );
#3330 = EDGE_CURVE ( 'NONE', #106116, #36944, #91535, .T. ) ;
#3329 = PLANE ( 'NONE',  #60984 ) ;
#3331 = DIRECTION ( 'NONE',  ( -0.7071067811865486830, -0.7071067811865464625, -0.000000000000000000 ) ) ;
#3332 = EDGE_CURVE ( 'NONE', #118907, #89121, #69079, .T. ) ;
#3333 = CARTESIAN_POINT ( 'NONE',  ( -36.48921356237310221, -27.52281430457080802, 5.000000000000000000 ) ) ;
#3334 = VERTEX_POINT ( 'NONE', #46650 ) ;
#3335 = VECTOR ( 'NONE', #37942, 999.9999999999998863 ) ;
#3336 = CARTESIAN_POINT ( 'NONE',  ( -28.17183060077627133, -11.24070752338416845, 4.000000000000000000 ) ) ;
#3337 = AXIS2_PLACEMENT_3D ( 'NONE', #100074, #32687, #98623 ) ;
#3338 = CARTESIAN_POINT ( 'NONE',  ( 26.66623647476855652, 7.934999999999990727, -1.457635852685135314E-15 ) ) ;
#3339 = CARTESIAN_POINT ( 'NONE',  ( 32.84387692260735747, -22.22499999999999787, 4.000000000000000000 ) ) ;
#3340 = DIRECTION ( 'NONE',  ( -0.000000000000000000, -0.3543493200069153248, -0.9351131265310291818 ) ) ;
#3341 = EDGE_CURVE ( 'NONE', #71785, #109962, #90838, .T. ) ;
#3342 = DIRECTION ( 'NONE',  ( 0.5735764363510444941, 0.8191520442889929088, 0.000000000000000000 ) ) ;
#3343 = ORIENTED_EDGE ( 'NONE', *, *, #80401, .F. ) ;
#3344 = AXIS2_PLACEMENT_3D ( 'NONE', #59086, #82942, #15493 ) ;
#3345 = ORIENTED_EDGE ( 'NONE', *, *, #65365, .T. ) ;
#3346 = ORIENTED_EDGE ( 'NONE', *, *, #120387, .T. ) ;
#3347 = CARTESIAN_POINT ( 'NONE',  ( 26.12840764549667583, 9.139736423841732040E-16, 0.000000000000000000 ) ) ;
#3348 = CARTESIAN_POINT ( 'NONE',  ( 62.99451991528749772, 28.92564299267982264, 4.000000000000000000 ) ) ;
#3349 = DIRECTION ( 'NONE',  ( -0.7071067811865486830, 0.7071067811865464625, 0.000000000000000000 ) ) ;
#3350 = FACE_OUTER_BOUND ( 'NONE', #104036, .T. ) ;
#3351 = DIRECTION ( 'NONE',  ( 0.3543493200069162685, -0.000000000000000000, -0.9351131265310288487 ) ) ;
#3352 = EDGE_CURVE ( 'NONE', #131899, #4118, #114417, .T. ) ;
#3353 = CARTESIAN_POINT ( 'NONE',  ( 27.53159235450332076, -2.500000000000000000, 3.061616997868384127E-16 ) ) ;
#3354 = MECHANICAL_DESIGN_GEOMETRIC_PRESENTATION_REPRESENTATION (  '', ( #65920 ), #119170 ) ;
#3355 = CARTESIAN_POINT ( 'NONE',  ( -25.39999999999996305, 0.000000000000000000, 0.000000000000000000 ) ) ;
#3356 = CARTESIAN_POINT ( 'NONE',  ( 23.63159235450331863, -7.703719777548943412E-31, 2.500000000000001332 ) ) ;
#3357 = LINE ( 'NONE', #102708, #18824 ) ;
#3358 = DIRECTION ( 'NONE',  ( 0.6830127018922180770, -0.6830127018922204085, -0.2588190451025213501 ) ) ;
#3359 = ORIENTED_EDGE ( 'NONE', *, *, #79397, .T. ) ;
#3360 = ORIENTED_EDGE ( 'NONE', *, *, #73043, .F. ) ;
#3361 = DIRECTION ( 'NONE',  ( 0.7071067811865486830, -0.7071067811865464625, -0.000000000000000000 ) ) ;
#3363 = ORIENTED_EDGE ( 'NONE', *, *, #120365, .F. ) ;
#3362 = DIRECTION ( 'NONE',  ( 1.400468248933915008E-15, 0.9647414015272156584, -0.2631995976047526442 ) ) ;
#3364 = DIRECTION ( 'NONE',  ( 0.000000000000000000, 0.000000000000000000, 1.000000000000000000 ) ) ;
#3365 = PLANE ( 'NONE',  #28683 ) ;
#3366 = VERTEX_POINT ( 'NONE', #81398 ) ;
#3367 = LINE ( 'NONE', #25860, #53152 ) ;
#3368 = ORIENTED_EDGE ( 'NONE', *, *, #62813, .F. ) ;
#3369 = SURFACE_STYLE_FILL_AREA ( #102724 ) ;
#3370 = EDGE_LOOP ( 'NONE', ( #40981, #44896, #79051, #110407 ) ) ;
#3371 = VECTOR ( 'NONE', #46007, 1000.000000000000227 ) ;
#3372 = LINE ( 'NONE', #36736, #112148 ) ;
#3373 = CARTESIAN_POINT ( 'NONE',  ( 106.6833603837962272, -2.130196079827426203, 7.949999999999997513 ) ) ;
#3375 = VECTOR ( 'NONE', #70458, 1000.000000000000000 ) ;
#3374 = CARTESIAN_POINT ( 'NONE',  ( -24.18398860626899705, 28.73617430169804265, 5.000000000000000000 ) ) ;
#3377 = EDGE_CURVE ( 'NONE', #107847, #20599, #26278, .T. ) ;
#3376 = AXIS2_PLACEMENT_3D ( 'NONE', #23881, #68146, #12973 ) ;
#3378 = VERTEX_POINT ( 'NONE', #63222 ) ;
#3379 = DIRECTION ( 'NONE',  ( -0.7071067811865487940, 0.7071067811865463515, 0.000000000000000000 ) ) ;
#3381 = ADVANCED_FACE ( 'NONE', ( #116120 ), #29819, .F. ) ;
#3380 = FACE_OUTER_BOUND ( 'NONE', #130926, .T. ) ;
#3382 = CARTESIAN_POINT ( 'NONE',  ( 17.81601139373099940, 28.73617430169775133, 5.000000000000000000 ) ) ;
#3383 = CARTESIAN_POINT ( 'NONE',  ( 19.25000000000000355, -7.464222240803106570E-16, -6.094999999999989981 ) ) ;
#3384 = CARTESIAN_POINT ( 'NONE',  ( 34.24999999999998579, -9.735942053221458872E-16, 7.950000000000000178 ) ) ;
#3385 = DIRECTION ( 'NONE',  ( -1.000000000000000000, -0.000000000000000000, -0.000000000000000000 ) ) ;
#3386 = FACE_OUTER_BOUND ( 'NONE', #133859, .T. ) ;
#3387 = VERTEX_POINT ( 'NONE', #138612 ) ;
#3388 = ADVANCED_FACE ( 'NONE', ( #107389 ), #16822, .F. ) ;
#3389 = EDGE_CURVE ( 'NONE', #65237, #14379, #8056, .T. ) ;
#3390 = DIRECTION ( 'NONE',  ( -0.6830127018922180770, -0.6830127018922204085, -0.2588190451025213501 ) ) ;
#3391 = EDGE_LOOP ( 'NONE', ( #34059, #68348, #105271, #88265 ) ) ;
#3392 = CARTESIAN_POINT ( 'NONE',  ( 96.10459685856477563, 1.637169565754164946, -6.109999999999999432 ) ) ;
#3393 = DIRECTION ( 'NONE',  ( 0.7071067811865486830, -0.7071067811865464625, -0.000000000000000000 ) ) ;
#3394 = CARTESIAN_POINT ( 'NONE',  ( 9.299744871391588674, -27.71228299555212971, 4.000000000000000000 ) ) ;
#3395 = DIRECTION ( 'NONE',  ( 0.6830127018922181881, 0.6830127018922202975, -0.2588190451025214056 ) ) ;
#3396 = CARTESIAN_POINT ( 'NONE',  ( 17.84878961325748037, 0.000000000000000000, 2.500000000000000444 ) ) ;
#3397 = ORIENTED_EDGE ( 'NONE', *, *, #39565, .F. ) ;
#3398 = EDGE_CURVE ( 'NONE', #23744, #75950, #70501, .T. ) ;
#3399 = DIRECTION ( 'NONE',  ( -0.7071067811865487940, 0.7071067811865463515, -0.000000000000000000 ) ) ;
#3400 = ADVANCED_FACE ( 'NONE', ( #105939 ), #5199, .F. ) ;
#3401 = EDGE_LOOP ( 'NONE', ( #15786, #93571, #6767, #130445, #60464 ) ) ;
#3402 = CARTESIAN_POINT ( 'NONE',  ( -24.20969143188526118, 6.176090689687629975, 5.000000000000000000 ) ) ;
#3403 = EDGE_CURVE ( 'NONE', #19559, #24434, #106655, .T. ) ;
#3404 = DIRECTION ( 'NONE',  ( 0.7071067811865486830, -0.7071067811865464625, -0.000000000000000000 ) ) ;
#3406 = VERTEX_POINT ( 'NONE', #105253 ) ;
#3405 = LINE ( 'NONE', #104136, #142364 ) ;
#3407 = CARTESIAN_POINT ( 'NONE',  ( -4.499999999999976019, 19.08746187583905751, 4.000000000000000000 ) ) ;
#3408 = CARTESIAN_POINT ( 'NONE',  ( -77.99451991528749772, 28.92564299267992567, 4.000000000000000000 ) ) ;
#3409 = CARTESIAN_POINT ( 'NONE',  ( 24.18398860626899705, 28.73617430169804265, 5.000000000000000000 ) ) ;
#3410 = CYLINDRICAL_SURFACE ( 'NONE', #2964, 7.950000000000000178 ) ;
#3411 = ORIENTED_EDGE ( 'NONE', *, *, #12605, .T. ) ;
#3412 = VERTEX_POINT ( 'NONE', #49490 ) ;
#3413 = ORIENTED_EDGE ( 'NONE', *, *, #73334, .T. ) ;
#3415 = EDGE_CURVE ( 'NONE', #56310, #98903, #40039, .T. ) ;
#3414 = CARTESIAN_POINT ( 'NONE',  ( 81.52126352523141861, -4.472830434245839371, -4.472830434245840259 ) ) ;
#3416 = ORIENTED_EDGE ( 'NONE', *, *, #23398, .T. ) ;
#3417 = ADVANCED_FACE ( 'NONE', ( #84929 ), #71949, .T. ) ;
#3418 = DIRECTION ( 'NONE',  ( 0.7071067811865487940, 0.7071067811865463515, 0.000000000000000000 ) ) ;
#3419 = CARTESIAN_POINT ( 'NONE',  ( -16.49999999999988987, 11.52377502935401843, -1.522421517564045867 ) ) ;
#3420 = CARTESIAN_POINT ( 'NONE',  ( -4.499999999999966249, 1.466399257802248446, 5.000000000000000000 ) ) ;
#3421 = DIRECTION ( 'NONE',  ( 0.000000000000000000, -0.2631995976047557528, -0.9647414015272147703 ) ) ;
#3422 = ORIENTED_EDGE ( 'NONE', *, *, #127631, .T. ) ;
#3423 = EDGE_CURVE ( 'NONE', #14564, #105099, #61775, .T. ) ;
#3424 = DIRECTION ( 'NONE',  ( 0.3543493200069163240, 0.000000000000000000, -0.9351131265310288487 ) ) ;
#3426 = CONICAL_SURFACE ( 'NONE', #107545, 2.500000000000000444, 0.9599310885968830309 ) ;
#3425 = DIRECTION ( 'NONE',  ( -0.7071067811865487940, 0.7071067811865463515, -0.000000000000000000 ) ) ;
#3427 = CARTESIAN_POINT ( 'NONE',  ( 51.29974487139158867, -27.71228299555242103, 4.000000000000000000 ) ) ;
#3428 = CARTESIAN_POINT ( 'NONE',  ( 80.41209685856479439, 5.291415217122921177, -3.054999999999994831 ) ) ;
#3429 = ORIENTED_EDGE ( 'NONE', *, *, #14355, .F. ) ;
#3430 = LINE ( 'NONE', #47722, #62824 ) ;
#3431 = CARTESIAN_POINT ( 'NONE',  ( 21.66240673564756491, 0.000000000000000000, 2.337593264352432421 ) ) ;
#3432 = EDGE_CURVE ( 'NONE', #99331, #81879, #82118, .T. ) ;
#3433 = DIRECTION ( 'NONE',  ( -1.000000000000000000, -0.000000000000000000, -0.000000000000000000 ) ) ;
#3434 = ORIENTED_EDGE ( 'NONE', *, *, #32196, .T. ) ;
#3435 = ORIENTED_EDGE ( 'NONE', *, *, #72183, .F. ) ;
#3436 = FACE_OUTER_BOUND ( 'NONE', #117001, .T. ) ;
#3437 = CARTESIAN_POINT ( 'NONE',  ( 27.99999999999999645, 9.521314400968980422E-16, 0.000000000000000000 ) ) ;
#3438 = DIRECTION ( 'NONE',  ( 1.734723475976806848E-16, -1.000000000000000000, 0.000000000000000000 ) ) ;
#3439 = EDGE_CURVE ( 'NONE', #19849, #29105, #115372, .T. ) ;
#3440 = CARTESIAN_POINT ( 'NONE',  ( 55.56056557994604361, -49.14999999999999147, -39.86617647058817937 ) ) ;
#3441 = DIRECTION ( 'NONE',  ( -0.6830127018922181881, 0.6830127018922202975, -0.2588190451025214056 ) ) ;
#3442 = DIRECTION ( 'NONE',  ( -0.000000000000000000, 0.000000000000000000, 1.000000000000000000 ) ) ;
#3443 = EDGE_CURVE ( 'NONE', #32886, #37230, #118247, .T. ) ;
#3444 = VECTOR ( 'NONE', #8543, 1000.000000000000000 ) ;
#3445 = VERTEX_POINT ( 'NONE', #50176 ) ;
#3446 = ORIENTED_EDGE ( 'NONE', *, *, #77637, .T. ) ;
#3447 =( GEOMETRIC_REPRESENTATION_CONTEXT ( 3 ) GLOBAL_UNCERTAINTY_ASSIGNED_CONTEXT ( ( #46051 ) ) GLOBAL_UNIT_ASSIGNED_CONTEXT ( ( #123452, #36410, #103772 ) ) REPRESENTATION_CONTEXT ( 'NONE', 'WORKASPACE' ) );
#3448 = CARTESIAN_POINT ( 'NONE',  ( 15.96626304157554266, -2.055000000000000160, 0.000000000000000000 ) ) ;
#3449 = EDGE_LOOP ( 'NONE', ( #140842, #77799, #55185, #4550 ) ) ;
#3450 = ADVANCED_FACE ( 'NONE', ( #71224 ), #7345, .F. ) ;
#3451 = PLANE ( 'NONE',  #98318 ) ;
#3452 = ORIENTED_EDGE ( 'NONE', *, *, #63708, .F. ) ;
#3453 = AXIS2_PLACEMENT_3D ( 'NONE', #45683, #34788, #79030 ) ;
#3454 = PLANE ( 'NONE',  #1977 ) ;
#3455 = PLANE ( 'NONE',  #58782 ) ;
#3456 = DIRECTION ( 'NONE',  ( 0.7071067811865487940, 0.7071067811865463515, -0.000000000000000000 ) ) ;
#3457 = FACE_OUTER_BOUND ( 'NONE', #6258, .T. ) ;
#3458 = CARTESIAN_POINT ( 'NONE',  ( -17.91685193227058548, 21.75929247661549937, 7.311836541448010429 ) ) ;
#3459 = EDGE_LOOP ( 'NONE', ( #108872, #49988, #138653, #129754 ) ) ;
#3460 = CARTESIAN_POINT ( 'NONE',  ( -0.005480084712502889671, 28.92564299267938210, 4.000000000000000000 ) ) ;
#3461 = CARTESIAN_POINT ( 'NONE',  ( -19.56363873141800980, -2.772201803466310288, 4.368625942145798469 ) ) ;
#3462 = ORIENTED_EDGE ( 'NONE', *, *, #83965, .F. ) ;
#3463 = DIRECTION ( 'NONE',  ( -0.000000000000000000, 0.3543493200069153248, 0.9351131265310292928 ) ) ;
#3464 = ORIENTED_EDGE ( 'NONE', *, *, #76577, .F. ) ;
#3465 = ORIENTED_EDGE ( 'NONE', *, *, #56811, .F. ) ;
#3466 = CARTESIAN_POINT ( 'NONE',  ( 29.99999999999979750, -2.904428200921286951, -6.989807076075011061 ) ) ;
#3467 = VERTEX_POINT ( 'NONE', #82810 ) ;
#3468 = EDGE_LOOP ( 'NONE', ( #62085, #26825, #34398, #39101 ) ) ;
#3469 = LINE ( 'NONE', #33486, #44141 ) ;
#3470 = ORIENTED_EDGE ( 'NONE', *, *, #42064, .T. ) ;
#3471 = VECTOR ( 'NONE', #112670, 1000.000000000000227 ) ;
#3472 = DIRECTION ( 'NONE',  ( 0.7071067811865486830, -0.7071067811865464625, -0.000000000000000000 ) ) ;
#3473 = VECTOR ( 'NONE', #34375, 999.9999999999998863 ) ;
#3474 = VECTOR ( 'NONE', #83611, 1000.000000000000227 ) ;
#3475 = CARTESIAN_POINT ( 'NONE',  ( -10.49999999999991829, -20.94781430457062044, 5.000000000000000000 ) ) ;
#3476 = CARTESIAN_POINT ( 'NONE',  ( 114.6254301918981042, 5.291415217122919401, 3.055000000000002824 ) ) ;
#3477 = FACE_OUTER_BOUND ( 'NONE', #30187, .T. ) ;
#3478 = AXIS2_PLACEMENT_3D ( 'NONE', #121133, #1473, #66077 ) ;
#3479 = EDGE_CURVE ( 'NONE', #97811, #21679, #139349, .T. ) ;
#3480 = FACE_OUTER_BOUND ( 'NONE', #127983, .T. ) ;
#3481 = DIRECTION ( 'NONE',  ( 2.110369192185896011E-16, -1.000000000000000000, 0.000000000000000000 ) ) ;
#3482 = DIRECTION ( 'NONE',  ( -0.7071067811865486830, -0.7071067811865464625, 0.000000000000000000 ) ) ;
#3483 = ORIENTED_EDGE ( 'NONE', *, *, #35043, .T. ) ;
#3484 = DIRECTION ( 'NONE',  ( -0.000000000000000000, 0.3543493200069153248, 0.9351131265310292928 ) ) ;
#3485 = PLANE ( 'NONE',  #93937 ) ;
#3486 = ORIENTED_EDGE ( 'NONE', *, *, #135795, .F. ) ;
#3487 = ORIENTED_EDGE ( 'NONE', *, *, #113439, .F. ) ;
#3488 = LINE ( 'NONE', #48453, #81988 ) ;
#3489 = EDGE_LOOP ( 'NONE', ( #43019, #127312, #43723, #106970 ) ) ;
#3490 = PLANE ( 'NONE',  #132482 ) ;
#3491 = DIRECTION ( 'NONE',  ( -1.000000000000000000, -1.224606353822377258E-16, -0.000000000000000000 ) ) ;
#3492 = ADVANCED_FACE ( 'NONE', ( #40723 ), #74057, .F. ) ;
#3493 = DIRECTION ( 'NONE',  ( -0.7071067811865486830, -0.7071067811865464625, 0.000000000000000000 ) ) ;
#3494 = LINE ( 'NONE', #115099, #44047 ) ;
#3495 = ORIENTED_EDGE ( 'NONE', *, *, #11216, .F. ) ;
#3496 = DIRECTION ( 'NONE',  ( 0.6830127018922180770, -0.6830127018922204085, -0.2588190451025213501 ) ) ;
#3497 = ORIENTED_EDGE ( 'NONE', *, *, #39825, .F. ) ;
#3499 = ADVANCED_FACE ( 'NONE', ( #87075 ), #31975, .F. ) ;
#3498 = DIRECTION ( 'NONE',  ( 0.7071067811865487940, -0.7071067811865463515, 0.000000000000000000 ) ) ;
#3500 = EDGE_CURVE ( 'NONE', #2711, #70215, #65355, .T. ) ;
#3501 = CARTESIAN_POINT ( 'NONE',  ( 25.44206980810188412, 7.934999999999993392, 2.126176841940951689 ) ) ;
#3502 = VERTEX_POINT ( 'NONE', #131289 ) ;
#3503 = LINE ( 'NONE', #47794, #110755 ) ;
#3504 = ADVANCED_FACE ( 'NONE', ( #96478 ), #108069, .T. ) ;
#3505 = CARTESIAN_POINT ( 'NONE',  ( -48.18398860626899705, 28.73617430169820608, 5.000000000000000000 ) ) ;
#3506 = ORIENTED_EDGE ( 'NONE', *, *, #23127, .T. ) ;
#3507 = EDGE_LOOP ( 'NONE', ( #107110, #73999, #127133, #68209 ) ) ;
#3508 = ORIENTED_EDGE ( 'NONE', *, *, #124080, .T. ) ;
#3509 = DIRECTION ( 'NONE',  ( -0.5735764363510503783, -0.8191520442889886899, 0.000000000000000000 ) ) ;
#3510 = CARTESIAN_POINT ( 'NONE',  ( 12.69999999999999574, -34.65000000000001279, 17.49210858042622618 ) ) ;
#3511 = DIRECTION ( 'NONE',  ( -0.7071067811865487940, 0.7071067811865463515, -0.000000000000000000 ) ) ;
#3512 = CARTESIAN_POINT ( 'NONE',  ( -45.48921356237309510, -27.52281430457087197, 5.000000000000000000 ) ) ;
#3513 = VERTEX_POINT ( 'NONE', #142189 ) ;
#3514 = LINE ( 'NONE', #135509, #16072 ) ;
#3515 = FACE_OUTER_BOUND ( 'NONE', #90201, .T. ) ;
#3516 = EDGE_CURVE ( 'NONE', #482, #51950, #64606, .T. ) ;
#3517 = CARTESIAN_POINT ( 'NONE',  ( -3.183988606268992161, 28.73617430169789699, 5.000000000000000000 ) ) ;
#3518 = CARTESIAN_POINT ( 'NONE',  ( 25.49999999999982236, -20.53675388469228125, 2.352720554255952834 ) ) ;
#3519 = ORIENTED_EDGE ( 'NONE', *, *, #112688, .T. ) ;
#3520 = EDGE_CURVE ( 'NONE', #99874, #72219, #8738, .T. ) ;
#3521 = DIRECTION ( 'NONE',  ( -1.000000000000000000, 0.000000000000000000, 0.000000000000000000 ) ) ;
#3522 = ORIENTED_EDGE ( 'NONE', *, *, #74489, .T. ) ;
#3523 = VERTEX_POINT ( 'NONE', #121117 ) ;
#3524 = ORIENTED_EDGE ( 'NONE', *, *, #102074, .T. ) ;
#3525 = PLANE ( 'NONE',  #63265 ) ;
#3526 = CARTESIAN_POINT ( 'NONE',  ( 104.6875000000000000, -5.819803920172573974, 5.819803920172573086 ) ) ;
#3527 = ADVANCED_FACE ( 'NONE', ( #63906 ), #108781, .F. ) ;
#3528 = ORIENTED_EDGE ( 'NONE', *, *, #10192, .T. ) ;
#3530 = ADVANCED_FACE ( 'NONE', ( #9474 ), #88517, .F. ) ;
#3529 =( NAMED_UNIT ( * ) PLANE_ANGLE_UNIT ( ) SI_UNIT ( $, .RADIAN. ) );
#3531 = VERTEX_POINT ( 'NONE', #10209 ) ;
#3532 = LINE ( 'NONE', #60114, #123960 ) ;
#3533 = DIRECTION ( 'NONE',  ( 0.7071067811865486830, 0.7071067811865464625, 0.000000000000000000 ) ) ;
#3534 = VECTOR ( 'NONE', #89551, 1000.000000000000000 ) ;
#3535 = CARTESIAN_POINT ( 'NONE',  ( 30.82876352523145158, 0.000000000000000000, -6.109999999999999432 ) ) ;
#3536 = DIRECTION ( 'NONE',  ( -0.000000000000000000, -0.3543493200069152693, 0.9351131265310292928 ) ) ;
#3537 =( BOUNDED_CURVE ( )  B_SPLINE_CURVE ( 2, ( #138028, #61913, #72821, #114807, #71352, #93800, #25682, #126417, #59081, #4581, #92352, #27829, #94498 ),
 .UNSPECIFIED., .F., .T. ) 
 B_SPLINE_CURVE_WITH_KNOTS ( ( 3, 2, 2, 2, 2, 2, 3 ),
 ( 0.3000000000000000444, 0.3083333333333334036, 0.3166666666666667074, 0.3250000000000000666, 0.3333333333333333703, 0.3416666666666667296, 0.3500000000000000333 ),
 .UNSPECIFIED. ) 
 CURVE ( )  GEOMETRIC_REPRESENTATION_ITEM ( )  RATIONAL_B_SPLINE_CURVE ( ( 0.9999999999999997780, 0.9659258262890685343, 1.000000000000000000, 0.9659258262890683122, 1.000000000000000000, 0.9659258262890683122, 1.000000000000000000, 0.9659258262890683122, 1.000000000000000000, 0.9659258262890683122, 1.000000000000000000, 0.9659258262890680902, 1.000000000000000222 ) ) 
 REPRESENTATION_ITEM ( '' )  );
#3538 = LINE ( 'NONE', #35533, #20781 ) ;
#3540 = LINE ( 'NONE', #83854, #32492 ) ;
#3539 = VECTOR ( 'NONE', #87444, 1000.000000000000000 ) ;
#3541 = CARTESIAN_POINT ( 'NONE',  ( 21.48921356237309155, -27.52281430457070499, 5.000000000000000000 ) ) ;
#3543 = EDGE_CURVE ( 'NONE', #26060, #96265, #53752, .T. ) ;
#3542 = CARTESIAN_POINT ( 'NONE',  ( 2.669897814527331992, 17.25929247661554555, 19.83885114516070658 ) ) ;
#3544 = DIRECTION ( 'NONE',  ( 0.7071067811865487940, 0.7071067811865463515, -0.000000000000000000 ) ) ;
#3545 = CARTESIAN_POINT ( 'NONE',  ( 30.45790314143522437, 6.871911579029515771, 3.967499999999989146 ) ) ;
#3546 = LINE ( 'NONE', #47153, #21346 ) ;
#3547 = DIRECTION ( 'NONE',  ( -0.000000000000000000, 0.3543493200069153248, 0.9351131265310292928 ) ) ;
#3548 = CARTESIAN_POINT ( 'NONE',  ( 69.18398860626899705, 28.73617430169835529, 5.000000000000000000 ) ) ;
#3549 = DIRECTION ( 'NONE',  ( -0.3543493200069162685, -0.000000000000000000, -0.9351131265310288487 ) ) ;
#3550 = ORIENTED_EDGE ( 'NONE', *, *, #103057, .T. ) ;
#3552 = ORIENTED_EDGE ( 'NONE', *, *, #92910, .F. ) ;
#3551 = EDGE_CURVE ( 'NONE', #5049, #29421, #95878, .T. ) ;
#3553 = ADVANCED_FACE ( 'NONE', ( #86378 ), #32712, .F. ) ;
#3554 = CARTESIAN_POINT ( 'NONE',  ( 90.68750000000001421, -5.819803920172573086, 5.819803920172572198 ) ) ;
#3555 = VERTEX_POINT ( 'NONE', #110222 ) ;
#3556 = VECTOR ( 'NONE', #133918, 1000.000000000000000 ) ;
#3557 = ORIENTED_EDGE ( 'NONE', *, *, #22856, .F. ) ;
#3558 = CARTESIAN_POINT ( 'NONE',  ( 25.39999999999999858, -57.15000000000009095, 34.92499999999998295 ) ) ;
#3559 = DIRECTION ( 'NONE',  ( 0.3543493200069164351, 2.781805975412904658E-17, -0.9351131265310288487 ) ) ;
#3560 = CARTESIAN_POINT ( 'NONE',  ( 11.47410930353643188, 8.505905029784415206, -4.231274956823338762 ) ) ;
#3561 = VERTEX_POINT ( 'NONE', #55167 ) ;
#3562 = CARTESIAN_POINT ( 'NONE',  ( 45.18398860626900415, 28.73617430169818832, 5.000000000000000000 ) ) ;
#3563 = ADVANCED_FACE ( 'NONE', ( #9 ), #121815, .T. ) ;
#3564 = DIRECTION ( 'NONE',  ( -0.7071067811865486830, 0.7071067811865464625, 0.000000000000000000 ) ) ;
#3565 = FACE_OUTER_BOUND ( 'NONE', #48736, .T. ) ;
#3566 = CARTESIAN_POINT ( 'NONE',  ( 126.3365831057324300, 6.972970002233967790, -1.493943918826199813 ) ) ;
#3567 = EDGE_CURVE ( 'NONE', #105583, #51106, #11610, .T. ) ;
#3568 = DIRECTION ( 'NONE',  ( 0.7071067811865487940, 0.7071067811865463515, 0.000000000000000000 ) ) ;
#3569 = LINE ( 'NONE', #125395, #58998 ) ;
#3570 = CARTESIAN_POINT ( 'NONE',  ( 66.29974487139159578, -27.71228299555252406, 4.000000000000000000 ) ) ;
#3571 = CARTESIAN_POINT ( 'NONE',  ( 12.70710678118645731, 2.259292476615688994, 5.000000000000000000 ) ) ;
#3572 = CARTESIAN_POINT ( 'NONE',  ( 0.000000000000000000, -4.068876922607777225, 4.000000000000000000 ) ) ;
#3573 = CARTESIAN_POINT ( 'NONE',  ( 33.48921356237309510, -27.52281430457078670, 5.000000000000000000 ) ) ;
#3574 = CARTESIAN_POINT ( 'NONE',  ( 25.39999999999999858, -43.14999999999999147, 34.92499999999998295 ) ) ;
#3575 = AXIS2_PLACEMENT_3D ( 'NONE', #28221, #39836, #84056 ) ;
#3576 = PLANE ( 'NONE',  #70091 ) ;
#3577 = EDGE_LOOP ( 'NONE', ( #118759, #87844, #72553, #94416 ) ) ;
#3578 = ORIENTED_EDGE ( 'NONE', *, *, #45322, .T. ) ;
#3579 = VECTOR ( 'NONE', #103608, 1000.000000000000000 ) ;
#3580 = CARTESIAN_POINT ( 'NONE',  ( 114.3337635252314470, 6.110000000000001208, 1.122388791418549305E-15 ) ) ;
#3581 = ORIENTED_EDGE ( 'NONE', *, *, #128326, .T. ) ;
#3582 = VECTOR ( 'NONE', #36358, 1000.000000000000000 ) ;
#3583 = EDGE_CURVE ( 'NONE', #112964, #38224, #45043, .T. ) ;
#3584 = LINE ( 'NONE', #25359, #133526 ) ;
#3585 = VECTOR ( 'NONE', #94657, 999.9999999999998863 ) ;
#3586 = CARTESIAN_POINT ( 'NONE',  ( 26.75159235450331963, -2.500000000000000444, 3.061616997868384620E-16 ) ) ;
#3587 = ORIENTED_EDGE ( 'NONE', *, *, #88857, .T. ) ;
#3588 = EDGE_CURVE ( 'NONE', #71830, #138961, #67493, .T. ) ;
#3589 = CARTESIAN_POINT ( 'NONE',  ( 3.299744871391591339, -27.71228299555208352, 4.000000000000000000 ) ) ;
#3590 = CYLINDRICAL_SURFACE ( 'NONE', #51191, 7.950000000000000178 ) ;
#3591 = CARTESIAN_POINT ( 'NONE',  ( 107.9745968585647660, 1.637169565754164058, -6.109999999999996767 ) ) ;
#3592 = VERTEX_POINT ( 'NONE', #100095 ) ;
#3593 = ORIENTED_EDGE ( 'NONE', *, *, #141464, .F. ) ;
#3594 = CARTESIAN_POINT ( 'NONE',  ( -6.938893903907228378E-15, -2.904428200921318481, -6.989807076074944447 ) ) ;
#3595 = CARTESIAN_POINT ( 'NONE',  ( 21.00548008471250938, 28.92564299267923644, 4.000000000000000000 ) ) ;
#3596 = ORIENTED_EDGE ( 'NONE', *, *, #125546, .T. ) ;
#3597 = ORIENTED_EDGE ( 'NONE', *, *, #69066, .T. ) ;
#3598 = VERTEX_POINT ( 'NONE', #748 ) ;
#3599 = CARTESIAN_POINT ( 'NONE',  ( -8.510786437626906675, -27.52281430457049183, 5.000000000000000000 ) ) ;
#3600 = CARTESIAN_POINT ( 'NONE',  ( 1.962903141435219601, -3.967499999999994476, 6.871911579029513106 ) ) ;
#3601 = EDGE_CURVE ( 'NONE', #112055, #60580, #89222, .T. ) ;
#3602 = FILL_AREA_STYLE_COLOUR ( '', #53782 ) ;
#3603 = CARTESIAN_POINT ( 'NONE',  ( 27.68840764549667455, 3.061616997868380183E-16, -2.500000000000001332 ) ) ;
#3604 = VERTEX_POINT ( 'NONE', #93099 ) ;
#3605 = ORIENTED_EDGE ( 'NONE', *, *, #130130, .F. ) ;
#3606 = PLANE ( 'NONE',  #96492 ) ;
#3607 = ORIENTED_EDGE ( 'NONE', *, *, #43777, .T. ) ;
#3608 = ORIENTED_EDGE ( 'NONE', *, *, #8739, .T. ) ;
#3609 = CARTESIAN_POINT ( 'NONE',  ( 5.816011393731002066, 28.73617430169783304, 5.000000000000000000 ) ) ;
#3610 = CARTESIAN_POINT ( 'NONE',  ( 14.99999999999990585, 8.966399257802175171, 5.000000000000000000 ) ) ;
#3611 = CARTESIAN_POINT ( 'NONE',  ( 21.29974487139158512, -27.71228299555221142, 4.000000000000000000 ) ) ;
#3612 = ORIENTED_EDGE ( 'NONE', *, *, #62969, .F. ) ;
#3613 = LINE ( 'NONE', #89933, #78410 ) ;
#3614 = DIRECTION ( 'NONE',  ( -0.3543493200069162685, -0.000000000000000000, -0.9351131265310288487 ) ) ;
#3615 = FACE_OUTER_BOUND ( 'NONE', #1981, .T. ) ;
#3616 = FACE_BOUND ( 'NONE', #97068, .T. ) ;
#3617 = ORIENTED_EDGE ( 'NONE', *, *, #100811, .T. ) ;
#3618 = DIRECTION ( 'NONE',  ( -0.7071067811865486830, 0.7071067811865463515, 0.000000000000000000 ) ) ;
#3619 = CARTESIAN_POINT ( 'NONE',  ( -9.328169399223467551, 2.259292476615694323, 4.000000000000000000 ) ) ;
#3620 = DIRECTION ( 'NONE',  ( 0.000000000000000000, 0.000000000000000000, -1.000000000000000000 ) ) ;
#3621 = ORIENTED_EDGE ( 'NONE', *, *, #55103, .F. ) ;
#3622 = CARTESIAN_POINT ( 'NONE',  ( -7.499999999999951150, 22.08746187583901843, 4.000000000000000000 ) ) ;
#3623 = ORIENTED_EDGE ( 'NONE', *, *, #98383, .F. ) ;
#3624 = ORIENTED_EDGE ( 'NONE', *, *, #27023, .F. ) ;
#3625 = ORIENTED_EDGE ( 'NONE', *, *, #119590, .T. ) ;
#3626 = VECTOR ( 'NONE', #47198, 1000.000000000000000 ) ;
#3627 = CARTESIAN_POINT ( 'NONE',  ( 36.37043019189811588, -3.055000000000001492, 5.291415217122917625 ) ) ;
#3628 = EDGE_LOOP ( 'NONE', ( #29084, #54341, #126120, #87490 ) ) ;
#3629 = CARTESIAN_POINT ( 'NONE',  ( -42.48921356237308800, -27.52281430457085065, 5.000000000000000000 ) ) ;
#3630 = VECTOR ( 'NONE', #35045, 1000.000000000000227 ) ;
#3631 = DIRECTION ( 'NONE',  ( 1.000000000000000000, 0.000000000000000000, 0.000000000000000000 ) ) ;
#3632 = LINE ( 'NONE', #102995, #10260 ) ;
#3633 = ORIENTED_EDGE ( 'NONE', *, *, #118658, .T. ) ;
#3634 = ADVANCED_FACE ( 'NONE', ( #38023 ), #73498, .T. ) ;
#3635 = CARTESIAN_POINT ( 'NONE',  ( 8.816011393731004731, 28.73617430169781173, 5.000000000000000000 ) ) ;
#3636 = CARTESIAN_POINT ( 'NONE',  ( -35.99451991528749772, 28.92564299267963079, 4.000000000000000000 ) ) ;
#3637 = PLANE ( 'NONE',  #57535 ) ;
#3638 = DIRECTION ( 'NONE',  ( -0.7071067811865486830, 0.7071067811865464625, 0.000000000000000000 ) ) ;
#3639 = VECTOR ( 'NONE', #8864, 999.9999999999998863 ) ;
#3640 = EDGE_CURVE ( 'NONE', #10027, #73248, #115310, .T. ) ;
#3641 = ORIENTED_EDGE ( 'NONE', *, *, #73765, .F. ) ;
#3642 = ORIENTED_EDGE ( 'NONE', *, *, #72735, .F. ) ;
#3643 = ORIENTED_EDGE ( 'NONE', *, *, #66682, .F. ) ;
#3644 = ORIENTED_EDGE ( 'NONE', *, *, #33729, .F. ) ;
#3645 = ORIENTED_EDGE ( 'NONE', *, *, #66822, .T. ) ;
#3647 = VERTEX_POINT ( 'NONE', #118399 ) ;
#3646 = ADVANCED_FACE ( 'NONE', ( #117662 ), #29963, .T. ) ;
#3648 = CARTESIAN_POINT ( 'NONE',  ( -8.999999999999934275, -1.447814304570815169, 5.000000000000000000 ) ) ;
#3649 = DIRECTION ( 'NONE',  ( -1.000000000000000000, 5.151277200819050839E-14, 0.000000000000000000 ) ) ;
#3650 = EDGE_CURVE ( 'NONE', #133870, #54574, #139497, .T. ) ;
#3651 = EDGE_CURVE ( 'NONE', #97655, #122495, #40180, .T. ) ;
#3652 = DIRECTION ( 'NONE',  ( -1.000000000000000000, 0.000000000000000000, 0.000000000000000000 ) ) ;
#3653 = ORIENTED_EDGE ( 'NONE', *, *, #99913, .F. ) ;
#3654 = DIRECTION ( 'NONE',  ( -1.000000000000000000, -1.224606353822377258E-16, -0.000000000000000000 ) ) ;
#3655 = EDGE_LOOP ( 'NONE', ( #129888, #120836, #26462, #126212 ) ) ;
#3656 = VECTOR ( 'NONE', #104884, 1000.000000000000227 ) ;
#3658 = EDGE_CURVE ( 'NONE', #34174, #20152, #84390, .T. ) ;
#3657 = DIRECTION ( 'NONE',  ( 1.318980745116185161E-16, -1.000000000000000000, 0.000000000000000000 ) ) ;
#3659 = EDGE_CURVE ( 'NONE', #6418, #75592, #115514, .T. ) ;
#3660 = CARTESIAN_POINT ( 'NONE',  ( 32.73373647476854842, 5.808823158059036373, 5.808823158059032821 ) ) ;
#3661 = VECTOR ( 'NONE', #6772, 1000.000000000000000 ) ;
#3662 = CARTESIAN_POINT ( 'NONE',  ( 0.9420698081018860082, 7.934999999999993392, 2.126176841940951689 ) ) ;
#3663 = VERTEX_POINT ( 'NONE', #27834 ) ;
#3665 = CYLINDRICAL_SURFACE ( 'NONE', #70793, 0.5000000000000004441 ) ;
#3664 = CARTESIAN_POINT ( 'NONE',  ( 100.3912635252314516, -4.472830434245839371, -4.472830434245839371 ) ) ;
#3666 = CIRCLE ( 'NONE', #29167, 5.999999999999998224 ) ;
#3667 = EDGE_CURVE ( 'NONE', #17718, #84184, #113400, .T. ) ;
#3668 = CARTESIAN_POINT ( 'NONE',  ( -30.00000000000000355, 2.375000000000000000, -4.320000000000002061 ) ) ;
#3669 = FACE_OUTER_BOUND ( 'NONE', #82346, .T. ) ;
#3670 = ORIENTED_EDGE ( 'NONE', *, *, #36206, .F. ) ;
#3671 = EDGE_LOOP ( 'NONE', ( #129027, #58220, #39192, #50932 ) ) ;
#3672 = DIRECTION ( 'NONE',  ( 0.6830127018922181881, 0.6830127018922202975, -0.2588190451025214056 ) ) ;
#3673 = ORIENTED_EDGE ( 'NONE', *, *, #66100, .F. ) ;
#3674 = LINE ( 'NONE', #93587, #44049 ) ;
#3675 = PLANE ( 'NONE',  #34828 ) ;
#3676 = DIRECTION ( 'NONE',  ( -0.000000000000000000, -0.3543493200069152693, 0.9351131265310292928 ) ) ;
#3677 = CARTESIAN_POINT ( 'NONE',  ( 56.90810577924025893, -46.18886352141517904, -34.92499999999998295 ) ) ;
#3678 = DIRECTION ( 'NONE',  ( -0.000000000000000000, 0.3543493200069153248, 0.9351131265310292928 ) ) ;
#3679 = ORIENTED_EDGE ( 'NONE', *, *, #89408, .T. ) ;
#3680 = DIRECTION ( 'NONE',  ( 0.7071067811865487940, 0.7071067811865463515, 0.000000000000000000 ) ) ;
#3681 = ADVANCED_FACE ( 'NONE', ( #85069 ), #49630, .F. ) ;
#3682 = DIRECTION ( 'NONE',  ( -0.7071067811865486830, 0.7071067811865464625, 0.000000000000000000 ) ) ;
#3683 = CARTESIAN_POINT ( 'NONE',  ( -63.18398860626900415, 28.73617430169831621, 5.000000000000000000 ) ) ;
#3684 = ORIENTED_EDGE ( 'NONE', *, *, #54317, .F. ) ;
#3685 = PLANE ( 'NONE',  #30446 ) ;
#3686 = CYLINDRICAL_SURFACE ( 'NONE', #118716, 2.500000000000000000 ) ;
#3687 = ORIENTED_EDGE ( 'NONE', *, *, #3987, .F. ) ;
#3689 = ORIENTED_EDGE ( 'NONE', *, *, #65043, .T. ) ;
#3688 = CARTESIAN_POINT ( 'NONE',  ( 36.18398860626899705, 28.73617430169812437, 5.000000000000000000 ) ) ;
#3690 = ORIENTED_EDGE ( 'NONE', *, *, #136284, .T. ) ;
#3691 = LINE ( 'NONE', #139276, #137332 ) ;
#3692 = DIRECTION ( 'NONE',  ( 0.7071067811865487940, 0.7071067811865463515, 0.000000000000000000 ) ) ;
#3693 = EDGE_CURVE ( 'NONE', #133079, #18391, #101151, .T. ) ;
#3694 = ORIENTED_EDGE ( 'NONE', *, *, #14525, .F. ) ;
#3695 = DIRECTION ( 'NONE',  ( 0.000000000000000000, -1.000000000000000000, 0.000000000000000000 ) ) ;
#3696 = PLANE ( 'NONE',  #90098 ) ;
#3697 = EDGE_LOOP ( 'NONE', ( #121818, #10630, #4080, #97755, #67196 ) ) ;
#3698 = DIRECTION ( 'NONE',  ( -2.891205793294675861E-16, 1.000000000000000000, 0.000000000000000000 ) ) ;
#3699 = LINE ( 'NONE', #90026, #72163 ) ;
#3700 = PLANE ( 'NONE',  #56025 ) ;
#3701 = EDGE_CURVE ( 'NONE', #121450, #116985, #105384, .T. ) ;
#3703 = AXIS2_PLACEMENT_3D ( 'NONE', #62105, #118597, #52623 ) ;
#3702 = CARTESIAN_POINT ( 'NONE',  ( 184.1500000000000057, -30.18000000000009564, -15.92500000000064375 ) ) ;
#3704 = CARTESIAN_POINT ( 'NONE',  ( 125.6998834332835884, -5.108784383707307697, 5.835737331199903899 ) ) ;
#3705 = CARTESIAN_POINT ( 'NONE',  ( 28.80836038379622011, 7.949999999999996625, 2.130196079827431088 ) ) ;
#3706 = CARTESIAN_POINT ( 'NONE',  ( -11.29289321881337216, 5.259292476615661016, 5.000000000000000000 ) ) ;
#3707 = ORIENTED_EDGE ( 'NONE', *, *, #112697, .F. ) ;
#3708 = ORIENTED_EDGE ( 'NONE', *, *, #22336, .T. ) ;
#3709 = VERTEX_POINT ( 'NONE', #93806 ) ;
#3710 = EDGE_CURVE ( 'NONE', #68343, #76248, #6040, .T. ) ;
#3711 = CARTESIAN_POINT ( 'NONE',  ( 124.3750000000000000, 7.950000000000000178, 1.460391307983218535E-15 ) ) ;
#3712 = EDGE_LOOP ( 'NONE', ( #62944, #26907, #113600, #140208 ) ) ;
#3713 = EDGE_LOOP ( 'NONE', ( #114435, #13870, #8632, #138126 ) ) ;
#3714 = ADVANCED_FACE ( 'NONE', ( #138756 ), #50316, .F. ) ;
#3715 = ORIENTED_EDGE ( 'NONE', *, *, #29440, .F. ) ;
#3716 = CIRCLE ( 'NONE', #101022, 2.500000000000000444 ) ;
#3717 = DIRECTION ( 'NONE',  ( -0.000000000000000000, 0.3543493200069153248, 0.9351131265310292928 ) ) ;
#3718 = CARTESIAN_POINT ( 'NONE',  ( 7.939999999999994174, -60.26999999999998892, -12.24790000000000134 ) ) ;
#3719 = ORIENTED_EDGE ( 'NONE', *, *, #46344, .F. ) ;
#3720 = PLANE ( 'NONE',  #124897 ) ;
#3721 = EDGE_CURVE ( 'NONE', #79129, #87604, #38720, .T. ) ;
#3722 = CARTESIAN_POINT ( 'NONE',  ( -1.179999999999997939, -9.043340090917734386, 10.00000000000000000 ) ) ;
#3723 = DIRECTION ( 'NONE',  ( 1.000000000000000000, 0.000000000000000000, 0.000000000000000000 ) ) ;
#3724 = CARTESIAN_POINT ( 'NONE',  ( 111.2712635252314612, 4.472830434245839371, 4.472830434245842035 ) ) ;
#3725 = ORIENTED_EDGE ( 'NONE', *, *, #105591, .F. ) ;
#3726 = LINE ( 'NONE', #15325, #53379 ) ;
#3727 = LINE ( 'NONE', #48018, #37733 ) ;
#3728 = LINE ( 'NONE', #80639, #54216 ) ;
#3729 = CARTESIAN_POINT ( 'NONE',  ( 0.7902862351827044662, 7.048400157404861588, 1.962111654240061398 ) ) ;
#3730 = CARTESIAN_POINT ( 'NONE',  ( 5.700255128608413102, -27.71228299555201957, 4.000000000000000000 ) ) ;
#3731 = ADVANCED_FACE ( 'NONE', ( #28568 ), #116978, .F. ) ;
#3732 = LINE ( 'NONE', #92193, #141822 ) ;
#3733 = CARTESIAN_POINT ( 'NONE',  ( -21.18398860626899349, 28.73617430169802134, 5.000000000000000000 ) ) ;
#3734 = CARTESIAN_POINT ( 'NONE',  ( 40.62086038379622721, -6.884901960086286188, 3.974999999999997424 ) ) ;
#3735 = VECTOR ( 'NONE', #101912, 1000.000000000000227 ) ;
#3736 = DIRECTION ( 'NONE',  ( 0.7071067811865487940, 0.7071067811865463515, 0.000000000000000000 ) ) ;
#3737 =( LENGTH_UNIT ( ) NAMED_UNIT ( * ) SI_UNIT ( .MILLI., .METRE. ) );
#3738 = ORIENTED_EDGE ( 'NONE', *, *, #9128, .T. ) ;
#3739 = ORIENTED_EDGE ( 'NONE', *, *, #41354, .F. ) ;
#3740 = CARTESIAN_POINT ( 'NONE',  ( 33.66666666666666430, 6.884901960086285300, 3.975000000000003642 ) ) ;
#3741 = ORIENTED_EDGE ( 'NONE', *, *, #43777, .F. ) ;
#3742 = VECTOR ( 'NONE', #4108, 999.9999999999998863 ) ;
#3743 = EDGE_LOOP ( 'NONE', ( #50089, #133570, #125348, #98410 ) ) ;
#3744 = ADVANCED_FACE ( 'NONE', ( #143023 ), #31415, .F. ) ;
#3745 = CARTESIAN_POINT ( 'NONE',  ( 32.99999999999977973, 8.587461875839167647, 4.000000000000000000 ) ) ;
#3746 = DIRECTION ( 'NONE',  ( -1.000000000000000000, -0.000000000000000000, 0.000000000000000000 ) ) ;
#3747 = EDGE_LOOP ( 'NONE', ( #34545, #33508, #91184, #83687 ) ) ;
#3748 = LINE ( 'NONE', #26268, #31656 ) ;
#3749 = DIRECTION ( 'NONE',  ( 0.7071067811865487940, 0.7071067811865463515, 0.000000000000000000 ) ) ;
#3750 = LINE ( 'NONE', #37134, #95303 ) ;
#3751 = CARTESIAN_POINT ( 'NONE',  ( 32.66709685856476852, -3.055000000000000160, -5.291415217122921177 ) ) ;
#3752 = ORIENTED_EDGE ( 'NONE', *, *, #8897, .T. ) ;
#3753 = DIRECTION ( 'NONE',  ( -0.7071067811865486830, -0.7071067811865464625, -0.000000000000000000 ) ) ;
#3754 = ORIENTED_EDGE ( 'NONE', *, *, #118260, .T. ) ;
#3755 = CARTESIAN_POINT ( 'NONE',  ( 0.000000000000000000, 7.588810512006213038, -3.013526669885226994 ) ) ;
#3756 = CARTESIAN_POINT ( 'NONE',  ( 12.69999999999999574, -25.83999999999998565, 13.17925390838733968 ) ) ;
#3757 = CARTESIAN_POINT ( 'NONE',  ( -7.140000000000001457, 0.000000000000000000, -40.00000000000000000 ) ) ;
#3758 = DIRECTION ( 'NONE',  ( -0.7071067811865486830, -0.7071067811865464625, 0.000000000000000000 ) ) ;
#3759 = EDGE_LOOP ( 'NONE', ( #136935, #2662, #111618, #92744 ) ) ;
#3760 = EDGE_CURVE ( 'NONE', #100040, #99958, #64754, .T. ) ;
#3761 = AXIS2_PLACEMENT_3D ( 'NONE', #89740, #111490, #134706 ) ;
#3762 = VERTEX_POINT ( 'NONE', #21949 ) ;
#3763 = DIRECTION ( 'NONE',  ( -0.000000000000000000, 0.3543493200069153248, 0.9351131265310292928 ) ) ;
#3764 = LINE ( 'NONE', #16068, #41581 ) ;
#3765 = CARTESIAN_POINT ( 'NONE',  ( 8.999999999999932498, -22.22500000000000853, 4.412002311790025999 ) ) ;
#3766 = VECTOR ( 'NONE', #62654, 999.9999999999998863 ) ;
#3767 = VECTOR ( 'NONE', #82133, 1000.000000000000000 ) ;
#3768 = CIRCLE ( 'NONE', #29261, 2.055000000000001048 ) ;
#3769 = CARTESIAN_POINT ( 'NONE',  ( 46.28709685856477307, 3.054999999999997495, 5.291415217122919401 ) ) ;
#3770 = CARTESIAN_POINT ( 'NONE',  ( 9.328169399223463998, -3.740707523384244837, 4.000000000000000000 ) ) ;
#3771 = CARTESIAN_POINT ( 'NONE',  ( 60.18398860626900415, 28.73617430169829490, 5.000000000000000000 ) ) ;
#3772 = VERTEX_POINT ( 'NONE', #120515 ) ;
#3773 = ORIENTED_EDGE ( 'NONE', *, *, #117751, .F. ) ;
#3774 = VECTOR ( 'NONE', #60868, 1000.000000000000227 ) ;
#3775 = CARTESIAN_POINT ( 'NONE',  ( -6.183988606268994381, 28.73617430169791476, 5.000000000000000000 ) ) ;
#3776 = ORIENTED_EDGE ( 'NONE', *, *, #112393, .F. ) ;
#3777 = EDGE_CURVE ( 'NONE', #121813, #70885, #43710, .T. ) ;
#3778 = EDGE_CURVE ( 'NONE', #108671, #42790, #8871, .T. ) ;
#3779 = CARTESIAN_POINT ( 'NONE',  ( -28.82816939922333432, 12.75929247661558996, 4.000000000000000000 ) ) ;
#3780 = ORIENTED_EDGE ( 'NONE', *, *, #86903, .F. ) ;
#3781 = DIRECTION ( 'NONE',  ( 0.7071067811865487940, -0.7071067811865463515, 0.000000000000000000 ) ) ;
#3782 = DIRECTION ( 'NONE',  ( 0.7071067811865487940, -0.7071067811865463515, -0.000000000000000000 ) ) ;
#3783 = FACE_BOUND ( 'NONE', #18436, .T. ) ;
#3784 = EDGE_CURVE ( 'NONE', #44987, #45460, #96618, .T. ) ;
#3785 = DIRECTION ( 'NONE',  ( -0.3543493200069162685, -0.000000000000000000, -0.9351131265310288487 ) ) ;
#3786 = PRESENTATION_STYLE_ASSIGNMENT (( #58989 ) ) ;
#3787 = CARTESIAN_POINT ( 'NONE',  ( -32.99999999999977263, 19.93112307739198386, 4.000000000000000000 ) ) ;
#3788 = SURFACE_STYLE_FILL_AREA ( #37178 ) ;
#3790 = ORIENTED_EDGE ( 'NONE', *, *, #97733, .T. ) ;
#3789 = CARTESIAN_POINT ( 'NONE',  ( 1.499999999999987566, -14.70932175296477062, -11.46312253303837636 ) ) ;
#3791 = CARTESIAN_POINT ( 'NONE',  ( 26.99999999999982236, -19.44781430457063465, 5.000000000000000000 ) ) ;
#3792 = ORIENTED_EDGE ( 'NONE', *, *, #141574, .F. ) ;
#3793 = ORIENTED_EDGE ( 'NONE', *, *, #23027, .T. ) ;
#3794 = CARTESIAN_POINT ( 'NONE',  ( 67.28709685856478018, 3.054999999999997495, 5.291415217122919401 ) ) ;
#3795 = CIRCLE ( 'NONE', #82606, 2.247899999999998677 ) ;
#3796 = ORIENTED_EDGE ( 'NONE', *, *, #47475, .T. ) ;
#3797 = CARTESIAN_POINT ( 'NONE',  ( 30.48921356237309510, -27.52281430457076894, 5.000000000000000000 ) ) ;
#3798 = ORIENTED_EDGE ( 'NONE', *, *, #42342, .F. ) ;
#3799 = FACE_OUTER_BOUND ( 'NONE', #140007, .T. ) ;
#3800 = AXIS2_PLACEMENT_3D ( 'NONE', #112391, #58040, #135580 ) ;
#3801 =( BOUNDED_CURVE ( )  B_SPLINE_CURVE ( 2, ( #73847, #139119, #84047, #128243, #39077, #118020, #38371, #83303, #127513, #18725, #116634, #107176, #52093 ),
 .UNSPECIFIED., .F., .F. ) 
 B_SPLINE_CURVE_WITH_KNOTS ( ( 3, 2, 2, 2, 2, 2, 3 ),
 ( 0.9333333333333333481, 0.9361111111111111160, 0.9388888888888888840, 0.9416666666666666519, 0.9444444444444444198, 0.9472222222222221877, 0.9499999999999999556 ),
 .UNSPECIFIED. ) 
 CURVE ( )  GEOMETRIC_REPRESENTATION_ITEM ( )  RATIONAL_B_SPLINE_CURVE ( ( 1.000000000000000000, 0.9659258262890683122, 1.000000000000000000, 0.9659258262890683122, 1.000000000000000000, 0.9659258262890683122, 1.000000000000000000, 0.9659258262890683122, 1.000000000000000000, 0.9659258262890683122, 1.000000000000000000, 0.9659258262890683122, 1.000000000000000000 ) ) 
 REPRESENTATION_ITEM ( '' )  );
#3802 = CARTESIAN_POINT ( 'NONE',  ( -24.48921356237309510, -27.52281430457072631, 5.000000000000000000 ) ) ;
#3803 = DIRECTION ( 'NONE',  ( -0.6830127018922181881, 0.6830127018922202975, -0.2588190451025214056 ) ) ;
#3804 = CARTESIAN_POINT ( 'NONE',  ( -33.29974487139158867, -27.71228299555229313, 4.000000000000000000 ) ) ;
#3805 = FACE_OUTER_BOUND ( 'NONE', #56449, .T. ) ;
#3806 = CARTESIAN_POINT ( 'NONE',  ( 29.34328999833768847, 3.759292476615678336, 13.27625715073272517 ) ) ;
#3807 = DIRECTION ( 'NONE',  ( 1.000000000000000000, 0.000000000000000000, 0.000000000000000000 ) ) ;
#3808 = ORIENTED_EDGE ( 'NONE', *, *, #46123, .F. ) ;
#3809 =( GEOMETRIC_REPRESENTATION_CONTEXT ( 3 ) GLOBAL_UNCERTAINTY_ASSIGNED_CONTEXT ( ( #30502 ) ) GLOBAL_UNIT_ASSIGNED_CONTEXT ( ( #103757, #72641, #27642 ) ) REPRESENTATION_CONTEXT ( 'NONE', 'WORKASPACE' ) );
#3810 = VERTEX_POINT ( 'NONE', #9627 ) ;
#3811 = CARTESIAN_POINT ( 'NONE',  ( -48.18398860626899705, 28.73617430169820608, 5.000000000000000000 ) ) ;
#3812 = CARTESIAN_POINT ( 'NONE',  ( 0.000000000000000000, 0.000000000000000000, 5.000000000000000000 ) ) ;
#3813 = ORIENTED_EDGE ( 'NONE', *, *, #31879, .T. ) ;
#3814 = ORIENTED_EDGE ( 'NONE', *, *, #63147, .T. ) ;
#3815 = ORIENTED_EDGE ( 'NONE', *, *, #31375, .T. ) ;
#3816 = VECTOR ( 'NONE', #59667, 1000.000000000000000 ) ;
#3817 = EDGE_CURVE ( 'NONE', #109916, #91920, #86519, .T. ) ;
#3818 = CARTESIAN_POINT ( 'NONE',  ( 30.48921356237309510, -27.52281430457076894, 5.000000000000000000 ) ) ;
#3819 = ORIENTED_EDGE ( 'NONE', *, *, #105571, .T. ) ;
#3820 = LINE ( 'NONE', #105318, #104191 ) ;
#3821 = AXIS2_PLACEMENT_3D ( 'NONE', #67543, #24016, #99395 ) ;
#3822 = EDGE_CURVE ( 'NONE', #98397, #42229, #121959, .T. ) ;
#3823 = EDGE_CURVE ( 'NONE', #58068, #22022, #140858, .T. ) ;
#3824 = CARTESIAN_POINT ( 'NONE',  ( 5.608736474768551972, -5.808823158059033709, 5.808823158059035485 ) ) ;
#3825 = CARTESIAN_POINT ( 'NONE',  ( -7.499999999999945821, 12.05218569542904561, 5.000000000000000000 ) ) ;
#3826 = ADVANCED_FACE ( 'NONE', ( #130745 ), #22399, .T. ) ;
#3827 = ORIENTED_EDGE ( 'NONE', *, *, #24964, .F. ) ;
#3828 = AXIS2_PLACEMENT_3D ( 'NONE', #103299, #37359, #81594 ) ;
#3829 = LINE ( 'NONE', #36512, #91993 ) ;
#3830 = ADVANCED_FACE ( 'NONE', ( #64043 ), #13199, .T. ) ;
#3831 = DIRECTION ( 'NONE',  ( -1.000000000000000000, -1.224606353822377258E-16, -0.000000000000000000 ) ) ;
#3832 = CARTESIAN_POINT ( 'NONE',  ( 24.50000000000000000, 0.000000000000000000, 6.094999999999989981 ) ) ;
#3834 = VERTEX_POINT ( 'NONE', #43012 ) ;
#3833 = DIRECTION ( 'NONE',  ( 0.3543493200069162685, -0.000000000000000000, -0.9351131265310288487 ) ) ;
#3835 = ORIENTED_EDGE ( 'NONE', *, *, #24367, .T. ) ;
#3836 = EDGE_CURVE ( 'NONE', #66460, #6035, #21242, .T. ) ;
#3837 = CARTESIAN_POINT ( 'NONE',  ( 3.183988606268992161, 28.73617430169789699, 5.000000000000000000 ) ) ;
#3838 = DIRECTION ( 'NONE',  ( -0.000000000000000000, 0.3543493200069153248, 0.9351131265310292928 ) ) ;
#3839 = DIRECTION ( 'NONE',  ( 1.000000000000000000, 0.000000000000000000, 0.000000000000000000 ) ) ;
#3840 = EDGE_LOOP ( 'NONE', ( #137749, #121038, #124948, #32635 ) ) ;
#3841 = CARTESIAN_POINT ( 'NONE',  ( -5.999999999999963585, 20.70535890316560668, 1.956823837851930481 ) ) ;
#3842 = DIRECTION ( 'NONE',  ( -0.7071067811865486830, -0.7071067811865464625, -0.000000000000000000 ) ) ;
#3843 = EDGE_CURVE ( 'NONE', #4395, #28418, #104084, .T. ) ;
#3844 = DIRECTION ( 'NONE',  ( 0.000000000000000000, 0.000000000000000000, -1.000000000000000000 ) ) ;
#3845 = PLANE ( 'NONE',  #51188 ) ;
#3846 = LINE ( 'NONE', #48130, #9724 ) ;
#3847 = ORIENTED_EDGE ( 'NONE', *, *, #1702, .T. ) ;
#3848 = CARTESIAN_POINT ( 'NONE',  ( 33.48921356237309510, -27.52281430457078670, 5.000000000000000000 ) ) ;
#3849 = LINE ( 'NONE', #48133, #137313 ) ;
#3850 = LINE ( 'NONE', #114775, #30689 ) ;
#3851 = EDGE_CURVE ( 'NONE', #52853, #49616, #40961, .T. ) ;
#3852 = CARTESIAN_POINT ( 'NONE',  ( 0.000000000000000000, 10.93112307739207978, 4.000000000000000000 ) ) ;
#3853 = PRESENTATION_LAYER_ASSIGNMENT (  '', '', ( #8408 ) ) ;
#3854 = CARTESIAN_POINT ( 'NONE',  ( 2.924914550060624840, 2.500000000000000888, 0.000000000000000000 ) ) ;
#3855 = EDGE_CURVE ( 'NONE', #7505, #43144, #90055, .T. ) ;
#3856 = ORIENTED_EDGE ( 'NONE', *, *, #143155, .F. ) ;
#3857 = ORIENTED_EDGE ( 'NONE', *, *, #130066, .F. ) ;
#3858 = CARTESIAN_POINT ( 'NONE',  ( 32.16170612452599897, -6.740707523384223521, 16.75550250614875480 ) ) ;
#3859 = DIRECTION ( 'NONE',  ( 1.000000000000000000, 0.000000000000000000, 0.000000000000000000 ) ) ;
#3860 = EDGE_CURVE ( 'NONE', #12969, #57857, #45180, .T. ) ;
#3861 = VECTOR ( 'NONE', #102788, 1000.000000000000000 ) ;
#3862 = AXIS2_PLACEMENT_3D ( 'NONE', #134908, #25378, #81229 ) ;
#3863 = CARTESIAN_POINT ( 'NONE',  ( 1.145403141435219485, -2.126176841940958351, -7.934999999999989839 ) ) ;
#3864 = LINE ( 'NONE', #80084, #13419 ) ;
#3865 = AXIS2_PLACEMENT_3D ( 'NONE', #51228, #83133, #95423 ) ;
#3866 = LINE ( 'NONE', #5318, #138742 ) ;
#3867 = DIRECTION ( 'NONE',  ( 0.000000000000000000, -0.3543493200069152138, 0.9351131265310292928 ) ) ;
#3868 = CARTESIAN_POINT ( 'NONE',  ( 30.48921356237309510, -27.52281430457076894, 5.000000000000000000 ) ) ;
#3869 = VERTEX_POINT ( 'NONE', #133588 ) ;
#3870 = DIRECTION ( 'NONE',  ( 1.000000000000000000, 0.000000000000000000, 0.000000000000000000 ) ) ;
#3871 = AXIS2_PLACEMENT_3D ( 'NONE', #23770, #133952, #45551 ) ;
#3872 = CARTESIAN_POINT ( 'NONE',  ( 36.18398860626899705, 28.73617430169812437, 5.000000000000000000 ) ) ;
#3873 = VECTOR ( 'NONE', #6598, 1000.000000000000000 ) ;
#3874 = CARTESIAN_POINT ( 'NONE',  ( -14.51078643762690490, -27.52281430457045275, 5.000000000000000000 ) ) ;
#3875 = CARTESIAN_POINT ( 'NONE',  ( 47.30793019189811588, -6.109999999999999432, 1.637169565754158507 ) ) ;
#3876 = DIRECTION ( 'NONE',  ( -0.7071067811865486830, -0.7071067811865464625, 0.000000000000000000 ) ) ;
#3877 = CARTESIAN_POINT ( 'NONE',  ( -6.183988606268994381, 28.73617430169791476, 5.000000000000000000 ) ) ;
#3878 = ORIENTED_EDGE ( 'NONE', *, *, #99618, .F. ) ;
#3879 = CARTESIAN_POINT ( 'NONE',  ( 18.70710678118641468, -12.74070752338415247, 5.000000000000000000 ) ) ;
#3880 = EDGE_CURVE ( 'NONE', #96580, #31310, #34268, .T. ) ;
#3881 = EDGE_LOOP ( 'NONE', ( #60027, #47426, #63642, #119578 ) ) ;
#3882 = DIRECTION ( 'NONE',  ( -0.7071067811865487940, 0.7071067811865463515, -0.000000000000000000 ) ) ;
#3883 = SURFACE_SIDE_STYLE ('',( #14805 ) ) ;
#3884 = FACE_OUTER_BOUND ( 'NONE', #74681, .T. ) ;
#3885 = DIRECTION ( 'NONE',  ( -0.7071067811865487940, 0.7071067811865463515, 0.000000000000000000 ) ) ;
#3886 = DIRECTION ( 'NONE',  ( 0.7071067811865486830, -0.7071067811865464625, -0.000000000000000000 ) ) ;
#3887 = DIRECTION ( 'NONE',  ( -0.7071067811865486830, -0.7071067811865464625, 0.000000000000000000 ) ) ;
#3888 = VERTEX_POINT ( 'NONE', #23370 ) ;
#3889 = FACE_OUTER_BOUND ( 'NONE', #107226, .T. ) ;
#3890 = CARTESIAN_POINT ( 'NONE',  ( -13.49999999999990052, -7.912538124160676922, 4.000000000000000000 ) ) ;
#3891 = UNCERTAINTY_MEASURE_WITH_UNIT (LENGTH_MEASURE( 1.000000000000000082E-05 ), #7913, 'distance_accuracy_value', 'NONE');
#3892 = AXIS2_PLACEMENT_3D ( 'NONE', #74870, #19729, #21875 ) ;
#3893 = CARTESIAN_POINT ( 'NONE',  ( -28.99806943317882002, -22.22500000000000142, 4.500000000000000888 ) ) ;
#3894 = EDGE_CURVE ( 'NONE', #122495, #91285, #14655, .T. ) ;
#3895 = CARTESIAN_POINT ( 'NONE',  ( 118.2500000000000000, -9.735942053221458872E-16, 7.950000000000000178 ) ) ;
#3896 = CARTESIAN_POINT ( 'NONE',  ( 78.97502705046288440, -5.819803920172572198, 5.819803920172572198 ) ) ;
#3897 = AXIS2_PLACEMENT_3D ( 'NONE', #57590, #101773, #135157 ) ;
#3898 = CARTESIAN_POINT ( 'NONE',  ( 36.29974487139159578, -27.71228299555231445, 4.000000000000000000 ) ) ;
#3899 = ORIENTED_EDGE ( 'NONE', *, *, #125868, .F. ) ;
#3900 = ORIENTED_EDGE ( 'NONE', *, *, #19303, .T. ) ;
#3901 = CARTESIAN_POINT ( 'NONE',  ( 62.10416666666665719, 2.130196079827422206, 7.950000000000001954 ) ) ;
#3902 = FACE_OUTER_BOUND ( 'NONE', #3671, .T. ) ;
#3903 = EDGE_CURVE ( 'NONE', #75959, #135574, #52640, .T. ) ;
#3904 = PLANE ( 'NONE',  #90233 ) ;
#3905 = LINE ( 'NONE', #115526, #135466 ) ;
#3906 = COLOUR_RGB ( '', 0.40784314, 0.44705882, 0.49803922) ;
#3907 = ORIENTED_EDGE ( 'NONE', *, *, #45178, .T. ) ;
#3908 = CARTESIAN_POINT ( 'NONE',  ( 6.707106781186499944, -9.740707523384186217, 5.000000000000000000 ) ) ;
#3909 = EDGE_CURVE ( 'NONE', #98989, #50205, #100937, .T. ) ;
#3910 = CARTESIAN_POINT ( 'NONE',  ( 20.65000000000000213, 0.000000000000000000, 0.000000000000000000 ) ) ;
#3911 = CARTESIAN_POINT ( 'NONE',  ( 52.20876352523143282, -7.482591942790329030E-16, 6.110000000000001208 ) ) ;
#3912 = LINE ( 'NONE', #27136, #34436 ) ;
#3913 = ORIENTED_EDGE ( 'NONE', *, *, #97483, .T. ) ;
#3914 = ORIENTED_EDGE ( 'NONE', *, *, #47579, .F. ) ;
#3915 = CARTESIAN_POINT ( 'NONE',  ( -20.99999999999985789, 19.93112307739198386, 4.000000000000000000 ) ) ;
#3916 = CARTESIAN_POINT ( 'NONE',  ( -13.49999999999991473, 13.08746187583912146, 4.000000000000000000 ) ) ;
#3917 = VECTOR ( 'NONE', #94749, 1000.000000000000227 ) ;
#3918 = LINE ( 'NONE', #45375, #48621 ) ;
#3919 = EDGE_CURVE ( 'NONE', #140124, #103327, #24108, .T. ) ;
#3920 = CARTESIAN_POINT ( 'NONE',  ( -36.48921356237310221, -27.52281430457080802, 5.000000000000000000 ) ) ;
#3922 = VERTEX_POINT ( 'NONE', #68362 ) ;
#3921 = CARTESIAN_POINT ( 'NONE',  ( -5.816011393731002066, 28.73617430169783304, 5.000000000000000000 ) ) ;
#3923 = DIRECTION ( 'NONE',  ( 0.6830127018922180770, -0.6830127018922204085, -0.2588190451025213501 ) ) ;
#3924 = CARTESIAN_POINT ( 'NONE',  ( -36.49816348513933661, -17.24070752338410628, 8.407044977365309535 ) ) ;
#3925 = DIRECTION ( 'NONE',  ( 0.000000000000000000, -1.000000000000000000, 0.000000000000000000 ) ) ;
#3926 = DIRECTION ( 'NONE',  ( 0.7071067811865486830, -0.7071067811865464625, -0.000000000000000000 ) ) ;
#3927 = ORIENTED_EDGE ( 'NONE', *, *, #143472, .T. ) ;
#3928 = EDGE_CURVE ( 'NONE', #117254, #13095, #24805, .T. ) ;
#3929 = ORIENTED_EDGE ( 'NONE', *, *, #34878, .T. ) ;
#3930 = STYLED_ITEM ( 'NONE', ( #74094 ), #92605 ) ;
#3931 = LINE ( 'NONE', #81578, #76552 ) ;
#3932 = LINE ( 'NONE', #94544, #80348 ) ;
#3933 = DIRECTION ( 'NONE',  ( -0.6830127018922181881, 0.6830127018922202975, -0.2588190451025214056 ) ) ;
#3934 = CARTESIAN_POINT ( 'NONE',  ( 8.999999999999937828, 7.931123077392104648, 4.000000000000000000 ) ) ;
#3935 = ORIENTED_EDGE ( 'NONE', *, *, #59123, .T. ) ;
#3936 = VERTEX_POINT ( 'NONE', #48719 ) ;
#3937 = CARTESIAN_POINT ( 'NONE',  ( 8.999999999999941380, -12.03360074219761700, 5.000000000000000000 ) ) ;
#3938 = DIRECTION ( 'NONE',  ( 0.7071067811865487940, 0.7071067811865463515, 0.000000000000000000 ) ) ;
#3939 = ORIENTED_EDGE ( 'NONE', *, *, #82209, .T. ) ;
#3940 = ADVANCED_FACE ( 'NONE', ( #59612 ), #137156, .F. ) ;
#3941 = SURFACE_SIDE_STYLE ('',( #68571 ) ) ;
#3942 = ORIENTED_EDGE ( 'NONE', *, *, #16365, .F. ) ;
#3943 = DIRECTION ( 'NONE',  ( 1.000000000000000000, 0.000000000000000000, 0.000000000000000000 ) ) ;
#3944 = LINE ( 'NONE', #92414, #114151 ) ;
#3945 = AXIS2_PLACEMENT_3D ( 'NONE', #126826, #22675, #34310 ) ;
#3946 = FACE_BOUND ( 'NONE', #24047, .T. ) ;
#3947 = EDGE_CURVE ( 'NONE', #139810, #88227, #106625, .T. ) ;
#3948 = CARTESIAN_POINT ( 'NONE',  ( -25.39999999999996305, 0.000000000000000000, 0.000000000000000000 ) ) ;
#3949 = FACE_OUTER_BOUND ( 'NONE', #8694, .T. ) ;
#3950 = CARTESIAN_POINT ( 'NONE',  ( 0.000000000000000000, 0.000000000000000000, 5.000000000000000000 ) ) ;
#3951 = CARTESIAN_POINT ( 'NONE',  ( -66.48921356237309510, -27.52281430457101763, 5.000000000000000000 ) ) ;
#3952 = AXIS2_PLACEMENT_3D ( 'NONE', #100993, #77832, #111887 ) ;
#3954 = VECTOR ( 'NONE', #135042, 1000.000000000000227 ) ;
#3953 = AXIS2_PLACEMENT_3D ( 'NONE', #130436, #31126, #32544 ) ;
#3955 = ORIENTED_EDGE ( 'NONE', *, *, #15196, .T. ) ;
#3956 = AXIS2_PLACEMENT_3D ( 'NONE', #136991, #46456, #103618 ) ;
#3957 = ORIENTED_EDGE ( 'NONE', *, *, #115566, .T. ) ;
#3958 = CARTESIAN_POINT ( 'NONE',  ( 90.47459685856479439, 1.637169565754164280, -6.109999999999996767 ) ) ;
#3959 = VERTEX_POINT ( 'NONE', #83498 ) ;
#3960 = LINE ( 'NONE', #123687, #35079 ) ;
#3961 = VECTOR ( 'NONE', #18954, 999.9999999999998863 ) ;
#3962 = CARTESIAN_POINT ( 'NONE',  ( -51.48921356237309510, -27.52281430457091460, 5.000000000000000000 ) ) ;
#3963 = DIRECTION ( 'NONE',  ( 0.3543493200069162685, -0.000000000000000000, -0.9351131265310288487 ) ) ;
#3964 = ORIENTED_EDGE ( 'NONE', *, *, #68959, .F. ) ;
#3965 = FACE_OUTER_BOUND ( 'NONE', #119508, .T. ) ;
#3966 =( NAMED_UNIT ( * ) SI_UNIT ( $, .STERADIAN. ) SOLID_ANGLE_UNIT ( ) );
#3968 = LINE ( 'NONE', #69303, #17275 ) ;
#3967 = CARTESIAN_POINT ( 'NONE',  ( 67.79166666666667140, 3.975000000000003642, -6.884901960086285300 ) ) ;
#3969 = DIRECTION ( 'NONE',  ( -0.000000000000000000, -0.3543493200069152693, 0.9351131265310292928 ) ) ;
#3970 = PLANE ( 'NONE',  #72259 ) ;
#3971 = VERTEX_POINT ( 'NONE', #95051 ) ;
#3972 = CARTESIAN_POINT ( 'NONE',  ( 4.198949119135569656E-17, -1.320799999999990870, 4.000000000000000000 ) ) ;
#3973 = CARTESIAN_POINT ( 'NONE',  ( 12.29974487139158512, -27.71228299555214747, 4.000000000000000000 ) ) ;
#3974 = ORIENTED_EDGE ( 'NONE', *, *, #100908, .F. ) ;
#3975 = ORIENTED_EDGE ( 'NONE', *, *, #136004, .F. ) ;
#3976 = ORIENTED_EDGE ( 'NONE', *, *, #113381, .F. ) ;
#3977 = CARTESIAN_POINT ( 'NONE',  ( 42.58376352523143993, -6.110000000000001208, -3.741295971395164515E-16 ) ) ;
#3978 = VECTOR ( 'NONE', #102503, 1000.000000000000000 ) ;
#3979 = ORIENTED_EDGE ( 'NONE', *, *, #79015, .T. ) ;
#3980 = EDGE_CURVE ( 'NONE', #95449, #98838, #35803, .T. ) ;
#3981 = PRESENTATION_LAYER_ASSIGNMENT (  '', '', ( #66572 ) ) ;
#3982 = CARTESIAN_POINT ( 'NONE',  ( 10.25413961620377457, 3.047499999999993214, -5.278424836066146320 ) ) ;
#3983 = CARTESIAN_POINT ( 'NONE',  ( -19.28515664589288647, 1.196650378695323758, -30.59010235425024860 ) ) ;
#3984 = EDGE_LOOP ( 'NONE', ( #27200, #68259, #9378, #62061 ) ) ;
#3985 = EDGE_CURVE ( 'NONE', #19842, #22107, #71925, .T. ) ;
#3986 = CARTESIAN_POINT ( 'NONE',  ( 16.76840764549667639, 0.000000000000000000, 2.500000000000001332 ) ) ;
#3988 = ORIENTED_EDGE ( 'NONE', *, *, #120443, .T. ) ;
#3987 = EDGE_CURVE ( 'NONE', #73784, #105152, #72657, .T. ) ;
#3989 = PLANE ( 'NONE',  #139044 ) ;
#3990 = AXIS2_PLACEMENT_3D ( 'NONE', #141080, #8396, #64257 ) ;
#3991 = CARTESIAN_POINT ( 'NONE',  ( 15.29974487139158867, -27.71228299555216879, 4.000000000000000000 ) ) ;
#3993 = ORIENTED_EDGE ( 'NONE', *, *, #141672, .F. ) ;
#3992 = PLANE ( 'NONE',  #97974 ) ;
#3994 = VERTEX_POINT ( 'NONE', #40700 ) ;
#3995 = EDGE_CURVE ( 'NONE', #24646, #76671, #16791, .T. ) ;
#3996 = PLANE ( 'NONE',  #113983 ) ;
#3997 = CARTESIAN_POINT ( 'NONE',  ( 29.99999999999979750, 11.96639925780214320, 5.000000000000000000 ) ) ;
#3998 = ORIENTED_EDGE ( 'NONE', *, *, #134154, .T. ) ;
#3999 = DIRECTION ( 'NONE',  ( 0.000000000000000000, 0.000000000000000000, -1.000000000000000000 ) ) ;
#4000 = ORIENTED_EDGE ( 'NONE', *, *, #123003, .T. ) ;
#4001 = ORIENTED_EDGE ( 'NONE', *, *, #5014, .F. ) ;
#4002 = VERTEX_POINT ( 'NONE', #76181 ) ;
#4003 = ORIENTED_EDGE ( 'NONE', *, *, #128318, .T. ) ;
#4004 = VECTOR ( 'NONE', #26767, 1000.000000000000000 ) ;
#4005 = SURFACE_STYLE_USAGE ( .BOTH. , #25818 ) ;
#4006 = EDGE_CURVE ( 'NONE', #16006, #7225, #120343, .T. ) ;
#4007 = CARTESIAN_POINT ( 'NONE',  ( -6.722509707016169678, 22.22500000000000142, 15.68697783646059918 ) ) ;
#4008 = CARTESIAN_POINT ( 'NONE',  ( -50.99451991528749062, 28.92564299267973738, 4.000000000000000000 ) ) ;
#4009 = EDGE_CURVE ( 'NONE', #42725, #118417, #131995, .T. ) ;
#4010 = FACE_OUTER_BOUND ( 'NONE', #38579, .T. ) ;
#4011 = ORIENTED_EDGE ( 'NONE', *, *, #127323, .T. ) ;
#4012 = LINE ( 'NONE', #67198, #7917 ) ;
#4013 = EDGE_CURVE ( 'NONE', #140226, #13056, #3047, .T. ) ;
#4014 = CARTESIAN_POINT ( 'NONE',  ( 18.35373647476854941, -5.808823158059035485, -5.808823158059033709 ) ) ;
#4015 = FACE_OUTER_BOUND ( 'NONE', #87948, .T. ) ;
#4016 = CARTESIAN_POINT ( 'NONE',  ( -7.362461875838964609, 22.22500000000000142, 4.000000000000000000 ) ) ;
#4017 = VECTOR ( 'NONE', #106508, 1000.000000000000227 ) ;
#4018 = CARTESIAN_POINT ( 'NONE',  ( -54.18398860626899705, 28.73617430169825226, 5.000000000000000000 ) ) ;
#4019 = ORIENTED_EDGE ( 'NONE', *, *, #92997, .T. ) ;
#4020 = ORIENTED_EDGE ( 'NONE', *, *, #299, .T. ) ;
#4021 = VERTEX_POINT ( 'NONE', #118221 ) ;
#4022 = DIRECTION ( 'NONE',  ( -0.000000000000000000, 0.000000000000000000, 1.000000000000000000 ) ) ;
#4023 = LINE ( 'NONE', #16355, #125165 ) ;
#4024 = ADVANCED_FACE ( 'NONE', ( #8031 ), #52271, .T. ) ;
#4025 = CARTESIAN_POINT ( 'NONE',  ( 3.489213562373097322, -27.52281430457057709, 5.000000000000000000 ) ) ;
#4026 = DIRECTION ( 'NONE',  ( -0.000000000000000000, 0.000000000000000000, 1.000000000000000000 ) ) ;
#4027 = DIRECTION ( 'NONE',  ( 0.7071067811865486830, -0.7071067811865464625, -0.000000000000000000 ) ) ;
#4028 = DIRECTION ( 'NONE',  ( -0.3543493200069162685, -0.000000000000000000, -0.9351131265310288487 ) ) ;
#4029 = CARTESIAN_POINT ( 'NONE',  ( -10.21498419724184004, -3.740707523384238176, 15.76143240460121575 ) ) ;
#4030 = CARTESIAN_POINT ( 'NONE',  ( 27.99507522778789692, -5.240707523384221744, 12.38332538355489731 ) ) ;
#4031 = LINE ( 'NONE', #80957, #77330 ) ;
#4032 = LINE ( 'NONE', #91133, #67550 ) ;
#4033 = EDGE_CURVE ( 'NONE', #95860, #31073, #129838, .T. ) ;
#4034 = ORIENTED_EDGE ( 'NONE', *, *, #67685, .T. ) ;
#4035 = CARTESIAN_POINT ( 'NONE',  ( 16.85424587240084904, -0.3099398835762542936, -34.40694344753310929 ) ) ;
#4036 = ORIENTED_EDGE ( 'NONE', *, *, #50050, .F. ) ;
#4037 = VECTOR ( 'NONE', #138155, 999.9999999999998863 ) ;
#4038 = LINE ( 'NONE', #57802, #4270 ) ;
#4040 = VERTEX_POINT ( 'NONE', #52967 ) ;
#4039 = LINE ( 'NONE', #100575, #92764 ) ;
#4041 = VECTOR ( 'NONE', #92420, 1000.000000000000114 ) ;
#4042 = LINE ( 'NONE', #94665, #62555 ) ;
#4043 = DIRECTION ( 'NONE',  ( -0.000000000000000000, 0.3543493200069153248, 0.9351131265310292928 ) ) ;
#4044 = ORIENTED_EDGE ( 'NONE', *, *, #138609, .F. ) ;
#4045 = DIRECTION ( 'NONE',  ( -1.000000000000000000, -1.224606353822377258E-16, -0.000000000000000000 ) ) ;
#4046 = VERTEX_POINT ( 'NONE', #141430 ) ;
#4047 =( NAMED_UNIT ( * ) SI_UNIT ( $, .STERADIAN. ) SOLID_ANGLE_UNIT ( ) );
#4048 = ORIENTED_EDGE ( 'NONE', *, *, #104810, .T. ) ;
#4049 = VECTOR ( 'NONE', #94759, 1000.000000000000000 ) ;
#4050 = PRESENTATION_LAYER_ASSIGNMENT (  '', '', ( #103637 ) ) ;
#4051 = FACE_OUTER_BOUND ( 'NONE', #35684, .T. ) ;
#4052 = ADVANCED_FACE ( 'NONE', ( #42141 ), #86352, .F. ) ;
#4053 = CARTESIAN_POINT ( 'NONE',  ( 100.5583603837962272, -7.949999999999997513, -2.130196079827425759 ) ) ;
#4054 = DIRECTION ( 'NONE',  ( -0.7071067811865486830, -0.7071067811865464625, 0.000000000000000000 ) ) ;
#4055 = DIRECTION ( 'NONE',  ( -0.7071067811865487940, 0.7071067811865463515, -0.000000000000000000 ) ) ;
#4056 = VERTEX_POINT ( 'NONE', #42852 ) ;
#4057 = LINE ( 'NONE', #15662, #116322 ) ;
#4058 = LINE ( 'NONE', #92533, #21797 ) ;
#4059 = EDGE_CURVE ( 'NONE', #92120, #12987, #87050, .T. ) ;
#4060 = LINE ( 'NONE', #38898, #103975 ) ;
#4061 = CARTESIAN_POINT ( 'NONE',  ( 20.12500000000000000, 6.094999999999989981, -1.119633336120465690E-15 ) ) ;
#4062 = CARTESIAN_POINT ( 'NONE',  ( 22.82816939922336985, -2.240707523384260824, 4.000000000000000000 ) ) ;
#4063 = ORIENTED_EDGE ( 'NONE', *, *, #52192, .F. ) ;
#4064 = DIRECTION ( 'NONE',  ( 0.000000000000000000, 0.000000000000000000, 1.000000000000000000 ) ) ;
#4065 = ORIENTED_EDGE ( 'NONE', *, *, #38338, .F. ) ;
#4066 = EDGE_CURVE ( 'NONE', #109845, #65462, #56615, .T. ) ;
#4067 = CARTESIAN_POINT ( 'NONE',  ( 95.66709685856477563, -3.055000000000000160, -5.291415217122921177 ) ) ;
#4068 = CARTESIAN_POINT ( 'NONE',  ( -63.18398860626900415, 28.73617430169831621, 5.000000000000000000 ) ) ;
#4069 = CARTESIAN_POINT ( 'NONE',  ( 10.17183060077640100, 12.75929247661558819, 4.000000000000000000 ) ) ;
#4070 = DIRECTION ( 'NONE',  ( 0.7071067811865487940, 0.7071067811865463515, 0.000000000000000000 ) ) ;
#4071 = CARTESIAN_POINT ( 'NONE',  ( -31.49999999999977973, 12.05218569542904383, 5.000000000000000000 ) ) ;
#4072 = VERTEX_POINT ( 'NONE', #78322 ) ;
#4073 = CARTESIAN_POINT ( 'NONE',  ( 2.282422613574298431, -21.73023691814492508, 5.000000000000000888 ) ) ;
#4074 = DIRECTION ( 'NONE',  ( -1.000000000000000000, -1.224606353822377258E-16, -0.000000000000000000 ) ) ;
#4075 = VERTEX_POINT ( 'NONE', #23183 ) ;
#4076 = CARTESIAN_POINT ( 'NONE',  ( 1.499999999999994449, 0.4311230773921780335, 4.000000000000000000 ) ) ;
#4077 = EDGE_CURVE ( 'NONE', #115305, #86507, #101481, .T. ) ;
#4078 = LINE ( 'NONE', #14301, #35635 ) ;
#4080 = ORIENTED_EDGE ( 'NONE', *, *, #128523, .T. ) ;
#4079 = LINE ( 'NONE', #2701, #98374 ) ;
#4082 = AXIS2_PLACEMENT_3D ( 'NONE', #42213, #88572, #102303 ) ;
#4081 = PLANE ( 'NONE',  #122392 ) ;
#4083 = CARTESIAN_POINT ( 'NONE',  ( 26.99999999999981526, -3.033600742197705369, 5.000000000000000000 ) ) ;
#4084 = CARTESIAN_POINT ( 'NONE',  ( 21.48921356237309155, -27.52281430457070499, 5.000000000000000000 ) ) ;
#4085 = CARTESIAN_POINT ( 'NONE',  ( -6.489213562373093325, -27.52281430457059841, 5.000000000000000000 ) ) ;
#4086 = EDGE_LOOP ( 'NONE', ( #790, #100349, #114558, #107282 ) ) ;
#4087 = VERTEX_POINT ( 'NONE', #91357 ) ;
#4088 = ORIENTED_EDGE ( 'NONE', *, *, #61253, .F. ) ;
#4089 = CARTESIAN_POINT ( 'NONE',  ( 87.20876352523143282, -7.482591942790329030E-16, 6.110000000000001208 ) ) ;
#4090 = ORIENTED_EDGE ( 'NONE', *, *, #66742, .F. ) ;
#4091 = CARTESIAN_POINT ( 'NONE',  ( 34.00193056682073944, -22.22500000000000142, 4.500000000000000888 ) ) ;
#4092 = DIRECTION ( 'NONE',  ( -0.000000000000000000, -1.000000000000000000, -0.000000000000000000 ) ) ;
#4093 = LINE ( 'NONE', #138972, #108189 ) ;
#4094 = DIRECTION ( 'NONE',  ( 0.6830127018922181881, 0.6830127018922202975, -0.2588190451025214056 ) ) ;
#4095 = ORIENTED_EDGE ( 'NONE', *, *, #130697, .F. ) ;
#4096 = CARTESIAN_POINT ( 'NONE',  ( 14.14114973822191423, 6.572112357556697759, 4.331981551378865092 ) ) ;
#4097 = CARTESIAN_POINT ( 'NONE',  ( -54.18398860626899705, 28.73617430169825226, 5.000000000000000000 ) ) ;
#4098 = CARTESIAN_POINT ( 'NONE',  ( 73.26626352523143737, 4.472830434245839371, -4.472830434245838482 ) ) ;
#4099 = ORIENTED_EDGE ( 'NONE', *, *, #119713, .T. ) ;
#4100 = EDGE_CURVE ( 'NONE', #7339, #93773, #132732, .T. ) ;
#4101 = DIRECTION ( 'NONE',  ( -0.5735764363510501562, 0.8191520442889890230, 1.003171929053521419E-16 ) ) ;
#4102 = CARTESIAN_POINT ( 'NONE',  ( 17.20710678118642178, -8.240707523384195099, 5.000000000000000000 ) ) ;
#4103 = VERTEX_POINT ( 'NONE', #67471 ) ;
#4104 = ORIENTED_EDGE ( 'NONE', *, *, #109273, .T. ) ;
#4105 = EDGE_CURVE ( 'NONE', #84436, #129923, #65432, .T. ) ;
#4106 = DIRECTION ( 'NONE',  ( 1.000000000000000000, 0.000000000000000000, 0.000000000000000000 ) ) ;
#4107 = ADVANCED_FACE ( 'NONE', ( #90635 ), #36248, .F. ) ;
#4108 = DIRECTION ( 'NONE',  ( -0.7071067811865487940, 0.7071067811865463515, -0.000000000000000000 ) ) ;
#4109 = PLANE ( 'NONE',  #36982 ) ;
#4110 = CARTESIAN_POINT ( 'NONE',  ( 51.18398860626899705, 28.73617430169823095, 5.000000000000000000 ) ) ;
#4111 = FILL_AREA_STYLE_COLOUR ( '', #91954 ) ;
#4112 = CARTESIAN_POINT ( 'NONE',  ( 3.291777089830458358, -15.74070752338412404, 19.73771281079098472 ) ) ;
#4113 = LINE ( 'NONE', #6268, #136808 ) ;
#4114 = ORIENTED_EDGE ( 'NONE', *, *, #63185, .F. ) ;
#4115 = VECTOR ( 'NONE', #61154, 999.9999999999998863 ) ;
#4116 = VERTEX_POINT ( 'NONE', #14483 ) ;
#4117 = DIRECTION ( 'NONE',  ( -0.5735764363510499342, -0.8191520442889891340, 0.000000000000000000 ) ) ;
#4118 = VERTEX_POINT ( 'NONE', #45718 ) ;
#4119 = ADVANCED_FACE ( 'NONE', ( #11589 ), #134135, .F. ) ;
#4120 = CARTESIAN_POINT ( 'NONE',  ( 66.29974487139159578, -27.71228299555252406, 4.000000000000000000 ) ) ;
#4121 = ORIENTED_EDGE ( 'NONE', *, *, #134231, .T. ) ;
#4122 = CARTESIAN_POINT ( 'NONE',  ( 69.35002705046288440, -5.819803920172573086, -5.819803920172573086 ) ) ;
#4123 = DIRECTION ( 'NONE',  ( -0.000000000000000000, -0.3543493200069152693, 0.9351131265310292928 ) ) ;
#4124 = CARTESIAN_POINT ( 'NONE',  ( -34.49999999999976552, 18.05432934483075513, 4.994342998332167660 ) ) ;
#4125 = VECTOR ( 'NONE', #42433, 999.9999999999998863 ) ;
#4126 = DIRECTION ( 'NONE',  ( 0.6830127018922181881, 0.6830127018922202975, -0.2588190451025214056 ) ) ;
#4127 = EDGE_LOOP ( 'NONE', ( #53914, #3819, #40808, #17412 ) ) ;
#4128 = CARTESIAN_POINT ( 'NONE',  ( -16.95484226663322858, -21.74070752338405299, 21.72585301388580703 ) ) ;
#4129 = DIRECTION ( 'NONE',  ( -1.000000000000000000, 0.000000000000000000, 0.000000000000000000 ) ) ;
#4130 = VECTOR ( 'NONE', #122756, 1000.000000000000000 ) ;
#4131 = ORIENTED_EDGE ( 'NONE', *, *, #26668, .F. ) ;
#4132 = LINE ( 'NONE', #49874, #103733 ) ;
#4133 = VERTEX_POINT ( 'NONE', #123273 ) ;
#4134 = ORIENTED_EDGE ( 'NONE', *, *, #134870, .F. ) ;
#4135 = DIRECTION ( 'NONE',  ( 0.7071067811865487940, 0.7071067811865463515, 0.000000000000000000 ) ) ;
#4136 = VERTEX_POINT ( 'NONE', #58028 ) ;
#4137 = ORIENTED_EDGE ( 'NONE', *, *, #54109, .T. ) ;
#4138 = CARTESIAN_POINT ( 'NONE',  ( 77.58376352523144703, -6.110000000000001208, -3.741295971395164515E-16 ) ) ;
#4139 = AXIS2_PLACEMENT_3D ( 'NONE', #52002, #89435, #141888 ) ;
#4140 = ORIENTED_EDGE ( 'NONE', *, *, #124875, .F. ) ;
#4141 = AXIS2_PLACEMENT_3D ( 'NONE', #55758, #44163, #88387 ) ;
#4142 = DIRECTION ( 'NONE',  ( -2.781805975412905890E-17, 0.3543493200069152693, 0.9351131265310292928 ) ) ;
#4143 = EDGE_CURVE ( 'NONE', #107270, #38431, #102229, .T. ) ;
#4144 = FACE_OUTER_BOUND ( 'NONE', #102604, .T. ) ;
#4145 = CARTESIAN_POINT ( 'NONE',  ( 122.6462635252314328, -4.472830434245840259, 4.472830434245838482 ) ) ;
#4146 = DIRECTION ( 'NONE',  ( 0.7071067811865487940, 0.7071067811865463515, 0.000000000000000000 ) ) ;
#4147 = ADVANCED_FACE ( 'NONE', ( #92736 ), #28926, .F. ) ;
#4148 = CARTESIAN_POINT ( 'NONE',  ( 17.99999999999986855, 9.631307414974335401, -9.079085613539497501 ) ) ;
#4149 = LINE ( 'NONE', #79702, #139345 ) ;
#4150 = DIRECTION ( 'NONE',  ( -0.3543493200069163240, 0.000000000000000000, 0.9351131265310288487 ) ) ;
#4151 = CARTESIAN_POINT ( 'NONE',  ( -34.92500000000001137, 22.22500000000000142, 4.000000000000000000 ) ) ;
#4152 = EDGE_CURVE ( 'NONE', #46538, #126680, #106441, .T. ) ;
#4153 = ADVANCED_FACE ( 'NONE', ( #94164 ), #139130, .F. ) ;
#4154 = DIRECTION ( 'NONE',  ( -0.000000000000000000, -0.3543493200069152693, 0.9351131265310292928 ) ) ;
#4155 = ORIENTED_EDGE ( 'NONE', *, *, #21425, .T. ) ;
#4156 = SURFACE_STYLE_USAGE ( .BOTH. , #17921 ) ;
#4157 = CARTESIAN_POINT ( 'NONE',  ( 2.816011393730999401, 28.73617430169785436, 5.000000000000000000 ) ) ;
#4158 = ORIENTED_EDGE ( 'NONE', *, *, #4681, .F. ) ;
#4159 = EDGE_LOOP ( 'NONE', ( #49526, #92374, #127745, #134673, #20295 ) ) ;
#4160 = DIRECTION ( 'NONE',  ( 0.7071067811865487940, 0.7071067811865463515, -0.000000000000000000 ) ) ;
#4161 = ORIENTED_EDGE ( 'NONE', *, *, #7495, .F. ) ;
#4162 = VECTOR ( 'NONE', #37637, 1000.000000000000000 ) ;
#4163 = FACE_OUTER_BOUND ( 'NONE', #52087, .T. ) ;
#4164 = CARTESIAN_POINT ( 'NONE',  ( 21.15294044719737698, 3.821174125832445049E-16, 0.000000000000000000 ) ) ;
#4165 = EDGE_CURVE ( 'NONE', #60444, #125103, #38380, .T. ) ;
#4166 = CARTESIAN_POINT ( 'NONE',  ( 29.99451991528749417, 28.92564299267958816, 4.000000000000000000 ) ) ;
#4167 = ADVANCED_FACE ( 'NONE', ( #93472 ), #15854, .F. ) ;
#4168 = CARTESIAN_POINT ( 'NONE',  ( -48.18398860626899705, 28.73617430169820608, 5.000000000000000000 ) ) ;
#4169 = EDGE_LOOP ( 'NONE', ( #88080, #119651, #87715, #129237 ) ) ;
#4170 = DIRECTION ( 'NONE',  ( -0.7071067811865486830, -0.7071067811865464625, -0.000000000000000000 ) ) ;
#4171 = ORIENTED_EDGE ( 'NONE', *, *, #40357, .T. ) ;
#4172 = DIRECTION ( 'NONE',  ( -0.000000000000000000, -0.3543493200069152693, 0.9351131265310292928 ) ) ;
#4173 = ADVANCED_FACE ( 'NONE', ( #70343 ), #114489, .F. ) ;
#4174 = CARTESIAN_POINT ( 'NONE',  ( 23.98373647476855197, -5.808823158059035485, -5.808823158059033709 ) ) ;
#4175 = ADVANCED_FACE ( 'NONE', ( #4243 ), #81924, .T. ) ;
#4176 = DIRECTION ( 'NONE',  ( 0.7071067811865486830, -0.7071067811865464625, -0.000000000000000000 ) ) ;
#4177 = PLANE ( 'NONE',  #65164 ) ;
#4178 = ORIENTED_EDGE ( 'NONE', *, *, #54914, .T. ) ;
#4179 = EDGE_LOOP ( 'NONE', ( #14215, #46831, #63893, #116608 ) ) ;
#4180 = ORIENTED_EDGE ( 'NONE', *, *, #39223, .F. ) ;
#4181 = CARTESIAN_POINT ( 'NONE',  ( -26.20710678118635428, 3.759292476615680112, 5.000000000000000000 ) ) ;
#4182 = DIRECTION ( 'NONE',  ( -1.000000000000000000, -0.000000000000000000, -0.000000000000000000 ) ) ;
#4183 = EDGE_CURVE ( 'NONE', #81752, #61225, #5714, .T. ) ;
#4185 = VECTOR ( 'NONE', #52864, 1000.000000000000000 ) ;
#4184 = DIRECTION ( 'NONE',  ( -0.7071067811865486830, -0.7071067811865464625, 0.000000000000000000 ) ) ;
#4186 = CARTESIAN_POINT ( 'NONE',  ( 10.15640092694706453, 2.500000000000000444, 3.061616997868383634E-16 ) ) ;
#4187 = VERTEX_POINT ( 'NONE', #96041 ) ;
#4188 = LINE ( 'NONE', #36194, #37008 ) ;
#4189 = VECTOR ( 'NONE', #4740, 1000.000000000000000 ) ;
#4190 = CARTESIAN_POINT ( 'NONE',  ( -3.469446951953614189E-15, -1.068876922607807645, 4.000000000000000000 ) ) ;
#4191 = CARTESIAN_POINT ( 'NONE',  ( -3.489213562373097322, -27.52281430457057709, 5.000000000000000000 ) ) ;
#4192 = VERTEX_POINT ( 'NONE', #140280 ) ;
#4193 = LINE ( 'NONE', #27424, #134414 ) ;
#4194 = EDGE_CURVE ( 'NONE', #105497, #47322, #128685, .T. ) ;
#4195 = FACE_OUTER_BOUND ( 'NONE', #93538, .T. ) ;
#4196 = ORIENTED_EDGE ( 'NONE', *, *, #34004, .T. ) ;
#4198 = ORIENTED_EDGE ( 'NONE', *, *, #110254, .F. ) ;
#4197 = FILL_AREA_STYLE_COLOUR ( '', #16370 ) ;
#4199 = VERTEX_POINT ( 'NONE', #49729 ) ;
#4200 = CARTESIAN_POINT ( 'NONE',  ( 36.18398860626899705, 28.73617430169812437, 5.000000000000000000 ) ) ;
#4201 = ADVANCED_FACE ( 'NONE', ( #19904 ), #38827, .F. ) ;
#4202 = CARTESIAN_POINT ( 'NONE',  ( -28.77325839282149289, -11.24070752338416845, 18.24660765846975963 ) ) ;
#4204 = EDGE_CURVE ( 'NONE', #138815, #49616, #83786, .T. ) ;
#4203 = CARTESIAN_POINT ( 'NONE',  ( -45.48921356237309510, -27.52281430457087197, 5.000000000000000000 ) ) ;
#4205 = ORIENTED_EDGE ( 'NONE', *, *, #123667, .T. ) ;
#4206 = CARTESIAN_POINT ( 'NONE',  ( 7.499999999999951150, -10.04351517176477948, -1.623559851933805698 ) ) ;
#4207 = UNCERTAINTY_MEASURE_WITH_UNIT (LENGTH_MEASURE( 1.000000000000000082E-05 ), #53487, 'distance_accuracy_value', 'NONE');
#4208 = ORIENTED_EDGE ( 'NONE', *, *, #83296, .F. ) ;
#4209 = DIRECTION ( 'NONE',  ( 0.7071067811865486830, -0.7071067811865464625, -0.000000000000000000 ) ) ;
#4210 = CARTESIAN_POINT ( 'NONE',  ( 6.668467411598530070, -18.74070752338408496, 20.73178291233842430 ) ) ;
#4211 = ADVANCED_FACE ( 'NONE', ( #19209 ), #72212, .T. ) ;
#4212 = CARTESIAN_POINT ( 'NONE',  ( 128.4125270504628986, -7.949999999999998401, -4.867971026610728450E-16 ) ) ;
#4213 = CARTESIAN_POINT ( 'NONE',  ( -24.69326993309583429, -3.740707523384241728, 12.88036043432873257 ) ) ;
#4214 = CARTESIAN_POINT ( 'NONE',  ( 48.78752705046289151, 0.000000000000000000, -7.949999999999998401 ) ) ;
#4215 = DIRECTION ( 'NONE',  ( -1.000000000000000000, -1.224606353822377258E-16, -0.000000000000000000 ) ) ;
#4216 = FACE_OUTER_BOUND ( 'NONE', #132647, .T. ) ;
#4217 = CARTESIAN_POINT ( 'NONE',  ( 24.39999999999999858, -2.599999999999900169, -1.445354724476153568E-14 ) ) ;
#4218 = CARTESIAN_POINT ( 'NONE',  ( 30.31206980810188512, 7.934999999999993392, 2.126176841940951689 ) ) ;
#4219 = LINE ( 'NONE', #47843, #99999 ) ;
#4220 = CARTESIAN_POINT ( 'NONE',  ( 15.21247294953710671, 0.000000000000000000, 6.094999999999989981 ) ) ;
#4221 = PLANE ( 'NONE',  #97560 ) ;
#4222 = PLANE ( 'NONE',  #33850 ) ;
#4223 = EDGE_LOOP ( 'NONE', ( #99920, #142610, #110916, #116699 ) ) ;
#4224 = ORIENTED_EDGE ( 'NONE', *, *, #5775, .T. ) ;
#4225 = CARTESIAN_POINT ( 'NONE',  ( 95.20833333333334281, -3.974999999999999201, -6.884901960086287964 ) ) ;
#4226 = ORIENTED_EDGE ( 'NONE', *, *, #50412, .F. ) ;
#4227 = ORIENTED_EDGE ( 'NONE', *, *, #131620, .F. ) ;
#4228 = FILL_AREA_STYLE_COLOUR ( '', #87383 ) ;
#4229 = CARTESIAN_POINT ( 'NONE',  ( -27.18398860626900060, 28.73617430169806042, 5.000000000000000000 ) ) ;
#4230 = CARTESIAN_POINT ( 'NONE',  ( 14.69272197276067438, 9.496641765041323069, -0.2911197889769509550 ) ) ;
#4231 = ORIENTED_EDGE ( 'NONE', *, *, #106630, .T. ) ;
#4232 = MECHANICAL_DESIGN_GEOMETRIC_PRESENTATION_REPRESENTATION (  '', ( #34422 ), #124659 ) ;
#4233 = CIRCLE ( 'NONE', #22685, 2.500000000000000888 ) ;
#4235 = DIRECTION ( 'NONE',  ( -0.7071067811865486830, -0.7071067811865464625, -0.000000000000000000 ) ) ;
#4234 = VECTOR ( 'NONE', #60382, 1000.000000000000000 ) ;
#4236 = LINE ( 'NONE', #59443, #108950 ) ;
#4237 = COLOUR_RGB ( '', 0.09019608, 0.27058824, 0.51372549) ;
#4238 = DIRECTION ( 'NONE',  ( -0.3543493200069162685, -0.000000000000000000, -0.9351131265310288487 ) ) ;
#4239 = CARTESIAN_POINT ( 'NONE',  ( 125.6139270598129229, -2.020146860515199094, -7.575422191809951578 ) ) ;
#4240 = AXIS2_PLACEMENT_3D ( 'NONE', #95538, #83253, #29563 ) ;
#4241 = PLANE ( 'NONE',  #97905 ) ;
#4242 = CARTESIAN_POINT ( 'NONE',  ( 45.48921356237309510, -27.52281430457087197, 5.000000000000000000 ) ) ;
#4243 = FACE_OUTER_BOUND ( 'NONE', #51956, .T. ) ;
#4245 = CARTESIAN_POINT ( 'NONE',  ( 16.31507112947232230, 22.22500000000000142, -14.41677840540084254 ) ) ;
#4244 = VECTOR ( 'NONE', #24717, 999.9999999999998863 ) ;
#4246 = DIRECTION ( 'NONE',  ( 0.7071067811865486830, -0.7071067811865464625, -0.000000000000000000 ) ) ;
#4247 = DIRECTION ( 'NONE',  ( 0.6830127018922181881, 0.6830127018922202975, -0.2588190451025214056 ) ) ;
#4248 = VECTOR ( 'NONE', #124314, 1000.000000000000227 ) ;
#4249 = CARTESIAN_POINT ( 'NONE',  ( 13.17183060077637613, -11.24070752338416668, 4.000000000000000000 ) ) ;
#4250 = LINE ( 'NONE', #69616, #100066 ) ;
#4251 = EDGE_LOOP ( 'NONE', ( #13017, #99300, #14901, #42051 ) ) ;
#4252 = VERTEX_POINT ( 'NONE', #127241 ) ;
#4253 = CARTESIAN_POINT ( 'NONE',  ( 115.3545968585647614, -1.637169565754161615, 6.110000000000000320 ) ) ;
#4254 = ORIENTED_EDGE ( 'NONE', *, *, #4566, .F. ) ;
#4255 = ADVANCED_FACE ( 'NONE', ( #129382 ), #30069, .F. ) ;
#4256 = CARTESIAN_POINT ( 'NONE',  ( 13.82816939922343558, 18.75929247661552424, 4.000000000000000000 ) ) ;
#4257 = CONICAL_SURFACE ( 'NONE', #36705, 2.552699999999928693, 1.029744258676634772 ) ;
#4258 = LINE ( 'NONE', #68216, #122068 ) ;
#4259 = EDGE_LOOP ( 'NONE', ( #71090, #59683, #72791, #79294 ) ) ;
#4260 = DIRECTION ( 'NONE',  ( -1.000000000000000000, -1.224606353822377258E-16, -0.000000000000000000 ) ) ;
#4261 = FACE_OUTER_BOUND ( 'NONE', #136404, .T. ) ;
#4262 = VECTOR ( 'NONE', #133760, 1000.000000000000000 ) ;
#4263 = CARTESIAN_POINT ( 'NONE',  ( 108.9954301918981088, 5.291415217122916737, 3.055000000000001936 ) ) ;
#4264 = ORIENTED_EDGE ( 'NONE', *, *, #82601, .T. ) ;
#4265 = ORIENTED_EDGE ( 'NONE', *, *, #36449, .F. ) ;
#4266 = CARTESIAN_POINT ( 'NONE',  ( 1.199999999999999956, -0.6000000000000001998, 4.543283425070392845 ) ) ;
#4267 = FACE_OUTER_BOUND ( 'NONE', #27129, .T. ) ;
#4268 = LINE ( 'NONE', #104347, #40868 ) ;
#4269 = VECTOR ( 'NONE', #47698, 1000.000000000000227 ) ;
#4270 = VECTOR ( 'NONE', #92517, 1000.000000000000114 ) ;
#4271 = EDGE_LOOP ( 'NONE', ( #81073, #94967, #15577, #132278 ) ) ;
#4272 = ORIENTED_EDGE ( 'NONE', *, *, #35365, .F. ) ;
#4273 = EDGE_CURVE ( 'NONE', #103631, #117466, #41674, .T. ) ;
#4274 = ORIENTED_EDGE ( 'NONE', *, *, #20642, .F. ) ;
#4275 = DIRECTION ( 'NONE',  ( -0.7071067811865487940, 0.7071067811865463515, 0.000000000000000000 ) ) ;
#4276 = EDGE_CURVE ( 'NONE', #37184, #105472, #130125, .T. ) ;
#4277 = CARTESIAN_POINT ( 'NONE',  ( 3.275403141435219823, -2.126176841940958351, -7.934999999999988951 ) ) ;
#4278 =( LENGTH_UNIT ( ) NAMED_UNIT ( * ) SI_UNIT ( .MILLI., .METRE. ) );
#4279 = VERTEX_POINT ( 'NONE', #39557 ) ;
#4281 = ORIENTED_EDGE ( 'NONE', *, *, #121146, .F. ) ;
#4280 = EDGE_CURVE ( 'NONE', #87140, #131250, #73496, .T. ) ;
#4282 = LINE ( 'NONE', #115215, #10809 ) ;
#4283 = ORIENTED_EDGE ( 'NONE', *, *, #28653, .T. ) ;
#4284 = ORIENTED_EDGE ( 'NONE', *, *, #142424, .F. ) ;
#4285 = CIRCLE ( 'NONE', #64597, 2.552699999999990865 ) ;
#4286 = CARTESIAN_POINT ( 'NONE',  ( -27.79333936457828358, 21.75929247661549581, 4.998822639870701856 ) ) ;
#4287 = EDGE_CURVE ( 'NONE', #10814, #4770, #6145, .T. ) ;
#4288 = PLANE ( 'NONE',  #65190 ) ;
#4289 = ORIENTED_EDGE ( 'NONE', *, *, #77343, .F. ) ;
#4290 = LINE ( 'NONE', #28271, #101564 ) ;
#4291 = CARTESIAN_POINT ( 'NONE',  ( -14.51078643762690490, -27.52281430457045275, 5.000000000000000000 ) ) ;
#4292 = EDGE_CURVE ( 'NONE', #105516, #33114, #116381, .T. ) ;
#4293 = DIRECTION ( 'NONE',  ( -0.6830127018922181881, 0.6830127018922202975, -0.2588190451025214056 ) ) ;
#4294 = CARTESIAN_POINT ( 'NONE',  ( 11.01088028653940754, -22.02621442084248571, 4.990779571109220214 ) ) ;
#4295 = FACE_BOUND ( 'NONE', #134171, .T. ) ;
#4296 = ORIENTED_EDGE ( 'NONE', *, *, #117997, .T. ) ;
#4297 = LINE ( 'NONE', #92801, #36480 ) ;
#4298 = DIRECTION ( 'NONE',  ( -0.7071067811865486830, -0.7071067811865464625, 0.000000000000000000 ) ) ;
#4299 =( NAMED_UNIT ( * ) PLANE_ANGLE_UNIT ( ) SI_UNIT ( $, .RADIAN. ) );
#4300 = ORIENTED_EDGE ( 'NONE', *, *, #110869, .F. ) ;
#4301 = CARTESIAN_POINT ( 'NONE',  ( 30.29974487139158867, -27.71228299555227537, 4.000000000000000000 ) ) ;
#4302 = VERTEX_POINT ( 'NONE', #50423 ) ;
#4304 = ORIENTED_EDGE ( 'NONE', *, *, #31247, .T. ) ;
#4303 = ADVANCED_FACE ( 'NONE', ( #94608 ), #138863, .T. ) ;
#4305 = ORIENTED_EDGE ( 'NONE', *, *, #12597, .F. ) ;
#4306 = CARTESIAN_POINT ( 'NONE',  ( 35.20376352523143737, 6.109999999999998543, 1.122388791418548911E-15 ) ) ;
#4307 = ORIENTED_EDGE ( 'NONE', *, *, #110008, .F. ) ;
#4308 = CARTESIAN_POINT ( 'NONE',  ( 35.99451991528749772, 28.92564299267963079, 4.000000000000000000 ) ) ;
#4309 = CARTESIAN_POINT ( 'NONE',  ( 15.18398860626900237, 28.73617430169797871, 5.000000000000000000 ) ) ;
#4310 = CARTESIAN_POINT ( 'NONE',  ( -21.18398860626899349, 28.73617430169802134, 5.000000000000000000 ) ) ;
#4311 = EDGE_CURVE ( 'NONE', #79253, #5780, #8294, .T. ) ;
#4312 = ORIENTED_EDGE ( 'NONE', *, *, #76951, .F. ) ;
#4313 = DIRECTION ( 'NONE',  ( 0.7071067811865486830, -0.7071067811865464625, -0.000000000000000000 ) ) ;
#4314 = CARTESIAN_POINT ( 'NONE',  ( 69.18398860626899705, 28.73617430169835529, 5.000000000000000000 ) ) ;
#4315 = EDGE_CURVE ( 'NONE', #103174, #5826, #70929, .T. ) ;
#4316 = EDGE_CURVE ( 'NONE', #133459, #99209, #139598, .T. ) ;
#4317 =( NAMED_UNIT ( * ) SI_UNIT ( $, .STERADIAN. ) SOLID_ANGLE_UNIT ( ) );
#4318 = AXIS2_PLACEMENT_3D ( 'NONE', #118898, #85544, #74719 ) ;
#4319 = DIRECTION ( 'NONE',  ( 0.6830127018922180770, -0.6830127018922204085, -0.2588190451025213501 ) ) ;
#4320 = LINE ( 'NONE', #48624, #50576 ) ;
#4321 = PLANE ( 'NONE',  #79570 ) ;
#4322 = ORIENTED_EDGE ( 'NONE', *, *, #67245, .F. ) ;
#4323 = VERTEX_POINT ( 'NONE', #30825 ) ;
#4324 = COLOUR_RGB ( '', 0.66274510, 0.83137255, 0.94901961) ;
#4325 = VERTEX_POINT ( 'NONE', #52544 ) ;
#4326 = ORIENTED_EDGE ( 'NONE', *, *, #125652, .T. ) ;
#4327 = FILL_AREA_STYLE_COLOUR ( '', #10280 ) ;
#4328 = VECTOR ( 'NONE', #107666, 1000.000000000000227 ) ;
#4329 = ORIENTED_EDGE ( 'NONE', *, *, #33893, .F. ) ;
#4330 = EDGE_CURVE ( 'NONE', #81604, #92832, #75051, .T. ) ;
#4332 = ORIENTED_EDGE ( 'NONE', *, *, #14074, .F. ) ;
#4331 = CIRCLE ( 'NONE', #13596, 2.500000000000000444 ) ;
#4333 = LINE ( 'NONE', #36335, #42126 ) ;
#4334 = FACE_OUTER_BOUND ( 'NONE', #92913, .T. ) ;
#4335 = ADVANCED_FACE ( 'NONE', ( #89458 ), #22737, .F. ) ;
#4336 = ADVANCED_FACE ( 'NONE', ( #9744 ), #110473, .F. ) ;
#4337 = DIRECTION ( 'NONE',  ( -0.6830127018922180770, -0.6830127018922204085, -0.2588190451025213501 ) ) ;
#4338 = EDGE_LOOP ( 'NONE', ( #53119, #113201, #137774, #82378 ) ) ;
#4339 = CARTESIAN_POINT ( 'NONE',  ( 13.13598696172163116, 4.584330080086930965E-16, 0.000000000000000000 ) ) ;
#4341 = EDGE_LOOP ( 'NONE', ( #115221, #1741, #89023, #22914 ) ) ;
#4340 = VECTOR ( 'NONE', #113927, 1000.000000000000000 ) ;
#4342 = FACE_OUTER_BOUND ( 'NONE', #123688, .T. ) ;
#4343 = CARTESIAN_POINT ( 'NONE',  ( 15.48921356237309510, -27.52281430457066236, 5.000000000000000000 ) ) ;
#4344 = CARTESIAN_POINT ( 'NONE',  ( -0.9537635252314473622, -7.934999999999990727, 4.858786175617117713E-16 ) ) ;
#4345 = EDGE_LOOP ( 'NONE', ( #112899, #19970, #51704, #46723 ) ) ;
#4346 = CARTESIAN_POINT ( 'NONE',  ( 99.95376352523145158, -6.109999999999999432, -3.741295971395163529E-16 ) ) ;
#4347 =( BOUNDED_CURVE ( )  B_SPLINE_CURVE ( 2, ( #79809, #45732, #91370, #89902, #35579, #111675, #90650, #123986, #58776, #134147, #134884, #24648, #80489 ),
 .UNSPECIFIED., .F., .T. ) 
 B_SPLINE_CURVE_WITH_KNOTS ( ( 3, 2, 2, 2, 2, 2, 3 ),
 ( 0.2499999999999999445, 0.2527777777777777124, 0.2555555555555554803, 0.2583333333333333037, 0.2611111111111110716, 0.2638888888888888395, 0.2666666666666666075 ),
 .UNSPECIFIED. ) 
 CURVE ( )  GEOMETRIC_REPRESENTATION_ITEM ( )  RATIONAL_B_SPLINE_CURVE ( ( 1.000000000000000666, 0.9659258262890676461, 1.000000000000000000, 0.9659258262890683122, 1.000000000000000000, 0.9659258262890683122, 1.000000000000000000, 0.9659258262890683122, 1.000000000000000000, 0.9659258262890683122, 1.000000000000000000, 0.9659258262890689783, 0.9999999999999993339 ) ) 
 REPRESENTATION_ITEM ( '' )  );
#4348 = ADVANCED_FACE ( 'NONE', ( #77881 ), #44576, .F. ) ;
#4349 = CARTESIAN_POINT ( 'NONE',  ( -8.999999999999944933, -2.904428200921325143, -6.989807076074924019 ) ) ;
#4350 = DIRECTION ( 'NONE',  ( -0.7071067811865486830, 0.7071067811865464625, 0.000000000000000000 ) ) ;
#4351 = EDGE_LOOP ( 'NONE', ( #103833, #86726, #24032, #24093, #31848, #24286 ) ) ;
#4352 = ORIENTED_EDGE ( 'NONE', *, *, #81520, .F. ) ;
#4353 = EDGE_LOOP ( 'NONE', ( #81695, #43172, #9424, #135312 ) ) ;
#4354 = AXIS2_PLACEMENT_3D ( 'NONE', #111621, #70303, #47824 ) ;
#4355 =( NAMED_UNIT ( * ) SI_UNIT ( $, .STERADIAN. ) SOLID_ANGLE_UNIT ( ) );
#4356 = CARTESIAN_POINT ( 'NONE',  ( 39.18398860626899705, 28.73617430169814568, 5.000000000000000000 ) ) ;
#4357 = LINE ( 'NONE', #1992, #28863 ) ;
#4358 = EDGE_CURVE ( 'NONE', #94978, #13138, #1002, .T. ) ;
#4359 = FACE_OUTER_BOUND ( 'NONE', #98391, .T. ) ;
#4360 = SURFACE_SIDE_STYLE ('',( #15271 ) ) ;
#4361 = EDGE_LOOP ( 'NONE', ( #93428, #89119, #88624, #38765 ) ) ;
#4362 = FACE_OUTER_BOUND ( 'NONE', #126626, .T. ) ;
#4363 = LINE ( 'NONE', #80593, #4752 ) ;
#4364 = DIRECTION ( 'NONE',  ( -0.000000000000000000, 0.000000000000000000, 1.000000000000000000 ) ) ;
#4365 = ORIENTED_EDGE ( 'NONE', *, *, #81342, .T. ) ;
#4366 = PLANE ( 'NONE',  #102174 ) ;
#4367 = VECTOR ( 'NONE', #82975, 1000.000000000000000 ) ;
#4369 = VECTOR ( 'NONE', #85219, 1000.000000000000000 ) ;
#4368 = CARTESIAN_POINT ( 'NONE',  ( 24.48921356237309510, -27.52281430457072631, 5.000000000000000000 ) ) ;
#4370 = ORIENTED_EDGE ( 'NONE', *, *, #109635, .F. ) ;
#4372 = ORIENTED_EDGE ( 'NONE', *, *, #61857, .F. ) ;
#4371 = CARTESIAN_POINT ( 'NONE',  ( 2.999999999999988898, 20.96639925780204905, 5.000000000000000000 ) ) ;
#4373 = ORIENTED_EDGE ( 'NONE', *, *, #77923, .F. ) ;
#4374 = CARTESIAN_POINT ( 'NONE',  ( -18.46799460936313864, 3.072550929180732471, -30.05020605058495065 ) ) ;
#4375 = VECTOR ( 'NONE', #37484, 1000.000000000000000 ) ;
#4376 = CARTESIAN_POINT ( 'NONE',  ( -11.29289321881337749, 8.259292476615629042, 5.000000000000000000 ) ) ;
#4377 = VERTEX_POINT ( 'NONE', #54713 ) ;
#4378 = CARTESIAN_POINT ( 'NONE',  ( 5.068407645496677105, 9.139736423841732040E-16, 0.000000000000000000 ) ) ;
#4379 = VECTOR ( 'NONE', #105491, 999.9999999999998863 ) ;
#4380 = EDGE_CURVE ( 'NONE', #78474, #15318, #277, .T. ) ;
#4381 = ADVANCED_FACE ( 'NONE', ( #45283 ), #120636, .F. ) ;
#4382 = FACE_OUTER_BOUND ( 'NONE', #91867, .T. ) ;
#4383 = ORIENTED_EDGE ( 'NONE', *, *, #142724, .F. ) ;
#4384 = CARTESIAN_POINT ( 'NONE',  ( 28.49999999999979750, 10.08746187583915344, 4.000000000000000000 ) ) ;
#4385 = DIRECTION ( 'NONE',  ( 0.000000000000000000, 0.9647414015272156584, -0.2631995976047526442 ) ) ;
#4386 = CARTESIAN_POINT ( 'NONE',  ( 2.187499999999999556, 4.461849672132297329, -4.461849672132302658 ) ) ;
#4387 = CARTESIAN_POINT ( 'NONE',  ( 13.49999999999991296, -1.533600742197722910, 5.000000000000000000 ) ) ;
#4388 = VECTOR ( 'NONE', #20467, 999.9999999999998863 ) ;
#4389 = CARTESIAN_POINT ( 'NONE',  ( -24.48921356237309510, -27.52281430457072631, 5.000000000000000000 ) ) ;
#4390 = CARTESIAN_POINT ( 'NONE',  ( 17.06332250466817158, 2.500000000000000888, 0.000000000000000000 ) ) ;
#4391 = EDGE_CURVE ( 'NONE', #140149, #25103, #11878, .T. ) ;
#4392 = CARTESIAN_POINT ( 'NONE',  ( -11.99999999999991651, -4.447814304570786526, 5.000000000000000000 ) ) ;
#4393 = DIRECTION ( 'NONE',  ( 1.000000000000000000, 0.000000000000000000, 0.000000000000000000 ) ) ;
#4394 = EDGE_LOOP ( 'NONE', ( #43317, #106850, #131338, #104280 ) ) ;
#4395 = VERTEX_POINT ( 'NONE', #65617 ) ;
#4396 = VERTEX_POINT ( 'NONE', #109784 ) ;
#4397 = CARTESIAN_POINT ( 'NONE',  ( 120.2916666666666714, 3.975000000000003642, -6.884901960086285300 ) ) ;
#4398 = ORIENTED_EDGE ( 'NONE', *, *, #27406, .F. ) ;
#4399 = ORIENTED_EDGE ( 'NONE', *, *, #63527, .F. ) ;
#4400 = EDGE_LOOP ( 'NONE', ( #131207, #15353, #116582, #68784 ) ) ;
#4401 = DIRECTION ( 'NONE',  ( -0.6830127018922180770, -0.6830127018922204085, -0.2588190451025213501 ) ) ;
#4402 = DIRECTION ( 'NONE',  ( 0.7071067811865486830, -0.7071067811865464625, -0.000000000000000000 ) ) ;
#4403 = ORIENTED_EDGE ( 'NONE', *, *, #118266, .F. ) ;
#4404 = CARTESIAN_POINT ( 'NONE',  ( -30.32816939922331656, 14.25929247661556865, 4.000000000000000000 ) ) ;
#4405 = LINE ( 'NONE', #35729, #32519 ) ;
#4406 = LINE ( 'NONE', #28390, #81187 ) ;
#4407 = CARTESIAN_POINT ( 'NONE',  ( 115.3545968585647614, -1.637169565754161615, 6.110000000000000320 ) ) ;
#4408 = ORIENTED_EDGE ( 'NONE', *, *, #102549, .T. ) ;
#4409 = CARTESIAN_POINT ( 'NONE',  ( -14.99451991528749595, 28.92564299267948513, 4.000000000000000000 ) ) ;
#4410 = DIRECTION ( 'NONE',  ( -0.6830127018922181881, 0.6830127018922202975, -0.2588190451025214056 ) ) ;
#4411 = CARTESIAN_POINT ( 'NONE',  ( 34.49999999999976552, 4.464255608400454101, 4.994342998332159667 ) ) ;
#4412 = CARTESIAN_POINT ( 'NONE',  ( 11.81601139373100651, 28.73617430169779041, 5.000000000000000000 ) ) ;
#4413 = PLANE ( 'NONE',  #125573 ) ;
#4414 = LINE ( 'NONE', #46630, #119858 ) ;
#4415 = CARTESIAN_POINT ( 'NONE',  ( 39.01669371712955581, 7.950000000000001066, -2.130196079827421318 ) ) ;
#4416 = CARTESIAN_POINT ( 'NONE',  ( 11.99999999999991473, 7.931123077392106424, 4.000000000000000000 ) ) ;
#4417 = DIRECTION ( 'NONE',  ( -0.6830127018922181881, 0.6830127018922202975, -0.2588190451025214056 ) ) ;
#4418 = VERTEX_POINT ( 'NONE', #88039 ) ;
#4419 = ORIENTED_EDGE ( 'NONE', *, *, #66726, .T. ) ;
#4420 = CARTESIAN_POINT ( 'NONE',  ( 35.12499999999999289, -7.950000000000000178, -4.867971026610729436E-16 ) ) ;
#4421 = EDGE_LOOP ( 'NONE', ( #134278, #139734, #52048, #87188, #21958 ) ) ;
#4422 = VERTEX_POINT ( 'NONE', #56166 ) ;
#4423 = DIRECTION ( 'NONE',  ( -0.6830127018922180770, -0.6830127018922204085, -0.2588190451025213501 ) ) ;
#4424 = ADVANCED_FACE ( 'NONE', ( #100351 ), #129038, .T. ) ;
#4425 = CARTESIAN_POINT ( 'NONE',  ( 24.29974487139158867, -27.71228299555223273, 4.000000000000000000 ) ) ;
#4426 = FACE_OUTER_BOUND ( 'NONE', #3697, .T. ) ;
#4427 = ORIENTED_EDGE ( 'NONE', *, *, #139798, .T. ) ;
#4428 = DIRECTION ( 'NONE',  ( 1.000000000000000000, 0.000000000000000000, 0.000000000000000000 ) ) ;
#4429 = DIRECTION ( 'NONE',  ( -0.7071067811865486830, -0.7071067811865464625, 0.000000000000000000 ) ) ;
#4430 = CARTESIAN_POINT ( 'NONE',  ( -45.29974487139158867, -27.71228299555237840, 4.000000000000000000 ) ) ;
#4431 = CARTESIAN_POINT ( 'NONE',  ( 29.16709685856476497, -3.055000000000000160, -5.291415217122921177 ) ) ;
#4432 = ORIENTED_EDGE ( 'NONE', *, *, #85426, .F. ) ;
#4433 = PLANE ( 'NONE',  #68834 ) ;
#4434 = VERTEX_POINT ( 'NONE', #32977 ) ;
#4435 = LINE ( 'NONE', #57494, #68115 ) ;
#4436 = VECTOR ( 'NONE', #13293, 999.9999999999998863 ) ;
#4437 = VECTOR ( 'NONE', #54218, 1000.000000000000000 ) ;
#4438 = AXIS2_PLACEMENT_3D ( 'NONE', #31109, #140553, #97014 ) ;
#4439 = CARTESIAN_POINT ( 'NONE',  ( -2.903329358125931403, -2.240707523384260824, 15.26439735382751905 ) ) ;
#4440 = DIRECTION ( 'NONE',  ( 0.7071067811865487940, -0.7071067811865463515, 0.000000000000000000 ) ) ;
#4442 = ADVANCED_FACE ( 'NONE', ( #8986 ), #66302, .T. ) ;
#4441 = VECTOR ( 'NONE', #45431, 1000.000000000000000 ) ;
#4443 = DIRECTION ( 'NONE',  ( -0.000000000000000000, 0.000000000000000000, 1.000000000000000000 ) ) ;
#4444 = EDGE_LOOP ( 'NONE', ( #28106, #142001, #131924, #126948 ) ) ;
#4445 = EDGE_CURVE ( 'NONE', #10019, #47408, #54978, .T. ) ;
#4446 = ADVANCED_FACE ( 'NONE', ( #75744 ), #131544, .T. ) ;
#4447 = VERTEX_POINT ( 'NONE', #22045 ) ;
#4448 = DIRECTION ( 'NONE',  ( 0.7071067811865487940, 0.7071067811865463515, 0.000000000000000000 ) ) ;
#4449 = CARTESIAN_POINT ( 'NONE',  ( 34.92499999999998295, 21.73644205237997795, 4.195230610814717487 ) ) ;
#4450 = DIRECTION ( 'NONE',  ( 0.7071067811865487940, 0.7071067811865463515, 0.000000000000000000 ) ) ;
#4451 = EDGE_CURVE ( 'NONE', #71937, #106339, #24218, .T. ) ;
#4452 = EDGE_CURVE ( 'NONE', #84436, #44653, #69896, .T. ) ;
#4453 = VECTOR ( 'NONE', #74162, 1000.000000000000000 ) ;
#4454 = CARTESIAN_POINT ( 'NONE',  ( 47.01626352523143026, -4.472830434245839371, 4.472830434245839371 ) ) ;
#4455 = ORIENTED_EDGE ( 'NONE', *, *, #127119, .F. ) ;
#4456 = CARTESIAN_POINT ( 'NONE',  ( -32.99999999999976552, 12.83542986846994083, -1.025386466790294548 ) ) ;
#4457 = EDGE_CURVE ( 'NONE', #52896, #18442, #113336, .T. ) ;
#4458 = FACE_OUTER_BOUND ( 'NONE', #59021, .T. ) ;
#4459 = ORIENTED_EDGE ( 'NONE', *, *, #6741, .F. ) ;
#4460 = ORIENTED_EDGE ( 'NONE', *, *, #39893, .T. ) ;
#4461 = VECTOR ( 'NONE', #55652, 1000.000000000000000 ) ;
#4462 = AXIS2_PLACEMENT_3D ( 'NONE', #101054, #102525, #125700 ) ;
#4463 = DIRECTION ( 'NONE',  ( -0.000000000000000000, 0.3543493200069153248, 0.9351131265310291818 ) ) ;
#4464 = EDGE_LOOP ( 'NONE', ( #21588, #64579, #72111, #86706 ) ) ;
#4465 = ADVANCED_FACE ( 'NONE', ( #103875 ), #58322, .F. ) ;
#4466 = STYLED_ITEM ( 'NONE', ( #105922 ), #96794 ) ;
#4467 = PLANE ( 'NONE',  #118231 ) ;
#4468 = ORIENTED_EDGE ( 'NONE', *, *, #2997, .T. ) ;
#4469 = CARTESIAN_POINT ( 'NONE',  ( 0.000000000000000000, 0.000000000000000000, 5.000000000000000000 ) ) ;
#4470 = AXIS2_PLACEMENT_3D ( 'NONE', #57500, #90092, #13231 ) ;
#4471 = EDGE_CURVE ( 'NONE', #134440, #113476, #91606, .T. ) ;
#4472 = CIRCLE ( 'NONE', #64785, 2.247899999999995568 ) ;
#4474 = AXIS2_PLACEMENT_3D ( 'NONE', #130539, #10847, #42820 ) ;
#4473 = DIRECTION ( 'NONE',  ( 0.7071067811865486830, -0.7071067811865464625, -0.000000000000000000 ) ) ;
#4475 = FACE_BOUND ( 'NONE', #80602, .T. ) ;
#4476 = DIRECTION ( 'NONE',  ( 0.7071067811865487940, -0.7071067811865463515, -0.000000000000000000 ) ) ;
#4477 = FACE_OUTER_BOUND ( 'NONE', #86662, .T. ) ;
#4479 = VECTOR ( 'NONE', #39451, 1000.000000000000227 ) ;
#4478 = CARTESIAN_POINT ( 'NONE',  ( -2.816011393730999401, 28.73617430169785436, 5.000000000000000000 ) ) ;
#4480 = LINE ( 'NONE', #115409, #80506 ) ;
#4482 = ORIENTED_EDGE ( 'NONE', *, *, #105415, .F. ) ;
#4481 = CARTESIAN_POINT ( 'NONE',  ( -36.18398860626899705, 28.73617430169812437, 5.000000000000000000 ) ) ;
#4483 = VECTOR ( 'NONE', #73510, 1000.000000000000000 ) ;
#4484 = ADVANCED_FACE ( 'NONE', ( #68464 ), #15428, .T. ) ;
#4485 = PLANE ( 'NONE',  #111939 ) ;
#4486 = EDGE_LOOP ( 'NONE', ( #96374, #22334, #37714, #16444 ) ) ;
#4487 = ORIENTED_EDGE ( 'NONE', *, *, #70818, .T. ) ;
#4488 = CARTESIAN_POINT ( 'NONE',  ( 64.51626352523145158, -4.472830434245838482, 4.472830434245838482 ) ) ;
#4489 = ORIENTED_EDGE ( 'NONE', *, *, #128918, .F. ) ;
#4490 = DIRECTION ( 'NONE',  ( -0.3543493200069162685, -0.000000000000000000, -0.9351131265310288487 ) ) ;
#4491 = CARTESIAN_POINT ( 'NONE',  ( 17.99999999999987921, -10.44781430457071814, 5.000000000000000000 ) ) ;
#4492 = EDGE_CURVE ( 'NONE', #14551, #118295, #47444, .T. ) ;
#4493 = ORIENTED_EDGE ( 'NONE', *, *, #112721, .T. ) ;
#4494 = FACE_OUTER_BOUND ( 'NONE', #58383, .T. ) ;
#4495 = MECHANICAL_DESIGN_GEOMETRIC_PRESENTATION_REPRESENTATION (  '', ( #18400 ), #32319 ) ;
#4496 = ADVANCED_FACE ( 'NONE', ( #124233 ), #37957, .F. ) ;
#4497 = CARTESIAN_POINT ( 'NONE',  ( -54.18398860626899705, 28.73617430169825226, 5.000000000000000000 ) ) ;
#4498 = DIRECTION ( 'NONE',  ( -0.7071067811865486830, -0.7071067811865464625, 0.000000000000000000 ) ) ;
#4499 = EDGE_CURVE ( 'NONE', #49517, #138986, #48115, .T. ) ;
#4500 = DIRECTION ( 'NONE',  ( -1.000000000000000000, -0.000000000000000000, -0.000000000000000000 ) ) ;
#4501 = DIRECTION ( 'NONE',  ( 0.7071067811865486830, -0.7071067811865464625, -0.000000000000000000 ) ) ;
#4502 = ORIENTED_EDGE ( 'NONE', *, *, #56252, .F. ) ;
#4503 = B_SPLINE_CURVE_WITH_KNOTS ( 'NONE', 3,
 ( #32332, #76565, #120745, #21451 ),
 .UNSPECIFIED., .F., .F.,
 ( 4, 4 ),
 ( 0.000000000000000000, 0.001824211539880358363 ),
 .UNSPECIFIED. ) ;
#4504 = ORIENTED_EDGE ( 'NONE', *, *, #54253, .F. ) ;
#4505 = DIRECTION ( 'NONE',  ( 0.7071067811865487940, 0.7071067811865463515, -0.000000000000000000 ) ) ;
#4506 = LINE ( 'NONE', #37943, #136957 ) ;
#4507 = ORIENTED_EDGE ( 'NONE', *, *, #108622, .T. ) ;
#4508 = EDGE_CURVE ( 'NONE', #26708, #125846, #3829, .T. ) ;
#4509 = ORIENTED_EDGE ( 'NONE', *, *, #129381, .F. ) ;
#4510 = ORIENTED_EDGE ( 'NONE', *, *, #58996, .F. ) ;
#4511 = FACE_OUTER_BOUND ( 'NONE', #19918, .T. ) ;
#4512 = CARTESIAN_POINT ( 'NONE',  ( 23.99451991528749062, 28.92564299267954908, 4.000000000000000000 ) ) ;
#4513 = ORIENTED_EDGE ( 'NONE', *, *, #58773, .T. ) ;
#4514 = DIRECTION ( 'NONE',  ( -0.000000000000000000, 0.000000000000000000, 1.000000000000000000 ) ) ;
#4515 = CARTESIAN_POINT ( 'NONE',  ( -3.299744871391591339, -27.71228299555208352, 4.000000000000000000 ) ) ;
#4516 = CARTESIAN_POINT ( 'NONE',  ( 5.171236474768553748, 0.000000000000000000, 7.934999999999990727 ) ) ;
#4517 = DIRECTION ( 'NONE',  ( -0.7071067811865477948, 8.659560562354931626E-17, -0.7071067811865473507 ) ) ;
#4518 = ORIENTED_EDGE ( 'NONE', *, *, #126994, .F. ) ;
#4519 = EDGE_CURVE ( 'NONE', #110495, #113106, #26356, .T. ) ;
#4520 = LINE ( 'NONE', #56880, #57366 ) ;
#4521 = LINE ( 'NONE', #35111, #120700 ) ;
#4522 = DIRECTION ( 'NONE',  ( 1.000000000000000000, 0.000000000000000000, 0.000000000000000000 ) ) ;
#4524 = VERTEX_POINT ( 'NONE', #126363 ) ;
#4523 = CARTESIAN_POINT ( 'NONE',  ( -35.56319896779149303, -12.74070752338414891, 9.898150129686460019 ) ) ;
#4525 = CARTESIAN_POINT ( 'NONE',  ( -34.92500000000001137, 22.22500000000000142, 4.000000000000000000 ) ) ;
#4526 = ORIENTED_EDGE ( 'NONE', *, *, #316, .F. ) ;
#4527 = DIRECTION ( 'NONE',  ( -1.000000000000000000, -1.224606353822377258E-16, -0.000000000000000000 ) ) ;
#4528 = EDGE_CURVE ( 'NONE', #134155, #12475, #123555, .T. ) ;
#4529 = DIRECTION ( 'NONE',  ( -0.7071067811865487940, 0.7071067811865463515, -0.000000000000000000 ) ) ;
#4530 = DIRECTION ( 'NONE',  ( 0.000000000000000000, 1.000000000000000000, 0.000000000000000000 ) ) ;
#4531 = ORIENTED_EDGE ( 'NONE', *, *, #67079, .T. ) ;
#4532 = CARTESIAN_POINT ( 'NONE',  ( -33.43654659701051912, -22.22500000000000142, 5.564030635702776451 ) ) ;
#4533 = EDGE_CURVE ( 'NONE', #48333, #79691, #124938, .T. ) ;
#4534 = DIRECTION ( 'NONE',  ( -1.000000000000000000, -1.224606353822377258E-16, -0.000000000000000000 ) ) ;
#4535 = DIRECTION ( 'NONE',  ( -0.7071067811865486830, -0.7071067811865464625, -0.000000000000000000 ) ) ;
#4536 = DIRECTION ( 'NONE',  ( 1.000000000000000000, 0.000000000000000000, 0.000000000000000000 ) ) ;
#4537 = VECTOR ( 'NONE', #106112, 999.9999999999998863 ) ;
#4538 = EDGE_LOOP ( 'NONE', ( #59722, #20676, #143343, #125451, #122426, #85300, #53491, #47215 ) ) ;
#4539 = VECTOR ( 'NONE', #114583, 1000.000000000000000 ) ;
#4540 = AXIS2_PLACEMENT_3D ( 'NONE', #69357, #125137, #25826 ) ;
#4541 = AXIS2_PLACEMENT_3D ( 'NONE', #86986, #63826, #53660 ) ;
#4542 = CARTESIAN_POINT ( 'NONE',  ( -14.81601139373099585, 28.73617430169776910, 5.000000000000000000 ) ) ;
#4543 = CARTESIAN_POINT ( 'NONE',  ( 34.42499999999998295, -22.22500000000000142, 0.4999999999999995559 ) ) ;
#4544 = DIRECTION ( 'NONE',  ( -0.000000000000000000, -0.3543493200069153248, -0.9351131265310291818 ) ) ;
#4545 = AXIS2_PLACEMENT_3D ( 'NONE', #77860, #122049, #125657 ) ;
#4546 = CARTESIAN_POINT ( 'NONE',  ( -22.49999999999984368, -1.695981523266240076, 4.571483868317929300 ) ) ;
#4547 = EDGE_CURVE ( 'NONE', #64350, #141614, #4520, .T. ) ;
#4548 = DIRECTION ( 'NONE',  ( -1.000000000000000000, -1.224606353822377258E-16, -0.000000000000000000 ) ) ;
#4549 = ORIENTED_EDGE ( 'NONE', *, *, #137433, .T. ) ;
#4550 = ORIENTED_EDGE ( 'NONE', *, *, #31669, .T. ) ;
#4551 = FACE_OUTER_BOUND ( 'NONE', #31005, .T. ) ;
#4552 = VECTOR ( 'NONE', #63538, 1000.000000000000000 ) ;
#4553 = PLANE ( 'NONE',  #89903 ) ;
#4554 = CARTESIAN_POINT ( 'NONE',  ( 3.187069808101886448, -2.126176841940956130, 7.934999999999991616 ) ) ;
#4555 = DIRECTION ( 'NONE',  ( -0.3543493200069162685, -0.000000000000000000, -0.9351131265310288487 ) ) ;
#4556 = ADVANCED_FACE ( 'NONE', ( #93030 ), #137262, .F. ) ;
#4557 = CARTESIAN_POINT ( 'NONE',  ( 34.92499999999998295, 6.324594729295675677, 11.02525794543158000 ) ) ;
#4558 = LINE ( 'NONE', #123593, #106114 ) ;
#4559 = LINE ( 'NONE', #37265, #106922 ) ;
#4560 = ORIENTED_EDGE ( 'NONE', *, *, #134300, .T. ) ;
#4561 = CARTESIAN_POINT ( 'NONE',  ( -2.510786437626908008, -27.52281430457053446, 5.000000000000000000 ) ) ;
#4562 = CARTESIAN_POINT ( 'NONE',  ( -0.7933393645784717618, 21.75929247661549581, 4.998822639870701856 ) ) ;
#4563 = AXIS2_PLACEMENT_3D ( 'NONE', #130558, #41377, #43531 ) ;
#4564 = DIRECTION ( 'NONE',  ( -0.6830127018922181881, 0.6830127018922202975, -0.2588190451025214056 ) ) ;
#4565 = CARTESIAN_POINT ( 'NONE',  ( 44.68293019189811588, -1.637169565754159173, -6.109999999999999432 ) ) ;
#4566 = EDGE_CURVE ( 'NONE', #58909, #131858, #101038, .T. ) ;
#4567 = DIRECTION ( 'NONE',  ( -0.7071067811865486830, 0.7071067811865464625, 0.000000000000000000 ) ) ;
#4568 = PRESENTATION_LAYER_ASSIGNMENT (  '', '', ( #44078 ) ) ;
#4569 = EDGE_CURVE ( 'NONE', #136335, #119204, #24909, .T. ) ;
#4570 = ORIENTED_EDGE ( 'NONE', *, *, #75403, .T. ) ;
#4571 =( NAMED_UNIT ( * ) PLANE_ANGLE_UNIT ( ) SI_UNIT ( $, .RADIAN. ) );
#4572 = ORIENTED_EDGE ( 'NONE', *, *, #10276, .F. ) ;
#4573 = ORIENTED_EDGE ( 'NONE', *, *, #89697, .F. ) ;
#4574 = CARTESIAN_POINT ( 'NONE',  ( -16.49999999999988631, 19.39370406404965763, 1.459788787078239558 ) ) ;
#4575 = VECTOR ( 'NONE', #55135, 1000.000000000000000 ) ;
#4576 = LINE ( 'NONE', #69957, #62312 ) ;
#4577 = CARTESIAN_POINT ( 'NONE',  ( 0.000000000000000000, 9.735942053221458872E-16, -7.950000000000000178 ) ) ;
#4578 = FACE_OUTER_BOUND ( 'NONE', #91247, .T. ) ;
#4579 = ADVANCED_FACE ( 'NONE', ( #13303 ), #57576, .F. ) ;
#4580 = PLANE ( 'NONE',  #139132 ) ;
#4581 = CARTESIAN_POINT ( 'NONE',  ( 11.81250000000000178, -4.461849672132299993, -4.461849672132299105 ) ) ;
#4582 = CONICAL_SURFACE ( 'NONE', #104167, 2.055000000000000604, 0.9599310885968764806 ) ;
#4583 = VERTEX_POINT ( 'NONE', #60437 ) ;
#4584 = CARTESIAN_POINT ( 'NONE',  ( -34.49999999999974420, -17.94567065516885762, 4.994342998332165884 ) ) ;
#4585 = CARTESIAN_POINT ( 'NONE',  ( -13.26601651615776767, 1.700382741644379081, 5.000000000000000000 ) ) ;
#4586 = VECTOR ( 'NONE', #105241, 1000.000000000000000 ) ;
#4587 = CARTESIAN_POINT ( 'NONE',  ( 1.499999999999990896, 13.08746187583910725, 4.000000000000000000 ) ) ;
#4588 = CARTESIAN_POINT ( 'NONE',  ( 117.8125000000000000, 5.819803920172571310, 5.819803920172576639 ) ) ;
#4589 = CARTESIAN_POINT ( 'NONE',  ( 69.35002705046287019, -5.819803920172572198, -5.819803920172572198 ) ) ;
#4590 = DIRECTION ( 'NONE',  ( 0.000000000000000000, 0.000000000000000000, 1.000000000000000000 ) ) ;
#4591 = VECTOR ( 'NONE', #5242, 1000.000000000000227 ) ;
#4592 = ORIENTED_EDGE ( 'NONE', *, *, #58124, .T. ) ;
#4593 = VERTEX_POINT ( 'NONE', #71300 ) ;
#4594 = CARTESIAN_POINT ( 'NONE',  ( 68.52083333333334281, 7.949999999999999289, 2.130196079827431532 ) ) ;
#4595 = DIRECTION ( 'NONE',  ( 0.3543493200069162685, -0.000000000000000000, -0.9351131265310288487 ) ) ;
#4596 = LINE ( 'NONE', #61248, #25435 ) ;
#4597 = DIRECTION ( 'NONE',  ( -1.000000000000000000, -1.224606353822377258E-16, -0.000000000000000000 ) ) ;
#4598 = AXIS2_PLACEMENT_3D ( 'NONE', #51576, #19636, #16780 ) ;
#4599 = ORIENTED_EDGE ( 'NONE', *, *, #42924, .T. ) ;
#4600 = CARTESIAN_POINT ( 'NONE',  ( -2.999999999999975575, -21.03360074219752107, 5.000000000000000000 ) ) ;
#4601 = DIRECTION ( 'NONE',  ( -0.3543493200069162685, -0.000000000000000000, -0.9351131265310288487 ) ) ;
#4602 = CARTESIAN_POINT ( 'NONE',  ( 52.64626352523142572, -4.472830434245840259, 4.472830434245839371 ) ) ;
#4603 = DIRECTION ( 'NONE',  ( -0.7071067811865486830, 0.7071067811865464625, 0.000000000000000000 ) ) ;
#4604 = ORIENTED_EDGE ( 'NONE', *, *, #23688, .F. ) ;
#4605 = ORIENTED_EDGE ( 'NONE', *, *, #62718, .F. ) ;
#4606 = VECTOR ( 'NONE', #77015, 1000.000000000000227 ) ;
#4607 = CARTESIAN_POINT ( 'NONE',  ( -7.140000000000001457, -39.92999999999999261, 18.93259187797432475 ) ) ;
#4608 = CARTESIAN_POINT ( 'NONE',  ( 27.72281430457040940, -21.72500000000000142, 5.000000000000000000 ) ) ;
#4609 = DIRECTION ( 'NONE',  ( 0.6830127018922180770, -0.6830127018922204085, -0.2588190451025213501 ) ) ;
#4610 = CARTESIAN_POINT ( 'NONE',  ( 25.39999999999999858, -2.599999999999908606, 1.319531433729349815E-14 ) ) ;
#4611 = LINE ( 'NONE', #60530, #18680 ) ;
#4612 = EDGE_CURVE ( 'NONE', #81346, #125922, #99682, .T. ) ;
#4613 = ADVANCED_FACE ( 'NONE', ( #49565 ), #115453, .T. ) ;
#4615 = VERTEX_POINT ( 'NONE', #76624 ) ;
#4614 = LINE ( 'NONE', #57674, #22076 ) ;
#4616 = DIRECTION ( 'NONE',  ( 0.9743982503113673976, -0.2248289345038710085, 0.000000000000000000 ) ) ;
#4617 = CARTESIAN_POINT ( 'NONE',  ( -11.20003122016829877, 8.259292476615627265, 16.85664084051843403 ) ) ;
#4618 = DIRECTION ( 'NONE',  ( 0.3543493200069163240, -0.000000000000000000, -0.9351131265310288487 ) ) ;
#4619 = VECTOR ( 'NONE', #47658, 1000.000000000000000 ) ;
#4620 = CARTESIAN_POINT ( 'NONE',  ( 27.79289321881326202, -8.240707523384200428, 5.000000000000000000 ) ) ;
#4621 = CLOSED_SHELL ( 'NONE', ( #52502, #91665, #52315, #13962, #78021, #75969, #134383, #125716, #55019, #90440, #104262, #68389, #21319 ) ) ;
#4623 = VERTEX_POINT ( 'NONE', #132448 ) ;
#4622 = EDGE_CURVE ( 'NONE', #84037, #6566, #21508, .T. ) ;
#4624 = ADVANCED_FACE ( 'NONE', ( #43977 ), #78044, .F. ) ;
#4625 = ORIENTED_EDGE ( 'NONE', *, *, #897, .F. ) ;
#4626 = ADVANCED_FACE ( 'NONE', ( #54171 ), #98359, .F. ) ;
#4627 = CYLINDRICAL_SURFACE ( 'NONE', #126308, 5.999999999999998224 ) ;
#4628 = DIRECTION ( 'NONE',  ( -0.7071067811865487940, 0.7071067811865463515, -0.000000000000000000 ) ) ;
#4630 = EDGE_CURVE ( 'NONE', #38512, #37121, #43271, .T. ) ;
#4629 = CARTESIAN_POINT ( 'NONE',  ( 29.01088028653927964, -22.02621442084248216, 4.990779571109221990 ) ) ;
#4631 = CARTESIAN_POINT ( 'NONE',  ( 124.1833603837965967, -2.130196079832207712, 7.949999999997237055 ) ) ;
#4632 = CARTESIAN_POINT ( 'NONE',  ( -28.49999999999980460, 22.01701374228153085, 2.453858888625695567 ) ) ;
#4633 = ORIENTED_EDGE ( 'NONE', *, *, #124622, .F. ) ;
#4634 = VERTEX_POINT ( 'NONE', #130993 ) ;
#4635 = EDGE_CURVE ( 'NONE', #14634, #85340, #65765, .T. ) ;
#4636 = LINE ( 'NONE', #7540, #491 ) ;
#4638 = VECTOR ( 'NONE', #33883, 1000.000000000000227 ) ;
#4637 = DIRECTION ( 'NONE',  ( 0.7071067811865487940, -0.7071067811865463515, 0.000000000000000000 ) ) ;
#4639 = VECTOR ( 'NONE', #5043, 1000.000000000000000 ) ;
#4640 = ADVANCED_FACE ( 'NONE', ( #87480 ), #88198, .F. ) ;
#4642 = ORIENTED_EDGE ( 'NONE', *, *, #12251, .F. ) ;
#4641 = VECTOR ( 'NONE', #46925, 1000.000000000000000 ) ;
#4643 = DIRECTION ( 'NONE',  ( 0.7071067811865487940, 0.7071067811865463515, 0.000000000000000000 ) ) ;
#4644 = ORIENTED_EDGE ( 'NONE', *, *, #20901, .T. ) ;
#4645 = VECTOR ( 'NONE', #19677, 1000.000000000000000 ) ;
#4646 = DIRECTION ( 'NONE',  ( -0.7071067811865487940, 0.7071067811865463515, -0.000000000000000000 ) ) ;
#4647 = DIRECTION ( 'NONE',  ( 0.7071067811865487940, 0.7071067811865463515, 0.000000000000000000 ) ) ;
#4648 = VECTOR ( 'NONE', #109430, 1000.000000000000000 ) ;
#4649 = AXIS2_PLACEMENT_3D ( 'NONE', #1386, #21016, #78281 ) ;
#4650 = AXIS2_PLACEMENT_3D ( 'NONE', #35322, #68654, #89663 ) ;
#4651 = VECTOR ( 'NONE', #74805, 1000.000000000000000 ) ;
#4652 =( BOUNDED_CURVE ( )  B_SPLINE_CURVE ( 2, ( #38213, #28043, #96128, #82427, #41054, #73685, #104880, #115713, #117858, #115003, #50509, #126612, #27302 ),
 .UNSPECIFIED., .F., .T. ) 
 B_SPLINE_CURVE_WITH_KNOTS ( ( 3, 2, 2, 2, 2, 2, 3 ),
 ( 0.09999999999998596123, 0.1027777777777660745, 0.1055555555555461877, 0.1083333333333263149, 0.1111111111111064281, 0.1138888888888865414, 0.1166666666666666685 ),
 .UNSPECIFIED. ) 
 CURVE ( )  GEOMETRIC_REPRESENTATION_ITEM ( )  RATIONAL_B_SPLINE_CURVE ( ( 1.000000000000172307, 0.9659258262888960056, 1.000000000000000000, 0.9659258262890683122, 1.000000000000000000, 0.9659258262890683122, 1.000000000000000000, 0.9659258262890683122, 1.000000000000000000, 0.9659258262890683122, 1.000000000000000000, 0.9659258262890683122, 1.000000000000000000 ) ) 
 REPRESENTATION_ITEM ( '' )  );
#4653 = VECTOR ( 'NONE', #9535, 1000.000000000000000 ) ;
#4654 = EDGE_CURVE ( 'NONE', #37030, #64397, #143272, .T. ) ;
#4655 = FACE_BOUND ( 'NONE', #116935, .T. ) ;
#4656 = CARTESIAN_POINT ( 'NONE',  ( -37.62823445044362103, -8.240707523384193323, 11.38925528200761228 ) ) ;
#4657 = CARTESIAN_POINT ( 'NONE',  ( 3.722814304570581712, -21.72499999999999432, 5.000000000000000000 ) ) ;
#4658 = DIRECTION ( 'NONE',  ( 0.7071067811865487940, 0.7071067811865463515, 0.000000000000000000 ) ) ;
#4659 = CARTESIAN_POINT ( 'NONE',  ( 0.000000000000000000, 0.000000000000000000, 0.000000000000000000 ) ) ;
#4660 = EDGE_CURVE ( 'NONE', #11497, #105889, #121509, .T. ) ;
#4661 = PLANE ( 'NONE',  #53283 ) ;
#4662 = SHAPE_DEFINITION_REPRESENTATION ( #15602, #40289 ) ;
#4663 = VERTEX_POINT ( 'NONE', #439 ) ;
#4664 = ORIENTED_EDGE ( 'NONE', *, *, #43389, .F. ) ;
#4665 = CARTESIAN_POINT ( 'NONE',  ( 94.55793019189810877, 6.110000000000000320, -1.637169565754156064 ) ) ;
#4666 = ORIENTED_EDGE ( 'NONE', *, *, #62977, .F. ) ;
#4667 = DIRECTION ( 'NONE',  ( -1.000000000000000000, -1.224606353822377258E-16, -0.000000000000000000 ) ) ;
#4668 = STYLED_ITEM ( 'NONE', ( #17992 ), #48749 ) ;
#4669 = PLANE ( 'NONE',  #107200 ) ;
#4670 = DIRECTION ( 'NONE',  ( -0.7071067811865486830, -0.7071067811865464625, 0.000000000000000000 ) ) ;
#4671 = AXIS2_PLACEMENT_3D ( 'NONE', #86380, #106660, #73365 ) ;
#4672 = CARTESIAN_POINT ( 'NONE',  ( -34.92500000000001137, -13.91861162105994332, 18.69616556237236793 ) ) ;
#4674 = EDGE_LOOP ( 'NONE', ( #48934, #60606, #68508, #139843 ) ) ;
#4673 = EDGE_CURVE ( 'NONE', #132626, #23262, #51447, .T. ) ;
#4675 = CARTESIAN_POINT ( 'NONE',  ( 11.99999999999991473, -9.033600742197648970, 5.000000000000000000 ) ) ;
#4676 = VECTOR ( 'NONE', #51651, 999.9999999999998863 ) ;
#4677 = CARTESIAN_POINT ( 'NONE',  ( -12.69999999999998153, 0.000000000000000000, 0.000000000000000000 ) ) ;
#4678 = CARTESIAN_POINT ( 'NONE',  ( -26.99999999999981171, 8.966399257802175171, 5.000000000000000000 ) ) ;
#4680 = DIRECTION ( 'NONE',  ( -0.6830127018922181881, 0.6830127018922202975, -0.2588190451025214056 ) ) ;
#4679 = LINE ( 'NONE', #125825, #105951 ) ;
#4681 = EDGE_CURVE ( 'NONE', #117376, #103116, #99766, .T. ) ;
#4682 = LINE ( 'NONE', #91069, #120166 ) ;
#4683 = CARTESIAN_POINT ( 'NONE',  ( -22.49999999999983658, 10.08746187583913922, 4.000000000000000000 ) ) ;
#4684 = ORIENTED_EDGE ( 'NONE', *, *, #105664, .F. ) ;
#4685 = AXIS2_PLACEMENT_3D ( 'NONE', #13349, #35156, #67803 ) ;
#4686 = CARTESIAN_POINT ( 'NONE',  ( 34.49999999999975842, -1.535744391599495273, 4.994342998332161443 ) ) ;
#4687 = EDGE_CURVE ( 'NONE', #13443, #120930, #59168, .T. ) ;
#4688 = CARTESIAN_POINT ( 'NONE',  ( 2.999999999999999112, 5.817072295949927426E-16, 4.750000000000000000 ) ) ;
#4689 = ORIENTED_EDGE ( 'NONE', *, *, #29115, .T. ) ;
#4690 = EDGE_LOOP ( 'NONE', ( #11672, #66259, #141755, #18964 ) ) ;
#4691 = ORIENTED_EDGE ( 'NONE', *, *, #123821, .F. ) ;
#4692 = CARTESIAN_POINT ( 'NONE',  ( 46.95876352523143993, 0.000000000000000000, -6.110000000000001208 ) ) ;
#4693 = ORIENTED_EDGE ( 'NONE', *, *, #59004, .T. ) ;
#4694 = EDGE_CURVE ( 'NONE', #31169, #33404, #35267, .T. ) ;
#4695 = VECTOR ( 'NONE', #118557, 1000.000000000000000 ) ;
#4696 = CARTESIAN_POINT ( 'NONE',  ( 13.17080628287043886, -3.047499999999997211, -5.278424836066143655 ) ) ;
#4697 = CARTESIAN_POINT ( 'NONE',  ( -13.89419556063288397, 5.740820235442677166, -29.07950590408880132 ) ) ;
#4698 = ORIENTED_EDGE ( 'NONE', *, *, #53683, .F. ) ;
#4699 = EDGE_CURVE ( 'NONE', #87818, #139479, #70051, .T. ) ;
#4700 = DIRECTION ( 'NONE',  ( 0.7071067811865487940, -0.7071067811865463515, 0.000000000000000000 ) ) ;
#4701 = VERTEX_POINT ( 'NONE', #47582 ) ;
#4702 = FACE_OUTER_BOUND ( 'NONE', #93176, .T. ) ;
#4703 = CARTESIAN_POINT ( 'NONE',  ( 9.591592354503321260, 9.902892378096218942E-16, 0.000000000000000000 ) ) ;
#4705 = ORIENTED_EDGE ( 'NONE', *, *, #55667, .F. ) ;
#4704 = CARTESIAN_POINT ( 'NONE',  ( 22.49999999999984723, 12.05218569542904739, 5.000000000000000000 ) ) ;
#4706 = ORIENTED_EDGE ( 'NONE', *, *, #82969, .F. ) ;
#4707 = CARTESIAN_POINT ( 'NONE',  ( -32.29289321881321939, -18.74070752338409207, 5.000000000000000000 ) ) ;
#4708 = CARTESIAN_POINT ( 'NONE',  ( -7.940000000000001279, -35.14999999999999147, -10.00000000000000178 ) ) ;
#4709 = ORIENTED_EDGE ( 'NONE', *, *, #84426, .T. ) ;
#4710 = CARTESIAN_POINT ( 'NONE',  ( 33.48921356237309510, -27.52281430457078670, 5.000000000000000000 ) ) ;
#4711 = ORIENTED_EDGE ( 'NONE', *, *, #95825, .F. ) ;
#4712 = EDGE_LOOP ( 'NONE', ( #70478, #32398, #61624, #29877 ) ) ;
#4713 = EDGE_CURVE ( 'NONE', #39610, #90585, #114213, .T. ) ;
#4714 = EDGE_LOOP ( 'NONE', ( #88066, #17537, #89064, #76430 ) ) ;
#4715 = ORIENTED_EDGE ( 'NONE', *, *, #3295, .T. ) ;
#4716 = CARTESIAN_POINT ( 'NONE',  ( -24.32816939922335919, -15.74070752338412049, 4.000000000000000000 ) ) ;
#4717 = AXIS2_PLACEMENT_3D ( 'NONE', #4339, #49385, #36341 ) ;
#4718 =( NAMED_UNIT ( * ) PLANE_ANGLE_UNIT ( ) SI_UNIT ( $, .RADIAN. ) );
#4719 = CARTESIAN_POINT ( 'NONE',  ( 33.48921356237309510, -27.52281430457078670, 5.000000000000000000 ) ) ;
#4720 = EDGE_CURVE ( 'NONE', #6614, #24067, #135289, .T. ) ;
#4721 = DIRECTION ( 'NONE',  ( -0.3543493200069162685, -0.000000000000000000, -0.9351131265310288487 ) ) ;
#4722 = DIRECTION ( 'NONE',  ( -0.000000000000000000, -0.3543493200069152693, 0.9351131265310292928 ) ) ;
#4723 = ORIENTED_EDGE ( 'NONE', *, *, #120226, .F. ) ;
#4724 = AXIS2_PLACEMENT_3D ( 'NONE', #114124, #92351, #137322 ) ;
#4725 = AXIS2_PLACEMENT_3D ( 'NONE', #121034, #54395, #45659 ) ;
#4726 = DIRECTION ( 'NONE',  ( 0.6830127018922181881, 0.6830127018922202975, -0.2588190451025214056 ) ) ;
#4727 = CARTESIAN_POINT ( 'NONE',  ( 20.83290314143522082, -3.967499999999994476, 6.871911579029513106 ) ) ;
#4728 = EDGE_CURVE ( 'NONE', #32830, #113567, #80243, .T. ) ;
#4729 = DIRECTION ( 'NONE',  ( 1.000000000000000000, 0.000000000000000000, 0.000000000000000000 ) ) ;
#4730 = DIRECTION ( 'NONE',  ( 0.3543493200069162685, -0.000000000000000000, -0.9351131265310288487 ) ) ;
#4731 = CARTESIAN_POINT ( 'NONE',  ( -34.36724870009786059, 22.27000000000001023, -12.13301201282878772 ) ) ;
#4732 = VERTEX_POINT ( 'NONE', #104018 ) ;
#4733 = ORIENTED_EDGE ( 'NONE', *, *, #28340, .T. ) ;
#4734 = EDGE_LOOP ( 'NONE', ( #66650, #123584, #135024 ) ) ;
#4735 = CARTESIAN_POINT ( 'NONE',  ( -2.000000000000000000, -2.375000000000000000, 4.319999999999998508 ) ) ;
#4736 = CARTESIAN_POINT ( 'NONE',  ( 96.03752705046289861, -9.735942053221456900E-16, 7.949999999999998401 ) ) ;
#4737 = FACE_OUTER_BOUND ( 'NONE', #105094, .T. ) ;
#4738 = LINE ( 'NONE', #57789, #82167 ) ;
#4739 = VECTOR ( 'NONE', #121161, 1000.000000000000000 ) ;
#4740 = DIRECTION ( 'NONE',  ( -0.000000000000000000, -0.3543493200069152693, 0.9351131265310292928 ) ) ;
#4741 = CARTESIAN_POINT ( 'NONE',  ( 70.78709685856478018, 3.054999999999997939, 5.291415217122920289 ) ) ;
#4742 = EDGE_CURVE ( 'NONE', #26904, #26060, #67911, .T. ) ;
#4743 = CARTESIAN_POINT ( 'NONE',  ( -11.99999999999992006, 7.588810512006196163, -3.013526669885200793 ) ) ;
#4744 = AXIS2_PLACEMENT_3D ( 'NONE', #15215, #92798, #59494 ) ;
#4745 = CIRCLE ( 'NONE', #11710, 3.499999999999999556 ) ;
#4746 = CARTESIAN_POINT ( 'NONE',  ( -8.510786437626906675, -27.52281430457049183, 5.000000000000000000 ) ) ;
#4747 = ADVANCED_FACE ( 'NONE', ( #58474 ), #126748, .T. ) ;
#4748 = CARTESIAN_POINT ( 'NONE',  ( -33.70710678118631165, -12.74070752338415602, 5.000000000000000000 ) ) ;
#4749 = LINE ( 'NONE', #104092, #25812 ) ;
#4750 = DIRECTION ( 'NONE',  ( 0.7071067811865487940, 0.7071067811865463515, 0.000000000000000000 ) ) ;
#4751 = EDGE_LOOP ( 'NONE', ( #110759, #50963, #124654, #53214, #112307 ) ) ;
#4752 = VECTOR ( 'NONE', #15985, 999.9999999999998863 ) ;
#4753 = CIRCLE ( 'NONE', #108884, 2.500000000000000444 ) ;
#4754 = AXIS2_PLACEMENT_3D ( 'NONE', #75786, #7635, #94645 ) ;
#4756 = CARTESIAN_POINT ( 'NONE',  ( -23.81601139373100295, 28.73617430169770870, 5.000000000000000000 ) ) ;
#4755 = VECTOR ( 'NONE', #88807, 1000.000000000000000 ) ;
#4757 = ORIENTED_EDGE ( 'NONE', *, *, #48946, .T. ) ;
#4758 = VECTOR ( 'NONE', #32234, 1000.000000000000114 ) ;
#4759 = CARTESIAN_POINT ( 'NONE',  ( -18.70710678118641468, 17.25929247661554200, 5.000000000000000000 ) ) ;
#4761 = VERTEX_POINT ( 'NONE', #13447 ) ;
#4760 = CARTESIAN_POINT ( 'NONE',  ( 34.47516574401890921, -16.50948238788420852, 4.998110765256833510 ) ) ;
#4762 = EDGE_CURVE ( 'NONE', #92431, #8931, #68597, .T. ) ;
#4763 = CARTESIAN_POINT ( 'NONE',  ( 26.48334561358936412, 22.22500000000000142, 4.500000000000000888 ) ) ;
#4764 = CARTESIAN_POINT ( 'NONE',  ( 156.1499999999997783, -52.14999999999999147, -34.92499999999975557 ) ) ;
#4765 = ORIENTED_EDGE ( 'NONE', *, *, #18418, .T. ) ;
#4766 = CARTESIAN_POINT ( 'NONE',  ( 0.000000000000000000, 0.000000000000000000, 5.000000000000000000 ) ) ;
#4767 = EDGE_LOOP ( 'NONE', ( #420, #35815, #13612, #55957 ) ) ;
#4768 = DIRECTION ( 'NONE',  ( -0.7071067811865486830, -0.7071067811865464625, 0.000000000000000000 ) ) ;
#4769 = AXIS2_PLACEMENT_3D ( 'NONE', #25165, #24459, #89036 ) ;
#4770 = VERTEX_POINT ( 'NONE', #37380 ) ;
#4771 = DIRECTION ( 'NONE',  ( -0.000000000000000000, 0.3543493200069153248, 0.9351131265310292928 ) ) ;
#4772 = CARTESIAN_POINT ( 'NONE',  ( 91.66252705046288440, 7.949999999999998401, 1.460391307983218338E-15 ) ) ;
#4773 = LINE ( 'NONE', #114301, #60213 ) ;
#4774 = PLANE ( 'NONE',  #143303 ) ;
#4775 = ORIENTED_EDGE ( 'NONE', *, *, #37968, .T. ) ;
#4776 = AXIS2_PLACEMENT_3D ( 'NONE', #125623, #48774, #116151 ) ;
#4777 = DIRECTION ( 'NONE',  ( -0.7071067811865486830, 0.7071067811865464625, 0.000000000000000000 ) ) ;
#4778 = PLANE ( 'NONE',  #62322 ) ;
#4779 = CARTESIAN_POINT ( 'NONE',  ( 27.85416666666666785, 1.633150327867695095, 6.094999999999988205 ) ) ;
#4781 = CIRCLE ( 'NONE', #136774, 2.500000000000000444 ) ;
#4780 = CARTESIAN_POINT ( 'NONE',  ( 72.48921356237309510, -27.52281430457106026, 5.000000000000000000 ) ) ;
#4782 = PLANE ( 'NONE',  #129969 ) ;
#4783 = ORIENTED_EDGE ( 'NONE', *, *, #125439, .F. ) ;
#4784 = AXIS2_PLACEMENT_3D ( 'NONE', #136833, #137564, #15716 ) ;
#4785 = DIRECTION ( 'NONE',  ( 1.000000000000000000, 0.000000000000000000, 0.000000000000000000 ) ) ;
#4786 = VERTEX_POINT ( 'NONE', #81619 ) ;
#4787 = VECTOR ( 'NONE', #108970, 1000.000000000000000 ) ;
#4788 = CARTESIAN_POINT ( 'NONE',  ( 88.95876352523143282, 0.000000000000000000, -6.110000000000001208 ) ) ;
#4789 = CARTESIAN_POINT ( 'NONE',  ( -8.999999999999937828, -10.77435723561695902, -9.972017380717208113 ) ) ;
#4790 = EDGE_CURVE ( 'NONE', #121707, #85225, #4679, .T. ) ;
#4791 = DIRECTION ( 'NONE',  ( 0.7071067811865487940, 0.7071067811865463515, 0.000000000000000000 ) ) ;
#4792 = FACE_OUTER_BOUND ( 'NONE', #15066, .T. ) ;
#4793 = ORIENTED_EDGE ( 'NONE', *, *, #93459, .F. ) ;
#4794 = AXIS2_PLACEMENT_3D ( 'NONE', #706, #66018, #131243 ) ;
#4795 = CARTESIAN_POINT ( 'NONE',  ( -45.48921356237309510, -27.52281430457087197, 5.000000000000000000 ) ) ;
#4796 = CARTESIAN_POINT ( 'NONE',  ( -34.92500000000001137, 1.512461875839480552, 4.000000000000000000 ) ) ;
#4797 = CARTESIAN_POINT ( 'NONE',  ( 23.99451991528749062, 28.92564299267954908, 4.000000000000000000 ) ) ;
#4798 = AXIS2_PLACEMENT_3D ( 'NONE', #29231, #93785, #7459 ) ;
#4799 = DIRECTION ( 'NONE',  ( 0.7071067811865487940, -0.7071067811865463515, 0.000000000000000000 ) ) ;
#4801 = ORIENTED_EDGE ( 'NONE', *, *, #5928, .F. ) ;
#4800 = LINE ( 'NONE', #136083, #123848 ) ;
#4802 = LINE ( 'NONE', #115008, #20567 ) ;
#4803 = DIRECTION ( 'NONE',  ( -0.7071067811865486830, 0.7071067811865464625, 0.000000000000000000 ) ) ;
#4804 = CARTESIAN_POINT ( 'NONE',  ( 1.534715839894093881, -2.368487323979017400, 6.120741323661095024 ) ) ;
#4805 = CARTESIAN_POINT ( 'NONE',  ( 45.18398860626900415, 28.73617430169818832, 5.000000000000000000 ) ) ;
#4806 = VERTEX_POINT ( 'NONE', #70745 ) ;
#4807 = ORIENTED_EDGE ( 'NONE', *, *, #20774, .T. ) ;
#4808 = VERTEX_POINT ( 'NONE', #48979 ) ;
#4809 = ADVANCED_FACE ( 'NONE', ( #137409 ), #134569, .F. ) ;
#4810 = CARTESIAN_POINT ( 'NONE',  ( 86.18793019189811844, 6.110000000000002984, -1.637169565754156730 ) ) ;
#4811 = CONICAL_SURFACE ( 'NONE', #28055, 2.055000000000000604, 0.9599310885968764806 ) ;
#4812 = EDGE_LOOP ( 'NONE', ( #105292, #1071, #59042, #72547 ) ) ;
#4813 = ADVANCED_FACE ( 'NONE', ( #130655 ), #138117, .F. ) ;
#4814 =( NAMED_UNIT ( * ) PLANE_ANGLE_UNIT ( ) SI_UNIT ( $, .RADIAN. ) );
#4815 = CARTESIAN_POINT ( 'NONE',  ( -4.828169399223493308, -20.24070752338407431, 4.000000000000000000 ) ) ;
#4816 = EDGE_CURVE ( 'NONE', #92449, #102139, #93884, .T. ) ;
#4817 = AXIS2_PLACEMENT_3D ( 'NONE', #44668, #1087, #82110 ) ;
#4818 = LINE ( 'NONE', #115024, #1695 ) ;
#4819 = CARTESIAN_POINT ( 'NONE',  ( -19.93618820137057668, -0.2700000000508183118, -40.00000000000000000 ) ) ;
#4820 = ORIENTED_EDGE ( 'NONE', *, *, #45308, .F. ) ;
#4821 = VECTOR ( 'NONE', #121743, 1000.000000000000000 ) ;
#4822 = EDGE_CURVE ( 'NONE', #57169, #138815, #82914, .T. ) ;
#4823 = CARTESIAN_POINT ( 'NONE',  ( 75.18398860626899705, 28.73617430169839793, 5.000000000000000000 ) ) ;
#4824 = LINE ( 'NONE', #16438, #32892 ) ;
#4825 = ORIENTED_EDGE ( 'NONE', *, *, #119211, .T. ) ;
#4826 = EDGE_CURVE ( 'NONE', #124937, #24394, #54519, .T. ) ;
#4827 = CARTESIAN_POINT ( 'NONE',  ( -69.18398860626899705, 28.73617430169835529, 5.000000000000000000 ) ) ;
#4828 = PLANE ( 'NONE',  #64045 ) ;
#4829 = DIRECTION ( 'NONE',  ( -1.000000000000000000, 0.000000000000000000, 0.000000000000000000 ) ) ;
#4830 = AXIS2_PLACEMENT_3D ( 'NONE', #46369, #83983, #139785 ) ;
#4831 = ORIENTED_EDGE ( 'NONE', *, *, #48583, .F. ) ;
#4832 = ORIENTED_EDGE ( 'NONE', *, *, #81920, .T. ) ;
#4833 = EDGE_CURVE ( 'NONE', #117516, #62013, #142243, .T. ) ;
#4834 = CARTESIAN_POINT ( 'NONE',  ( 65.02083333333332860, 7.949999999999998401, 2.130196079827431532 ) ) ;
#4835 = ADVANCED_FACE ( 'NONE', ( #42928 ), #74853, .T. ) ;
#4836 = DIRECTION ( 'NONE',  ( -0.000000000000000000, -0.000000000000000000, -1.000000000000000000 ) ) ;
#4837 = DIRECTION ( 'NONE',  ( -0.7071067811865486830, -0.7071067811865464625, 0.000000000000000000 ) ) ;
#4838 = DIRECTION ( 'NONE',  ( 0.7071067811865487940, 0.7071067811865463515, 0.000000000000000000 ) ) ;
#4839 = VECTOR ( 'NONE', #21057, 1000.000000000000000 ) ;
#4840 = DIRECTION ( 'NONE',  ( -0.7071067811865486830, -0.7071067811865464625, 0.000000000000000000 ) ) ;
#4841 = EDGE_CURVE ( 'NONE', #122222, #29201, #103660, .T. ) ;
#4842 = PLANE ( 'NONE',  #34871 ) ;
#4843 = DIRECTION ( 'NONE',  ( 0.6830127018922181881, 0.6830127018922202975, -0.2588190451025214056 ) ) ;
#4844 =( LENGTH_UNIT ( ) NAMED_UNIT ( * ) SI_UNIT ( .MILLI., .METRE. ) );
#4845 = ORIENTED_EDGE ( 'NONE', *, *, #104548, .F. ) ;
#4846 = EDGE_LOOP ( 'NONE', ( #143192, #120180, #103402, #19787 ) ) ;
#4847 = ORIENTED_EDGE ( 'NONE', *, *, #19629, .T. ) ;
#4848 = VECTOR ( 'NONE', #9377, 1000.000000000000000 ) ;
#4849 = SURFACE_STYLE_USAGE ( .BOTH. , #94045 ) ;
#4850 = VECTOR ( 'NONE', #111353, 1000.000000000000000 ) ;
#4851 = VECTOR ( 'NONE', #84608, 1000.000000000000000 ) ;
#4852 = SURFACE_STYLE_USAGE ( .BOTH. , #70905 ) ;
#4853 = ORIENTED_EDGE ( 'NONE', *, *, #15862, .F. ) ;
#4854 = CARTESIAN_POINT ( 'NONE',  ( -18.48921356237309510, -27.52281430457068367, 5.000000000000000000 ) ) ;
#4855 = CARTESIAN_POINT ( 'NONE',  ( 51.18398860626899705, 28.73617430169823095, 5.000000000000000000 ) ) ;
#4856 = LINE ( 'NONE', #17215, #131362 ) ;
#4857 = EDGE_CURVE ( 'NONE', #65916, #20734, #119028, .T. ) ;
#4858 = CARTESIAN_POINT ( 'NONE',  ( -30.48921356237309510, -27.52281430457076894, 5.000000000000000000 ) ) ;
#4859 = VECTOR ( 'NONE', #60490, 1000.000000000000227 ) ;
#4860 = VECTOR ( 'NONE', #69626, 1000.000000000000000 ) ;
#4861 = PLANE ( 'NONE',  #16623 ) ;
#4862 = ORIENTED_EDGE ( 'NONE', *, *, #87078, .T. ) ;
#4863 = AXIS2_PLACEMENT_3D ( 'NONE', #7424, #29900, #104617 ) ;
#4864 = LINE ( 'NONE', #38267, #26349 ) ;
#4865 = DIRECTION ( 'NONE',  ( -0.3543493200069162685, -0.000000000000000000, -0.9351131265310288487 ) ) ;
#4866 = ORIENTED_EDGE ( 'NONE', *, *, #68990, .F. ) ;
#4867 = PLANE ( 'NONE',  #89890 ) ;
#4868 = ORIENTED_EDGE ( 'NONE', *, *, #4152, .F. ) ;
#4869 = ORIENTED_EDGE ( 'NONE', *, *, #126938, .F. ) ;
#4870 = LINE ( 'NONE', #13636, #126922 ) ;
#4871 = ORIENTED_EDGE ( 'NONE', *, *, #110987, .F. ) ;
#4872 = ORIENTED_EDGE ( 'NONE', *, *, #107178, .F. ) ;
#4873 = AXIS2_PLACEMENT_3D ( 'NONE', #124151, #79980, #135069 ) ;
#4874 = CARTESIAN_POINT ( 'NONE',  ( 73.50043019189811844, -3.055000000000002380, 5.291415217122920289 ) ) ;
#4875 = VERTEX_POINT ( 'NONE', #87126 ) ;
#4876 = EDGE_CURVE ( 'NONE', #13143, #22841, #63955, .T. ) ;
#4877 = CARTESIAN_POINT ( 'NONE',  ( 10.49999999999992539, -17.56887692260763245, 4.000000000000000000 ) ) ;
#4878 = CARTESIAN_POINT ( 'NONE',  ( -34.42500000000001137, -21.72500000000000142, 0.5000000000000000000 ) ) ;
#4879 = CARTESIAN_POINT ( 'NONE',  ( 106.0212635252314612, -4.472830434245838482, -4.472830434245840259 ) ) ;
#4880 = DIRECTION ( 'NONE',  ( 0.7071067811865486830, -0.7071067811865464625, -0.000000000000000000 ) ) ;
#4881 = AXIS2_PLACEMENT_3D ( 'NONE', #81237, #125441, #48585 ) ;
#4882 = EDGE_CURVE ( 'NONE', #77399, #102312, #27195, .T. ) ;
#4883 = CARTESIAN_POINT ( 'NONE',  ( 6.792893218813413014, -2.240707523384257716, 5.000000000000000000 ) ) ;
#4884 = PLANE ( 'NONE',  #83766 ) ;
#4885 = DIRECTION ( 'NONE',  ( 0.7071067811865487940, 0.7071067811865463515, 0.000000000000000000 ) ) ;
#4886 = CARTESIAN_POINT ( 'NONE',  ( 15.98155265364320599, 18.75929247661552424, 20.33588619593439617 ) ) ;
#4887 = CARTESIAN_POINT ( 'NONE',  ( 0.000000000000000000, 0.000000000000000000, 5.000000000000000000 ) ) ;
#4888 = VECTOR ( 'NONE', #71792, 999.9999999999998863 ) ;
#4889 = VERTEX_POINT ( 'NONE', #105458 ) ;
#4890 = VECTOR ( 'NONE', #118801, 1000.000000000000000 ) ;
#4891 = CARTESIAN_POINT ( 'NONE',  ( 25.65999999999999659, -2.055000000000000160, 2.789133085058098087E-16 ) ) ;
#4892 = EDGE_CURVE ( 'NONE', #120044, #21301, #98699, .T. ) ;
#4893 = EDGE_LOOP ( 'NONE', ( #25214, #21585, #93354, #119818 ) ) ;
#4894 = VECTOR ( 'NONE', #12759, 1000.000000000000000 ) ;
#4895 = ORIENTED_EDGE ( 'NONE', *, *, #8146, .F. ) ;
#4896 = DIRECTION ( 'NONE',  ( -0.000000000000000000, -0.3543493200069152693, 0.9351131265310292928 ) ) ;
#4897 = EDGE_LOOP ( 'NONE', ( #37398, #25632, #42473, #5261 ) ) ;
#4898 = VECTOR ( 'NONE', #87570, 1000.000000000000000 ) ;
#4899 = CARTESIAN_POINT ( 'NONE',  ( -1.499999999999994449, -11.56887692260769462, 4.000000000000000000 ) ) ;
#4900 = CARTESIAN_POINT ( 'NONE',  ( 42.29974487139158157, -27.71228299555235708, 4.000000000000000000 ) ) ;
#4901 = EDGE_CURVE ( 'NONE', #118694, #63182, #22629, .T. ) ;
#4902 = AXIS2_PLACEMENT_3D ( 'NONE', #131416, #32095, #98758 ) ;
#4903 = CARTESIAN_POINT ( 'NONE',  ( -24.18398860626899705, 28.73617430169804265, 5.000000000000000000 ) ) ;
#4904 = DIRECTION ( 'NONE',  ( -1.000000000000000000, -1.224606353822377258E-16, -0.000000000000000000 ) ) ;
#4905 = ORIENTED_EDGE ( 'NONE', *, *, #20259, .T. ) ;
#4906 = FILL_AREA_STYLE_COLOUR ( '', #83444 ) ;
#4907 = ORIENTED_EDGE ( 'NONE', *, *, #40155, .F. ) ;
#4908 = CARTESIAN_POINT ( 'NONE',  ( 4.000000000000000000, -8.616843969807042924, 0.000000000000000000 ) ) ;
#4909 = VECTOR ( 'NONE', #99023, 999.9999999999998863 ) ;
#4910 = CARTESIAN_POINT ( 'NONE',  ( 29.96290314143522338, -3.967499999999994476, 6.871911579029513106 ) ) ;
#4911 = CARTESIAN_POINT ( 'NONE',  ( -11.58838509405160089, 22.22500000000000142, 4.777194822843815025 ) ) ;
#4912 = CARTESIAN_POINT ( 'NONE',  ( 16.82816939922340893, -14.24070752338414003, 4.000000000000000000 ) ) ;
#4913 = DIRECTION ( 'NONE',  ( 1.000000000000000000, 0.000000000000000000, 0.000000000000000000 ) ) ;
#4914 = ORIENTED_EDGE ( 'NONE', *, *, #59458, .F. ) ;
#4915 = ORIENTED_EDGE ( 'NONE', *, *, #6267, .T. ) ;
#4916 = MECHANICAL_DESIGN_GEOMETRIC_PRESENTATION_REPRESENTATION (  '', ( #51342 ), #48971 ) ;
#4917 = VERTEX_POINT ( 'NONE', #138840 ) ;
#4918 = CARTESIAN_POINT ( 'NONE',  ( -34.91764015037184521, 21.81495039010403048, 4.089230673112417058 ) ) ;
#4919 = LINE ( 'NONE', #71667, #76558 ) ;
#4920 = DIRECTION ( 'NONE',  ( 0.6830127018922181881, 0.6830127018922202975, -0.2588190451025214056 ) ) ;
#4921 = VECTOR ( 'NONE', #11358, 1000.000000000000000 ) ;
#4922 = CARTESIAN_POINT ( 'NONE',  ( 21.32816939922338051, 17.25929247661554911, 4.000000000000000000 ) ) ;
#4923 = DIRECTION ( 'NONE',  ( 0.000000000000000000, -0.3543493200069152138, 0.9351131265310292928 ) ) ;
#4924 = CARTESIAN_POINT ( 'NONE',  ( 60.48921356237309510, -27.52281430457097500, 5.000000000000000000 ) ) ;
#4925 = LINE ( 'NONE', #128201, #16204 ) ;
#4926 = EDGE_CURVE ( 'NONE', #76525, #1885, #142929, .T. ) ;
#4928 = EDGE_CURVE ( 'NONE', #25784, #79543, #16298, .T. ) ;
#4927 = CARTESIAN_POINT ( 'NONE',  ( -34.92500000000001137, 21.72500000000000142, 5.000000000000000000 ) ) ;
#4929 = LINE ( 'NONE', #69557, #99758 ) ;
#4930 = ORIENTED_EDGE ( 'NONE', *, *, #59542, .T. ) ;
#4931 = LINE ( 'NONE', #73812, #108805 ) ;
#4932 = DIRECTION ( 'NONE',  ( -0.7071067811865486830, -0.7071067811865464625, 0.000000000000000000 ) ) ;
#4933 = VERTEX_POINT ( 'NONE', #41462 ) ;
#4934 = DIRECTION ( 'NONE',  ( -0.7071067811865486830, -0.7071067811865464625, 0.000000000000000000 ) ) ;
#4935 = ADVANCED_FACE ( 'NONE', ( #129913 ), #30622, .T. ) ;
#4936 = EDGE_LOOP ( 'NONE', ( #118566, #49439, #35449 ) ) ;
#4937 = ORIENTED_EDGE ( 'NONE', *, *, #118742, .F. ) ;
#4938 = EDGE_CURVE ( 'NONE', #92320, #48278, #68271, .T. ) ;
#4939 = DIRECTION ( 'NONE',  ( 0.7071067811865486830, -0.7071067811865464625, -0.000000000000000000 ) ) ;
#4940 = CARTESIAN_POINT ( 'NONE',  ( 27.18398860626900060, 28.73617430169806042, 5.000000000000000000 ) ) ;
#4941 = PLANE ( 'NONE',  #71498 ) ;
#4943 = ORIENTED_EDGE ( 'NONE', *, *, #37089, .T. ) ;
#4942 = AXIS2_PLACEMENT_3D ( 'NONE', #138775, #93824, #59105 ) ;
#4944 = CARTESIAN_POINT ( 'NONE',  ( 3.489213562373097322, -27.52281430457057709, 5.000000000000000000 ) ) ;
#4945 = ORIENTED_EDGE ( 'NONE', *, *, #20200, .T. ) ;
#4946 = CARTESIAN_POINT ( 'NONE',  ( -3.183988606268992161, 28.73617430169789699, 5.000000000000000000 ) ) ;
#4947 = CARTESIAN_POINT ( 'NONE',  ( 2.999999999999985345, 14.58746187583909837, 4.000000000000000000 ) ) ;
#4948 = CARTESIAN_POINT ( 'NONE',  ( 32.57876352523145158, -7.482591942790327058E-16, 6.109999999999999432 ) ) ;
#4949 = PLANE ( 'NONE',  #32364 ) ;
#4950 = PLANE ( 'NONE',  #50918 ) ;
#4951 = DIRECTION ( 'NONE',  ( 0.5735764363510451602, 0.8191520442889924647, 0.000000000000000000 ) ) ;
#4952 = CARTESIAN_POINT ( 'NONE',  ( -25.39999999999996305, 0.000000000000000000, 0.000000000000000000 ) ) ;
#4953 = CARTESIAN_POINT ( 'NONE',  ( -50.99451991528749062, 28.92564299267973738, 4.000000000000000000 ) ) ;
#4954 = CARTESIAN_POINT ( 'NONE',  ( 33.08290314143522437, 3.967499999999992699, -6.871911579029513994 ) ) ;
#4955 = CARTESIAN_POINT ( 'NONE',  ( 6.249569808101886004, 3.967499999999998916, 6.871911579029510442 ) ) ;
#4956 = LINE ( 'NONE', #17983, #78343 ) ;
#4957 = VECTOR ( 'NONE', #128029, 1000.000000000000000 ) ;
#4958 = AXIS2_PLACEMENT_3D ( 'NONE', #61170, #27762, #8125 ) ;
#4959 = CARTESIAN_POINT ( 'NONE',  ( 0.000000000000000000, 0.000000000000000000, 0.000000000000000000 ) ) ;
#4960 = CARTESIAN_POINT ( 'NONE',  ( -25.39656807105341585, -14.24070752338413648, 19.24067776001720276 ) ) ;
#4961 = ORIENTED_EDGE ( 'NONE', *, *, #73302, .T. ) ;
#4962 = EDGE_CURVE ( 'NONE', #110890, #87848, #134207, .T. ) ;
#4963 = ORIENTED_EDGE ( 'NONE', *, *, #113865, .T. ) ;
#4964 = CONICAL_SURFACE ( 'NONE', #32766, 1.898649999999993065, 1.029744258676648316 ) ;
#4965 = CARTESIAN_POINT ( 'NONE',  ( 94.04166666666665719, -3.975000000000002753, 6.884901960086286188 ) ) ;
#4966 = AXIS2_PLACEMENT_3D ( 'NONE', #39517, #15549, #61299 ) ;
#4967 = VERTEX_POINT ( 'NONE', #24013 ) ;
#4968 = ORIENTED_EDGE ( 'NONE', *, *, #9052, .T. ) ;
#4969 = DIRECTION ( 'NONE',  ( 0.7071067811865487940, 0.7071067811865463515, 0.000000000000000000 ) ) ;
#4970 = DIRECTION ( 'NONE',  ( -0.6830127018922180770, -0.6830127018922204085, -0.2588190451025213501 ) ) ;
#4971 = VECTOR ( 'NONE', #7647, 1000.000000000000000 ) ;
#4972 = AXIS2_PLACEMENT_3D ( 'NONE', #40516, #18716, #43364 ) ;
#4973 = VECTOR ( 'NONE', #97711, 999.9999999999998863 ) ;
#4974 = VECTOR ( 'NONE', #42535, 1000.000000000000000 ) ;
#4975 = DIRECTION ( 'NONE',  ( -0.6830127018922180770, -0.6830127018922204085, -0.2588190451025213501 ) ) ;
#4976 = ORIENTED_EDGE ( 'NONE', *, *, #117660, .F. ) ;
#4977 = CARTESIAN_POINT ( 'NONE',  ( 19.49999999999986855, -2.947814304570800736, 5.000000000000000000 ) ) ;
#4978 = VECTOR ( 'NONE', #128361, 999.9999999999998863 ) ;
#4979 = DIRECTION ( 'NONE',  ( 0.7071067811865487940, 0.7071067811865463515, 0.000000000000000000 ) ) ;
#4980 = DIRECTION ( 'NONE',  ( 0.2400000000000085398, 0.000000000000000000, -0.9707728879609256456 ) ) ;
#4981 = CARTESIAN_POINT ( 'NONE',  ( 126.5282371893278537, 6.759817336840661106, 1.509802715116372207 ) ) ;
#4982 = LINE ( 'NONE', #83315, #44758 ) ;
#4983 = CARTESIAN_POINT ( 'NONE',  ( 34.92499999999998295, 15.75929247661555799, 4.255531930566167631 ) ) ;
#4984 = STYLED_ITEM ( 'NONE', ( #104537 ), #141940 ) ;
#4985 = LINE ( 'NONE', #115178, #70700 ) ;
#4986 = DIRECTION ( 'NONE',  ( 1.000000000000000000, 0.000000000000000000, 0.000000000000000000 ) ) ;
#4987 = FACE_OUTER_BOUND ( 'NONE', #112065, .T. ) ;
#4988 = FACE_OUTER_BOUND ( 'NONE', #136907, .T. ) ;
#4989 = ORIENTED_EDGE ( 'NONE', *, *, #9632, .F. ) ;
#4990 = ORIENTED_EDGE ( 'NONE', *, *, #122325, .F. ) ;
#4991 = EDGE_CURVE ( 'NONE', #100625, #72772, #21859, .T. ) ;
#4992 = CARTESIAN_POINT ( 'NONE',  ( 114.9170968585647756, 3.054999999999998828, 5.291415217122922066 ) ) ;
#4993 = ORIENTED_EDGE ( 'NONE', *, *, #113814, .F. ) ;
#4994 = EDGE_CURVE ( 'NONE', #50737, #5604, #132808, .T. ) ;
#4995 = LINE ( 'NONE', #83330, #119465 ) ;
#4996 = ORIENTED_EDGE ( 'NONE', *, *, #12227, .T. ) ;
#4997 = EDGE_CURVE ( 'NONE', #97211, #48429, #13106, .T. ) ;
#4998 = ADVANCED_FACE ( 'NONE', ( #11664 ), #87833, .F. ) ;
#4999 = FACE_OUTER_BOUND ( 'NONE', #90771, .T. ) ;
#5000 = DIRECTION ( 'NONE',  ( 0.000000000000000000, 0.000000000000000000, 1.000000000000000000 ) ) ;
#5001 = VECTOR ( 'NONE', #142220, 1000.000000000000227 ) ;
#5002 = AXIS2_PLACEMENT_3D ( 'NONE', #82997, #40230, #17020 ) ;
#5003 = CARTESIAN_POINT ( 'NONE',  ( 107.6829301918981088, -1.637169565754158951, -6.109999999999998543 ) ) ;
#5004 = ORIENTED_EDGE ( 'NONE', *, *, #11407, .T. ) ;
#5005 = VECTOR ( 'NONE', #84320, 1000.000000000000227 ) ;
#5006 = LINE ( 'NONE', #137729, #109029 ) ;
#5007 = ORIENTED_EDGE ( 'NONE', *, *, #60542, .T. ) ;
#5008 = DIRECTION ( 'NONE',  ( -0.000000000000000000, -0.3543493200069152693, 0.9351131265310292928 ) ) ;
#5009 = FILL_AREA_STYLE ('',( #59471 ) ) ;
#5010 = VECTOR ( 'NONE', #109685, 1000.000000000000000 ) ;
#5011 = CARTESIAN_POINT ( 'NONE',  ( 32.20666063542130075, 21.75929247661549937, 4.998822639870702744 ) ) ;
#5012 = ORIENTED_EDGE ( 'NONE', *, *, #123732, .T. ) ;
#5013 = VERTEX_POINT ( 'NONE', #56687 ) ;
#5014 = EDGE_CURVE ( 'NONE', #70001, #22050, #132075, .T. ) ;
#5015 = EDGE_LOOP ( 'NONE', ( #5266, #52642, #35865, #42399 ) ) ;
#5016 = CARTESIAN_POINT ( 'NONE',  ( -21.65671000166199889, 3.759292476615678336, 13.27625715073260615 ) ) ;
#5017 = EDGE_CURVE ( 'NONE', #71118, #141981, #23265, .T. ) ;
#5018 = CARTESIAN_POINT ( 'NONE',  ( -18.29974487139159223, -27.71228299555219010, 4.000000000000000000 ) ) ;
#5019 = CARTESIAN_POINT ( 'NONE',  ( 8.962903141435219823, -3.967499999999994476, 6.871911579029513106 ) ) ;
#5020 = VECTOR ( 'NONE', #139567, 999.9999999999998863 ) ;
#5021 = CARTESIAN_POINT ( 'NONE',  ( 21.29166666666666785, -3.047499999999994547, 5.278424836066145431 ) ) ;
#5022 = EDGE_CURVE ( 'NONE', #97224, #124154, #2208, .T. ) ;
#5023 = CARTESIAN_POINT ( 'NONE',  ( 15.29974487139158867, -27.71228299555216879, 4.000000000000000000 ) ) ;
#5024 = ORIENTED_EDGE ( 'NONE', *, *, #57313, .F. ) ;
#5025 = EDGE_LOOP ( 'NONE', ( #10485, #114535, #24984, #19673 ) ) ;
#5026 = DIRECTION ( 'NONE',  ( -0.3543493200069162685, -0.000000000000000000, -0.9351131265310288487 ) ) ;
#5027 = ORIENTED_EDGE ( 'NONE', *, *, #30389, .F. ) ;
#5028 = EDGE_LOOP ( 'NONE', ( #122163, #39685, #104539, #11677, #34961 ) ) ;
#5029 = AXIS2_PLACEMENT_3D ( 'NONE', #101497, #125411, #48559 ) ;
#5030 = EDGE_CURVE ( 'NONE', #53957, #2777, #59742, .T. ) ;
#5031 = VECTOR ( 'NONE', #85747, 1000.000000000000000 ) ;
#5032 = DIRECTION ( 'NONE',  ( 0.7071067811865487940, -0.7071067811865463515, 0.000000000000000000 ) ) ;
#5033 = PLANE ( 'NONE',  #134519 ) ;
#5034 = CARTESIAN_POINT ( 'NONE',  ( 21.80077440930739030, -2.123201397992801276, 4.669108085256719498 ) ) ;
#5035 = ORIENTED_EDGE ( 'NONE', *, *, #86316, .F. ) ;
#5036 = CARTESIAN_POINT ( 'NONE',  ( -51.48921356237309510, -27.52281430457091460, 5.000000000000000000 ) ) ;
#5037 = CARTESIAN_POINT ( 'NONE',  ( 9.591592354503321260, -2.500000000000000000, 3.061616997868384127E-16 ) ) ;
#5038 = ADVANCED_FACE ( 'NONE', ( #90710 ), #121865, .F. ) ;
#5039 = VECTOR ( 'NONE', #142806, 1000.000000000000227 ) ;
#5040 = DIRECTION ( 'NONE',  ( -2.781805975412905890E-17, 0.3543493200069152693, 0.9351131265310292928 ) ) ;
#5041 = CARTESIAN_POINT ( 'NONE',  ( 69.18398860626899705, 28.73617430169835529, 5.000000000000000000 ) ) ;
#5042 = ORIENTED_EDGE ( 'NONE', *, *, #23885, .F. ) ;
#5043 = DIRECTION ( 'NONE',  ( 0.7071067811865486830, -0.7071067811865464625, -0.000000000000000000 ) ) ;
#5044 = FACE_BOUND ( 'NONE', #4353, .T. ) ;
#5045 = ORIENTED_EDGE ( 'NONE', *, *, #139599, .F. ) ;
#5046 = LINE ( 'NONE', #127587, #18013 ) ;
#5047 = FACE_OUTER_BOUND ( 'NONE', #84772, .T. ) ;
#5048 = CARTESIAN_POINT ( 'NONE',  ( 131.5423521607622490, -49.05583548141700589, 39.86617647058822911 ) ) ;
#5049 = VERTEX_POINT ( 'NONE', #66803 ) ;
#5050 = EDGE_CURVE ( 'NONE', #10646, #130556, #79865, .T. ) ;
#5051 = CARTESIAN_POINT ( 'NONE',  ( -12.48921356237309155, -27.52281430457064104, 5.000000000000000000 ) ) ;
#5052 = EDGE_LOOP ( 'NONE', ( #34752, #109750, #16074, #88777 ) ) ;
#5053 = EDGE_CURVE ( 'NONE', #114924, #119580, #110275, .T. ) ;
#5054 = ORIENTED_EDGE ( 'NONE', *, *, #56782, .F. ) ;
#5055 = CONICAL_SURFACE ( 'NONE', #67642, 2.247899999999995568, 1.029744258676650315 ) ;
#5056 = ORIENTED_EDGE ( 'NONE', *, *, #119766, .F. ) ;
#5057 = EDGE_CURVE ( 'NONE', #104233, #53420, #110982, .T. ) ;
#5058 = CARTESIAN_POINT ( 'NONE',  ( 34.32876352523143737, 0.000000000000000000, -6.109999999999998543 ) ) ;
#5059 = ORIENTED_EDGE ( 'NONE', *, *, #104423, .T. ) ;
#5060 = DIRECTION ( 'NONE',  ( -1.000000000000000000, 0.000000000000000000, 0.000000000000000000 ) ) ;
#5061 = CARTESIAN_POINT ( 'NONE',  ( -18.29974487139159223, -27.71228299555219010, 4.000000000000000000 ) ) ;
#5062 = DIRECTION ( 'NONE',  ( -1.000000000000000000, -1.224606353822377258E-16, -0.000000000000000000 ) ) ;
#5063 = ORIENTED_EDGE ( 'NONE', *, *, #50610, .F. ) ;
#5064 = DIRECTION ( 'NONE',  ( -0.6830127018922180770, -0.6830127018922204085, -0.2588190451025213501 ) ) ;
#5065 = CONICAL_SURFACE ( 'NONE', #104651, 2.055000000000000604, 0.9599310885968764806 ) ;
#5066 = VECTOR ( 'NONE', #121188, 1000.000000000000000 ) ;
#5067 = VECTOR ( 'NONE', #73198, 1000.000000000000227 ) ;
#5068 = AXIS2_PLACEMENT_3D ( 'NONE', #42939, #87139, #131356 ) ;
#5069 = AXIS2_PLACEMENT_3D ( 'NONE', #21125, #42911, #74835 ) ;
#5070 = CARTESIAN_POINT ( 'NONE',  ( 34.82816939922328459, -11.24070752338417201, 4.000000000000000000 ) ) ;
#5071 = CARTESIAN_POINT ( 'NONE',  ( 34.04515773336645879, -21.74070752338406365, 21.72585301388592782 ) ) ;
#5072 = CARTESIAN_POINT ( 'NONE',  ( 18.29974487139159223, -27.71228299555219010, 4.000000000000000000 ) ) ;
#5073 = DIRECTION ( 'NONE',  ( -0.7071067811865486830, 0.7071067811865464625, 0.000000000000000000 ) ) ;
#5074 = ORIENTED_EDGE ( 'NONE', *, *, #48069, .F. ) ;
#5075 = EDGE_LOOP ( 'NONE', ( #43962, #102032, #21753, #7868, #81885, #110574, #66481, #71563, #88514, #84377, #113352, #35214, #62901, #23789, #945, #61389, #32422, #17877, #138049, #20012, #7582, #26219, #132492, #90114, #48275, #76497, #130553, #17107, #35980, #140198, #51998, #25018, #29237, #75805, #2145, #43933, #79853, #16251, #110508, #65189, #43334, #28756, #34859, #12466, #82071, #37964, #28910, #33171, #112106, #103810, #118441, #65019, #130644, #123819, #7352, #10792, #38255, #21010, #44210, #101201, #35923, #134125, #61518, #129303, #112630, #43540, #125019, #27182, #10834, #653, #91923, #107581, #46083, #130250, #118768, #98053, #76634, #17868, #138778, #113998, #66545, #25420, #28639, #132089, #18113, #124048, #25466, #115707, #55065, #107145, #61627, #101723, #34405, #103476, #81659, #3587, #99349, #11143, #41235, #8021, #28250, #46516, #84487, #57825, #108478, #127543, #131389, #15207, #82547, #78696, #139493, #84761, #32497, #60032, #143120, #117415, #123931, #48519, #123339, #133638, #102849, #53887, #19933, #3506, #87387, #21222, #3346, #112048, #110327, #78204, #29727, #29770, #103652, #7458, #111640, #43577, #45527, #130292, #67937, #111937, #127692, #38860, #100498, #124800, #34356, #137483, #18158, #59908, #86150, #26792, #108111, #21664, #126913, #117587, #9653, #83755, #105306, #136892, #100468, #120161, #108972, #20022, #128549, #14139 ) ) ;
#5076 = VECTOR ( 'NONE', #133769, 1000.000000000000000 ) ;
#5077 = ORIENTED_EDGE ( 'NONE', *, *, #125803, .F. ) ;
#5078 = CIRCLE ( 'NONE', #116157, 2.500000000000000444 ) ;
#5079 = ORIENTED_EDGE ( 'NONE', *, *, #96343, .F. ) ;
#5080 = DIRECTION ( 'NONE',  ( 0.000000000000000000, -0.000000000000000000, 1.000000000000000000 ) ) ;
#5081 = ORIENTED_EDGE ( 'NONE', *, *, #46857, .F. ) ;
#5082 = VERTEX_POINT ( 'NONE', #24712 ) ;
#5083 = LINE ( 'NONE', #72578, #51321 ) ;
#5084 = ADVANCED_FACE ( 'NONE', ( #100150 ), #122589, .F. ) ;
#5085 = CARTESIAN_POINT ( 'NONE',  ( 6.394038684143281692, 22.22500000000000142, 20.65732834419774377 ) ) ;
#5086 = ORIENTED_EDGE ( 'NONE', *, *, #50342, .T. ) ;
#5087 = CARTESIAN_POINT ( 'NONE',  ( 10.37159235450332062, 9.902892378096218942E-16, 0.000000000000000000 ) ) ;
#5088 = VERTEX_POINT ( 'NONE', #71816 ) ;
#5089 = DIRECTION ( 'NONE',  ( 0.7071067811865487940, 0.7071067811865463515, 0.000000000000000000 ) ) ;
#5090 = CARTESIAN_POINT ( 'NONE',  ( 10.49999999999993605, 13.08746187583911080, 4.000000000000000000 ) ) ;
#5091 = CARTESIAN_POINT ( 'NONE',  ( 3.421236474768552860, -9.717572351234235426E-16, -7.934999999999990727 ) ) ;
#5092 = VERTEX_POINT ( 'NONE', #16686 ) ;
#5094 = CARTESIAN_POINT ( 'NONE',  ( 22.17183060077631396, -17.24070752338410628, 4.000000000000000000 ) ) ;
#5093 = CARTESIAN_POINT ( 'NONE',  ( 100.5370968585647802, -3.054999999999999272, -5.291415217122919401 ) ) ;
#5095 =( NAMED_UNIT ( * ) SI_UNIT ( $, .STERADIAN. ) SOLID_ANGLE_UNIT ( ) );
#5096 = LINE ( 'NONE', #61001, #46565 ) ;
#5097 = ORIENTED_EDGE ( 'NONE', *, *, #141166, .F. ) ;
#5098 = VERTEX_POINT ( 'NONE', #5786 ) ;
#5099 = DIRECTION ( 'NONE',  ( 1.000000000000000000, 0.000000000000000000, 0.000000000000000000 ) ) ;
#5100 = VERTEX_POINT ( 'NONE', #2952 ) ;
#5101 = FACE_OUTER_BOUND ( 'NONE', #25965, .T. ) ;
#5102 = FILL_AREA_STYLE_COLOUR ( '', #42754 ) ;
#5103 = LINE ( 'NONE', #58877, #37724 ) ;
#5104 = CARTESIAN_POINT ( 'NONE',  ( 183.9400257540259531, -51.66308182546809746, -38.35990878063539355 ) ) ;
#5105 = ORIENTED_EDGE ( 'NONE', *, *, #116509, .T. ) ;
#5106 = AXIS2_PLACEMENT_3D ( 'NONE', #28098, #30230, #18614 ) ;
#5107 = DIRECTION ( 'NONE',  ( 0.7071067811865487940, 0.7071067811865463515, 0.000000000000000000 ) ) ;
#5108 = VECTOR ( 'NONE', #105783, 1000.000000000000000 ) ;
#5109 = AXIS2_PLACEMENT_3D ( 'NONE', #47096, #124590, #108503 ) ;
#5110 = CARTESIAN_POINT ( 'NONE',  ( 14.51078643762690490, -27.52281430457045275, 5.000000000000000000 ) ) ;
#5111 = CARTESIAN_POINT ( 'NONE',  ( 21.18398860626899349, 28.73617430169802134, 5.000000000000000000 ) ) ;
#5112 = EDGE_LOOP ( 'NONE', ( #125094, #75208, #103008, #52872 ) ) ;
#5113 = CARTESIAN_POINT ( 'NONE',  ( -13.08316395874281568, 3.014287036135060660, 4.000000000000000000 ) ) ;
#5114 = AXIS2_PLACEMENT_3D ( 'NONE', #44288, #78329, #2141 ) ;
#5115 = DIRECTION ( 'NONE',  ( 0.6830127018922181881, 0.6830127018922202975, -0.2588190451025214056 ) ) ;
#5116 = ORIENTED_EDGE ( 'NONE', *, *, #30766, .T. ) ;
#5117 = ADVANCED_FACE ( 'NONE', ( #15237 ), #37016, .F. ) ;
#5119 = ORIENTED_EDGE ( 'NONE', *, *, #142151, .F. ) ;
#5118 = PLANE ( 'NONE',  #6944 ) ;
#5121 = VERTEX_POINT ( 'NONE', #81997 ) ;
#5120 = ADVANCED_FACE ( 'NONE', ( #36319 ), #48617, .F. ) ;
#5122 = CARTESIAN_POINT ( 'NONE',  ( -27.18398860626900060, 28.73617430169806042, 5.000000000000000000 ) ) ;
#5123 = CARTESIAN_POINT ( 'NONE',  ( -16.49999999999987566, -2.947814304570798960, 5.000000000000000000 ) ) ;
#5124 = STYLED_ITEM ( 'NONE', ( #127792 ), #25975 ) ;
#5125 = ORIENTED_EDGE ( 'NONE', *, *, #126744, .F. ) ;
#5126 = DIRECTION ( 'NONE',  ( -0.000000000000000000, 0.3543493200069152138, -0.9351131265310292928 ) ) ;
#5127 = CARTESIAN_POINT ( 'NONE',  ( -23.99999999999982947, -21.41253812416053748, 4.000000000000000000 ) ) ;
#5128 = LINE ( 'NONE', #5850, #103938 ) ;
#5129 = ORIENTED_EDGE ( 'NONE', *, *, #84871, .T. ) ;
#5130 = EDGE_CURVE ( 'NONE', #764, #19509, #55072, .T. ) ;
#5131 = CARTESIAN_POINT ( 'NONE',  ( 34.92500000000001847, 2.730000000000007976, -36.39086428169088094 ) ) ;
#5132 = CARTESIAN_POINT ( 'NONE',  ( 26.70025512860841488, -27.71228299555187391, 4.000000000000000000 ) ) ;
#5133 = CARTESIAN_POINT ( 'NONE',  ( -6.792893218813407685, -17.24070752338409918, 5.000000000000000000 ) ) ;
#5134 = LINE ( 'NONE', #28368, #400 ) ;
#5135 = VECTOR ( 'NONE', #21472, 1000.000000000000000 ) ;
#5136 = CYLINDRICAL_SURFACE ( 'NONE', #12259, 6.094999999999989093 ) ;
#5137 = DIRECTION ( 'NONE',  ( -0.6830127018922181881, 0.6830127018922202975, -0.2588190451025214056 ) ) ;
#5138 = VECTOR ( 'NONE', #89169, 1000.000000000000000 ) ;
#5139 = DIRECTION ( 'NONE',  ( 0.6830127018922181881, 0.6830127018922202975, -0.2588190451025214056 ) ) ;
#5140 = CARTESIAN_POINT ( 'NONE',  ( 56.99451991528749062, 28.92564299267978001, 4.000000000000000000 ) ) ;
#5141 = CARTESIAN_POINT ( 'NONE',  ( 24.39999999999999858, -2.600000000000013856, 20.40202195861968448 ) ) ;
#5142 = ORIENTED_EDGE ( 'NONE', *, *, #104313, .T. ) ;
#5143 = EDGE_CURVE ( 'NONE', #60071, #48370, #140733, .T. ) ;
#5144 = ORIENTED_EDGE ( 'NONE', *, *, #23139, .T. ) ;
#5145 = VERTEX_POINT ( 'NONE', #60970 ) ;
#5146 = CARTESIAN_POINT ( 'NONE',  ( 118.3958333333333286, -2.130196079827427091, 7.949999999999999289 ) ) ;
#5147 = ORIENTED_EDGE ( 'NONE', *, *, #141225, .F. ) ;
#5148 = ORIENTED_EDGE ( 'NONE', *, *, #4822, .T. ) ;
#5149 = ORIENTED_EDGE ( 'NONE', *, *, #29661, .T. ) ;
#5150 = AXIS2_PLACEMENT_3D ( 'NONE', #129062, #76125, #42804 ) ;
#5151 = CARTESIAN_POINT ( 'NONE',  ( 2.999999999999976907, -21.03360074219752462, 5.000000000000000000 ) ) ;
#5152 = CARTESIAN_POINT ( 'NONE',  ( -27.48921356237309155, -27.52281430457074762, 5.000000000000000000 ) ) ;
#5153 = EDGE_CURVE ( 'NONE', #69796, #12358, #105130, .T. ) ;
#5154 = AXIS2_PLACEMENT_3D ( 'NONE', #122356, #67304, #78180 ) ;
#5155 = EDGE_CURVE ( 'NONE', #12589, #93689, #8620, .T. ) ;
#5156 = ORIENTED_EDGE ( 'NONE', *, *, #65784, .T. ) ;
#5157 = CARTESIAN_POINT ( 'NONE',  ( 4.658131166821905644, 2.500000000000001776, 3.061616997868385113E-16 ) ) ;
#5158 = LINE ( 'NONE', #3722, #125018 ) ;
#5159 = DIRECTION ( 'NONE',  ( 0.000000000000000000, -1.000000000000000000, 0.000000000000000000 ) ) ;
#5160 = CARTESIAN_POINT ( 'NONE',  ( 115.5004301918981042, -3.055000000000002380, 5.291415217122920289 ) ) ;
#5161 = EDGE_LOOP ( 'NONE', ( #133934, #96863, #25673, #79675 ) ) ;
#5162 = CARTESIAN_POINT ( 'NONE',  ( 54.48921356237310221, -27.52281430457093236, 5.000000000000000000 ) ) ;
#5163 = CARTESIAN_POINT ( 'NONE',  ( 106.1000270504628986, 5.819803920172570422, 5.819803920172575751 ) ) ;
#5165 = AXIS2_PLACEMENT_3D ( 'NONE', #117507, #137881, #71926 ) ;
#5164 = CARTESIAN_POINT ( 'NONE',  ( 0.000000000000000000, -34.64999999999999147, -39.50000000000000000 ) ) ;
#5166 = PLANE ( 'NONE',  #128497 ) ;
#5167 = LINE ( 'NONE', #16036, #30677 ) ;
#5168 = CARTESIAN_POINT ( 'NONE',  ( 60.18398860626900415, 28.73617430169829490, 5.000000000000000000 ) ) ;
#5169 = CARTESIAN_POINT ( 'NONE',  ( 34.20419371712955581, -6.884901960086285300, -3.975000000000000089 ) ) ;
#5170 = LINE ( 'NONE', #107370, #137004 ) ;
#5171 = CARTESIAN_POINT ( 'NONE',  ( -14.99999999999990230, 8.587461875839165870, 4.000000000000000000 ) ) ;
#5172 = ORIENTED_EDGE ( 'NONE', *, *, #88595, .F. ) ;
#5173 = EDGE_LOOP ( 'NONE', ( #99987, #77473 ) ) ;
#5174 = CARTESIAN_POINT ( 'NONE',  ( 38.91666666666665719, -6.884901960086287076, -3.975000000000000977 ) ) ;
#5175 = ORIENTED_EDGE ( 'NONE', *, *, #110228, .F. ) ;
#5176 = VERTEX_POINT ( 'NONE', #9340 ) ;
#5177 = FACE_OUTER_BOUND ( 'NONE', #82518, .T. ) ;
#5178 = EDGE_CURVE ( 'NONE', #1349, #124601, #118858, .T. ) ;
#5179 = LINE ( 'NONE', #117518, #108024 ) ;
#5180 = ORIENTED_EDGE ( 'NONE', *, *, #57135, .F. ) ;
#5181 = VECTOR ( 'NONE', #111797, 1000.000000000000000 ) ;
#5182 = CIRCLE ( 'NONE', #109314, 2.500000000000000888 ) ;
#5183 = VECTOR ( 'NONE', #64820, 1000.000000000000000 ) ;
#5184 = DIRECTION ( 'NONE',  ( 1.000000000000000000, 0.000000000000000000, 0.000000000000000000 ) ) ;
#5186 = ADVANCED_FACE ( 'NONE', ( #84130 ), #84809, .F. ) ;
#5185 = DIRECTION ( 'NONE',  ( -0.000000000000000000, 0.3543493200069153248, 0.9351131265310292928 ) ) ;
#5188 = ADVANCED_FACE ( 'NONE', ( #128332 ), #75373, .F. ) ;
#5187 = AXIS2_PLACEMENT_3D ( 'NONE', #143136, #88047, #132299 ) ;
#5189 = FACE_OUTER_BOUND ( 'NONE', #140682, .T. ) ;
#5191 = VECTOR ( 'NONE', #9327, 1000.000000000000000 ) ;
#5190 =( NAMED_UNIT ( * ) SI_UNIT ( $, .STERADIAN. ) SOLID_ANGLE_UNIT ( ) );
#5192 = CARTESIAN_POINT ( 'NONE',  ( 27.70876352523143993, -7.482591942790329030E-16, 6.110000000000001208 ) ) ;
#5193 = B_SPLINE_CURVE_WITH_KNOTS ( 'NONE', 3,
 ( #47167, #70333, #57298, #3560, #125387, #12320, #124657, #102217, #134861, #69600, #114479, #48527, #58017, #1421, #90622, #102919, #47856, #4230, #134124, #24627, #80467, #92728, #136967, #113785, #35555, #122499, #46435, #25333, #2869, #91346, #26072, #23175, #14474, #113052, #135556, #13725 ),
 .UNSPECIFIED., .F., .F.,
 ( 4, 2, 2, 2, 2, 2, 2, 2, 2, 2, 2, 2, 2, 2, 2, 2, 2, 4 ),
 ( 0.01387570424127936193, 0.01474184239350130252, 0.01560798054572324310, 0.01647411869794518369, 0.01734025685016712254, 0.01820639500238906486, 0.01907253315461100718, 0.01993867130683294603, 0.02037174038294391545, 0.02080480945905488488, 0.02167094761127682373, 0.02253708576349876258, 0.02340322391572070490, 0.02426936206794264722, 0.02513550022016458607, 0.02600163837238652492, 0.02686777652460846724, 0.02773391467683040609 ),
 .UNSPECIFIED. ) ;
#5194 = VERTEX_POINT ( 'NONE', #94947 ) ;
#5195 = CARTESIAN_POINT ( 'NONE',  ( 7.828169399223478209, 18.75929247661553134, 4.000000000000000000 ) ) ;
#5196 = ORIENTED_EDGE ( 'NONE', *, *, #111600, .T. ) ;
#5197 = VECTOR ( 'NONE', #36566, 999.9999999999998863 ) ;
#5198 = MECHANICAL_DESIGN_GEOMETRIC_PRESENTATION_REPRESENTATION (  '', ( #44598 ), #81624 ) ;
#5199 = PLANE ( 'NONE',  #96088 ) ;
#5200 = ADVANCED_FACE ( 'NONE', ( #50758 ), #31163, .F. ) ;
#5201 = FACE_OUTER_BOUND ( 'NONE', #50065, .T. ) ;
#5202 = CARTESIAN_POINT ( 'NONE',  ( -25.49999999999982236, -6.839392718269155402, -8.480912228396030983 ) ) ;
#5203 = FACE_OUTER_BOUND ( 'NONE', #73505, .T. ) ;
#5204 = EDGE_LOOP ( 'NONE', ( #126905, #63380, #79758, #78840 ) ) ;
#5206 = EDGE_CURVE ( 'NONE', #1885, #45596, #78255, .T. ) ;
#5205 = CARTESIAN_POINT ( 'NONE',  ( 51.18793019189810423, 6.110000000000002984, -1.637169565754156730 ) ) ;
#5207 = EDGE_LOOP ( 'NONE', ( #68193, #57456, #33431, #64376 ) ) ;
#5208 = DIRECTION ( 'NONE',  ( 0.6830127018922180770, -0.6830127018922204085, -0.2588190451025213501 ) ) ;
#5209 = ADVANCED_FACE ( 'NONE', ( #139217 ), #117406, .T. ) ;
#5210 = DIRECTION ( 'NONE',  ( -0.7071067811865486830, -0.7071067811865464625, -0.000000000000000000 ) ) ;
#5211 = LINE ( 'NONE', #70548, #142688 ) ;
#5212 = CARTESIAN_POINT ( 'NONE',  ( 3.005480084712505828, 28.92564299267936079, 4.000000000000000000 ) ) ;
#5213 = EDGE_CURVE ( 'NONE', #136929, #78067, #30436, .T. ) ;
#5214 = VECTOR ( 'NONE', #12643, 999.9999999999998863 ) ;
#5215 = EDGE_CURVE ( 'NONE', #98856, #139660, #53624, .T. ) ;
#5216 = CARTESIAN_POINT ( 'NONE',  ( 49.64126352523145158, 4.472830434245836706, 4.472830434245840259 ) ) ;
#5217 = EDGE_LOOP ( 'NONE', ( #1220, #58444, #7138, #128696 ) ) ;
#5218 = FACE_OUTER_BOUND ( 'NONE', #103278, .T. ) ;
#5219 = CARTESIAN_POINT ( 'NONE',  ( 32.67183060077624646, 8.259292476615641476, 4.000000000000000000 ) ) ;
#5220 = VERTEX_POINT ( 'NONE', #142071 ) ;
#5221 = EDGE_LOOP ( 'NONE', ( #19398, #116849, #39864, #109067 ) ) ;
#5222 = CARTESIAN_POINT ( 'NONE',  ( 27.18398860626900060, 28.73617430169806042, 5.000000000000000000 ) ) ;
#5223 = EDGE_CURVE ( 'NONE', #141807, #10669, #51480, .T. ) ;
#5224 = EDGE_LOOP ( 'NONE', ( #140424, #133525, #137951, #17815 ) ) ;
#5225 = COLOUR_RGB ( '', 0.08235294, 0.09019608, 0.10196078) ;
#5226 = CARTESIAN_POINT ( 'NONE',  ( 60.16252705046289151, 7.949999999999998401, 1.460391307983218338E-15 ) ) ;
#5227 = UNCERTAINTY_MEASURE_WITH_UNIT (LENGTH_MEASURE( 1.000000000000000082E-05 ), #53393, 'distance_accuracy_value', 'NONE');
#5228 = ORIENTED_EDGE ( 'NONE', *, *, #117649, .T. ) ;
#5229 = VECTOR ( 'NONE', #89646, 1000.000000000000000 ) ;
#5230 = LINE ( 'NONE', #62511, #25199 ) ;
#5231 = CARTESIAN_POINT ( 'NONE',  ( 0.000000000000000000, -60.00000000000000000, 0.000000000000000000 ) ) ;
#5232 = EDGE_CURVE ( 'NONE', #14025, #122052, #42038, .T. ) ;
#5233 = LINE ( 'NONE', #69845, #249 ) ;
#5234 = FACE_BOUND ( 'NONE', #17612, .T. ) ;
#5235 = DIRECTION ( 'NONE',  ( -1.000000000000000000, 0.000000000000000000, -0.000000000000000000 ) ) ;
#5236 = LINE ( 'NONE', #93707, #57273 ) ;
#5237 = EDGE_LOOP ( 'NONE', ( #98325, #60848, #131880, #72364 ) ) ;
#5238 = DIRECTION ( 'NONE',  ( 1.000000000000000000, 0.000000000000000000, 0.000000000000000000 ) ) ;
#5240 = VERTEX_POINT ( 'NONE', #42762 ) ;
#5239 = FACE_OUTER_BOUND ( 'NONE', #99203, .T. ) ;
#5241 = EDGE_CURVE ( 'NONE', #40729, #118475, #6477, .T. ) ;
#5242 = DIRECTION ( 'NONE',  ( -0.3543493200069162685, -0.000000000000000000, -0.9351131265310288487 ) ) ;
#5243 = ORIENTED_EDGE ( 'NONE', *, *, #76814, .F. ) ;
#5244 = EDGE_CURVE ( 'NONE', #4593, #84994, #73935, .T. ) ;
#5245 = EDGE_CURVE ( 'NONE', #45336, #104888, #63088, .T. ) ;
#5246 = ORIENTED_EDGE ( 'NONE', *, *, #129800, .T. ) ;
#5247 = CARTESIAN_POINT ( 'NONE',  ( 64.66209685856478018, -5.291415217122919401, 3.054999999999997939 ) ) ;
#5248 = ORIENTED_EDGE ( 'NONE', *, *, #43692, .F. ) ;
#5249 =( BOUNDED_CURVE ( )  B_SPLINE_CURVE ( 2, ( #85438, #105068, #60907, #49997, #94180, #17343, #97004, #128962, #18019, #19487, #73185, #84072, #129666 ),
 .UNSPECIFIED., .F., .T. ) 
 B_SPLINE_CURVE_WITH_KNOTS ( ( 3, 2, 2, 2, 2, 2, 3 ),
 ( 0.4833333333333333370, 0.4861111111111111049, 0.4888888888888888729, 0.4916666666666666408, 0.4944444444444444642, 0.4972222222222222321, 0.5000000000000000000 ),
 .UNSPECIFIED. ) 
 CURVE ( )  GEOMETRIC_REPRESENTATION_ITEM ( )  RATIONAL_B_SPLINE_CURVE ( ( 1.000000000000000000, 0.9659258262890683122, 1.000000000000000000, 0.9659258262890683122, 1.000000000000000000, 0.9659258262890683122, 1.000000000000000000, 0.9659258262890683122, 1.000000000000000000, 0.9659258262890683122, 1.000000000000000000, 0.9659258262890683122, 1.000000000000000000 ) ) 
 REPRESENTATION_ITEM ( '' )  );
#5250 = CARTESIAN_POINT ( 'NONE',  ( -29.99999999999978684, -7.068876922607743474, 4.000000000000000000 ) ) ;
#5251 = DIRECTION ( 'NONE',  ( -0.6830127018922181881, 0.6830127018922202975, -0.2588190451025214056 ) ) ;
#5252 = VECTOR ( 'NONE', #127963, 1000.000000000000000 ) ;
#5253 = ORIENTED_EDGE ( 'NONE', *, *, #6302, .T. ) ;
#5254 = FACE_OUTER_BOUND ( 'NONE', #125304, .T. ) ;
#5255 = AXIS2_PLACEMENT_3D ( 'NONE', #136596, #113414, #80822 ) ;
#5256 = ADVANCED_FACE ( 'NONE', ( #110109 ), #78962, .F. ) ;
#5257 = CARTESIAN_POINT ( 'NONE',  ( -34.92500000000001137, -22.22500000000000142, 4.000000000000000000 ) ) ;
#5258 = CARTESIAN_POINT ( 'NONE',  ( -37.26506670282027045, 12.75929247661558996, 18.34774599283964847 ) ) ;
#5259 = CARTESIAN_POINT ( 'NONE',  ( -14.20666063542142687, 21.75929247661549937, 4.998822639870708073 ) ) ;
#5260 = FACE_OUTER_BOUND ( 'NONE', #51654, .T. ) ;
#5261 = ORIENTED_EDGE ( 'NONE', *, *, #138909, .T. ) ;
#5262 = AXIS2_PLACEMENT_3D ( 'NONE', #51972, #115742, #60744 ) ;
#5263 = ORIENTED_EDGE ( 'NONE', *, *, #130098, .T. ) ;
#5264 = CARTESIAN_POINT ( 'NONE',  ( 15.83159235450332147, 9.902892378096218942E-16, 0.000000000000000000 ) ) ;
#5265 = LINE ( 'NONE', #38642, #120684 ) ;
#5266 = ORIENTED_EDGE ( 'NONE', *, *, #48611, .T. ) ;
#5267 = ORIENTED_EDGE ( 'NONE', *, *, #73471, .T. ) ;
#5268 = VERTEX_POINT ( 'NONE', #123169 ) ;
#5269 = CARTESIAN_POINT ( 'NONE',  ( 0.4892135623730947680, -27.52281430457055578, 5.000000000000000000 ) ) ;
#5270 = DIRECTION ( 'NONE',  ( 2.781805975412905274E-17, -0.3543493200069152138, 0.9351131265310292928 ) ) ;
#5271 = VECTOR ( 'NONE', #123975, 1000.000000000000227 ) ;
#5272 = ORIENTED_EDGE ( 'NONE', *, *, #3330, .T. ) ;
#5273 = LINE ( 'NONE', #16897, #113426 ) ;
#5274 = DIRECTION ( 'NONE',  ( -0.7071067811865486830, -0.7071067811865464625, 0.000000000000000000 ) ) ;
#5275 = CARTESIAN_POINT ( 'NONE',  ( 5.900403141435219823, -7.934999999999989839, 2.126176841940957907 ) ) ;
#5276 = CARTESIAN_POINT ( 'NONE',  ( 31.49999999999977973, -12.66682484999663494, -0.6294897503863212673 ) ) ;
#5277 = VERTEX_POINT ( 'NONE', #44929 ) ;
#5278 = CARTESIAN_POINT ( 'NONE',  ( 6.793339364578431017, 21.75929247661549226, 4.998822639870705409 ) ) ;
#5280 = ADVANCED_FACE ( 'NONE', ( #34016 ), #134774, .F. ) ;
#5279 = LINE ( 'NONE', #139431, #55867 ) ;
#5281 = EDGE_CURVE ( 'NONE', #29556, #93024, #122416, .T. ) ;
#5282 = CYLINDRICAL_SURFACE ( 'NONE', #140120, 0.5000000000000004441 ) ;
#5283 = VECTOR ( 'NONE', #19595, 1000.000000000000000 ) ;
#5285 = ORIENTED_EDGE ( 'NONE', *, *, #68839, .F. ) ;
#5284 = CARTESIAN_POINT ( 'NONE',  ( 7.499999999999951150, 10.94296225409028089, -9.576120664313240383 ) ) ;
#5286 = LINE ( 'NONE', #84336, #12351 ) ;
#5287 = ORIENTED_EDGE ( 'NONE', *, *, #120968, .F. ) ;
#5288 = PLANE ( 'NONE',  #68133 ) ;
#5289 = DIRECTION ( 'NONE',  ( 0.000000000000000000, -1.000000000000000000, 0.000000000000000000 ) ) ;
#5290 = AXIS2_PLACEMENT_3D ( 'NONE', #95168, #62568, #51695 ) ;
#5291 = CARTESIAN_POINT ( 'NONE',  ( 27.48921356237309155, -27.52281430457074762, 5.000000000000000000 ) ) ;
#5293 = ORIENTED_EDGE ( 'NONE', *, *, #53400, .T. ) ;
#5292 = AXIS2_PLACEMENT_3D ( 'NONE', #258, #44555, #131524 ) ;
#5294 = EDGE_CURVE ( 'NONE', #126528, #122084, #35464, .T. ) ;
#5295 = DIRECTION ( 'NONE',  ( 0.7071067811865487940, 0.7071067811865463515, -0.000000000000000000 ) ) ;
#5296 = PLANE ( 'NONE',  #46575 ) ;
#5297 = DIRECTION ( 'NONE',  ( -0.7071067811865486830, -0.7071067811865464625, 0.000000000000000000 ) ) ;
#5298 = VECTOR ( 'NONE', #129944, 1000.000000000000000 ) ;
#5299 = VECTOR ( 'NONE', #87578, 1000.000000000000000 ) ;
#5300 = ORIENTED_EDGE ( 'NONE', *, *, #13481, .F. ) ;
#5301 = LINE ( 'NONE', #126381, #13485 ) ;
#5302 = CARTESIAN_POINT ( 'NONE',  ( 34.92500000000002558, -21.76999999999999247, -37.00000000000000000 ) ) ;
#5303 = CARTESIAN_POINT ( 'NONE',  ( 22.06663961620377279, 1.633150327867675555, 6.094999999999998863 ) ) ;
#5304 = EDGE_CURVE ( 'NONE', #17012, #28108, #23081, .T. ) ;
#5305 = PLANE ( 'NONE',  #5435 ) ;
#5306 = FILL_AREA_STYLE_COLOUR ( '', #110919 ) ;
#5307 = EDGE_CURVE ( 'NONE', #126328, #8088, #134036, .T. ) ;
#5308 = VERTEX_POINT ( 'NONE', #131891 ) ;
#5309 = ORIENTED_EDGE ( 'NONE', *, *, #83609, .F. ) ;
#5310 = CYLINDRICAL_SURFACE ( 'NONE', #881, 0.5000000000000004441 ) ;
#5311 = DIRECTION ( 'NONE',  ( 0.3543493200069162685, -0.000000000000000000, -0.9351131265310288487 ) ) ;
#5312 = EDGE_CURVE ( 'NONE', #21371, #99152, #54360, .T. ) ;
#5313 = ADVANCED_FACE ( 'NONE', ( #111553 ), #23841, .F. ) ;
#5314 = B_SPLINE_CURVE_WITH_KNOTS ( 'NONE', 3,
 ( #95896, #85018, #8149, #54562, #98739, #142285, #52387, #141559, #41508, #76305 ),
 .UNSPECIFIED., .F., .F.,
 ( 4, 2, 2, 2, 4 ),
 ( 2.602085213965210642E-18, 0.001968391616361199817, 0.003936783232722403103, 0.005905174849083606389, 0.007873566465444809676 ),
 .UNSPECIFIED. ) ;
#5315 = CARTESIAN_POINT ( 'NONE',  ( 2.749569808101886004, 3.967499999999998916, 6.871911579029510442 ) ) ;
#5316 = DIRECTION ( 'NONE',  ( 0.7071067811865487940, 0.7071067811865463515, 0.000000000000000000 ) ) ;
#5317 = VECTOR ( 'NONE', #8169, 1000.000000000000000 ) ;
#5318 = CARTESIAN_POINT ( 'NONE',  ( 36.18398860626899705, 28.73617430169812437, 5.000000000000000000 ) ) ;
#5319 = CARTESIAN_POINT ( 'NONE',  ( 21.48921356237309155, -27.52281430457070499, 5.000000000000000000 ) ) ;
#5320 = PLANE ( 'NONE',  #102304 ) ;
#5321 = ORIENTED_EDGE ( 'NONE', *, *, #78197, .T. ) ;
#5322 = EDGE_CURVE ( 'NONE', #98347, #86060, #87665, .T. ) ;
#5323 = CARTESIAN_POINT ( 'NONE',  ( 21.48921356237309155, -27.52281430457070499, 5.000000000000000000 ) ) ;
#5324 = LINE ( 'NONE', #135867, #127994 ) ;
#5325 = LINE ( 'NONE', #95203, #113110 ) ;
#5326 = CARTESIAN_POINT ( 'NONE',  ( 45.41209685856478728, 5.291415217122922066, -3.054999999999995275 ) ) ;
#5327 = VECTOR ( 'NONE', #90535, 999.9999999999998863 ) ;
#5328 = FACE_OUTER_BOUND ( 'NONE', #12416, .T. ) ;
#5329 = EDGE_CURVE ( 'NONE', #14772, #69972, #77534, .T. ) ;
#5330 = ORIENTED_EDGE ( 'NONE', *, *, #30443, .F. ) ;
#5331 = CARTESIAN_POINT ( 'NONE',  ( 0.000000000000000000, -21.72500000000000142, 4.500000000000000888 ) ) ;
#5332 = CIRCLE ( 'NONE', #114116, 2.500000000000000444 ) ;
#5333 = ORIENTED_EDGE ( 'NONE', *, *, #83842, .T. ) ;
#5334 = ORIENTED_EDGE ( 'NONE', *, *, #99976, .T. ) ;
#5335 = LINE ( 'NONE', #116967, #89439 ) ;
#5336 = EDGE_CURVE ( 'NONE', #103352, #23962, #99221, .T. ) ;
#5337 = DIRECTION ( 'NONE',  ( -0.6830127018922181881, 0.6830127018922202975, -0.2588190451025214056 ) ) ;
#5338 = DIRECTION ( 'NONE',  ( 0.7071067811865487940, 0.7071067811865463515, -0.000000000000000000 ) ) ;
#5339 = CARTESIAN_POINT ( 'NONE',  ( 69.29974487139159578, -27.71228299555254537, 4.000000000000000000 ) ) ;
#5340 = SURFACE_STYLE_FILL_AREA ( #69961 ) ;
#5341 = VERTEX_POINT ( 'NONE', #22374 ) ;
#5342 = CARTESIAN_POINT ( 'NONE',  ( 8.673617379884035472E-16, -18.41253812416056945, 4.000000000000000000 ) ) ;
#5343 = CARTESIAN_POINT ( 'NONE',  ( -39.29974487139159578, -27.71228299555233576, 4.000000000000000000 ) ) ;
#5344 = ADVANCED_FACE ( 'NONE', ( #55771 ), #110808, .T. ) ;
#5345 = CARTESIAN_POINT ( 'NONE',  ( 34.42499999999998295, -21.72500000000000142, 4.500000000000000888 ) ) ;
#5346 = PLANE ( 'NONE',  #28838 ) ;
#5347 = DIRECTION ( 'NONE',  ( -0.6830127018922181881, 0.6830127018922202975, -0.2588190451025214056 ) ) ;
#5348 = VECTOR ( 'NONE', #12289, 1000.000000000000000 ) ;
#5349 = CARTESIAN_POINT ( 'NONE',  ( 62.49586038379623432, -3.974999999999998312, -6.884901960086286188 ) ) ;
#5350 = AXIS2_PLACEMENT_3D ( 'NONE', #109086, #76498, #54739 ) ;
#5351 = DIRECTION ( 'NONE',  ( -1.000000000000000000, -1.224606353822377258E-16, -0.000000000000000000 ) ) ;
#5352 = ORIENTED_EDGE ( 'NONE', *, *, #102088, .F. ) ;
#5353 = VERTEX_POINT ( 'NONE', #115793 ) ;
#5354 = CARTESIAN_POINT ( 'NONE',  ( 68.22916666666665719, 7.950000000000001954, -2.130196079827421762 ) ) ;
#5355 = DIRECTION ( 'NONE',  ( -0.000000000000000000, -0.3543493200069152693, 0.9351131265310292928 ) ) ;
#5356 = LINE ( 'NONE', #6054, #92491 ) ;
#5357 = CARTESIAN_POINT ( 'NONE',  ( -34.92500000000001137, 22.22500000000000142, 4.000000000000000000 ) ) ;
#5358 = ADVANCED_FACE ( 'NONE', ( #38992 ), #48441, .F. ) ;
#5359 = AXIS2_PLACEMENT_3D ( 'NONE', #126788, #139128, #36936 ) ;
#5360 = ORIENTED_EDGE ( 'NONE', *, *, #9632, .T. ) ;
#5361 = DIRECTION ( 'NONE',  ( 0.6830127018922181881, 0.6830127018922202975, -0.2588190451025214056 ) ) ;
#5362 = EDGE_CURVE ( 'NONE', #35109, #85516, #136875, .T. ) ;
#5363 = LINE ( 'NONE', #138051, #113851 ) ;
#5364 = CARTESIAN_POINT ( 'NONE',  ( 57.75043019189809712, 3.055000000000002824, -5.291415217122919401 ) ) ;
#5365 = EDGE_CURVE ( 'NONE', #64063, #79833, #57041, .T. ) ;
#5366 = DIRECTION ( 'NONE',  ( -0.7071067811865486830, -0.7071067811865464625, 0.000000000000000000 ) ) ;
#5367 = ORIENTED_EDGE ( 'NONE', *, *, #88840, .T. ) ;
#5368 = VERTEX_POINT ( 'NONE', #1855 ) ;
#5369 = AXIS2_PLACEMENT_3D ( 'NONE', #26537, #81661, #90356 ) ;
#5370 = CARTESIAN_POINT ( 'NONE',  ( -0.1839886062690032631, 28.73617430169787568, 5.000000000000000000 ) ) ;
#5371 = EDGE_CURVE ( 'NONE', #40384, #19769, #74495, .T. ) ;
#5372 = DIRECTION ( 'NONE',  ( 1.000000000000000000, 0.000000000000000000, 0.000000000000000000 ) ) ;
#5373 = CARTESIAN_POINT ( 'NONE',  ( 27.99999999999999645, -49.14999999999999147, -53.92499999999967741 ) ) ;
#5374 = CARTESIAN_POINT ( 'NONE',  ( -3.005480084712505828, 28.92564299267936079, 4.000000000000000000 ) ) ;
#5376 = ORIENTED_EDGE ( 'NONE', *, *, #121412, .F. ) ;
#5375 = CARTESIAN_POINT ( 'NONE',  ( 0.000000000000000000, 0.000000000000000000, 5.000000000000000000 ) ) ;
#5377 = CARTESIAN_POINT ( 'NONE',  ( 11.99999999999992717, 14.96639925780211478, 5.000000000000000000 ) ) ;
#5378 = DIRECTION ( 'NONE',  ( -0.7071067811865486830, 0.7071067811865464625, 0.000000000000000000 ) ) ;
#5379 = PRESENTATION_LAYER_ASSIGNMENT (  '', '', ( #142027 ) ) ;
#5380 = CARTESIAN_POINT ( 'NONE',  ( -24.52400138585431222, 22.03583458319438293, 4.979811245910084949 ) ) ;
#5381 = CARTESIAN_POINT ( 'NONE',  ( 26.20710678118635784, -8.240707523384202204, 5.000000000000000000 ) ) ;
#5382 = ORIENTED_EDGE ( 'NONE', *, *, #78695, .T. ) ;
#5383 = ORIENTED_EDGE ( 'NONE', *, *, #86397, .F. ) ;
#5384 = EDGE_CURVE ( 'NONE', #90006, #100364, #111366, .T. ) ;
#5385 = LINE ( 'NONE', #94541, #17430 ) ;
#5386 = LINE ( 'NONE', #103280, #67329 ) ;
#5387 = CARTESIAN_POINT ( 'NONE',  ( 111.4958603837962272, -3.974999999999998312, -6.884901960086286188 ) ) ;
#5388 = CARTESIAN_POINT ( 'NONE',  ( -34.49999999999975842, 15.05432934483078533, 4.994342998332167660 ) ) ;
#5389 = ORIENTED_EDGE ( 'NONE', *, *, #65968, .T. ) ;
#5390 = ORIENTED_EDGE ( 'NONE', *, *, #50054, .T. ) ;
#5391 = AXIS2_PLACEMENT_3D ( 'NONE', #62238, #106393, #117284 ) ;
#5392 = DIRECTION ( 'NONE',  ( -0.000000000000000000, 0.000000000000000000, 1.000000000000000000 ) ) ;
#5394 = EDGE_CURVE ( 'NONE', #12987, #23088, #132470, .T. ) ;
#5393 = CARTESIAN_POINT ( 'NONE',  ( -34.47516574401890210, 9.028067341115725952, 4.998110765256836174 ) ) ;
#5395 = ORIENTED_EDGE ( 'NONE', *, *, #141871, .F. ) ;
#5396 = CONICAL_SURFACE ( 'NONE', #100322, 2.055000000000000604, 0.9599310885968764806 ) ;
#5397 = ORIENTED_EDGE ( 'NONE', *, *, #116605, .F. ) ;
#5398 = DIRECTION ( 'NONE',  ( -0.000000000000000000, -0.3543493200069152693, 0.9351131265310292928 ) ) ;
#5399 = ORIENTED_EDGE ( 'NONE', *, *, #19090, .T. ) ;
#5400 = DIRECTION ( 'NONE',  ( 0.000000000000000000, 0.000000000000000000, 1.000000000000000000 ) ) ;
#5401 = VECTOR ( 'NONE', #119669, 1000.000000000000000 ) ;
#5402 = ORIENTED_EDGE ( 'NONE', *, *, #123377, .T. ) ;
#5403 = FACE_BOUND ( 'NONE', #109297, .T. ) ;
#5404 = CARTESIAN_POINT ( 'NONE',  ( 14.70692117890024697, 0.000000000000000000, 2.500000000000000444 ) ) ;
#5405 = LINE ( 'NONE', #48959, #28089 ) ;
#5406 = CARTESIAN_POINT ( 'NONE',  ( 51.48921356237309510, -27.52281430457091460, 5.000000000000000000 ) ) ;
#5408 = VERTEX_POINT ( 'NONE', #69324 ) ;
#5407 = DIRECTION ( 'NONE',  ( 1.000000000000000000, 0.000000000000000000, 0.000000000000000000 ) ) ;
#5409 = VECTOR ( 'NONE', #52334, 1000.000000000000227 ) ;
#5410 = LINE ( 'NONE', #26481, #32516 ) ;
#5411 = APPLICATION_PROTOCOL_DEFINITION ( 'draft international standard', 'automotive_design', 1998, #44916 ) ;
#5412 = ORIENTED_EDGE ( 'NONE', *, *, #129327, .T. ) ;
#5413 = EDGE_CURVE ( 'NONE', #117635, #74571, #37397, .T. ) ;
#5414 = VECTOR ( 'NONE', #71002, 1000.000000000000000 ) ;
#5415 = ORIENTED_EDGE ( 'NONE', *, *, #101835, .T. ) ;
#5416 = CARTESIAN_POINT ( 'NONE',  ( 90.91209685856478018, 5.291415217122921177, -3.054999999999994831 ) ) ;
#5417 = ORIENTED_EDGE ( 'NONE', *, *, #110926, .T. ) ;
#5418 = LINE ( 'NONE', #61312, #48935 ) ;
#5419 = CARTESIAN_POINT ( 'NONE',  ( 34.82816939922328459, -20.24070752338408141, 4.000000000000000000 ) ) ;
#5420 = EDGE_CURVE ( 'NONE', #120324, #135031, #103338, .T. ) ;
#5421 = VECTOR ( 'NONE', #136523, 1000.000000000000000 ) ;
#5422 = DIRECTION ( 'NONE',  ( 1.000000000000000000, 0.000000000000000000, 0.000000000000000000 ) ) ;
#5423 = ORIENTED_EDGE ( 'NONE', *, *, #3650, .T. ) ;
#5424 = PLANE ( 'NONE',  #106200 ) ;
#5425 = DIRECTION ( 'NONE',  ( -1.000000000000000000, -1.224606353822377258E-16, -0.000000000000000000 ) ) ;
#5426 = VECTOR ( 'NONE', #133011, 1000.000000000000000 ) ;
#5427 = LINE ( 'NONE', #51118, #1760 ) ;
#5429 = CARTESIAN_POINT ( 'NONE',  ( -0.1839886062690032631, 28.73617430169787568, 5.000000000000000000 ) ) ;
#5428 = CARTESIAN_POINT ( 'NONE',  ( 0.000000000000000000, 0.000000000000000000, 7.950000000000000178 ) ) ;
#5430 = LINE ( 'NONE', #52522, #127340 ) ;
#5431 = LINE ( 'NONE', #38810, #28343 ) ;
#5432 = ORIENTED_EDGE ( 'NONE', *, *, #91890, .F. ) ;
#5433 = LINE ( 'NONE', #114219, #126007 ) ;
#5434 = DIRECTION ( 'NONE',  ( -0.000000000000000000, -0.3543493200069153248, 0.9351131265310292928 ) ) ;
#5435 = AXIS2_PLACEMENT_3D ( 'NONE', #82214, #15448, #71318 ) ;
#5436 = ORIENTED_EDGE ( 'NONE', *, *, #113123, .F. ) ;
#5437 = ORIENTED_EDGE ( 'NONE', *, *, #73607, .T. ) ;
#5438 = ORIENTED_EDGE ( 'NONE', *, *, #124996, .F. ) ;
#5439 = CARTESIAN_POINT ( 'NONE',  ( 44.33376352523143993, 6.110000000000001208, 1.122388791418549305E-15 ) ) ;
#5440 = ORIENTED_EDGE ( 'NONE', *, *, #116761, .T. ) ;
#5441 = VECTOR ( 'NONE', #118484, 1000.000000000000227 ) ;
#5442 = AXIS2_PLACEMENT_3D ( 'NONE', #129028, #128344, #18091 ) ;
#5443 = CARTESIAN_POINT ( 'NONE',  ( 16.67080628287043709, -3.047499999999997211, -5.278424836066143655 ) ) ;
#5444 = CARTESIAN_POINT ( 'NONE',  ( -11.11660040884707357, 10.72905655457496543, -26.47562522530603957 ) ) ;
#5445 = ORIENTED_EDGE ( 'NONE', *, *, #100350, .F. ) ;
#5446 = DIRECTION ( 'NONE',  ( 0.000000000000000000, -1.387778780781446464E-15, 1.000000000000000000 ) ) ;
#5447 = ORIENTED_EDGE ( 'NONE', *, *, #93, .F. ) ;
#5448 = CARTESIAN_POINT ( 'NONE',  ( 51.48921356237309510, -27.52281430457091460, 5.000000000000000000 ) ) ;
#5449 = COLOUR_RGB ( '', 0.66274510, 0.83137255, 0.94901961) ;
#5450 = CARTESIAN_POINT ( 'NONE',  ( -33.32816939922329880, 8.259292476615641476, 4.000000000000000000 ) ) ;
#5452 = ORIENTED_EDGE ( 'NONE', *, *, #11165, .T. ) ;
#5451 = CARTESIAN_POINT ( 'NONE',  ( -14.99451991528749595, 28.92564299267948513, 4.000000000000000000 ) ) ;
#5453 = ORIENTED_EDGE ( 'NONE', *, *, #7910, .T. ) ;
#5454 = DIRECTION ( 'NONE',  ( -0.000000000000000000, 0.000000000000000000, 1.000000000000000000 ) ) ;
#5455 = LINE ( 'NONE', #141538, #71628 ) ;
#5456 = ORIENTED_EDGE ( 'NONE', *, *, #89348, .F. ) ;
#5458 = ADVANCED_FACE ( 'NONE', ( #101935 ), #70764, .F. ) ;
#5457 = LINE ( 'NONE', #28691, #4037 ) ;
#5459 = ORIENTED_EDGE ( 'NONE', *, *, #79236, .T. ) ;
#5460 = ORIENTED_EDGE ( 'NONE', *, *, #128680, .F. ) ;
#5461 = ORIENTED_EDGE ( 'NONE', *, *, #35306, .T. ) ;
#5462 = ORIENTED_EDGE ( 'NONE', *, *, #111476, .F. ) ;
#5463 = EDGE_CURVE ( 'NONE', #139982, #133491, #38122, .T. ) ;
#5464 = EDGE_CURVE ( 'NONE', #63294, #58140, #24845, .T. ) ;
#5465 = LINE ( 'NONE', #138160, #93462 ) ;
#5466 = VECTOR ( 'NONE', #110488, 1000.000000000000227 ) ;
#5467 = CARTESIAN_POINT ( 'NONE',  ( -11.99999999999990763, 2.966399257802230682, 5.000000000000000000 ) ) ;
#5468 = FACE_OUTER_BOUND ( 'NONE', #120833, .T. ) ;
#5469 = FACE_OUTER_BOUND ( 'NONE', #115963, .T. ) ;
#5470 = ADVANCED_FACE ( 'NONE', ( #114910 ), #14201, .F. ) ;
#5471 = ADVANCED_FACE ( 'NONE', ( #25794 ), #125847, .F. ) ;
#5472 = CARTESIAN_POINT ( 'NONE',  ( 21.44840764549667611, 3.061616997868385113E-16, -2.500000000000001332 ) ) ;
#5473 = VECTOR ( 'NONE', #140210, 1000.000000000000000 ) ;
#5474 = EDGE_LOOP ( 'NONE', ( #54486, #31306, #40166, #48365 ) ) ;
#5475 = LINE ( 'NONE', #27238, #49391 ) ;
#5476 = EDGE_CURVE ( 'NONE', #132130, #27153, #26520, .T. ) ;
#5477 = EDGE_CURVE ( 'NONE', #60182, #20317, #59868, .T. ) ;
#5478 = FACE_OUTER_BOUND ( 'NONE', #11652, .T. ) ;
#5479 = CARTESIAN_POINT ( 'NONE',  ( 5.755190629914537226, -2.055000000000000160, 0.000000000000000000 ) ) ;
#5480 = AXIS2_PLACEMENT_3D ( 'NONE', #116551, #60048, #62914 ) ;
#5481 = CARTESIAN_POINT ( 'NONE',  ( 96.08333333333332860, 6.884901960086290629, -3.974999999999994316 ) ) ;
#5482 = LINE ( 'NONE', #83078, #58259 ) ;
#5483 = VERTEX_POINT ( 'NONE', #80909 ) ;
#5484 = ORIENTED_EDGE ( 'NONE', *, *, #140971, .T. ) ;
#5485 = EDGE_CURVE ( 'NONE', #90489, #118217, #82345, .T. ) ;
#5486 = ORIENTED_EDGE ( 'NONE', *, *, #71263, .F. ) ;
#5487 = CARTESIAN_POINT ( 'NONE',  ( 4.184256412735922304, 4.202752102959690472E-16, 0.000000000000000000 ) ) ;
#5488 = DIRECTION ( 'NONE',  ( 0.7071067811865487940, 0.7071067811865463515, 0.000000000000000000 ) ) ;
#5489 = UNCERTAINTY_MEASURE_WITH_UNIT (LENGTH_MEASURE( 1.000000000000000082E-05 ), #69508, 'distance_accuracy_value', 'NONE');
#5490 = DIRECTION ( 'NONE',  ( -0.000000000000000000, 0.000000000000000000, -1.000000000000000000 ) ) ;
#5491 = EDGE_CURVE ( 'NONE', #106060, #18279, #48997, .T. ) ;
#5492 = CARTESIAN_POINT ( 'NONE',  ( 4.828169399223495084, -17.24070752338410628, 4.000000000000000000 ) ) ;
#5493 = CARTESIAN_POINT ( 'NONE',  ( 3.730677800976860414, -49.14999999999999147, -40.92499999999998295 ) ) ;
#5494 = CARTESIAN_POINT ( 'NONE',  ( 78.66209685856479439, -5.291415217122919401, 3.054999999999998384 ) ) ;
#5495 = VECTOR ( 'NONE', #4123, 1000.000000000000000 ) ;
#5496 = CARTESIAN_POINT ( 'NONE',  ( 75.03752705046288440, -9.735942053221456900E-16, 7.949999999999998401 ) ) ;
#5497 = EDGE_CURVE ( 'NONE', #80916, #4279, #114236, .T. ) ;
#5498 = LINE ( 'NONE', #128043, #66961 ) ;
#5499 = CARTESIAN_POINT ( 'NONE',  ( -29.99451991528749417, 28.92564299267958816, 4.000000000000000000 ) ) ;
#5500 = LINE ( 'NONE', #14955, #7262 ) ;
#5501 = DIRECTION ( 'NONE',  ( 0.7071067811865487940, -0.7071067811865463515, 0.000000000000000000 ) ) ;
#5502 = EDGE_LOOP ( 'NONE', ( #116858, #88069, #38211, #87346 ) ) ;
#5503 = DIRECTION ( 'NONE',  ( 0.7071067811865487940, 0.7071067811865463515, -0.000000000000000000 ) ) ;
#5504 = VERTEX_POINT ( 'NONE', #3986 ) ;
#5505 = EDGE_CURVE ( 'NONE', #122142, #2143, #47601, .T. ) ;
#5506 = PLANE ( 'NONE',  #110790 ) ;
#5508 = ORIENTED_EDGE ( 'NONE', *, *, #25375, .F. ) ;
#5507 = CARTESIAN_POINT ( 'NONE',  ( 9.489213562373095101, -27.52281430457062328, 5.000000000000000000 ) ) ;
#5509 = CARTESIAN_POINT ( 'NONE',  ( 23.99999999999983302, -16.60178936734445898, 0.8616154019348044590 ) ) ;
#5510 = LINE ( 'NONE', #26576, #121275 ) ;
#5511 = EDGE_LOOP ( 'NONE', ( #41415, #26073, #108408, #135094 ) ) ;
#5512 = ORIENTED_EDGE ( 'NONE', *, *, #26066, .T. ) ;
#5513 = CARTESIAN_POINT ( 'NONE',  ( 122.1416937171300390, -2.130196079821051303, -7.950000000003678124 ) ) ;
#5514 = ORIENTED_EDGE ( 'NONE', *, *, #129310, .F. ) ;
#5516 = ADVANCED_FACE ( 'NONE', ( #93196 ), #46909, .F. ) ;
#5515 = VECTOR ( 'NONE', #30976, 1000.000000000000000 ) ;
#5517 = LINE ( 'NONE', #49794, #140193 ) ;
#5518 = CARTESIAN_POINT ( 'NONE',  ( 95.16252705046289861, 7.949999999999998401, 1.460391307983218338E-15 ) ) ;
#5519 = CARTESIAN_POINT ( 'NONE',  ( 71.72916666666665719, 7.950000000000001954, -2.130196079827421762 ) ) ;
#5520 = VECTOR ( 'NONE', #122302, 1000.000000000000227 ) ;
#5521 = CARTESIAN_POINT ( 'NONE',  ( 0.000000000000000000, 0.000000000000000000, 0.000000000000000000 ) ) ;
#5522 = VERTEX_POINT ( 'NONE', #79529 ) ;
#5523 = LINE ( 'NONE', #124472, #125651 ) ;
#5524 = CARTESIAN_POINT ( 'NONE',  ( -10.49999999999992539, 15.05218569542901896, 5.000000000000000000 ) ) ;
#5525 = CARTESIAN_POINT ( 'NONE',  ( 27.70833333333333570, 3.047499999999997655, 5.278424836066143655 ) ) ;
#5526 = EDGE_CURVE ( 'NONE', #8455, #69699, #68623, .T. ) ;
#5527 = DIRECTION ( 'NONE',  ( -0.7071067811865486830, 0.7071067811865464625, 0.000000000000000000 ) ) ;
#5528 = DIRECTION ( 'NONE',  ( -1.000000000000000000, -0.000000000000000000, -0.000000000000000000 ) ) ;
#5529 = ORIENTED_EDGE ( 'NONE', *, *, #116995, .T. ) ;
#5530 = VECTOR ( 'NONE', #85008, 1000.000000000000000 ) ;
#5531 = CARTESIAN_POINT ( 'NONE',  ( -17.99999999999986855, 12.25461709320619086, -10.07315571508701346 ) ) ;
#5532 = EDGE_CURVE ( 'NONE', #94185, #68343, #112805, .T. ) ;
#5533 = VERTEX_POINT ( 'NONE', #35991 ) ;
#5534 = VECTOR ( 'NONE', #85717, 1000.000000000000227 ) ;
#5535 = CIRCLE ( 'NONE', #102847, 0.5000000000000004441 ) ;
#5536 = CARTESIAN_POINT ( 'NONE',  ( 85.60459685856478984, 1.637169565754164946, -6.109999999999999432 ) ) ;
#5537 = EDGE_CURVE ( 'NONE', #136698, #137282, #11680, .T. ) ;
#5538 = DIRECTION ( 'NONE',  ( 0.7071067811865487940, 0.7071067811865463515, 0.000000000000000000 ) ) ;
#5539 = DIRECTION ( 'NONE',  ( -0.7071067811865486830, -0.7071067811865464625, 0.000000000000000000 ) ) ;
#5540 = DIRECTION ( 'NONE',  ( 1.000000000000000000, 0.000000000000000000, 0.000000000000000000 ) ) ;
#5541 = VERTEX_POINT ( 'NONE', #97258 ) ;
#5542 =( NAMED_UNIT ( * ) SI_UNIT ( $, .STERADIAN. ) SOLID_ANGLE_UNIT ( ) );
#5543 = ADVANCED_FACE ( 'NONE', ( #30641 ), #108143, .T. ) ;
#5545 = ADVANCED_FACE ( 'NONE', ( #66123 ), #109599, .F. ) ;
#5544 = VECTOR ( 'NONE', #63325, 1000.000000000000227 ) ;
#5546 = LINE ( 'NONE', #116474, #78951 ) ;
#5547 = LINE ( 'NONE', #71555, #25414 ) ;
#5548 = DIRECTION ( 'NONE',  ( -1.000000000000000000, -1.224606353822377258E-16, -0.000000000000000000 ) ) ;
#5550 = ORIENTED_EDGE ( 'NONE', *, *, #116830, .F. ) ;
#5549 = DIRECTION ( 'NONE',  ( 0.000000000000000000, -1.000000000000000000, 0.000000000000000000 ) ) ;
#5551 = CARTESIAN_POINT ( 'NONE',  ( 13.12500000000000178, 6.094999999999989981, -1.119633336120465690E-15 ) ) ;
#5552 = DIRECTION ( 'NONE',  ( -0.7071067811865486830, -0.7071067811865464625, 0.000000000000000000 ) ) ;
#5553 = CARTESIAN_POINT ( 'NONE',  ( 1.586284118322663916, -3.036554765565917968, 5.760036735694805010 ) ) ;
#5554 = CARTESIAN_POINT ( 'NONE',  ( 59.18749999999998579, -5.819803920172573974, 5.819803920172573086 ) ) ;
#5555 = AXIS2_PLACEMENT_3D ( 'NONE', #129014, #114040, #92269 ) ;
#5556 = ORIENTED_EDGE ( 'NONE', *, *, #90587, .T. ) ;
#5557 = ORIENTED_EDGE ( 'NONE', *, *, #107950, .T. ) ;
#5558 = EDGE_LOOP ( 'NONE', ( #100792, #1255, #52559, #139846 ) ) ;
#5559 = CARTESIAN_POINT ( 'NONE',  ( 70.14626352523143282, -4.472830434245840259, 4.472830434245839371 ) ) ;
#5560 = VECTOR ( 'NONE', #9753, 999.9999999999998863 ) ;
#5561 = ORIENTED_EDGE ( 'NONE', *, *, #88034, .F. ) ;
#5562 = EDGE_CURVE ( 'NONE', #7059, #2171, #32786, .T. ) ;
#5563 = LINE ( 'NONE', #83152, #107669 ) ;
#5564 = DIRECTION ( 'NONE',  ( -0.000000000000000000, -0.3543493200069152693, 0.9351131265310292928 ) ) ;
#5565 = VECTOR ( 'NONE', #25127, 1000.000000000000227 ) ;
#5566 = LINE ( 'NONE', #102777, #82797 ) ;
#5567 = LINE ( 'NONE', #49838, #59495 ) ;
#5568 = ORIENTED_EDGE ( 'NONE', *, *, #11403, .T. ) ;
#5569 = DIRECTION ( 'NONE',  ( 0.3543493200069162685, -0.000000000000000000, -0.9351131265310288487 ) ) ;
#5570 = DIRECTION ( 'NONE',  ( 0.7071067811865487940, 0.7071067811865463515, 0.000000000000000000 ) ) ;
#5571 = ORIENTED_EDGE ( 'NONE', *, *, #24484, .T. ) ;
#5572 = ADVANCED_FACE ( 'NONE', ( #43629 ), #86445, .F. ) ;
#5573 = CARTESIAN_POINT ( 'NONE',  ( -12.69999999999998153, 0.000000000000000000, 2.500000000000000444 ) ) ;
#5574 = CARTESIAN_POINT ( 'NONE',  ( 33.47502705046289151, -5.819803920172573086, 5.819803920172573086 ) ) ;
#5575 = VECTOR ( 'NONE', #24576, 1000.000000000000000 ) ;
#5576 = CARTESIAN_POINT ( 'NONE',  ( -20.51078643762690490, -27.52281430457041012, 5.000000000000000000 ) ) ;
#5577 = ORIENTED_EDGE ( 'NONE', *, *, #20914, .F. ) ;
#5578 = ORIENTED_EDGE ( 'NONE', *, *, #35599, .T. ) ;
#5579 = EDGE_CURVE ( 'NONE', #19199, #98041, #42943, .T. ) ;
#5580 = DIRECTION ( 'NONE',  ( -0.6830127018922181881, 0.6830127018922202975, -0.2588190451025214056 ) ) ;
#5581 = LINE ( 'NONE', #83920, #52404 ) ;
#5582 = DIRECTION ( 'NONE',  ( -0.000000000000000000, -1.000000000000000000, -0.000000000000000000 ) ) ;
#5583 = DIRECTION ( 'NONE',  ( -0.7071067811865487940, 0.7071067811865463515, -0.000000000000000000 ) ) ;
#5584 = DIRECTION ( 'NONE',  ( -0.7071067811865486830, -0.7071067811865464625, -0.000000000000000000 ) ) ;
#5585 = DIRECTION ( 'NONE',  ( -0.7071067811865486830, -0.7071067811865464625, 0.000000000000000000 ) ) ;
#5586 = LINE ( 'NONE', #70213, #51246 ) ;
#5587 = ORIENTED_EDGE ( 'NONE', *, *, #119608, .F. ) ;
#5588 = VERTEX_POINT ( 'NONE', #53064 ) ;
#5589 = EDGE_LOOP ( 'NONE', ( #100201, #128538, #8060, #46993 ) ) ;
#5590 = ORIENTED_EDGE ( 'NONE', *, *, #63831, .F. ) ;
#5592 = ADVANCED_FACE ( 'NONE', ( #53822 ), #85693, .F. ) ;
#5591 = VECTOR ( 'NONE', #435, 999.9999999999998863 ) ;
#5593 = CARTESIAN_POINT ( 'NONE',  ( -14.99999999999989519, 9.631307414974306980, -9.079085613539573885 ) ) ;
#5595 = EDGE_CURVE ( 'NONE', #77074, #64995, #91895, .T. ) ;
#5594 = PRESENTATION_STYLE_ASSIGNMENT (( #4852 ) ) ;
#5596 = ORIENTED_EDGE ( 'NONE', *, *, #140747, .F. ) ;
#5597 = DIRECTION ( 'NONE',  ( 0.000000000000000000, 0.000000000000000000, 1.000000000000000000 ) ) ;
#5598 = DIRECTION ( 'NONE',  ( 0.6830127018922181881, 0.6830127018922202975, -0.2588190451025214056 ) ) ;
#5599 = PLANE ( 'NONE',  #87807 ) ;
#5600 = DIRECTION ( 'NONE',  ( 0.3543493200069163240, -0.000000000000000000, -0.9351131265310288487 ) ) ;
#5601 = ORIENTED_EDGE ( 'NONE', *, *, #24105, .F. ) ;
#5602 = CARTESIAN_POINT ( 'NONE',  ( 18.10180811604841011, 9.068207373850700748, 5.000000000000000000 ) ) ;
#5603 = DIRECTION ( 'NONE',  ( -0.000000000000000000, -0.000000000000000000, 1.000000000000000000 ) ) ;
#5604 = VERTEX_POINT ( 'NONE', #10274 ) ;
#5605 = CARTESIAN_POINT ( 'NONE',  ( 3.328169399223510627, 5.259292476615662792, 4.000000000000000000 ) ) ;
#5606 = ORIENTED_EDGE ( 'NONE', *, *, #16978, .T. ) ;
#5607 = EDGE_CURVE ( 'NONE', #14862, #70976, #98023, .T. ) ;
#5608 = ORIENTED_EDGE ( 'NONE', *, *, #50535, .T. ) ;
#5609 = DIRECTION ( 'NONE',  ( -1.000000000000000000, -1.224606353822377258E-16, -0.000000000000000000 ) ) ;
#5610 = ORIENTED_EDGE ( 'NONE', *, *, #167, .T. ) ;
#5611 = VERTEX_POINT ( 'NONE', #31342 ) ;
#5612 = CARTESIAN_POINT ( 'NONE',  ( 69.56293019189810423, 1.637169565754157174, 6.110000000000002984 ) ) ;
#5613 = VECTOR ( 'NONE', #126350, 1000.000000000000000 ) ;
#5614 = ORIENTED_EDGE ( 'NONE', *, *, #100147, .T. ) ;
#5615 = FACE_OUTER_BOUND ( 'NONE', #115634, .T. ) ;
#5616 = VECTOR ( 'NONE', #21789, 999.9999999999998863 ) ;
#5617 = DIRECTION ( 'NONE',  ( -0.7071067811865486830, 0.7071067811865464625, 0.000000000000000000 ) ) ;
#5618 = CARTESIAN_POINT ( 'NONE',  ( 105.7295968585647898, -6.110000000000000320, -1.637169565754161393 ) ) ;
#5619 = LINE ( 'NONE', #28118, #100422 ) ;
#5620 = AXIS2_PLACEMENT_3D ( 'NONE', #24962, #16210, #114131 ) ;
#5621 = DIRECTION ( 'NONE',  ( 0.000000000000000000, -1.000000000000000000, 0.000000000000000000 ) ) ;
#5622 = CARTESIAN_POINT ( 'NONE',  ( 0.000000000000000000, 0.000000000000000000, 5.000000000000000000 ) ) ;
#5623 = DIRECTION ( 'NONE',  ( -0.7071067811865487940, 0.7071067811865463515, 0.000000000000000000 ) ) ;
#5624 = PLANE ( 'NONE',  #106928 ) ;
#5625 = DIRECTION ( 'NONE',  ( 1.000000000000000000, 1.224606353822377258E-16, 0.000000000000000000 ) ) ;
#5626 = ORIENTED_EDGE ( 'NONE', *, *, #34573, .F. ) ;
#5627 = CARTESIAN_POINT ( 'NONE',  ( 131.8806778009765708, -49.14999999999999147, 40.92499999999998295 ) ) ;
#5629 = CARTESIAN_POINT ( 'NONE',  ( -24.29974487139158867, -27.71228299555223273, 4.000000000000000000 ) ) ;
#5628 = CIRCLE ( 'NONE', #123756, 4.582731094065999322 ) ;
#5630 = ORIENTED_EDGE ( 'NONE', *, *, #116140, .F. ) ;
#5631 = ORIENTED_EDGE ( 'NONE', *, *, #80022, .F. ) ;
#5632 = DIRECTION ( 'NONE',  ( 0.7071067811865487940, 0.7071067811865463515, -0.000000000000000000 ) ) ;
#5633 = ORIENTED_EDGE ( 'NONE', *, *, #127103, .F. ) ;
#5634 = CARTESIAN_POINT ( 'NONE',  ( 3.489213562373097322, -27.52281430457057709, 5.000000000000000000 ) ) ;
#5635 = LINE ( 'NONE', #49909, #38624 ) ;
#5636 = CARTESIAN_POINT ( 'NONE',  ( 17.99999999999987210, -16.06887692260766087, 4.000000000000000000 ) ) ;
#5637 = FACE_OUTER_BOUND ( 'NONE', #51398, .T. ) ;
#5638 = ADVANCED_FACE ( 'NONE', ( #64681 ), #100171, .F. ) ;
#5639 = VERTEX_POINT ( 'NONE', #41482 ) ;
#5640 = CARTESIAN_POINT ( 'NONE',  ( 0.8183591370940052068, -52.14999999999999147, 41.64499999999997470 ) ) ;
#5641 = ORIENTED_EDGE ( 'NONE', *, *, #109282, .T. ) ;
#5642 = VECTOR ( 'NONE', #53429, 1000.000000000000000 ) ;
#5643 = EDGE_CURVE ( 'NONE', #33187, #11149, #65421, .T. ) ;
#5644 = EDGE_CURVE ( 'NONE', #104233, #106314, #142259, .T. ) ;
#5645 = CARTESIAN_POINT ( 'NONE',  ( 32.00456980810188412, 6.871911579029510442, -3.967499999999998916 ) ) ;
#5646 = CARTESIAN_POINT ( 'NONE',  ( 19.58200623001875940, 3.061616997868383634E-16, -2.500000000000000444 ) ) ;
#5647 = VECTOR ( 'NONE', #84174, 1000.000000000000227 ) ;
#5648 = EDGE_CURVE ( 'NONE', #135168, #16747, #32046, .T. ) ;
#5649 = CARTESIAN_POINT ( 'NONE',  ( -5.510786437626906675, -27.52281430457051314, 5.000000000000000000 ) ) ;
#5650 = LINE ( 'NONE', #50614, #2602 ) ;
#5651 = EDGE_LOOP ( 'NONE', ( #62856, #691, #22807, #130085 ) ) ;
#5652 = ORIENTED_EDGE ( 'NONE', *, *, #99181, .T. ) ;
#5653 = ADVANCED_FACE ( 'NONE', ( #132093 ), #98713, .T. ) ;
#5654 = VERTEX_POINT ( 'NONE', #88590 ) ;
#5655 = DIRECTION ( 'NONE',  ( 0.5735764363510451602, 0.8191520442889924647, 0.000000000000000000 ) ) ;
#5656 = CARTESIAN_POINT ( 'NONE',  ( -34.62823445044363524, -8.240707523384193323, 11.38925528200760695 ) ) ;
#5657 = CARTESIAN_POINT ( 'NONE',  ( -13.49999999999990408, 18.43112307739199451, 4.000000000000000000 ) ) ;
#5658 = ADVANCED_FACE ( 'NONE', ( #33504 ), #121881, .F. ) ;
#5659 = CARTESIAN_POINT ( 'NONE',  ( -33.18398860626899705, 28.73617430169810305, 5.000000000000000000 ) ) ;
#5660 = CARTESIAN_POINT ( 'NONE',  ( 22.49999999999985434, 13.56627193232217188, -10.57019076586063555 ) ) ;
#5661 = CARTESIAN_POINT ( 'NONE',  ( -50.99451991528749062, 28.92564299267973738, 4.000000000000000000 ) ) ;
#5662 = EDGE_CURVE ( 'NONE', #28576, #85226, #61817, .T. ) ;
#5663 = DIRECTION ( 'NONE',  ( -1.000000000000000000, -1.224606353822377258E-16, -0.000000000000000000 ) ) ;
#5664 = ADVANCED_FACE ( 'NONE', ( #81282 ), #113152, .F. ) ;
#5665 = LINE ( 'NONE', #47121, #111383 ) ;
#5666 = CARTESIAN_POINT ( 'NONE',  ( 25.49999999999981881, 8.900465351122173630, -2.516491619111572930 ) ) ;
#5667 = ORIENTED_EDGE ( 'NONE', *, *, #102531, .F. ) ;
#5668 = DIRECTION ( 'NONE',  ( 0.7071067811865487940, 0.7071067811865463515, 0.000000000000000000 ) ) ;
#5669 = DIRECTION ( 'NONE',  ( 0.7071067811865486830, -0.7071067811865464625, -0.000000000000000000 ) ) ;
#5670 = EDGE_LOOP ( 'NONE', ( #52680, #134963, #33535, #24789, #7325 ) ) ;
#5671 = ADVANCED_FACE ( 'NONE', ( #26172 ), #35652, .F. ) ;
#5672 = CARTESIAN_POINT ( 'NONE',  ( -34.49999999999976552, 8.319652575858347276, -8.582050562765903834 ) ) ;
#5674 = VERTEX_POINT ( 'NONE', #122610 ) ;
#5673 = CARTESIAN_POINT ( 'NONE',  ( 34.49999999999975842, -1.535744391599495273, 4.994342998332161443 ) ) ;
#5675 = ADVANCED_FACE ( 'NONE', ( #13827 ), #5800, .F. ) ;
#5676 = CARTESIAN_POINT ( 'NONE',  ( 153.6500000000000057, 5.817072295949924468E-16, -4.749999999999997335 ) ) ;
#5677 = PLANE ( 'NONE',  #101587 ) ;
#5678 = EDGE_LOOP ( 'NONE', ( #133052, #110609, #1717, #135772 ) ) ;
#5679 = DIRECTION ( 'NONE',  ( 0.000000000000000000, -0.3543493200069153248, -0.9351131265310291818 ) ) ;
#5680 = UNCERTAINTY_MEASURE_WITH_UNIT (LENGTH_MEASURE( 1.000000000000000082E-05 ), #58105, 'distance_accuracy_value', 'NONE');
#5681 = VERTEX_POINT ( 'NONE', #94264 ) ;
#5682 = EDGE_CURVE ( 'NONE', #106911, #141737, #13233, .T. ) ;
#5683 = CARTESIAN_POINT ( 'NONE',  ( 16.49230000000001439, 3.130000000000008331, -22.35000000000000142 ) ) ;
#5684 = DIRECTION ( 'NONE',  ( -0.6830127018922180770, -0.6830127018922204085, -0.2588190451025213501 ) ) ;
#5685 = CARTESIAN_POINT ( 'NONE',  ( 118.6416937171295700, -2.130196079827424871, -7.949999999999999289 ) ) ;
#5686 = CARTESIAN_POINT ( 'NONE',  ( -4.499999999999966249, 4.087461875839200509, 4.000000000000000000 ) ) ;
#5687 = CARTESIAN_POINT ( 'NONE',  ( 4.828169399223495084, -20.24070752338407431, 4.000000000000000000 ) ) ;
#5688 = PLANE ( 'NONE',  #95414 ) ;
#5689 = SURFACE_SIDE_STYLE ('',( #62255 ) ) ;
#5690 = DIRECTION ( 'NONE',  ( 8.673617379884034239E-17, -1.000000000000000000, 0.000000000000000000 ) ) ;
#5691 = CARTESIAN_POINT ( 'NONE',  ( 33.37456980810188156, 6.871911579029510442, -3.967499999999998916 ) ) ;
#5692 = CARTESIAN_POINT ( 'NONE',  ( 11.20790314143521904, -6.871911579029513106, -3.967499999999993587 ) ) ;
#5693 = CARTESIAN_POINT ( 'NONE',  ( 9.183988606268997046, 28.73617430169793607, 5.000000000000000000 ) ) ;
#5694 = DIRECTION ( 'NONE',  ( -0.000000000000000000, 0.000000000000000000, 1.000000000000000000 ) ) ;
#5695 = DIRECTION ( 'NONE',  ( 0.000000000000000000, 0.000000000000000000, 1.000000000000000000 ) ) ;
#5696 = VERTEX_POINT ( 'NONE', #26869 ) ;
#5697 = AXIS2_PLACEMENT_3D ( 'NONE', #63789, #9338, #52863 ) ;
#5698 = ORIENTED_EDGE ( 'NONE', *, *, #87684, .F. ) ;
#5699 = CARTESIAN_POINT ( 'NONE',  ( 83.68750000000000000, -5.819803920172573086, 5.819803920172572198 ) ) ;
#5701 = VERTEX_POINT ( 'NONE', #49380 ) ;
#5700 = SURFACE_STYLE_FILL_AREA ( #105035 ) ;
#5702 = ORIENTED_EDGE ( 'NONE', *, *, #13266, .T. ) ;
#5703 = EDGE_CURVE ( 'NONE', #23510, #95696, #6495, .T. ) ;
#5704 = CARTESIAN_POINT ( 'NONE',  ( 3.087196949643290278, -2.500000000000000444, 0.000000000000000000 ) ) ;
#5705 = LINE ( 'NONE', #81173, #32482 ) ;
#5706 = DIRECTION ( 'NONE',  ( 0.7071067811865487940, 0.7071067811865463515, 0.000000000000000000 ) ) ;
#5707 = VERTEX_POINT ( 'NONE', #137797 ) ;
#5708 = DIRECTION ( 'NONE',  ( -0.7071067811865486830, -0.7071067811865464625, 0.000000000000000000 ) ) ;
#5709 = LINE ( 'NONE', #6392, #44111 ) ;
#5710 = LINE ( 'NONE', #73163, #95050 ) ;
#5711 = CARTESIAN_POINT ( 'NONE',  ( 126.6276089467980057, 6.187174973706484060, 2.918809472323000254 ) ) ;
#5712 = CARTESIAN_POINT ( 'NONE',  ( 5.241399257802002332, 21.72500000000000853, 5.000000000000000000 ) ) ;
#5713 = DIRECTION ( 'NONE',  ( 0.000000000000000000, -0.3543493200069152138, 0.9351131265310292928 ) ) ;
#5714 = LINE ( 'NONE', #138404, #26292 ) ;
#5715 = DIRECTION ( 'NONE',  ( 0.7071067811865487940, 0.7071067811865463515, 0.000000000000000000 ) ) ;
#5716 = CARTESIAN_POINT ( 'NONE',  ( 20.99451991528748707, 28.92564299267952777, 4.000000000000000000 ) ) ;
#5717 = CARTESIAN_POINT ( 'NONE',  ( 34.60343192894621467, -14.24070752338413293, 19.24067776001733776 ) ) ;
#5718 = CYLINDRICAL_SURFACE ( 'NONE', #117018, 2.500000000000000000 ) ;
#5719 = EDGE_CURVE ( 'NONE', #19509, #127065, #137072, .T. ) ;
#5720 = VECTOR ( 'NONE', #20883, 999.9999999999998863 ) ;
#5721 = ORIENTED_EDGE ( 'NONE', *, *, #12537, .T. ) ;
#5722 = EDGE_LOOP ( 'NONE', ( #75783, #5698, #23656, #100113 ) ) ;
#5723 = CARTESIAN_POINT ( 'NONE',  ( 103.2504301918981184, 3.055000000000002824, -5.291415217122919401 ) ) ;
#5724 = ORIENTED_EDGE ( 'NONE', *, *, #134703, .F. ) ;
#5725 = AXIS2_PLACEMENT_3D ( 'NONE', #16429, #117177, #38929 ) ;
#5726 = EDGE_CURVE ( 'NONE', #59180, #33017, #139233, .T. ) ;
#5727 = CARTESIAN_POINT ( 'NONE',  ( 7.729166666666666075, -6.094999999999989093, 1.633150327867691542 ) ) ;
#5728 = ORIENTED_EDGE ( 'NONE', *, *, #120272, .T. ) ;
#5729 = DIRECTION ( 'NONE',  ( 1.000000000000000000, 0.000000000000000000, 0.000000000000000000 ) ) ;
#5730 = DIRECTION ( 'NONE',  ( 0.7071067811865487940, 0.7071067811865463515, 0.000000000000000000 ) ) ;
#5731 = CARTESIAN_POINT ( 'NONE',  ( 105.4954301918981230, 5.291415217122916737, 3.055000000000001936 ) ) ;
#5732 = STYLED_ITEM ( 'NONE', ( #133041 ), #88424 ) ;
#5733 = VERTEX_POINT ( 'NONE', #139947 ) ;
#5734 = ADVANCED_FACE ( 'NONE', ( #126877 ), #128348, .F. ) ;
#5735 = CARTESIAN_POINT ( 'NONE',  ( 122.2875270504628844, 0.000000000000000000, -7.949999999999998401 ) ) ;
#5736 = ORIENTED_EDGE ( 'NONE', *, *, #102296, .F. ) ;
#5737 = PLANE ( 'NONE',  #121724 ) ;
#5738 = CARTESIAN_POINT ( 'NONE',  ( 2.999999999999999112, -1.600000000000012301, -20.40202195861969514 ) ) ;
#5739 = LINE ( 'NONE', #16632, #128812 ) ;
#5740 = CARTESIAN_POINT ( 'NONE',  ( 13.82816939922343025, -20.24070752338408496, 4.000000000000000000 ) ) ;
#5741 = EDGE_LOOP ( 'NONE', ( #6724, #87544, #126370, #29250 ) ) ;
#5742 = ORIENTED_EDGE ( 'NONE', *, *, #63734, .T. ) ;
#5743 = EDGE_CURVE ( 'NONE', #4252, #123709, #117421, .T. ) ;
#5744 = ORIENTED_EDGE ( 'NONE', *, *, #50492, .F. ) ;
#5745 = CARTESIAN_POINT ( 'NONE',  ( -14.99999999999989519, 20.70535890316560312, 1.956823837851950909 ) ) ;
#5746 = LINE ( 'NONE', #41246, #63919 ) ;
#5747 = CARTESIAN_POINT ( 'NONE',  ( 10.85873647476855197, 5.808823158059031044, -5.808823158059037262 ) ) ;
#5748 = CARTESIAN_POINT ( 'NONE',  ( 33.18398860626899705, 28.73617430169810305, 5.000000000000000000 ) ) ;
#5750 = VECTOR ( 'NONE', #114755, 1000.000000000000000 ) ;
#5749 = SHAPE_REPRESENTATION_RELATIONSHIP ( 'NONE' , 'NONE' ,  #88538, #11968 ) ;
#5751 = MECHANICAL_DESIGN_GEOMETRIC_PRESENTATION_REPRESENTATION (  '', ( #89104 ), #121561 ) ;
#5752 = DIRECTION ( 'NONE',  ( 0.3543493200069163240, -0.000000000000000000, -0.9351131265310288487 ) ) ;
#5753 = ORIENTED_EDGE ( 'NONE', *, *, #87193, .F. ) ;
#5755 = ORIENTED_EDGE ( 'NONE', *, *, #86999, .T. ) ;
#5754 = VECTOR ( 'NONE', #31131, 1000.000000000000000 ) ;
#5756 = LINE ( 'NONE', #8584, #64147 ) ;
#5757 = ORIENTED_EDGE ( 'NONE', *, *, #139949, .T. ) ;
#5758 = EDGE_LOOP ( 'NONE', ( #106567, #106554, #117757, #33928, #96740 ) ) ;
#5759 = CARTESIAN_POINT ( 'NONE',  ( 109.4329301918981088, 1.637169565754156508, 6.110000000000000320 ) ) ;
#5760 = FACE_OUTER_BOUND ( 'NONE', #71463, .T. ) ;
#5762 = ADVANCED_FACE ( 'NONE', ( #4334 ), #51501, .F. ) ;
#5761 = DIRECTION ( 'NONE',  ( -1.000000000000000000, -1.224606353822377258E-16, -0.000000000000000000 ) ) ;
#5763 = ORIENTED_EDGE ( 'NONE', *, *, #99810, .F. ) ;
#5764 = CARTESIAN_POINT ( 'NONE',  ( 5.979166666666666075, 6.094999999999988205, -1.633150327867694651 ) ) ;
#5765 = PLANE ( 'NONE',  #52495 ) ;
#5766 = DIRECTION ( 'NONE',  ( -0.3543493200069162685, -0.000000000000000000, -0.9351131265310288487 ) ) ;
#5767 = DIRECTION ( 'NONE',  ( -1.000000000000000000, -1.224606353822377258E-16, -0.000000000000000000 ) ) ;
#5768 = ORIENTED_EDGE ( 'NONE', *, *, #45487, .F. ) ;
#5769 = LINE ( 'NONE', #50739, #67213 ) ;
#5770 = FACE_BOUND ( 'NONE', #110690, .T. ) ;
#5771 = EDGE_LOOP ( 'NONE', ( #92201, #131655, #134228, #23621 ) ) ;
#5772 = CARTESIAN_POINT ( 'NONE',  ( 15.48921356237309510, -27.52281430457066236, 5.000000000000000000 ) ) ;
#5773 = DIRECTION ( 'NONE',  ( -0.000000000000000000, 0.3543493200069153248, 0.9351131265310292928 ) ) ;
#5774 = CARTESIAN_POINT ( 'NONE',  ( -18.48921356237309510, -27.52281430457068367, 5.000000000000000000 ) ) ;
#5775 = EDGE_CURVE ( 'NONE', #7970, #127842, #95694, .T. ) ;
#5776 = ORIENTED_EDGE ( 'NONE', *, *, #142102, .T. ) ;
#5777 = CARTESIAN_POINT ( 'NONE',  ( 38.99451991528749062, 28.92564299267965211, 4.000000000000000000 ) ) ;
#5778 = ORIENTED_EDGE ( 'NONE', *, *, #57619, .T. ) ;
#5779 = ORIENTED_EDGE ( 'NONE', *, *, #36107, .F. ) ;
#5780 = VERTEX_POINT ( 'NONE', #40623 ) ;
#5781 = CARTESIAN_POINT ( 'NONE',  ( 35.34959685856478728, 6.109999999999996767, 1.637169565754163836 ) ) ;
#5782 = VERTEX_POINT ( 'NONE', #16709 ) ;
#5783 = CARTESIAN_POINT ( 'NONE',  ( 0.000000000000000000, 21.72500000000000142, 4.500000000000000888 ) ) ;
#5784 = CARTESIAN_POINT ( 'NONE',  ( 23.99451991528749062, 28.92564299267954908, 4.000000000000000000 ) ) ;
#5785 = FACE_OUTER_BOUND ( 'NONE', #135149, .T. ) ;
#5787 = FACE_OUTER_BOUND ( 'NONE', #91778, .T. ) ;
#5786 = CARTESIAN_POINT ( 'NONE',  ( 19.49999999999986144, -16.91253812416058366, 4.000000000000000000 ) ) ;
#5788 = FACE_OUTER_BOUND ( 'NONE', #77311, .T. ) ;
#5789 = CARTESIAN_POINT ( 'NONE',  ( 9.183988606268997046, 28.73617430169793607, 5.000000000000000000 ) ) ;
#5790 = DIRECTION ( 'NONE',  ( 0.6830127018922181881, 0.6830127018922202975, -0.2588190451025214056 ) ) ;
#5791 = CARTESIAN_POINT ( 'NONE',  ( 22.49999999999983658, -14.56887692260766620, 4.000000000000000000 ) ) ;
#5792 = ORIENTED_EDGE ( 'NONE', *, *, #7677, .T. ) ;
#5793 = VERTEX_POINT ( 'NONE', #129033 ) ;
#5794 = VERTEX_POINT ( 'NONE', #142089 ) ;
#5795 = EDGE_LOOP ( 'NONE', ( #100958, #36759, #91151, #34117 ) ) ;
#5796 = DIRECTION ( 'NONE',  ( -1.000000000000000000, -1.224606353822377258E-16, -0.000000000000000000 ) ) ;
#5797 = EDGE_LOOP ( 'NONE', ( #31914, #143302, #75467, #27848 ) ) ;
#5798 = ORIENTED_EDGE ( 'NONE', *, *, #51055, .T. ) ;
#5799 = DIRECTION ( 'NONE',  ( -1.000000000000000000, 0.000000000000000000, 0.000000000000000000 ) ) ;
#5800 = PLANE ( 'NONE',  #140525 ) ;
#5801 = LINE ( 'NONE', #84151, #34735 ) ;
#5802 = VERTEX_POINT ( 'NONE', #20258 ) ;
#5803 = CARTESIAN_POINT ( 'NONE',  ( -45.18398860626900415, 28.73617430169818832, 5.000000000000000000 ) ) ;
#5804 = ORIENTED_EDGE ( 'NONE', *, *, #970, .T. ) ;
#5805 = CARTESIAN_POINT ( 'NONE',  ( 2.207106781186521260, -17.24070752338411339, 5.000000000000000000 ) ) ;
#5806 = AXIS2_PLACEMENT_3D ( 'NONE', #42515, #65715, #109878 ) ;
#5807 = DIRECTION ( 'NONE',  ( -0.7071067811865486830, -0.7071067811865464625, 0.000000000000000000 ) ) ;
#5808 = EDGE_CURVE ( 'NONE', #44292, #65489, #142774, .T. ) ;
#5809 = ORIENTED_EDGE ( 'NONE', *, *, #100029, .T. ) ;
#5811 = CARTESIAN_POINT ( 'NONE',  ( 6.160000000000001030, 9.521314400968980422E-16, 0.000000000000000000 ) ) ;
#5810 = CARTESIAN_POINT ( 'NONE',  ( 101.9954301918981230, 5.291415217122917625, 3.055000000000002380 ) ) ;
#5812 = EDGE_CURVE ( 'NONE', #82267, #34219, #121713, .T. ) ;
#5813 = AXIS2_PLACEMENT_3D ( 'NONE', #73026, #72321, #17856 ) ;
#5814 = PRESENTATION_STYLE_ASSIGNMENT (( #105159 ) ) ;
#5815 = CARTESIAN_POINT ( 'NONE',  ( 0.000000000000000000, 0.000000000000000000, 7.950000000000000178 ) ) ;
#5816 = EDGE_LOOP ( 'NONE', ( #12831, #126658, #73613, #89706 ) ) ;
#5817 = ORIENTED_EDGE ( 'NONE', *, *, #12976, .F. ) ;
#5818 = EDGE_CURVE ( 'NONE', #69618, #2772, #136177, .T. ) ;
#5819 = CARTESIAN_POINT ( 'NONE',  ( -66.48921356237309510, -27.52281430457101763, 5.000000000000000000 ) ) ;
#5820 = ORIENTED_EDGE ( 'NONE', *, *, #43700, .T. ) ;
#5821 = DIRECTION ( 'NONE',  ( 0.6830127018922181881, 0.6830127018922202975, -0.2588190451025214056 ) ) ;
#5822 = DIRECTION ( 'NONE',  ( 0.7071067811865487940, 0.7071067811865463515, 0.000000000000000000 ) ) ;
#5823 = DIRECTION ( 'NONE',  ( 0.000000000000000000, -1.000000000000000000, -1.286409696682840916E-16 ) ) ;
#5824 = EDGE_CURVE ( 'NONE', #4199, #11154, #123900, .T. ) ;
#5825 = CARTESIAN_POINT ( 'NONE',  ( -36.29974487139159578, -27.71228299555231445, 4.000000000000000000 ) ) ;
#5826 = VERTEX_POINT ( 'NONE', #112303 ) ;
#5827 = CARTESIAN_POINT ( 'NONE',  ( 15.70710678118643422, -15.74070752338412760, 5.000000000000000000 ) ) ;
#5828 = LINE ( 'NONE', #103552, #119294 ) ;
#5829 = VECTOR ( 'NONE', #113026, 1000.000000000000000 ) ;
#5830 = CARTESIAN_POINT ( 'NONE',  ( -24.29974487139158867, -27.71228299555223273, 4.000000000000000000 ) ) ;
#5831 = DIRECTION ( 'NONE',  ( -0.7071067811865486830, -0.7071067811865464625, 0.000000000000000000 ) ) ;
#5832 = EDGE_LOOP ( 'NONE', ( #100433, #111507, #56268, #60240 ) ) ;
#5833 = CARTESIAN_POINT ( 'NONE',  ( -14.99999999999989875, -1.209798855135683748, 4.371887122346860721 ) ) ;
#5834 = CARTESIAN_POINT ( 'NONE',  ( 2.816011393730999401, 28.73617430169785436, 5.000000000000000000 ) ) ;
#5835 = ORIENTED_EDGE ( 'NONE', *, *, #25142, .T. ) ;
#5836 = EDGE_CURVE ( 'NONE', #100683, #75407, #110403, .T. ) ;
#5838 = ORIENTED_EDGE ( 'NONE', *, *, #126830, .T. ) ;
#5837 = CARTESIAN_POINT ( 'NONE',  ( -5.903329358125916748, -2.240707523384260824, 15.26439735382751195 ) ) ;
#5839 = EDGE_CURVE ( 'NONE', #21613, #21499, #81109, .T. ) ;
#5840 = ORIENTED_EDGE ( 'NONE', *, *, #768, .F. ) ;
#5841 = CARTESIAN_POINT ( 'NONE',  ( -10.91502770842411785, 10.86848332146160168, -26.39372705248169027 ) ) ;
#5842 = FILL_AREA_STYLE_COLOUR ( '', #108488 ) ;
#5843 = ORIENTED_EDGE ( 'NONE', *, *, #121000, .T. ) ;
#5844 = LINE ( 'NONE', #61715, #30373 ) ;
#5845 = UNCERTAINTY_MEASURE_WITH_UNIT (LENGTH_MEASURE( 1.000000000000000082E-05 ), #115592, 'distance_accuracy_value', 'NONE');
#5846 = ADVANCED_FACE ( 'NONE', ( #11508 ), #55790, .F. ) ;
#5847 = VECTOR ( 'NONE', #121093, 1000.000000000000227 ) ;
#5848 = DIRECTION ( 'NONE',  ( -0.7071067811865486830, -0.7071067811865464625, 0.000000000000000000 ) ) ;
#5849 = VECTOR ( 'NONE', #77625, 1000.000000000000000 ) ;
#5850 = CARTESIAN_POINT ( 'NONE',  ( -28.43312800248725125, -21.74070752338406365, 6.915939825044140399 ) ) ;
#5851 = VERTEX_POINT ( 'NONE', #6323 ) ;
#5852 = FACE_OUTER_BOUND ( 'NONE', #69100, .T. ) ;
#5853 = CARTESIAN_POINT ( 'NONE',  ( -33.72281430457037743, -21.72499999999999432, 5.000000000000000000 ) ) ;
#5854 = FACE_OUTER_BOUND ( 'NONE', #83506, .T. ) ;
#5855 = CARTESIAN_POINT ( 'NONE',  ( -2.816011393730999401, 28.73617430169785436, 5.000000000000000000 ) ) ;
#5856 = CARTESIAN_POINT ( 'NONE',  ( 72.18398860626899705, 28.73617430169837661, 5.000000000000000000 ) ) ;
#5857 = EDGE_CURVE ( 'NONE', #104032, #131707, #137625, .T. ) ;
#5858 = CARTESIAN_POINT ( 'NONE',  ( 26.75159235450331963, 3.061616997868380183E-16, -2.500000000000001332 ) ) ;
#5859 = DIRECTION ( 'NONE',  ( -0.000000000000000000, 0.000000000000000000, 1.000000000000000000 ) ) ;
#5860 = CARTESIAN_POINT ( 'NONE',  ( 28.00000000000002487, -49.14999999999999147, 34.92500000000003268 ) ) ;
#5861 = CARTESIAN_POINT ( 'NONE',  ( -60.48921356237309510, -27.52281430457097500, 5.000000000000000000 ) ) ;
#5862 = ORIENTED_EDGE ( 'NONE', *, *, #137011, .F. ) ;
#5863 = ORIENTED_EDGE ( 'NONE', *, *, #117573, .T. ) ;
#5864 = ORIENTED_EDGE ( 'NONE', *, *, #31052, .F. ) ;
#5865 = CARTESIAN_POINT ( 'NONE',  ( 110.6666666666666572, 6.884901960086285300, 3.975000000000003642 ) ) ;
#5866 = ORIENTED_EDGE ( 'NONE', *, *, #57115, .F. ) ;
#5867 = ORIENTED_EDGE ( 'NONE', *, *, #121527, .T. ) ;
#5868 = ORIENTED_EDGE ( 'NONE', *, *, #126098, .F. ) ;
#5869 = EDGE_CURVE ( 'NONE', #118949, #14811, #5828, .T. ) ;
#5870 = CARTESIAN_POINT ( 'NONE',  ( 152.4000000000000057, -17.48000000000005016, 33.92499999999998295 ) ) ;
#5871 = ORIENTED_EDGE ( 'NONE', *, *, #129327, .F. ) ;
#5872 = DIRECTION ( 'NONE',  ( 0.000000000000000000, 0.000000000000000000, 1.000000000000000000 ) ) ;
#5873 = PLANE ( 'NONE',  #21001 ) ;
#5874 = PLANE ( 'NONE',  #51098 ) ;
#5875 = PLANE ( 'NONE',  #37181 ) ;
#5876 = CARTESIAN_POINT ( 'NONE',  ( 111.8545968585647756, -1.637169565754161615, 6.110000000000000320 ) ) ;
#5877 = ORIENTED_EDGE ( 'NONE', *, *, #39549, .F. ) ;
#5878 = DIRECTION ( 'NONE',  ( -1.000000000000000000, -0.000000000000000000, -0.000000000000000000 ) ) ;
#5879 = DIRECTION ( 'NONE',  ( 0.7071067811865487940, -0.7071067811865463515, 0.000000000000000000 ) ) ;
#5880 = PLANE ( 'NONE',  #68208 ) ;
#5881 = CARTESIAN_POINT ( 'NONE',  ( -29.99451991528749417, 28.92564299267958816, 4.000000000000000000 ) ) ;
#5882 = DIRECTION ( 'NONE',  ( -0.7071067811865486830, -0.7071067811865464625, -0.000000000000000000 ) ) ;
#5883 = PLANE ( 'NONE',  #138044 ) ;
#5884 = CARTESIAN_POINT ( 'NONE',  ( 42.22502705046289861, 5.819803920172573086, -5.819803920172572198 ) ) ;
#5885 = ADVANCED_FACE ( 'NONE', ( #58535 ), #93952, .F. ) ;
#5886 = CARTESIAN_POINT ( 'NONE',  ( -14.91685193227060324, 21.75929247661549937, 7.311836541448015758 ) ) ;
#5887 = FILL_AREA_STYLE_COLOUR ( '', #129432 ) ;
#5888 = ORIENTED_EDGE ( 'NONE', *, *, #21651, .F. ) ;
#5889 = ORIENTED_EDGE ( 'NONE', *, *, #92510, .F. ) ;
#5890 = CARTESIAN_POINT ( 'NONE',  ( 37.89583333333332860, -2.130196079827427091, 7.949999999999999289 ) ) ;
#5891 = ORIENTED_EDGE ( 'NONE', *, *, #50407, .F. ) ;
#5892 = LINE ( 'NONE', #14668, #122730 ) ;
#5893 = DIRECTION ( 'NONE',  ( -0.7071067811865486830, -0.7071067811865464625, 0.000000000000000000 ) ) ;
#5894 = PLANE ( 'NONE',  #45753 ) ;
#5895 = CARTESIAN_POINT ( 'NONE',  ( 32.20710678118632586, -11.24070752338416845, 5.000000000000000000 ) ) ;
#5896 = DIRECTION ( 'NONE',  ( -0.6830127018922180770, -0.6830127018922204085, -0.2588190451025213501 ) ) ;
#5897 = DIRECTION ( 'NONE',  ( 0.6830127018922181881, 0.6830127018922202975, -0.2588190451025214056 ) ) ;
#5898 = CARTESIAN_POINT ( 'NONE',  ( 30.62543019189810423, 5.291415217122919401, 3.055000000000002824 ) ) ;
#5899 = VERTEX_POINT ( 'NONE', #30428 ) ;
#5900 = EDGE_CURVE ( 'NONE', #108030, #94785, #76072, .T. ) ;
#5901 = CARTESIAN_POINT ( 'NONE',  ( 18.63999999999999702, -2.055000000000000160, 0.000000000000000000 ) ) ;
#5902 = EDGE_LOOP ( 'NONE', ( #46119, #25945, #122339, #12117 ) ) ;
#5903 = CARTESIAN_POINT ( 'NONE',  ( -15.48921356237309510, -27.52281430457066236, 5.000000000000000000 ) ) ;
#5904 = LINE ( 'NONE', #138613, #112472 ) ;
#5905 = CARTESIAN_POINT ( 'NONE',  ( -2.999999999999976463, 4.552185695429124657, 5.000000000000000000 ) ) ;
#5906 = DIRECTION ( 'NONE',  ( 0.6830127018922181881, 0.6830127018922202975, -0.2588190451025214056 ) ) ;
#5907 = ORIENTED_EDGE ( 'NONE', *, *, #75688, .T. ) ;
#5908 = CARTESIAN_POINT ( 'NONE',  ( 58.77126352523142572, 4.472830434245839371, 4.472830434245842035 ) ) ;
#5909 = ADVANCED_FACE ( 'NONE', ( #65942 ), #10085, .F. ) ;
#5910 = ORIENTED_EDGE ( 'NONE', *, *, #132851, .F. ) ;
#5911 = DIRECTION ( 'NONE',  ( 0.6830127018922180770, -0.6830127018922204085, -0.2588190451025213501 ) ) ;
#5912 = CARTESIAN_POINT ( 'NONE',  ( 75.48921356237309510, -27.52281430457107803, 5.000000000000000000 ) ) ;
#5913 = CARTESIAN_POINT ( 'NONE',  ( 31.49999999999977973, -17.91344420646039737, 1.358650452708537681 ) ) ;
#5914 = LINE ( 'NONE', #5212, #141294 ) ;
#5915 = VECTOR ( 'NONE', #91011, 999.9999999999998863 ) ;
#5916 = CARTESIAN_POINT ( 'NONE',  ( 52.12043019189811588, 3.055000000000001936, -5.291415217122916737 ) ) ;
#5917 = ORIENTED_EDGE ( 'NONE', *, *, #56181, .T. ) ;
#5918 = AXIS2_PLACEMENT_3D ( 'NONE', #41789, #131659, #107027 ) ;
#5919 = DIRECTION ( 'NONE',  ( -0.000000000000000000, -0.3543493200069152693, 0.9351131265310292928 ) ) ;
#5920 = ADVANCED_FACE ( 'NONE', ( #31156 ), #142753, .T. ) ;
#5921 = PLANE ( 'NONE',  #124260 ) ;
#5922 = ORIENTED_EDGE ( 'NONE', *, *, #40593, .T. ) ;
#5923 = ORIENTED_EDGE ( 'NONE', *, *, #16193, .T. ) ;
#5924 = LINE ( 'NONE', #6621, #28476 ) ;
#5925 = VERTEX_POINT ( 'NONE', #55048 ) ;
#5926 =( BOUNDED_CURVE ( )  B_SPLINE_CURVE ( 3, ( #20520, #12519, #44480, #100959 ),
 .UNSPECIFIED., .F., .F. ) 
 B_SPLINE_CURVE_WITH_KNOTS ( ( 4, 4 ),
 ( 6.095931195673056635, 6.243513561394028244 ),
 .UNSPECIFIED. ) 
 CURVE ( )  GEOMETRIC_REPRESENTATION_ITEM ( )  RATIONAL_B_SPLINE_CURVE ( ( 1.000000000000000000, 0.9981857772260753769, 0.9981857772260753769, 1.000000000000000000 ) ) 
 REPRESENTATION_ITEM ( '' )  );
#5927 = CARTESIAN_POINT ( 'NONE',  ( 59.72502705046289861, 5.819803920172573974, -5.819803920172573086 ) ) ;
#5928 = EDGE_CURVE ( 'NONE', #35299, #133165, #139923, .T. ) ;
#5929 = ORIENTED_EDGE ( 'NONE', *, *, #63416, .F. ) ;
#5930 = CARTESIAN_POINT ( 'NONE',  ( 22.49999999999984723, -4.533600742197692490, 5.000000000000000000 ) ) ;
#5931 = CARTESIAN_POINT ( 'NONE',  ( 26.40000000000000568, -17.48000000000005016, 33.92499999999998295 ) ) ;
#5932 = EDGE_CURVE ( 'NONE', #77443, #96830, #77525, .T. ) ;
#5933 = FACE_BOUND ( 'NONE', #118698, .T. ) ;
#5934 = CARTESIAN_POINT ( 'NONE',  ( -27.29974487139158512, -27.71228299555225405, 4.000000000000000000 ) ) ;
#5935 = CARTESIAN_POINT ( 'NONE',  ( 0.2569208697893814453, 4.202752102959690472E-16, 0.000000000000000000 ) ) ;
#5937 = EDGE_CURVE ( 'NONE', #140592, #131858, #101384, .T. ) ;
#5936 = CARTESIAN_POINT ( 'NONE',  ( 21.48921356237309155, -27.52281430457070499, 5.000000000000000000 ) ) ;
#5938 = ORIENTED_EDGE ( 'NONE', *, *, #40608, .T. ) ;
#5939 = CARTESIAN_POINT ( 'NONE',  ( -2.999999999999978240, -3.485240976185081330, -4.108735105802402643 ) ) ;
#5941 = VERTEX_POINT ( 'NONE', #2029 ) ;
#5940 = DIRECTION ( 'NONE',  ( 0.000000000000000000, 0.000000000000000000, 1.000000000000000000 ) ) ;
#5942 = ORIENTED_EDGE ( 'NONE', *, *, #80045, .T. ) ;
#5943 = DIRECTION ( 'NONE',  ( -0.6830127018922181881, 0.6830127018922202975, -0.2588190451025214056 ) ) ;
#5944 = CIRCLE ( 'NONE', #114720, 2.055000000000000604 ) ;
#5945 = VERTEX_POINT ( 'NONE', #24536 ) ;
#5947 = ORIENTED_EDGE ( 'NONE', *, *, #92590, .T. ) ;
#5946 = VECTOR ( 'NONE', #140047, 1000.000000000000000 ) ;
#5948 = CARTESIAN_POINT ( 'NONE',  ( 68.01626352523145158, -4.472830434245838482, 4.472830434245838482 ) ) ;
#5949 = VERTEX_POINT ( 'NONE', #68790 ) ;
#5950 = CIRCLE ( 'NONE', #45358, 2.500000000000000888 ) ;
#5951 = PLANE ( 'NONE',  #88052 ) ;
#5952 = CONICAL_SURFACE ( 'NONE', #10620, 2.055000000000000604, 0.9599310885968764806 ) ;
#5953 = CARTESIAN_POINT ( 'NONE',  ( 21.18398860626899349, 28.73617430169802134, 5.000000000000000000 ) ) ;
#5954 = ORIENTED_EDGE ( 'NONE', *, *, #68503, .F. ) ;
#5955 =( LENGTH_UNIT ( ) NAMED_UNIT ( * ) SI_UNIT ( .MILLI., .METRE. ) );
#5956 = EDGE_CURVE ( 'NONE', #39954, #101036, #102117, .T. ) ;
#5957 = CARTESIAN_POINT ( 'NONE',  ( -15.48921356237309510, -27.52281430457066236, 5.000000000000000000 ) ) ;
#5958 = CARTESIAN_POINT ( 'NONE',  ( -19.49999999999986855, -11.56887692260769640, 4.000000000000000000 ) ) ;
#5959 = DIRECTION ( 'NONE',  ( 0.7071067811865487940, 0.7071067811865463515, -0.000000000000000000 ) ) ;
#5960 = DIRECTION ( 'NONE',  ( -0.7071067811865486830, -0.7071067811865464625, 0.000000000000000000 ) ) ;
#5961 = LINE ( 'NONE', #18264, #74063 ) ;
#5962 = EDGE_LOOP ( 'NONE', ( #71684, #83183, #137721, #5744 ) ) ;
#5963 = ORIENTED_EDGE ( 'NONE', *, *, #120606, .F. ) ;
#5964 = DIRECTION ( 'NONE',  ( 0.7071067811865487940, 0.7071067811865463515, 0.000000000000000000 ) ) ;
#5965 = CARTESIAN_POINT ( 'NONE',  ( -5.700255128608413102, -27.71228299555201957, 4.000000000000000000 ) ) ;
#5966 = VERTEX_POINT ( 'NONE', #16495 ) ;
#5967 = ORIENTED_EDGE ( 'NONE', *, *, #74661, .T. ) ;
#5968 = VERTEX_POINT ( 'NONE', #104210 ) ;
#5969 = FACE_OUTER_BOUND ( 'NONE', #49967, .T. ) ;
#5970 = LINE ( 'NONE', #138687, #77635 ) ;
#5971 = CARTESIAN_POINT ( 'NONE',  ( -22.25154412867562215, -11.24070752338416845, 10.39518518046014428 ) ) ;
#5972 = EDGE_LOOP ( 'NONE', ( #131728, #84926, #48273, #75427, #99710 ) ) ;
#5973 = DIRECTION ( 'NONE',  ( -0.7071067811865487940, 0.7071067811865463515, -0.000000000000000000 ) ) ;
#5974 =( LENGTH_UNIT ( ) NAMED_UNIT ( * ) SI_UNIT ( .MILLI., .METRE. ) );
#5975 = CARTESIAN_POINT ( 'NONE',  ( 12.46290314143521982, -3.967499999999994476, 6.871911579029513106 ) ) ;
#5976 = EDGE_CURVE ( 'NONE', #49913, #55910, #118498, .T. ) ;
#5977 = DIRECTION ( 'NONE',  ( -0.000000000000000000, 0.000000000000000000, 1.000000000000000000 ) ) ;
#5978 = ORIENTED_EDGE ( 'NONE', *, *, #78620, .F. ) ;
#5979 = EDGE_CURVE ( 'NONE', #119189, #126916, #98194, .T. ) ;
#5980 = CARTESIAN_POINT ( 'NONE',  ( -15.70710678118642711, -9.740707523384180888, 5.000000000000000000 ) ) ;
#5981 = CARTESIAN_POINT ( 'NONE',  ( 2.924914550060625285, 4.584330080086930965E-16, 0.000000000000000000 ) ) ;
#5983 = ORIENTED_EDGE ( 'NONE', *, *, #18800, .F. ) ;
#5982 = CARTESIAN_POINT ( 'NONE',  ( -51.29974487139158867, -27.71228299555242103, 4.000000000000000000 ) ) ;
#5984 = LINE ( 'NONE', #93755, #114184 ) ;
#5985 = ORIENTED_EDGE ( 'NONE', *, *, #11317, .F. ) ;
#5986 = DIRECTION ( 'NONE',  ( 0.3543493200069162685, -0.000000000000000000, -0.9351131265310288487 ) ) ;
#5987 = LINE ( 'NONE', #124946, #104760 ) ;
#5988 = ADVANCED_FACE ( 'NONE', ( #88763 ), #64140, .F. ) ;
#5989 = EDGE_CURVE ( 'NONE', #13100, #65062, #2409, .T. ) ;
#5990 = DIRECTION ( 'NONE',  ( -1.000000000000000000, -0.000000000000000000, -0.000000000000000000 ) ) ;
#5991 = VERTEX_POINT ( 'NONE', #113325 ) ;
#5992 = FACE_OUTER_BOUND ( 'NONE', #113046, .T. ) ;
#5993 = DIRECTION ( 'NONE',  ( -0.7071067811865486830, -0.7071067811865464625, -0.000000000000000000 ) ) ;
#5994 = CARTESIAN_POINT ( 'NONE',  ( 4.911592354503321545, -3.851859888774471706E-31, 2.500000000000001332 ) ) ;
#5995 = DIRECTION ( 'NONE',  ( 0.6830127018922181881, 0.6830127018922202975, -0.2588190451025214056 ) ) ;
#5996 = ORIENTED_EDGE ( 'NONE', *, *, #102459, .T. ) ;
#5997 = CARTESIAN_POINT ( 'NONE',  ( -2.999999999999988898, 20.58746187583904330, 4.000000000000000000 ) ) ;
#5998 = DIRECTION ( 'NONE',  ( -0.5735764363510501562, 0.8191520442889890230, 1.003171929053521419E-16 ) ) ;
#5999 = LINE ( 'NONE', #50275, #16807 ) ;
#6000 = CARTESIAN_POINT ( 'NONE',  ( 15.29974487139158867, -27.71228299555216879, 4.000000000000000000 ) ) ;
#6001 = EDGE_CURVE ( 'NONE', #75950, #130884, #33651, .T. ) ;
#6002 = DIRECTION ( 'NONE',  ( 0.000000000000000000, -1.000000000000000000, 0.000000000000000000 ) ) ;
#6003 = EDGE_LOOP ( 'NONE', ( #90568, #40275, #8693, #76532 ) ) ;
#6004 = EDGE_CURVE ( 'NONE', #13171, #10686, #5970, .T. ) ;
#6005 = ORIENTED_EDGE ( 'NONE', *, *, #33335, .F. ) ;
#6006 = CARTESIAN_POINT ( 'NONE',  ( -28.49999999999980105, -7.912538124160673370, 4.000000000000000000 ) ) ;
#6007 = CARTESIAN_POINT ( 'NONE',  ( 6.229065384000522343, 3.061616997868383634E-16, -2.500000000000000444 ) ) ;
#6008 = CARTESIAN_POINT ( 'NONE',  ( 1.291236474768552966, -9.717572351234235426E-16, -7.934999999999990727 ) ) ;
#6009 = AXIS2_PLACEMENT_3D ( 'NONE', #102249, #137001, #104341 ) ;
#6010 = CARTESIAN_POINT ( 'NONE',  ( 16.76840764549667639, 2.499999999999998224, 3.061616997868380183E-16 ) ) ;
#6011 = PLANE ( 'NONE',  #87804 ) ;
#6012 = CARTESIAN_POINT ( 'NONE',  ( 17.99451991528748351, 28.92564299267950645, 4.000000000000000000 ) ) ;
#6013 = EDGE_CURVE ( 'NONE', #123729, #4663, #15151, .T. ) ;
#6014 = CARTESIAN_POINT ( 'NONE',  ( -20.99451991528748707, 28.92564299267952777, 4.000000000000000000 ) ) ;
#6015 = ORIENTED_EDGE ( 'NONE', *, *, #40694, .F. ) ;
#6016 = CARTESIAN_POINT ( 'NONE',  ( -34.42500000000001137, -15.02281430457042077, 5.000000000000000000 ) ) ;
#6017 = DIRECTION ( 'NONE',  ( 0.7071067811865486830, -0.7071067811865464625, -0.000000000000000000 ) ) ;
#6018 = DIRECTION ( 'NONE',  ( 0.7071067811865486830, -0.7071067811865464625, -0.000000000000000000 ) ) ;
#6019 = ADVANCED_FACE ( 'NONE', ( #51671 ), #49552, .F. ) ;
#6020 = DIRECTION ( 'NONE',  ( -0.000000000000000000, 0.000000000000000000, 1.000000000000000000 ) ) ;
#6021 = CARTESIAN_POINT ( 'NONE',  ( 50.51626352523143737, -4.472830434245839371, 4.472830434245839371 ) ) ;
#6022 = CARTESIAN_POINT ( 'NONE',  ( 25.39999999999999858, -7.600000000000061817, 28.92499999999998650 ) ) ;
#6023 = VERTEX_POINT ( 'NONE', #39375 ) ;
#6024 = SURFACE_STYLE_USAGE ( .BOTH. , #103918 ) ;
#6025 = VERTEX_POINT ( 'NONE', #52363 ) ;
#6026 = AXIS2_PLACEMENT_3D ( 'NONE', #130914, #131611, #73658 ) ;
#6027 = ORIENTED_EDGE ( 'NONE', *, *, #62008, .F. ) ;
#6028 = EDGE_CURVE ( 'NONE', #107292, #25402, #140785, .T. ) ;
#6029 = DIRECTION ( 'NONE',  ( 0.7071067811865487940, -0.7071067811865463515, 0.000000000000000000 ) ) ;
#6030 = LINE ( 'NONE', #83671, #34674 ) ;
#6031 = LINE ( 'NONE', #37285, #125268 ) ;
#6032 = CARTESIAN_POINT ( 'NONE',  ( 34.92499999999998295, -5.240707523384228850, 4.255531930566196941 ) ) ;
#6033 = CARTESIAN_POINT ( 'NONE',  ( -24.91272823266826109, 2.053671025133813277, 5.000000000000000000 ) ) ;
#6034 = LINE ( 'NONE', #93094, #82455 ) ;
#6035 = VERTEX_POINT ( 'NONE', #140071 ) ;
#6036 = EDGE_CURVE ( 'NONE', #39260, #64733, #97975, .T. ) ;
#6037 = DIRECTION ( 'NONE',  ( 0.6830127018922181881, 0.6830127018922202975, -0.2588190451025214056 ) ) ;
#6038 = LINE ( 'NONE', #47502, #39923 ) ;
#6039 = EDGE_CURVE ( 'NONE', #44190, #78861, #128529, .T. ) ;
#6040 = LINE ( 'NONE', #40860, #140466 ) ;
#6041 = DIRECTION ( 'NONE',  ( -0.6830127018922181881, 0.6830127018922202975, -0.2588190451025214056 ) ) ;
#6042 = VECTOR ( 'NONE', #92227, 1000.000000000000000 ) ;
#6043 = DIRECTION ( 'NONE',  ( -0.7071067811865486830, -0.7071067811865464625, 0.000000000000000000 ) ) ;
#6045 = VECTOR ( 'NONE', #116093, 1000.000000000000000 ) ;
#6044 = VECTOR ( 'NONE', #132218, 1000.000000000000227 ) ;
#6046 = CARTESIAN_POINT ( 'NONE',  ( 69.64169371712952739, -2.130196079827424871, -7.949999999999999289 ) ) ;
#6047 = EDGE_CURVE ( 'NONE', #120101, #135455, #129060, .T. ) ;
#6048 = VECTOR ( 'NONE', #117323, 1000.000000000000000 ) ;
#6049 = CARTESIAN_POINT ( 'NONE',  ( 7.139999999999991687, -35.69931938766895740, -8.025146269613541605 ) ) ;
#6050 = ORIENTED_EDGE ( 'NONE', *, *, #122077, .T. ) ;
#6051 = ORIENTED_EDGE ( 'NONE', *, *, #2027, .T. ) ;
#6052 = CARTESIAN_POINT ( 'NONE',  ( 66.18749999999997158, -5.819803920172573086, 5.819803920172572198 ) ) ;
#6053 = CARTESIAN_POINT ( 'NONE',  ( -26.67183060077628554, 8.259292476615630818, 4.000000000000000000 ) ) ;
#6054 = CARTESIAN_POINT ( 'NONE',  ( -60.29974487139158867, -27.71228299555248142, 4.000000000000000000 ) ) ;
#6055 = VECTOR ( 'NONE', #21036, 1000.000000000000227 ) ;
#6056 = ORIENTED_EDGE ( 'NONE', *, *, #140735, .T. ) ;
#6057 = ADVANCED_FACE ( 'NONE', ( #130627 ), #97215, .T. ) ;
#6058 = CARTESIAN_POINT ( 'NONE',  ( -30.90450307870169766, 22.22500000000000142, 3.476483422452860239 ) ) ;
#6059 = FACE_OUTER_BOUND ( 'NONE', #96904, .T. ) ;
#6060 = CARTESIAN_POINT ( 'NONE',  ( 57.89626352523144703, 4.472830434245840259, -4.472830434245839371 ) ) ;
#6061 = DIRECTION ( 'NONE',  ( 1.000000000000000000, 1.224606353822377258E-16, 0.000000000000000000 ) ) ;
#6062 = ORIENTED_EDGE ( 'NONE', *, *, #94553, .T. ) ;
#6063 = ORIENTED_EDGE ( 'NONE', *, *, #71013, .T. ) ;
#6064 = DIRECTION ( 'NONE',  ( -0.000000000000000000, -0.3543493200069152693, 0.9351131265310292928 ) ) ;
#6065 = CARTESIAN_POINT ( 'NONE',  ( 15.18398860626900237, 28.73617430169797871, 5.000000000000000000 ) ) ;
#6066 = FACE_OUTER_BOUND ( 'NONE', #64628, .T. ) ;
#6067 = DIRECTION ( 'NONE',  ( -0.7071067811865486830, -0.7071067811865464625, 0.000000000000000000 ) ) ;
#6068 = CARTESIAN_POINT ( 'NONE',  ( -24.18398860626899705, 28.73617430169804265, 5.000000000000000000 ) ) ;
#6070 = EDGE_LOOP ( 'NONE', ( #28776, #43217, #123868, #124565 ) ) ;
#6069 = CARTESIAN_POINT ( 'NONE',  ( -16.64463492972600633, 0.4092709014657676114, -33.72289106502642397 ) ) ;
#6071 = DIRECTION ( 'NONE',  ( 0.6830127018922181881, 0.6830127018922202975, -0.2588190451025214056 ) ) ;
#6072 = CARTESIAN_POINT ( 'NONE',  ( 32.99451991528749062, 28.92564299267960948, 4.000000000000000000 ) ) ;
#6073 = CARTESIAN_POINT ( 'NONE',  ( 156.1499999999997783, -52.14999999999999147, -34.92499999999975557 ) ) ;
#6074 = LINE ( 'NONE', #28606, #4537 ) ;
#6075 = CARTESIAN_POINT ( 'NONE',  ( 77.99451991528749772, 28.92564299267992567, 4.000000000000000000 ) ) ;
#6076 = EDGE_LOOP ( 'NONE', ( #4019, #108807, #56374, #62669 ) ) ;
#6077 = ORIENTED_EDGE ( 'NONE', *, *, #81606, .F. ) ;
#6078 = CONICAL_SURFACE ( 'NONE', #77958, 2.055000000000001048, 0.9599310885968758145 ) ;
#6079 =( BOUNDED_CURVE ( )  B_SPLINE_CURVE ( 3, ( #113315, #130476, #114044, #40607 ),
 .UNSPECIFIED., .F., .T. ) 
 B_SPLINE_CURVE_WITH_KNOTS ( ( 4, 4 ),
 ( 1.864375635226932282, 1.933014472006554740 ),
 .UNSPECIFIED. ) 
 CURVE ( )  GEOMETRIC_REPRESENTATION_ITEM ( )  RATIONAL_B_SPLINE_CURVE ( ( 1.000000000000000000, 0.9996074310407762065, 0.9996074310407762065, 1.000000000000000000 ) ) 
 REPRESENTATION_ITEM ( '' )  );
#6080 = CARTESIAN_POINT ( 'NONE',  ( -20.99999999999985079, 16.93112307739201583, 4.000000000000000000 ) ) ;
#6081 = LINE ( 'NONE', #140907, #51084 ) ;
#6082 = LINE ( 'NONE', #50357, #24737 ) ;
#6083 = EDGE_CURVE ( 'NONE', #106022, #65082, #76223, .T. ) ;
#6084 = CARTESIAN_POINT ( 'NONE',  ( 110.7666937171295558, -7.949999999999998401, 2.130196079827423983 ) ) ;
#6085 = ORIENTED_EDGE ( 'NONE', *, *, #43646, .F. ) ;
#6086 = ORIENTED_EDGE ( 'NONE', *, *, #57634, .T. ) ;
#6087 = VECTOR ( 'NONE', #58225, 1000.000000000000000 ) ;
#6088 = CARTESIAN_POINT ( 'NONE',  ( 184.1500000000000057, -14.29000000000013593, 12.69999999999954632 ) ) ;
#6089 = ORIENTED_EDGE ( 'NONE', *, *, #35438, .F. ) ;
#6090 = VERTEX_POINT ( 'NONE', #52316 ) ;
#6091 = PLANE ( 'NONE',  #88476 ) ;
#6092 = ORIENTED_EDGE ( 'NONE', *, *, #14896, .T. ) ;
#6093 = DIRECTION ( 'NONE',  ( -0.000000000000000000, 0.000000000000000000, 1.000000000000000000 ) ) ;
#6095 = VECTOR ( 'NONE', #88825, 1000.000000000000000 ) ;
#6094 = DIRECTION ( 'NONE',  ( -0.6830127018922181881, 0.6830127018922202975, -0.2588190451025214056 ) ) ;
#6096 = ADVANCED_FACE ( 'NONE', ( #31996 ), #120389, .F. ) ;
#6097 = FACE_BOUND ( 'NONE', #23335, .T. ) ;
#6098 = CARTESIAN_POINT ( 'NONE',  ( 21.18398860626899349, 28.73617430169802134, 5.000000000000000000 ) ) ;
#6099 = EDGE_CURVE ( 'NONE', #40406, #27902, #137847, .T. ) ;
#6101 = ORIENTED_EDGE ( 'NONE', *, *, #65636, .T. ) ;
#6100 = DIRECTION ( 'NONE',  ( 0.000000000000000000, -0.9647414015272149923, 0.2631995976047557528 ) ) ;
#6102 =( BOUNDED_CURVE ( )  B_SPLINE_CURVE ( 3, ( #120506, #140851, #85769, #87212 ),
 .UNSPECIFIED., .F., .F. ) 
 B_SPLINE_CURVE_WITH_KNOTS ( ( 4, 4 ),
 ( 3.794322559382540927, 3.828945978481788526 ),
 .UNSPECIFIED. ) 
 CURVE ( )  GEOMETRIC_REPRESENTATION_ITEM ( )  RATIONAL_B_SPLINE_CURVE ( ( 1.000000000000000000, 0.9999001040657221617, 0.9999001040657221617, 1.000000000000000000 ) ) 
 REPRESENTATION_ITEM ( '' )  );
#6103 = EDGE_CURVE ( 'NONE', #72705, #8853, #13776, .T. ) ;
#6104 = APPLICATION_PROTOCOL_DEFINITION ( 'draft international standard', 'automotive_design', 1998, #23477 ) ;
#6106 = ORIENTED_EDGE ( 'NONE', *, *, #44004, .T. ) ;
#6105 = AXIS2_PLACEMENT_3D ( 'NONE', #94586, #114888, #27192 ) ;
#6107 = VERTEX_POINT ( 'NONE', #769 ) ;
#6108 = CARTESIAN_POINT ( 'NONE',  ( 92.37043019189810877, -3.055000000000001492, 5.291415217122917625 ) ) ;
#6109 = ORIENTED_EDGE ( 'NONE', *, *, #28072, .F. ) ;
#6110 =( GEOMETRIC_REPRESENTATION_CONTEXT ( 3 ) GLOBAL_UNCERTAINTY_ASSIGNED_CONTEXT ( ( #66366 ) ) GLOBAL_UNIT_ASSIGNED_CONTEXT ( ( #12189, #133982, #23043 ) ) REPRESENTATION_CONTEXT ( 'NONE', 'WORKASPACE' ) );
#6111 = ADVANCED_FACE ( 'NONE', ( #56658 ), #32, .F. ) ;
#6112 = FACE_OUTER_BOUND ( 'NONE', #73549, .T. ) ;
#6113 = MECHANICAL_DESIGN_GEOMETRIC_PRESENTATION_REPRESENTATION (  '', ( #89567 ), #91836 ) ;
#6114 = FACE_OUTER_BOUND ( 'NONE', #5816, .T. ) ;
#6115 = LINE ( 'NONE', #27188, #121942 ) ;
#6116 = EDGE_CURVE ( 'NONE', #76142, #127787, #47218, .T. ) ;
#6117 = CARTESIAN_POINT ( 'NONE',  ( 2.999999999999983569, 20.70535890316561733, 1.956823837851910053 ) ) ;
#6118 = ORIENTED_EDGE ( 'NONE', *, *, #114527, .T. ) ;
#6119 = CARTESIAN_POINT ( 'NONE',  ( 4.499999999999977796, 3.052185695429134871, 5.000000000000000000 ) ) ;
#6120 = CARTESIAN_POINT ( 'NONE',  ( 9.299744871391588674, -27.71228299555212971, 4.000000000000000000 ) ) ;
#6121 = VECTOR ( 'NONE', #80189, 1000.000000000000000 ) ;
#6122 = FACE_OUTER_BOUND ( 'NONE', #135234, .T. ) ;
#6124 = DIRECTION ( 'NONE',  ( 1.000000000000000000, 0.000000000000000000, 0.000000000000000000 ) ) ;
#6123 = DIRECTION ( 'NONE',  ( -1.000000000000000000, -1.743732761913359971E-15, 0.000000000000000000 ) ) ;
#6125 = DIRECTION ( 'NONE',  ( 0.000000000000000000, 1.000000000000000000, -0.000000000000000000 ) ) ;
#6126 = CYLINDRICAL_SURFACE ( 'NONE', #131908, 2.500000000000000000 ) ;
#6127 = EDGE_CURVE ( 'NONE', #17782, #4192, #2174, .T. ) ;
#6128 = CARTESIAN_POINT ( 'NONE',  ( 9.183988606268997046, 28.73617430169793607, 5.000000000000000000 ) ) ;
#6129 = ORIENTED_EDGE ( 'NONE', *, *, #106107, .T. ) ;
#6130 = DIRECTION ( 'NONE',  ( 0.7071067811865487940, 0.7071067811865463515, 0.000000000000000000 ) ) ;
#6131 = CARTESIAN_POINT ( 'NONE',  ( 4.499999999999972466, 16.08746187583908238, 4.000000000000000000 ) ) ;
#6132 = ORIENTED_EDGE ( 'NONE', *, *, #33506, .T. ) ;
#6134 = ORIENTED_EDGE ( 'NONE', *, *, #94707, .F. ) ;
#6133 = VECTOR ( 'NONE', #96664, 1000.000000000000000 ) ;
#6135 = ORIENTED_EDGE ( 'NONE', *, *, #123913, .T. ) ;
#6136 = CARTESIAN_POINT ( 'NONE',  ( 41.12543019189809712, 5.291415217122919401, 3.055000000000002824 ) ) ;
#6137 = EDGE_CURVE ( 'NONE', #10551, #40384, #70840, .T. ) ;
#6138 = VERTEX_POINT ( 'NONE', #11635 ) ;
#6139 = AXIS2_PLACEMENT_3D ( 'NONE', #95089, #106667, #108796 ) ;
#6140 = VECTOR ( 'NONE', #38596, 1000.000000000000227 ) ;
#6141 = AXIS2_PLACEMENT_3D ( 'NONE', #137176, #68375, #93668 ) ;
#6142 = CARTESIAN_POINT ( 'NONE',  ( 13.46247294953710494, -7.464222240803106570E-16, -6.094999999999989981 ) ) ;
#6143 = CARTESIAN_POINT ( 'NONE',  ( -15.35539145651694781, 3.520240452094296923, -29.92141252516384142 ) ) ;
#6144 = ORIENTED_EDGE ( 'NONE', *, *, #86457, .T. ) ;
#6145 = LINE ( 'NONE', #93904, #10938 ) ;
#6146 = EDGE_CURVE ( 'NONE', #86443, #122293, #88543, .T. ) ;
#6147 = ORIENTED_EDGE ( 'NONE', *, *, #11903, .T. ) ;
#6148 = CARTESIAN_POINT ( 'NONE',  ( 63.18398860626900415, 28.73617430169831621, 5.000000000000000000 ) ) ;
#6149 = AXIS2_PLACEMENT_3D ( 'NONE', #78136, #108558, #120151 ) ;
#6150 = DIRECTION ( 'NONE',  ( 0.7071067811865486830, -0.7071067811865464625, -0.000000000000000000 ) ) ;
#6152 = ORIENTED_EDGE ( 'NONE', *, *, #93674, .F. ) ;
#6151 = LINE ( 'NONE', #49733, #139709 ) ;
#6153 = ORIENTED_EDGE ( 'NONE', *, *, #83552, .T. ) ;
#6154 = DIRECTION ( 'NONE',  ( -0.000000000000000000, -0.3543493200069152693, 0.9351131265310292928 ) ) ;
#6155 = LINE ( 'NONE', #86453, #57459 ) ;
#6156 = ADVANCED_FACE ( 'NONE', ( #21834 ), #91397, .F. ) ;
#6157 = ADVANCED_FACE ( 'NONE', ( #112419 ), #45761, .F. ) ;
#6158 = ORIENTED_EDGE ( 'NONE', *, *, #12075, .F. ) ;
#6159 = PLANE ( 'NONE',  #62078 ) ;
#6160 = ORIENTED_EDGE ( 'NONE', *, *, #23573, .T. ) ;
#6161 = VERTEX_POINT ( 'NONE', #90684 ) ;
#6162 = EDGE_LOOP ( 'NONE', ( #135687, #45480, #50369 ) ) ;
#6163 = ORIENTED_EDGE ( 'NONE', *, *, #38798, .T. ) ;
#6164 = CARTESIAN_POINT ( 'NONE',  ( -16.49999999999988987, 10.08746187583914633, 4.000000000000000000 ) ) ;
#6165 = ADVANCED_FACE ( 'NONE', ( #22514 ), #134917, .F. ) ;
#6166 = CARTESIAN_POINT ( 'NONE',  ( 0.000000000000000000, 0.000000000000000000, 5.000000000000000000 ) ) ;
#6167 = CARTESIAN_POINT ( 'NONE',  ( 45.29974487139158867, -27.71228299555237840, 4.000000000000000000 ) ) ;
#6168 = EDGE_CURVE ( 'NONE', #124077, #55125, #124013, .T. ) ;
#6169 = DIRECTION ( 'NONE',  ( -0.7071067811865486830, -0.7071067811865464625, -0.000000000000000000 ) ) ;
#6170 = ORIENTED_EDGE ( 'NONE', *, *, #130276, .T. ) ;
#6171 = CARTESIAN_POINT ( 'NONE',  ( 65.75000000000000000, -9.735942053221458872E-16, 7.950000000000000178 ) ) ;
#6172 = ORIENTED_EDGE ( 'NONE', *, *, #59400, .T. ) ;
#6173 = CARTESIAN_POINT ( 'NONE',  ( 48.18398860626899705, 28.73617430169820608, 5.000000000000000000 ) ) ;
#6174 = CARTESIAN_POINT ( 'NONE',  ( 30.16623647476855652, 7.934999999999990727, -1.457635852685135314E-15 ) ) ;
#6175 = FACE_OUTER_BOUND ( 'NONE', #10922, .T. ) ;
#6176 = AXIS2_PLACEMENT_3D ( 'NONE', #9184, #290, #88785 ) ;
#6177 = CARTESIAN_POINT ( 'NONE',  ( 97.10416666666665719, 2.130196079827422206, 7.950000000000001954 ) ) ;
#6178 = ADVANCED_FACE ( 'NONE', ( #14530 ), #58808, .F. ) ;
#6179 = DIRECTION ( 'NONE',  ( -0.6830127018922180770, -0.6830127018922204085, -0.2588190451025213501 ) ) ;
#6180 = VERTEX_POINT ( 'NONE', #113833 ) ;
#6181 = VERTEX_POINT ( 'NONE', #3610 ) ;
#6182 = ORIENTED_EDGE ( 'NONE', *, *, #88186, .F. ) ;
#6183 = DIRECTION ( 'NONE',  ( 0.7071067811865486830, -0.7071067811865464625, -0.000000000000000000 ) ) ;
#6184 = DIRECTION ( 'NONE',  ( 0.7071067811865486830, -0.7071067811865464625, -0.000000000000000000 ) ) ;
#6185 = CARTESIAN_POINT ( 'NONE',  ( 0.7070132642930391231, -21.74070752338405654, 4.999753212805213565 ) ) ;
#6186 = CARTESIAN_POINT ( 'NONE',  ( -2.207106781186525701, -5.240707523384230626, 5.000000000000000000 ) ) ;
#6187 = EDGE_CURVE ( 'NONE', #46869, #21681, #47903, .T. ) ;
#6188 = CARTESIAN_POINT ( 'NONE',  ( 0.7113915074146799356, -49.19295221407797669, -41.21232802154111141 ) ) ;
#6189 = CARTESIAN_POINT ( 'NONE',  ( 72.82876352523145158, 0.000000000000000000, -6.109999999999999432 ) ) ;
#6190 = FACE_OUTER_BOUND ( 'NONE', #119830, .T. ) ;
#6191 = DIRECTION ( 'NONE',  ( -0.000000000000000000, -0.3543493200069152693, 0.9351131265310292928 ) ) ;
#6192 = LINE ( 'NONE', #125158, #14783 ) ;
#6193 = CARTESIAN_POINT ( 'NONE',  ( 9.183988606268997046, 28.73617430169793607, 5.000000000000000000 ) ) ;
#6194 = CARTESIAN_POINT ( 'NONE',  ( -33.18398860626899705, 28.73617430169810305, 5.000000000000000000 ) ) ;
#6195 = EDGE_LOOP ( 'NONE', ( #37305, #94825, #34967, #140249 ) ) ;
#6196 = LINE ( 'NONE', #104837, #49994 ) ;
#6197 = ORIENTED_EDGE ( 'NONE', *, *, #121037, .T. ) ;
#6198 = LINE ( 'NONE', #53309, #64677 ) ;
#6200 = ORIENTED_EDGE ( 'NONE', *, *, #115474, .F. ) ;
#6199 = FACE_OUTER_BOUND ( 'NONE', #116966, .T. ) ;
#6201 = VECTOR ( 'NONE', #88374, 1000.000000000000227 ) ;
#6202 = CARTESIAN_POINT ( 'NONE',  ( 34.42499999999998295, -21.72500000000000142, 0.5000000000000000000 ) ) ;
#6203 = CARTESIAN_POINT ( 'NONE',  ( -6.005480084712508493, 28.92564299267933947, 4.000000000000000000 ) ) ;
#6204 = ORIENTED_EDGE ( 'NONE', *, *, #41484, .F. ) ;
#6205 = ORIENTED_EDGE ( 'NONE', *, *, #103164, .F. ) ;
#6206 = CARTESIAN_POINT ( 'NONE',  ( 27.18398860626900060, 28.73617430169806042, 5.000000000000000000 ) ) ;
#6207 = CARTESIAN_POINT ( 'NONE',  ( 27.48921356237309155, -27.52281430457074762, 5.000000000000000000 ) ) ;
#6208 = DIRECTION ( 'NONE',  ( 4.681814790819592407E-17, 0.3543493200069153248, 0.9351131265310292928 ) ) ;
#6209 = VECTOR ( 'NONE', #133495, 999.9999999999998863 ) ;
#6210 = EDGE_CURVE ( 'NONE', #111332, #130548, #89267, .T. ) ;
#6211 = CARTESIAN_POINT ( 'NONE',  ( 96.18336038379621300, -2.130196079827426203, 7.949999999999997513 ) ) ;
#6213 = ADVANCED_FACE ( 'NONE', ( #124715 ), #21277, .F. ) ;
#6212 = LINE ( 'NONE', #94675, #2308 ) ;
#6214 = SURFACE_SIDE_STYLE ('',( #49800 ) ) ;
#6215 = ORIENTED_EDGE ( 'NONE', *, *, #86557, .T. ) ;
#6216 = VECTOR ( 'NONE', #35953, 1000.000000000000000 ) ;
#6217 = LINE ( 'NONE', #96801, #12201 ) ;
#6218 = PLANE ( 'NONE',  #87762 ) ;
#6219 = CARTESIAN_POINT ( 'NONE',  ( 20.85416666666666075, 1.633150327867695095, 6.094999999999988205 ) ) ;
#6220 = DIRECTION ( 'NONE',  ( -0.7071067811865486830, -0.7071067811865464625, 0.000000000000000000 ) ) ;
#6221 = LINE ( 'NONE', #38203, #5010 ) ;
#6222 = VERTEX_POINT ( 'NONE', #53173 ) ;
#6223 = LINE ( 'NONE', #5531, #97737 ) ;
#6224 = ORIENTED_EDGE ( 'NONE', *, *, #69725, .F. ) ;
#6225 = CARTESIAN_POINT ( 'NONE',  ( 88.52126352523143282, -4.472830434245839371, -4.472830434245840259 ) ) ;
#6226 = DIRECTION ( 'NONE',  ( -0.6830127018922180770, -0.6830127018922204085, -0.2588190451025213501 ) ) ;
#6227 = CARTESIAN_POINT ( 'NONE',  ( -34.92500000000001137, -22.22500000000000142, 4.000000000000000000 ) ) ;
#6228 = LINE ( 'NONE', #115706, #78026 ) ;
#6229 = ORIENTED_EDGE ( 'NONE', *, *, #125512, .T. ) ;
#6230 = CARTESIAN_POINT ( 'NONE',  ( -60.48921356237309510, -27.52281430457097500, 5.000000000000000000 ) ) ;
#6231 = LINE ( 'NONE', #71554, #122907 ) ;
#6232 = VECTOR ( 'NONE', #111125, 1000.000000000000000 ) ;
#6233 = DIRECTION ( 'NONE',  ( -0.000000000000000000, 0.3543493200069153248, 0.9351131265310291818 ) ) ;
#6234 = ORIENTED_EDGE ( 'NONE', *, *, #6647, .T. ) ;
#6235 = PLANE ( 'NONE',  #122501 ) ;
#6236 = FACE_OUTER_BOUND ( 'NONE', #5972, .T. ) ;
#6237 = VECTOR ( 'NONE', #76152, 1000.000000000000227 ) ;
#6238 = FILL_AREA_STYLE ('',( #84582 ) ) ;
#6239 = AXIS2_PLACEMENT_3D ( 'NONE', #6814, #40237, #118468 ) ;
#6240 = VERTEX_POINT ( 'NONE', #51779 ) ;
#6241 = ORIENTED_EDGE ( 'NONE', *, *, #53739, .F. ) ;
#6242 = AXIS2_PLACEMENT_3D ( 'NONE', #58229, #46643, #2324 ) ;
#6243 = CARTESIAN_POINT ( 'NONE',  ( 76.41709685856476142, 3.054999999999998828, 5.291415217122922066 ) ) ;
#6244 = ORIENTED_EDGE ( 'NONE', *, *, #137133, .F. ) ;
#6245 = DIRECTION ( 'NONE',  ( 0.000000000000000000, 0.000000000000000000, 1.000000000000000000 ) ) ;
#6246 = VECTOR ( 'NONE', #87593, 1000.000000000000000 ) ;
#6247 = ADVANCED_FACE ( 'NONE', ( #87248 ), #106839, .T. ) ;
#6249 = VECTOR ( 'NONE', #24832, 1000.000000000000114 ) ;
#6248 = CARTESIAN_POINT ( 'NONE',  ( 25.77149322861319547, 20.25929247661551003, 7.808871592221828806 ) ) ;
#6250 = LINE ( 'NONE', #17858, #112870 ) ;
#6251 = ORIENTED_EDGE ( 'NONE', *, *, #69555, .F. ) ;
#6252 = CARTESIAN_POINT ( 'NONE',  ( -22.49999999999984013, 8.319652575858368593, -8.582050562765878965 ) ) ;
#6253 = LINE ( 'NONE', #83158, #21269 ) ;
#6254 = ORIENTED_EDGE ( 'NONE', *, *, #8560, .T. ) ;
#6255 = CARTESIAN_POINT ( 'NONE',  ( 184.1500000000000057, -30.18000000000009564, 15.92499999999935945 ) ) ;
#6256 = CARTESIAN_POINT ( 'NONE',  ( 19.62719212111867151, -2.766370489448051195, 4.185522593092497523 ) ) ;
#6257 = ORIENTED_EDGE ( 'NONE', *, *, #68273, .T. ) ;
#6258 = EDGE_LOOP ( 'NONE', ( #30584, #78388, #115128, #54437 ) ) ;
#6259 = ADVANCED_FACE ( 'NONE', ( #10377 ), #97373, .F. ) ;
#6260 = EDGE_CURVE ( 'NONE', #1174, #89442, #138319, .T. ) ;
#6261 = EDGE_CURVE ( 'NONE', #88226, #134318, #142405, .T. ) ;
#6262 = DIRECTION ( 'NONE',  ( -0.7071067811865487940, 0.7071067811865463515, -0.000000000000000000 ) ) ;
#6263 = DIRECTION ( 'NONE',  ( -0.7071067811865486830, -0.7071067811865464625, 0.000000000000000000 ) ) ;
#6264 = VECTOR ( 'NONE', #121697, 1000.000000000000000 ) ;
#6265 = CARTESIAN_POINT ( 'NONE',  ( 53.74586038379622011, 3.974999999999996980, 6.884901960086287964 ) ) ;
#6266 = EDGE_CURVE ( 'NONE', #85257, #83184, #39743, .T. ) ;
#6267 = EDGE_CURVE ( 'NONE', #109290, #4040, #28847, .T. ) ;
#6268 = CARTESIAN_POINT ( 'NONE',  ( -26.95328719879335821, -22.22500000000000142, 1.979220021349709979 ) ) ;
#6269 = VERTEX_POINT ( 'NONE', #4891 ) ;
#6270 = AXIS2_PLACEMENT_3D ( 'NONE', #8493, #19414, #64355 ) ;
#6271 = EDGE_LOOP ( 'NONE', ( #17812, #77484, #66796, #71598 ) ) ;
#6272 = VERTEX_POINT ( 'NONE', #7037 ) ;
#6273 = EDGE_CURVE ( 'NONE', #70402, #40720, #73089, .T. ) ;
#6274 = ORIENTED_EDGE ( 'NONE', *, *, #47752, .T. ) ;
#6275 = VECTOR ( 'NONE', #135418, 1000.000000000000000 ) ;
#6276 = DIRECTION ( 'NONE',  ( -0.000000000000000000, 0.3543493200069153248, 0.9351131265310292928 ) ) ;
#6277 = EDGE_CURVE ( 'NONE', #116174, #63949, #51319, .T. ) ;
#6278 = EDGE_LOOP ( 'NONE', ( #93735, #76007, #88672, #139863 ) ) ;
#6279 = DIRECTION ( 'NONE',  ( -0.7071067811865486830, -0.7071067811865464625, -0.000000000000000000 ) ) ;
#6280 = LINE ( 'NONE', #83936, #5495 ) ;
#6281 = DIRECTION ( 'NONE',  ( 0.6830127018922180770, -0.6830127018922204085, -0.2588190451025213501 ) ) ;
#6282 = AXIS2_PLACEMENT_3D ( 'NONE', #100607, #10691, #24453 ) ;
#6283 = DIRECTION ( 'NONE',  ( 0.7071067811865487940, 0.7071067811865463515, 0.000000000000000000 ) ) ;
#6284 = CARTESIAN_POINT ( 'NONE',  ( 20.67906569311139009, 2.055000000000001048, 0.000000000000000000 ) ) ;
#6285 = ORIENTED_EDGE ( 'NONE', *, *, #113058, .F. ) ;
#6286 = LINE ( 'NONE', #15733, #139787 ) ;
#6287 = CARTESIAN_POINT ( 'NONE',  ( 51.29974487139158867, -27.71228299555242103, 4.000000000000000000 ) ) ;
#6288 = ORIENTED_EDGE ( 'NONE', *, *, #47317, .F. ) ;
#6289 = LINE ( 'NONE', #104198, #71388 ) ;
#6290 = ORIENTED_EDGE ( 'NONE', *, *, #14014, .F. ) ;
#6291 = CARTESIAN_POINT ( 'NONE',  ( 11.85830628287044242, -1.633150327867709528, 6.094999999999979323 ) ) ;
#6292 = ORIENTED_EDGE ( 'NONE', *, *, #28839, .T. ) ;
#6293 = ORIENTED_EDGE ( 'NONE', *, *, #53671, .F. ) ;
#6294 = CARTESIAN_POINT ( 'NONE',  ( 76.56293019189810423, 1.637169565754157174, 6.110000000000002984 ) ) ;
#6295 = EDGE_CURVE ( 'NONE', #137809, #3283, #49903, .T. ) ;
#6296 = ORIENTED_EDGE ( 'NONE', *, *, #109201, .T. ) ;
#6297 = CARTESIAN_POINT ( 'NONE',  ( -30.48921356237309510, -27.52281430457076894, 5.000000000000000000 ) ) ;
#6298 = CARTESIAN_POINT ( 'NONE',  ( -31.49999999999977263, 3.052185695429138423, 5.000000000000000000 ) ) ;
#6299 = AXIS2_PLACEMENT_3D ( 'NONE', #79846, #99374, #34161 ) ;
#6300 = CARTESIAN_POINT ( 'NONE',  ( 106.3129301918981042, -1.637169565754159617, -6.110000000000001208 ) ) ;
#6301 = PLANE ( 'NONE',  #121190 ) ;
#6302 = EDGE_CURVE ( 'NONE', #6161, #107344, #95509, .T. ) ;
#6303 = LINE ( 'NONE', #30996, #127439 ) ;
#6304 = CARTESIAN_POINT ( 'NONE',  ( 0.3281693992235254487, -18.74070752338409918, 4.000000000000000000 ) ) ;
#6305 = DIRECTION ( 'NONE',  ( -1.000000000000000000, 0.000000000000000000, 0.000000000000000000 ) ) ;
#6306 = CARTESIAN_POINT ( 'NONE',  ( 35.51669371712954870, 7.950000000000000178, -2.130196079827421318 ) ) ;
#6308 = EDGE_CURVE ( 'NONE', #90006, #132730, #15764, .T. ) ;
#6307 = DIRECTION ( 'NONE',  ( -0.000000000000000000, -0.3543493200069152693, 0.9351131265310292928 ) ) ;
#6309 = ORIENTED_EDGE ( 'NONE', *, *, #7550, .F. ) ;
#6310 = AXIS2_PLACEMENT_3D ( 'NONE', #32310, #142502, #122870 ) ;
#6311 = CARTESIAN_POINT ( 'NONE',  ( 26.99999999999980815, 14.58746187583910903, 4.000000000000000000 ) ) ;
#6312 = DIRECTION ( 'NONE',  ( 0.7071067811865486830, -0.7071067811865464625, -0.000000000000000000 ) ) ;
#6313 = ORIENTED_EDGE ( 'NONE', *, *, #6349, .T. ) ;
#6314 = ADVANCED_FACE ( 'NONE', ( #84654 ), #137618, .F. ) ;
#6315 = ORIENTED_EDGE ( 'NONE', *, *, #131542, .F. ) ;
#6316 = CARTESIAN_POINT ( 'NONE',  ( 20.19999999999999929, 9.521314400968980422E-16, 0.000000000000000000 ) ) ;
#6317 = ORIENTED_EDGE ( 'NONE', *, *, #76259, .T. ) ;
#6318 = EDGE_CURVE ( 'NONE', #130467, #69156, #43095, .T. ) ;
#6319 = AXIS2_PLACEMENT_3D ( 'NONE', #89117, #36849, #112982 ) ;
#6320 = ADVANCED_FACE ( 'NONE', ( #29530 ), #126701, .F. ) ;
#6321 = FACE_OUTER_BOUND ( 'NONE', #39398, .T. ) ;
#6322 = DIRECTION ( 'NONE',  ( 0.000000000000000000, -1.000000000000000000, 0.000000000000000000 ) ) ;
#6323 = CARTESIAN_POINT ( 'NONE',  ( -26.99999999999980815, -1.447814304570813393, 5.000000000000000000 ) ) ;
#6324 = AXIS2_PLACEMENT_3D ( 'NONE', #1990, #36804, #81050 ) ;
#6325 = FACE_OUTER_BOUND ( 'NONE', #85481, .T. ) ;
#6326 = CARTESIAN_POINT ( 'NONE',  ( 1.499999999999994449, -17.94781430457065241, 5.000000000000000000 ) ) ;
#6327 = ORIENTED_EDGE ( 'NONE', *, *, #13694, .T. ) ;
#6328 =( NAMED_UNIT ( * ) PLANE_ANGLE_UNIT ( ) SI_UNIT ( $, .RADIAN. ) );
#6329 = ORIENTED_EDGE ( 'NONE', *, *, #24203, .T. ) ;
#6330 = CIRCLE ( 'NONE', #119775, 2.500000000000000444 ) ;
#6331 = COLOUR_RGB ( '', 0.08235294, 0.09019608, 0.10196078) ;
#6332 = VECTOR ( 'NONE', #95614, 1000.000000000000000 ) ;
#6333 = CARTESIAN_POINT ( 'NONE',  ( 6.249569808101886004, 3.967499999999998916, 6.871911579029510442 ) ) ;
#6334 = CARTESIAN_POINT ( 'NONE',  ( 23.32000000000000028, -2.055000000000000160, 0.000000000000000000 ) ) ;
#6335 = DIRECTION ( 'NONE',  ( 1.000000000000000000, 0.000000000000000000, 0.000000000000000000 ) ) ;
#6336 = ADVANCED_FACE ( 'NONE', ( #11325 ), #133866, .F. ) ;
#6337 = CARTESIAN_POINT ( 'NONE',  ( 14.47113640696344028, -9.396276906557130104, 1.425181317190020058 ) ) ;
#6338 = EDGE_LOOP ( 'NONE', ( #110820, #8572 ) ) ;
#6339 = ORIENTED_EDGE ( 'NONE', *, *, #22405, .T. ) ;
#6340 = ORIENTED_EDGE ( 'NONE', *, *, #44357, .F. ) ;
#6341 = DIRECTION ( 'NONE',  ( -1.000000000000000000, -1.224606353822377258E-16, -0.000000000000000000 ) ) ;
#6342 = CARTESIAN_POINT ( 'NONE',  ( 78.48921356237309510, -27.52281430457109934, 5.000000000000000000 ) ) ;
#6343 = VECTOR ( 'NONE', #87446, 1000.000000000000000 ) ;
#6344 = LINE ( 'NONE', #10482, #89010 ) ;
#6345 = CARTESIAN_POINT ( 'NONE',  ( 0.2569208697893813342, -0.4000000000000003553, 2.015694669338588429 ) ) ;
#6346 = LINE ( 'NONE', #73802, #113062 ) ;
#6347 = CARTESIAN_POINT ( 'NONE',  ( -10.49999999999992184, -17.56887692260763956, 4.000000000000000000 ) ) ;
#6348 = CARTESIAN_POINT ( 'NONE',  ( 2.292893218813440992, 17.25929247661554200, 5.000000000000000000 ) ) ;
#6349 = EDGE_CURVE ( 'NONE', #106517, #141915, #22920, .T. ) ;
#6350 = PRESENTATION_STYLE_ASSIGNMENT (( #7812 ) ) ;
#6351 = ORIENTED_EDGE ( 'NONE', *, *, #72046, .T. ) ;
#6352 = CARTESIAN_POINT ( 'NONE',  ( 73.62500000000000000, -7.950000000000000178, -4.867971026610729436E-16 ) ) ;
#6353 = LINE ( 'NONE', #50631, #68533 ) ;
#6354 = VERTEX_POINT ( 'NONE', #112294 ) ;
#6355 =( BOUNDED_CURVE ( )  B_SPLINE_CURVE ( 3, ( #74740, #8002, #98596, #96423 ),
 .UNSPECIFIED., .F., .T. ) 
 B_SPLINE_CURVE_WITH_KNOTS ( ( 4, 4 ),
 ( 2.779374508378132713, 4.199602562396796301 ),
 .UNSPECIFIED. ) 
 CURVE ( )  GEOMETRIC_REPRESENTATION_ITEM ( )  RATIONAL_B_SPLINE_CURVE ( ( 1.000000000000000000, 0.8388583629366715977, 0.8388583629366715977, 1.000000000000000000 ) ) 
 REPRESENTATION_ITEM ( '' )  );
#6356 = DIRECTION ( 'NONE',  ( -0.7071067811865487940, 0.7071067811865463515, -0.000000000000000000 ) ) ;
#6359 = EDGE_CURVE ( 'NONE', #55719, #15722, #2045, .T. ) ;
#6358 = ORIENTED_EDGE ( 'NONE', *, *, #32502, .T. ) ;
#6357 = CARTESIAN_POINT ( 'NONE',  ( 24.32816939922335209, 8.259292476615634371, 4.000000000000000000 ) ) ;
#6360 = DIRECTION ( 'NONE',  ( 0.7071067811865486830, -0.7071067811865464625, -0.000000000000000000 ) ) ;
#6362 = VECTOR ( 'NONE', #80751, 1000.000000000000000 ) ;
#6361 = DIRECTION ( 'NONE',  ( 0.7071067811865486830, -0.7071067811865464625, -0.000000000000000000 ) ) ;
#6363 = ORIENTED_EDGE ( 'NONE', *, *, #70716, .F. ) ;
#6364 = LINE ( 'NONE', #48499, #141521 ) ;
#6365 = EDGE_LOOP ( 'NONE', ( #104413, #132437, #110631, #104691 ) ) ;
#6366 = DIRECTION ( 'NONE',  ( 0.7071067811865487940, -0.7071067811865463515, 0.000000000000000000 ) ) ;
#6367 = CARTESIAN_POINT ( 'NONE',  ( 123.3083603837962130, 7.949999999999997513, 2.130196079827431088 ) ) ;
#6368 = VECTOR ( 'NONE', #98548, 999.9999999999998863 ) ;
#6369 = PLANE ( 'NONE',  #108681 ) ;
#6370 = CARTESIAN_POINT ( 'NONE',  ( 19.49999999999986500, -14.70932175296475108, -11.46312253303841544 ) ) ;
#6371 = CARTESIAN_POINT ( 'NONE',  ( -45.18398860626900415, 28.73617430169818832, 5.000000000000000000 ) ) ;
#6372 = CARTESIAN_POINT ( 'NONE',  ( 18.28838880452753202, -2.745211937670052560, 5.000000000000000000 ) ) ;
#6373 = DIRECTION ( 'NONE',  ( -0.7071067811865486830, 0.7071067811865464625, 0.000000000000000000 ) ) ;
#6374 = CARTESIAN_POINT ( 'NONE',  ( 30.16623647476855652, 7.934999999999990727, -1.457635852685135314E-15 ) ) ;
#6375 = CARTESIAN_POINT ( 'NONE',  ( 10.04123647476855297, 0.000000000000000000, 7.934999999999990727 ) ) ;
#6376 = DIRECTION ( 'NONE',  ( 0.7071067811865486830, -0.7071067811865464625, -0.000000000000000000 ) ) ;
#6377 = CARTESIAN_POINT ( 'NONE',  ( -34.45011844616454511, 16.51628081163731210, 5.000000000000000888 ) ) ;
#6378 = DIRECTION ( 'NONE',  ( -0.7071067811865487940, 0.7071067811865463515, -0.000000000000000000 ) ) ;
#6379 = EDGE_LOOP ( 'NONE', ( #65743, #142958, #61480, #86783 ) ) ;
#6380 = EDGE_CURVE ( 'NONE', #140629, #126534, #102133, .T. ) ;
#6381 = VERTEX_POINT ( 'NONE', #111560 ) ;
#6382 = CARTESIAN_POINT ( 'NONE',  ( 82.66666666666667140, 6.884901960086285300, 3.975000000000003642 ) ) ;
#6383 = EDGE_CURVE ( 'NONE', #3235, #28808, #23086, .T. ) ;
#6384 = SURFACE_STYLE_USAGE ( .BOTH. , #49966 ) ;
#6385 = VERTEX_POINT ( 'NONE', #122423 ) ;
#6386 = PRODUCT_DEFINITION_SHAPE ( 'NONE', 'NONE',  #114782 ) ;
#6387 = DIRECTION ( 'NONE',  ( 0.7071067811865486830, -0.7071067811865464625, -0.000000000000000000 ) ) ;
#6388 = DIRECTION ( 'NONE',  ( -0.7071067811865486830, -0.7071067811865464625, -0.000000000000000000 ) ) ;
#6389 = DIRECTION ( 'NONE',  ( 1.000000000000000000, 0.000000000000000000, 0.000000000000000000 ) ) ;
#6390 = ORIENTED_EDGE ( 'NONE', *, *, #94489, .F. ) ;
#6391 = CARTESIAN_POINT ( 'NONE',  ( 65.99451991528749772, 28.92564299267984396, 4.000000000000000000 ) ) ;
#6392 = CARTESIAN_POINT ( 'NONE',  ( 8.031592354503320763, 2.500000000000001776, 0.000000000000000000 ) ) ;
#6393 = DIRECTION ( 'NONE',  ( -0.3543493200069162685, -0.000000000000000000, -0.9351131265310288487 ) ) ;
#6394 = DIRECTION ( 'NONE',  ( -0.7071067811865486830, -0.7071067811865464625, 0.000000000000000000 ) ) ;
#6395 = ADVANCED_FACE ( 'NONE', ( #67368 ), #113705, .T. ) ;
#6396 = CARTESIAN_POINT ( 'NONE',  ( -48.48921356237309510, -27.52281430457089328, 5.000000000000000000 ) ) ;
#6397 = CARTESIAN_POINT ( 'NONE',  ( -20.20710678118640047, 9.759292476615620160, 5.000000000000000000 ) ) ;
#6398 =( NAMED_UNIT ( * ) SI_UNIT ( $, .STERADIAN. ) SOLID_ANGLE_UNIT ( ) );
#6399 = FACE_OUTER_BOUND ( 'NONE', #95298, .T. ) ;
#6400 = DIRECTION ( 'NONE',  ( -0.6830127018922180770, -0.6830127018922204085, -0.2588190451025213501 ) ) ;
#6401 = DIRECTION ( 'NONE',  ( -0.000000000000000000, 0.3543493200069152138, -0.9351131265310292928 ) ) ;
#6402 = LINE ( 'NONE', #50682, #114722 ) ;
#6403 = CARTESIAN_POINT ( 'NONE',  ( 33.32816939922330590, 8.259292476615641476, 4.000000000000000000 ) ) ;
#6404 = EDGE_LOOP ( 'NONE', ( #63848, #56010, #39368, #102203 ) ) ;
#6405 = ORIENTED_EDGE ( 'NONE', *, *, #113080, .F. ) ;
#6406 = CARTESIAN_POINT ( 'NONE',  ( 99.60459685856476142, 1.637169565754164946, -6.109999999999999432 ) ) ;
#6407 = VECTOR ( 'NONE', #8272, 1000.000000000000000 ) ;
#6408 = EDGE_LOOP ( 'NONE', ( #84459, #11315, #37532, #89468 ) ) ;
#6409 = CARTESIAN_POINT ( 'NONE',  ( 123.3803752239310541, -44.19516442798762768, 34.92499999999998295 ) ) ;
#6410 = LINE ( 'NONE', #118793, #103326 ) ;
#6411 = ORIENTED_EDGE ( 'NONE', *, *, #11682, .F. ) ;
#6412 = DIRECTION ( 'NONE',  ( -0.6830127018922180770, -0.6830127018922204085, -0.2588190451025213501 ) ) ;
#6413 = CARTESIAN_POINT ( 'NONE',  ( 0.000000000000000000, 0.000000000000000000, 5.000000000000000000 ) ) ;
#6414 = AXIS2_PLACEMENT_3D ( 'NONE', #119813, #131446, #53908 ) ;
#6415 = CARTESIAN_POINT ( 'NONE',  ( 91.20376352523145158, 6.109999999999998543, 1.122388791418548911E-15 ) ) ;
#6416 = ORIENTED_EDGE ( 'NONE', *, *, #114822, .T. ) ;
#6417 = DIRECTION ( 'NONE',  ( 0.000000000000000000, -1.000000000000000000, 0.000000000000000000 ) ) ;
#6418 = VERTEX_POINT ( 'NONE', #56525 ) ;
#6419 = DIRECTION ( 'NONE',  ( 0.7071067811865486830, -0.7071067811865464625, -0.000000000000000000 ) ) ;
#6420 = LINE ( 'NONE', #50007, #42585 ) ;
#6421 = DIRECTION ( 'NONE',  ( 0.6830127018922180770, -0.6830127018922204085, -0.2588190451025213501 ) ) ;
#6422 = VECTOR ( 'NONE', #67943, 1000.000000000000227 ) ;
#6423 = CARTESIAN_POINT ( 'NONE',  ( 16.49999999999988631, -8.568876922607721269, 4.000000000000000000 ) ) ;
#6424 = EDGE_CURVE ( 'NONE', #46535, #89080, #23850, .T. ) ;
#6425 = EDGE_LOOP ( 'NONE', ( #110653, #55389, #64217, #42236 ) ) ;
#6426 = ORIENTED_EDGE ( 'NONE', *, *, #54087, .F. ) ;
#6427 = AXIS2_PLACEMENT_3D ( 'NONE', #98853, #42374, #53209 ) ;
#6428 = ORIENTED_EDGE ( 'NONE', *, *, #119260, .T. ) ;
#6429 = CARTESIAN_POINT ( 'NONE',  ( -32.57672154193627279, 11.25929247661560240, 17.85071094206591980 ) ) ;
#6430 = EDGE_CURVE ( 'NONE', #106470, #130798, #325, .T. ) ;
#6431 = DIRECTION ( 'NONE',  ( -1.000000000000000000, -1.224606353822377258E-16, -0.000000000000000000 ) ) ;
#6432 = CARTESIAN_POINT ( 'NONE',  ( 5.317069808101886785, -2.126176841940956130, 7.934999999999990727 ) ) ;
#6433 = VECTOR ( 'NONE', #116188, 1000.000000000000000 ) ;
#6434 = AXIS2_PLACEMENT_3D ( 'NONE', #115071, #112965, #112273 ) ;
#6435 = LINE ( 'NONE', #138445, #140581 ) ;
#6436 = EDGE_CURVE ( 'NONE', #10426, #23231, #46351, .T. ) ;
#6437 = ADVANCED_FACE ( 'NONE', ( #135482 ), #58676, .F. ) ;
#6438 = ADVANCED_FACE ( 'NONE', ( #15087 ), #3485, .F. ) ;
#6439 = VERTEX_POINT ( 'NONE', #70256 ) ;
#6440 = EDGE_LOOP ( 'NONE', ( #110970, #142495, #99455, #102318 ) ) ;
#6442 = EDGE_CURVE ( 'NONE', #118295, #83675, #136168, .T. ) ;
#6441 = FACE_OUTER_BOUND ( 'NONE', #125490, .T. ) ;
#6443 = ORIENTED_EDGE ( 'NONE', *, *, #126478, .F. ) ;
#6444 = ORIENTED_EDGE ( 'NONE', *, *, #60436, .F. ) ;
#6445 = ADVANCED_FACE ( 'NONE', ( #89802 ), #103517, .F. ) ;
#6446 = CARTESIAN_POINT ( 'NONE',  ( 112.9329301918981230, 1.637169565754156508, 6.110000000000000320 ) ) ;
#6447 = EDGE_CURVE ( 'NONE', #106060, #117536, #137084, .T. ) ;
#6448 = DIRECTION ( 'NONE',  ( -0.000000000000000000, 0.000000000000000000, 1.000000000000000000 ) ) ;
#6449 = LINE ( 'NONE', #50027, #77323 ) ;
#6450 = VERTEX_POINT ( 'NONE', #34930 ) ;
#6451 = CARTESIAN_POINT ( 'NONE',  ( 56.99999999999999289, 0.000000000000000000, -7.950000000000000178 ) ) ;
#6452 = LINE ( 'NONE', #84106, #22353 ) ;
#6453 = DIRECTION ( 'NONE',  ( 0.7071067811865486830, -0.7071067811865464625, -0.000000000000000000 ) ) ;
#6454 = DIRECTION ( 'NONE',  ( -1.000000000000000000, -1.224606353822377258E-16, -0.000000000000000000 ) ) ;
#6455 = VERTEX_POINT ( 'NONE', #78424 ) ;
#6456 = VECTOR ( 'NONE', #72795, 1000.000000000000227 ) ;
#6457 = EDGE_CURVE ( 'NONE', #26438, #32517, #13840, .T. ) ;
#6458 = CARTESIAN_POINT ( 'NONE',  ( 14.17270155891586825, -22.22500000000000142, -13.60495448913695249 ) ) ;
#6459 = CARTESIAN_POINT ( 'NONE',  ( 18.17159235450331778, -3.851859888774471706E-31, 2.500000000000001332 ) ) ;
#6460 = VERTEX_POINT ( 'NONE', #24741 ) ;
#6461 = CARTESIAN_POINT ( 'NONE',  ( -20.99451991528748707, 28.92564299267952777, 4.000000000000000000 ) ) ;
#6462 = CARTESIAN_POINT ( 'NONE',  ( 0.8348607551137282590, -0.4000000000000004108, 2.317232462839659224 ) ) ;
#6463 = SURFACE_STYLE_FILL_AREA ( #65214 ) ;
#6464 = ORIENTED_EDGE ( 'NONE', *, *, #61025, .F. ) ;
#6465 = DIRECTION ( 'NONE',  ( -0.3543493200069163240, -0.000000000000000000, 0.9351131265310288487 ) ) ;
#6466 = VERTEX_POINT ( 'NONE', #134970 ) ;
#6467 = VECTOR ( 'NONE', #96359, 1000.000000000000000 ) ;
#6468 = EDGE_LOOP ( 'NONE', ( #91660, #91671, #2360, #143260 ) ) ;
#6469 = EDGE_CURVE ( 'NONE', #126032, #12409, #68299, .T. ) ;
#6470 = EDGE_LOOP ( 'NONE', ( #136519, #119054, #125253, #118105 ) ) ;
#6471 = LINE ( 'NONE', #117400, #41800 ) ;
#6472 = CARTESIAN_POINT ( 'NONE',  ( 34.75611968250419181, 10.70565069852394302, 4.955485411084881164 ) ) ;
#6473 = LINE ( 'NONE', #41286, #33355 ) ;
#6474 = PLANE ( 'NONE',  #34631 ) ;
#6475 = CARTESIAN_POINT ( 'NONE',  ( 63.29974487139158867, -27.71228299555250274, 4.000000000000000000 ) ) ;
#6476 = FACE_OUTER_BOUND ( 'NONE', #63877, .T. ) ;
#6478 = DIRECTION ( 'NONE',  ( -0.7071067811865486830, 0.7071067811865464625, 0.000000000000000000 ) ) ;
#6477 = LINE ( 'NONE', #139931, #45878 ) ;
#6479 = AXIS2_PLACEMENT_3D ( 'NONE', #139930, #7938, #86249 ) ;
#6480 = CARTESIAN_POINT ( 'NONE',  ( 5.292893218813421896, 20.25929247661551713, 5.000000000000000000 ) ) ;
#6481 = VECTOR ( 'NONE', #103377, 1000.000000000000000 ) ;
#6482 = SURFACE_STYLE_USAGE ( .BOTH. , #83396 ) ;
#6483 = DIRECTION ( 'NONE',  ( 0.7071067811865487940, 0.7071067811865463515, 0.000000000000000000 ) ) ;
#6484 = CARTESIAN_POINT ( 'NONE',  ( 39.18398860626899705, 28.73617430169814568, 5.000000000000000000 ) ) ;
#6485 = ORIENTED_EDGE ( 'NONE', *, *, #86231, .F. ) ;
#6486 = EDGE_CURVE ( 'NONE', #71266, #17986, #111765, .T. ) ;
#6487 = ORIENTED_EDGE ( 'NONE', *, *, #81182, .F. ) ;
#6488 = VERTEX_POINT ( 'NONE', #103701 ) ;
#6489 = VERTEX_POINT ( 'NONE', #56714 ) ;
#6490 = CARTESIAN_POINT ( 'NONE',  ( -1.252866409880302623, 0.4270777084541245161, 3.798888653466065968 ) ) ;
#6491 = VERTEX_POINT ( 'NONE', #79172 ) ;
#6492 = EDGE_CURVE ( 'NONE', #31789, #27164, #23293, .T. ) ;
#6493 = ORIENTED_EDGE ( 'NONE', *, *, #42727, .F. ) ;
#6494 = CARTESIAN_POINT ( 'NONE',  ( -6.328169399223487090, -9.740707523384186217, 4.000000000000000000 ) ) ;
#6495 = LINE ( 'NONE', #93567, #94267 ) ;
#6496 = LINE ( 'NONE', #73258, #131904 ) ;
#6497 = ORIENTED_EDGE ( 'NONE', *, *, #50851, .T. ) ;
#6498 = FACE_OUTER_BOUND ( 'NONE', #38814, .T. ) ;
#6499 = VERTEX_POINT ( 'NONE', #125499 ) ;
#6500 = EDGE_CURVE ( 'NONE', #82848, #44234, #113896, .T. ) ;
#6501 = DIRECTION ( 'NONE',  ( 0.000000000000000000, 0.000000000000000000, 1.000000000000000000 ) ) ;
#6502 = FACE_OUTER_BOUND ( 'NONE', #112165, .T. ) ;
#6503 = CARTESIAN_POINT ( 'NONE',  ( 11.15040314143521982, 7.934999999999989839, -2.126176841940961904 ) ) ;
#6504 = ORIENTED_EDGE ( 'NONE', *, *, #71864, .T. ) ;
#6505 = CARTESIAN_POINT ( 'NONE',  ( 99.80793019189812298, -6.109999999999999432, 1.637169565754158507 ) ) ;
#6506 = PRESENTATION_LAYER_ASSIGNMENT (  '', '', ( #57508 ) ) ;
#6508 = EDGE_CURVE ( 'NONE', #78770, #9427, #2242, .T. ) ;
#6507 = LINE ( 'NONE', #73969, #118426 ) ;
#6509 = DIRECTION ( 'NONE',  ( -0.000000000000000000, -0.3543493200069152693, 0.9351131265310292928 ) ) ;
#6510 = ORIENTED_EDGE ( 'NONE', *, *, #72524, .F. ) ;
#6511 = ORIENTED_EDGE ( 'NONE', *, *, #85915, .F. ) ;
#6512 = CARTESIAN_POINT ( 'NONE',  ( -39.18398860626899705, 28.73617430169814568, 5.000000000000000000 ) ) ;
#6513 = ORIENTED_EDGE ( 'NONE', *, *, #369, .T. ) ;
#6514 = CARTESIAN_POINT ( 'NONE',  ( 151.4000000000000057, -16.48000000000005016, -33.92499999999998295 ) ) ;
#6515 = DIRECTION ( 'NONE',  ( 0.000000000000000000, -0.9647414015272155474, 0.2631995976047525887 ) ) ;
#6516 = CARTESIAN_POINT ( 'NONE',  ( 183.7681020908649714, -51.95642703809001972, -39.54367611436801866 ) ) ;
#6517 = ORIENTED_EDGE ( 'NONE', *, *, #53098, .F. ) ;
#6518 = DIRECTION ( 'NONE',  ( -0.3543493200069162685, -0.000000000000000000, -0.9351131265310288487 ) ) ;
#6519 = DIRECTION ( 'NONE',  ( -0.3543493200069162685, -0.000000000000000000, -0.9351131265310288487 ) ) ;
#6520 = DIRECTION ( 'NONE',  ( -0.6830127018922181881, 0.6830127018922202975, -0.2588190451025214056 ) ) ;
#6521 = VERTEX_POINT ( 'NONE', #69713 ) ;
#6522 = CARTESIAN_POINT ( 'NONE',  ( -7.940000000000001279, -35.14999999999999147, -10.00000000000000178 ) ) ;
#6523 = VECTOR ( 'NONE', #94747, 1000.000000000000000 ) ;
#6524 = VECTOR ( 'NONE', #135837, 1000.000000000000000 ) ;
#6525 = CARTESIAN_POINT ( 'NONE',  ( 17.06332250466817158, 4.584330080086930965E-16, 0.000000000000000000 ) ) ;
#6526 = ORIENTED_EDGE ( 'NONE', *, *, #116222, .T. ) ;
#6527 = AXIS2_PLACEMENT_3D ( 'NONE', #26477, #69283, #23615 ) ;
#6530 = ADVANCED_FACE ( 'NONE', ( #100875 ), #123376, .T. ) ;
#6529 = VERTEX_POINT ( 'NONE', #58137 ) ;
#6528 = PLANE ( 'NONE',  #32457 ) ;
#6531 = VECTOR ( 'NONE', #119413, 1000.000000000000000 ) ;
#6532 = EDGE_CURVE ( 'NONE', #97836, #130434, #135579, .T. ) ;
#6533 = ORIENTED_EDGE ( 'NONE', *, *, #58883, .F. ) ;
#6534 = CARTESIAN_POINT ( 'NONE',  ( 17.53719725875415847, 2.055000000000001048, 2.516649172247811554E-16 ) ) ;
#6535 = CARTESIAN_POINT ( 'NONE',  ( -14.81601139373099585, 28.73617430169776910, 5.000000000000000000 ) ) ;
#6536 = VECTOR ( 'NONE', #97245, 1000.000000000000000 ) ;
#6537 = VERTEX_POINT ( 'NONE', #103026 ) ;
#6538 = DIRECTION ( 'NONE',  ( -0.7071067811865486830, 0.7071067811865464625, 0.000000000000000000 ) ) ;
#6539 = CIRCLE ( 'NONE', #133986, 5.968999999999998529 ) ;
#6540 =( BOUNDED_CURVE ( )  B_SPLINE_CURVE ( 3, ( #51410, #71742, #60154, #104319 ),
 .UNSPECIFIED., .F., .T. ) 
 B_SPLINE_CURVE_WITH_KNOTS ( ( 4, 4 ),
 ( 1.964434688349485869, 3.503810798801452187 ),
 .UNSPECIFIED. ) 
 CURVE ( )  GEOMETRIC_REPRESENTATION_ITEM ( )  RATIONAL_B_SPLINE_CURVE ( ( 1.000000000000000000, 0.8120851936182275077, 0.8120851936182275077, 1.000000000000000000 ) ) 
 REPRESENTATION_ITEM ( '' )  );
#6541 = CARTESIAN_POINT ( 'NONE',  ( 21.79289321881331176, -17.24070752338410628, 5.000000000000000000 ) ) ;
#6542 = CARTESIAN_POINT ( 'NONE',  ( 9.792893218813397027, 9.759292476615621936, 5.000000000000000000 ) ) ;
#6543 = CARTESIAN_POINT ( 'NONE',  ( -12.48921356237309155, -27.52281430457064104, 5.000000000000000000 ) ) ;
#6544 = CARTESIAN_POINT ( 'NONE',  ( 19.35824297541128303, 15.75929247661556332, 19.34181609438695304 ) ) ;
#6545 = CARTESIAN_POINT ( 'NONE',  ( 2.770833333333333925, 6.094999999999991758, 1.633150327867686880 ) ) ;
#6546 = LINE ( 'NONE', #61723, #51720 ) ;
#6547 = CARTESIAN_POINT ( 'NONE',  ( 15.18398860626900237, 28.73617430169797871, 5.000000000000000000 ) ) ;
#6549 = VECTOR ( 'NONE', #105351, 1000.000000000000000 ) ;
#6548 = FACE_OUTER_BOUND ( 'NONE', #41963, .T. ) ;
#6550 = DIRECTION ( 'NONE',  ( 0.7071067811865487940, 0.7071067811865463515, 0.000000000000000000 ) ) ;
#6551 = CARTESIAN_POINT ( 'NONE',  ( -34.49999999999975131, -10.91253812416064228, 4.000000000000000000 ) ) ;
#6552 = FACE_OUTER_BOUND ( 'NONE', #50547, .T. ) ;
#6553 = ORIENTED_EDGE ( 'NONE', *, *, #107751, .T. ) ;
#6554 = EDGE_CURVE ( 'NONE', #10831, #24144, #47276, .T. ) ;
#6555 = ORIENTED_EDGE ( 'NONE', *, *, #123057, .F. ) ;
#6556 = ORIENTED_EDGE ( 'NONE', *, *, #25142, .F. ) ;
#6557 = CARTESIAN_POINT ( 'NONE',  ( 113.1458333333333144, 2.130196079827431976, -7.949999999999999289 ) ) ;
#6558 = VECTOR ( 'NONE', #96959, 1000.000000000000000 ) ;
#6559 = ADVANCED_FACE ( 'NONE', ( #47962 ), #3665, .T. ) ;
#6560 = ORIENTED_EDGE ( 'NONE', *, *, #1789, .T. ) ;
#6561 = VERTEX_POINT ( 'NONE', #17429 ) ;
#6562 = ORIENTED_EDGE ( 'NONE', *, *, #27556, .F. ) ;
#6563 = CARTESIAN_POINT ( 'NONE',  ( -21.18398860626899349, 28.73617430169802134, 5.000000000000000000 ) ) ;
#6564 = AXIS2_PLACEMENT_3D ( 'NONE', #35541, #11567, #81163 ) ;
#6565 = DIRECTION ( 'NONE',  ( -0.7071067811865487940, 0.7071067811865463515, -0.000000000000000000 ) ) ;
#6566 = VERTEX_POINT ( 'NONE', #115275 ) ;
#6567 = DIRECTION ( 'NONE',  ( 0.6830127018922180770, -0.6830127018922204085, -0.2588190451025213501 ) ) ;
#6568 = VECTOR ( 'NONE', #90022, 999.9999999999998863 ) ;
#6569 = CARTESIAN_POINT ( 'NONE',  ( 6.183988606268994381, 28.73617430169791476, 5.000000000000000000 ) ) ;
#6570 = VECTOR ( 'NONE', #135479, 1000.000000000000227 ) ;
#6571 = DIRECTION ( 'NONE',  ( -1.000000000000000000, -1.224606353822377258E-16, -0.000000000000000000 ) ) ;
#6572 = LINE ( 'NONE', #30534, #113753 ) ;
#6573 = CARTESIAN_POINT ( 'NONE',  ( 103.8337635252314328, 6.110000000000001208, 1.122388791418549305E-15 ) ) ;
#6574 = VERTEX_POINT ( 'NONE', #116748 ) ;
#6575 = EDGE_CURVE ( 'NONE', #25422, #129576, #82027, .T. ) ;
#6576 = LINE ( 'NONE', #4409, #144 ) ;
#6577 = FACE_OUTER_BOUND ( 'NONE', #128170, .T. ) ;
#6578 = CARTESIAN_POINT ( 'NONE',  ( -30.18398860626900060, 28.73617430169808173, 5.000000000000000000 ) ) ;
#6579 = CARTESIAN_POINT ( 'NONE',  ( 83.78752705046288440, 0.000000000000000000, -7.949999999999998401 ) ) ;
#6580 = AXIS2_PLACEMENT_3D ( 'NONE', #96258, #27446, #5690 ) ;
#6581 = DIRECTION ( 'NONE',  ( -0.7071067811865486830, -0.7071067811865464625, 0.000000000000000000 ) ) ;
#6582 = DIRECTION ( 'NONE',  ( -1.000000000000000000, 0.000000000000000000, 0.000000000000000000 ) ) ;
#6583 = CARTESIAN_POINT ( 'NONE',  ( 36.39169371712955581, 2.130196079827421762, 7.950000000000001066 ) ) ;
#6584 = CARTESIAN_POINT ( 'NONE',  ( -45.18398860626900415, 28.73617430169818832, 5.000000000000000000 ) ) ;
#6585 = FILL_AREA_STYLE_COLOUR ( '', #97108 ) ;
#6586 = ORIENTED_EDGE ( 'NONE', *, *, #98632, .F. ) ;
#6587 = ORIENTED_EDGE ( 'NONE', *, *, #69438, .F. ) ;
#6588 = CARTESIAN_POINT ( 'NONE',  ( 26.08333333333333215, 6.884901960086290629, -3.974999999999994316 ) ) ;
#6589 = ORIENTED_EDGE ( 'NONE', *, *, #113692, .T. ) ;
#6590 = CARTESIAN_POINT ( 'NONE',  ( -45.48921356237309510, -27.52281430457087197, 5.000000000000000000 ) ) ;
#6591 = DIRECTION ( 'NONE',  ( 0.7071067811865487940, -0.7071067811865463515, 0.000000000000000000 ) ) ;
#6592 = VECTOR ( 'NONE', #88065, 999.9999999999998863 ) ;
#6593 = CARTESIAN_POINT ( 'NONE',  ( 4.499999999999968914, 3.653845994658392993, -4.504631822206380143 ) ) ;
#6594 = VECTOR ( 'NONE', #34246, 1000.000000000000000 ) ;
#6595 = LINE ( 'NONE', #116113, #25603 ) ;
#6596 = CARTESIAN_POINT ( 'NONE',  ( 29.89626352523142927, 4.472830434245840259, -4.472830434245839371 ) ) ;
#6597 = ORIENTED_EDGE ( 'NONE', *, *, #51752, .T. ) ;
#6598 = DIRECTION ( 'NONE',  ( 0.7071067811865486830, -0.7071067811865464625, -0.000000000000000000 ) ) ;
#6599 = VERTEX_POINT ( 'NONE', #71850 ) ;
#6600 = DIRECTION ( 'NONE',  ( 0.6830127018922180770, -0.6830127018922204085, -0.2588190451025213501 ) ) ;
#6601 = DIRECTION ( 'NONE',  ( -0.3543493200069162685, -0.000000000000000000, -0.9351131265310288487 ) ) ;
#6602 = FACE_OUTER_BOUND ( 'NONE', #109818, .T. ) ;
#6603 = LINE ( 'NONE', #50888, #69652 ) ;
#6604 = ORIENTED_EDGE ( 'NONE', *, *, #136946, .F. ) ;
#6605 = CARTESIAN_POINT ( 'NONE',  ( 55.41709685856477563, 3.054999999999998828, 5.291415217122922066 ) ) ;
#6606 = ORIENTED_EDGE ( 'NONE', *, *, #112550, .F. ) ;
#6607 = CYLINDRICAL_SURFACE ( 'NONE', #107239, 7.950000000000000178 ) ;
#6608 = PLANE ( 'NONE',  #136474 ) ;
#6609 = DIRECTION ( 'NONE',  ( 0.7071067811865486830, -0.7071067811865464625, -0.000000000000000000 ) ) ;
#6610 = FACE_OUTER_BOUND ( 'NONE', #16587, .T. ) ;
#6611 = ADVANCED_FACE ( 'NONE', ( #126206 ), #82709, .F. ) ;
#6612 = CARTESIAN_POINT ( 'NONE',  ( 45.26626352523144448, 4.472830434245839371, -4.472830434245838482 ) ) ;
#6613 = EDGE_CURVE ( 'NONE', #82440, #101030, #26883, .T. ) ;
#6615 = EDGE_CURVE ( 'NONE', #51943, #113850, #15965, .T. ) ;
#6614 = VERTEX_POINT ( 'NONE', #5094 ) ;
#6616 = DIRECTION ( 'NONE',  ( -0.000000000000000000, 0.000000000000000000, 1.000000000000000000 ) ) ;
#6618 = EDGE_CURVE ( 'NONE', #55005, #127158, #137811, .T. ) ;
#6617 = FACE_OUTER_BOUND ( 'NONE', #82475, .T. ) ;
#6619 = ORIENTED_EDGE ( 'NONE', *, *, #9325, .T. ) ;
#6620 = VERTEX_POINT ( 'NONE', #50086 ) ;
#6621 = CARTESIAN_POINT ( 'NONE',  ( 34.92499999999998295, 16.81783344222320764, 7.048977539241891854 ) ) ;
#6622 = ORIENTED_EDGE ( 'NONE', *, *, #60220, .F. ) ;
#6623 = EDGE_CURVE ( 'NONE', #138876, #106778, #38486, .T. ) ;
#6624 = CARTESIAN_POINT ( 'NONE',  ( -28.49999999999980460, -19.53360074219753884, 5.000000000000000000 ) ) ;
#6625 = ORIENTED_EDGE ( 'NONE', *, *, #98170, .T. ) ;
#6626 = CARTESIAN_POINT ( 'NONE',  ( 9.489213562373095101, -27.52281430457062328, 5.000000000000000000 ) ) ;
#6627 = ADVANCED_FACE ( 'NONE', ( #72593 ), #127639, .F. ) ;
#6628 = VECTOR ( 'NONE', #90314, 1000.000000000000227 ) ;
#6629 = VECTOR ( 'NONE', #62057, 999.9999999999998863 ) ;
#6630 = AXIS2_PLACEMENT_3D ( 'NONE', #2177, #114543, #45765 ) ;
#6631 = LINE ( 'NONE', #117554, #85859 ) ;
#6632 = AXIS2_PLACEMENT_3D ( 'NONE', #113117, #13782, #25387 ) ;
#6633 = ADVANCED_FACE ( 'NONE', ( #105158 ), #19843, .T. ) ;
#6634 = FACE_BOUND ( 'NONE', #127900, .T. ) ;
#6635 = EDGE_CURVE ( 'NONE', #17037, #64792, #23450, .T. ) ;
#6636 = CARTESIAN_POINT ( 'NONE',  ( -8.816011393731004731, 28.73617430169781173, 5.000000000000000000 ) ) ;
#6637 = CARTESIAN_POINT ( 'NONE',  ( -1.499999999999980460, 10.46639925780215918, 5.000000000000000000 ) ) ;
#6638 = CARTESIAN_POINT ( 'NONE',  ( 33.32816939922329880, -9.740707523384177335, 4.000000000000000000 ) ) ;
#6639 = ORIENTED_EDGE ( 'NONE', *, *, #88874, .T. ) ;
#6640 = DIRECTION ( 'NONE',  ( 0.6830127018922180770, -0.6830127018922204085, -0.2588190451025213501 ) ) ;
#6642 = ORIENTED_EDGE ( 'NONE', *, *, #72988, .T. ) ;
#6641 = LINE ( 'NONE', #127029, #1870 ) ;
#6643 = ORIENTED_EDGE ( 'NONE', *, *, #3068, .F. ) ;
#6644 = AXIS2_PLACEMENT_3D ( 'NONE', #136167, #90540, #123174 ) ;
#6645 = VECTOR ( 'NONE', #107082, 1000.000000000000000 ) ;
#6646 = CARTESIAN_POINT ( 'NONE',  ( 60.48921356237309510, -27.52281430457097500, 5.000000000000000000 ) ) ;
#6647 = EDGE_CURVE ( 'NONE', #29058, #68553, #54680, .T. ) ;
#6648 = EDGE_LOOP ( 'NONE', ( #32639, #99634, #24726, #73212 ) ) ;
#6649 = CARTESIAN_POINT ( 'NONE',  ( 52.84959685856478728, 6.109999999999996767, 1.637169565754163836 ) ) ;
#6650 = EDGE_LOOP ( 'NONE', ( #43418, #19939, #55018, #7695 ) ) ;
#6651 = CARTESIAN_POINT ( 'NONE',  ( -34.42500000000001137, -22.22500000000000142, 5.000000000000000000 ) ) ;
#6652 = DIRECTION ( 'NONE',  ( 0.7071067811865487940, -0.7071067811865463515, 0.000000000000000000 ) ) ;
#6653 = ORIENTED_EDGE ( 'NONE', *, *, #23459, .T. ) ;
#6654 = CARTESIAN_POINT ( 'NONE',  ( 31.92500000000002203, -22.26999999999999247, -39.50000000000000000 ) ) ;
#6655 = AXIS2_PLACEMENT_3D ( 'NONE', #96417, #41345, #76139 ) ;
#6656 = AXIS2_PLACEMENT_3D ( 'NONE', #90986, #135214, #11217 ) ;
#6657 = CARTESIAN_POINT ( 'NONE',  ( 35.85416666666665719, -2.130196079827501698, -7.949999999999956657 ) ) ;
#6658 = CARTESIAN_POINT ( 'NONE',  ( 18.42327845806342879, 11.25929247661560240, 17.85071094206580256 ) ) ;
#6659 = DIRECTION ( 'NONE',  ( -0.7071067811865486830, -0.7071067811865464625, 0.000000000000000000 ) ) ;
#6660 = CARTESIAN_POINT ( 'NONE',  ( 17.99999999999987566, -12.03360074219761700, 5.000000000000000000 ) ) ;
#6661 = CARTESIAN_POINT ( 'NONE',  ( -24.18398860626899705, 28.73617430169804265, 5.000000000000000000 ) ) ;
#6662 = ORIENTED_EDGE ( 'NONE', *, *, #35406, .F. ) ;
#6663 = ADVANCED_FACE ( 'NONE', ( #78568 ), #65581, .F. ) ;
#6664 = ORIENTED_EDGE ( 'NONE', *, *, #95843, .T. ) ;
#6665 = VECTOR ( 'NONE', #18384, 1000.000000000000000 ) ;
#6666 = DIRECTION ( 'NONE',  ( 0.000000000000000000, -1.000000000000000000, 0.000000000000000000 ) ) ;
#6667 = FACE_OUTER_BOUND ( 'NONE', #57202, .T. ) ;
#6668 = EDGE_LOOP ( 'NONE', ( #70299, #40983, #25379, #68741 ) ) ;
#6669 =( GEOMETRIC_REPRESENTATION_CONTEXT ( 3 ) GLOBAL_UNCERTAINTY_ASSIGNED_CONTEXT ( ( #1228 ) ) GLOBAL_UNIT_ASSIGNED_CONTEXT ( ( #8180, #51740, #52420 ) ) REPRESENTATION_CONTEXT ( 'NONE', 'WORKASPACE' ) );
#6670 = ORIENTED_EDGE ( 'NONE', *, *, #32522, .T. ) ;
#6671 = AXIS2_PLACEMENT_3D ( 'NONE', #142632, #32447, #86113 ) ;
#6672 = ORIENTED_EDGE ( 'NONE', *, *, #41107, .T. ) ;
#6673 = PLANE ( 'NONE',  #46714 ) ;
#6674 = CARTESIAN_POINT ( 'NONE',  ( 54.32919371712956291, -3.975000000000001865, 6.884901960086284411 ) ) ;
#6675 = DIRECTION ( 'NONE',  ( 0.7071067811865487940, 0.7071067811865463515, 0.000000000000000000 ) ) ;
#6676 = VERTEX_POINT ( 'NONE', #10422 ) ;
#6677 = VECTOR ( 'NONE', #50493, 1000.000000000000000 ) ;
#6678 = DIRECTION ( 'NONE',  ( -0.6830127018922181881, 0.6830127018922202975, -0.2588190451025214056 ) ) ;
#6679 = VECTOR ( 'NONE', #117401, 999.9999999999998863 ) ;
#6680 = EDGE_CURVE ( 'NONE', #115089, #82492, #122034, .T. ) ;
#6681 = CARTESIAN_POINT ( 'NONE',  ( -4.828169399223497749, -17.24070752338410273, 4.000000000000000000 ) ) ;
#6682 = CARTESIAN_POINT ( 'NONE',  ( 11.44206980810188767, 7.934999999999993392, 2.126176841940951689 ) ) ;
#6683 = CARTESIAN_POINT ( 'NONE',  ( -23.99999999999982947, -4.447814304570784749, 5.000000000000000000 ) ) ;
#6684 = ORIENTED_EDGE ( 'NONE', *, *, #97463, .F. ) ;
#6685 = CARTESIAN_POINT ( 'NONE',  ( 22.19018167574434486, -18.74070752338409207, 7.910009926591455631 ) ) ;
#6687 = EDGE_CURVE ( 'NONE', #87956, #115779, #11116, .T. ) ;
#6686 = CARTESIAN_POINT ( 'NONE',  ( 23.20666063542136115, 21.75929247661548871, 4.998822639870701856 ) ) ;
#6688 = DIRECTION ( 'NONE',  ( -0.000000000000000000, 0.000000000000000000, 1.000000000000000000 ) ) ;
#6689 = VECTOR ( 'NONE', #64456, 1000.000000000000000 ) ;
#6691 = ORIENTED_EDGE ( 'NONE', *, *, #92956, .T. ) ;
#6690 = LINE ( 'NONE', #60441, #26366 ) ;
#6692 = DIRECTION ( 'NONE',  ( -0.000000000000000000, 0.000000000000000000, 1.000000000000000000 ) ) ;
#6693 = ORIENTED_EDGE ( 'NONE', *, *, #8978, .T. ) ;
#6694 = DIRECTION ( 'NONE',  ( -0.000000000000000000, 0.000000000000000000, 1.000000000000000000 ) ) ;
#6695 = FACE_OUTER_BOUND ( 'NONE', #75409, .T. ) ;
#6696 = CARTESIAN_POINT ( 'NONE',  ( -27.18398860626900060, 28.73617430169806042, 5.000000000000000000 ) ) ;
#6697 = ORIENTED_EDGE ( 'NONE', *, *, #132137, .T. ) ;
#6698 = EDGE_CURVE ( 'NONE', #97116, #36198, #45255, .T. ) ;
#6699 = DIRECTION ( 'NONE',  ( -0.7071067811865486830, -0.7071067811865464625, 0.000000000000000000 ) ) ;
#6700 = DIRECTION ( 'NONE',  ( 0.3543493200069162685, -0.000000000000000000, -0.9351131265310288487 ) ) ;
#6701 = DIRECTION ( 'NONE',  ( -0.000000000000000000, 0.3543493200069153248, 0.9351131265310292928 ) ) ;
#6702 = EDGE_LOOP ( 'NONE', ( #74959, #86419, #30724, #30274 ) ) ;
#6703 = DIRECTION ( 'NONE',  ( 1.000000000000000000, 0.000000000000000000, 0.000000000000000000 ) ) ;
#6704 = DIRECTION ( 'NONE',  ( 0.6830127018922181881, 0.6830127018922202975, -0.2588190451025214056 ) ) ;
#6705 = PLANE ( 'NONE',  #139568 ) ;
#6706 = CARTESIAN_POINT ( 'NONE',  ( -26.81601139373100651, 28.73617430169768738, 5.000000000000000000 ) ) ;
#6707 = DIRECTION ( 'NONE',  ( 0.6830127018922181881, 0.6830127018922202975, -0.2588190451025214056 ) ) ;
#6709 = EDGE_CURVE ( 'NONE', #81442, #7890, #5950, .T. ) ;
#6708 = EDGE_LOOP ( 'NONE', ( #64672, #10605, #105317, #142378 ) ) ;
#6710 = ORIENTED_EDGE ( 'NONE', *, *, #32929, .T. ) ;
#6711 = CARTESIAN_POINT ( 'NONE',  ( 27.18398860626900060, 28.73617430169806042, 5.000000000000000000 ) ) ;
#6712 = CARTESIAN_POINT ( 'NONE',  ( 14.74000000000000021, 9.521314400968980422E-16, 0.000000000000000000 ) ) ;
#6713 = CARTESIAN_POINT ( 'NONE',  ( 10.62456980810188689, -6.871911579029512218, 3.967499999999996252 ) ) ;
#6714 = CARTESIAN_POINT ( 'NONE',  ( -54.48921356237310221, -27.52281430457093236, 5.000000000000000000 ) ) ;
#6715 = CARTESIAN_POINT ( 'NONE',  ( -33.70710678118630454, 11.25929247661560417, 5.000000000000000000 ) ) ;
#6716 = PLANE ( 'NONE',  #12024 ) ;
#6717 = ORIENTED_EDGE ( 'NONE', *, *, #83126, .F. ) ;
#6718 = LINE ( 'NONE', #139468, #74310 ) ;
#6719 = LINE ( 'NONE', #136033, #132296 ) ;
#6720 = DIRECTION ( 'NONE',  ( 0.7071067811865487940, 0.7071067811865463515, -0.000000000000000000 ) ) ;
#6721 = DIRECTION ( 'NONE',  ( 1.000000000000000000, 0.000000000000000000, 0.000000000000000000 ) ) ;
#6722 = CARTESIAN_POINT ( 'NONE',  ( 47.89126352523143737, -4.472830434245839371, -4.472830434245839371 ) ) ;
#6723 = DIRECTION ( 'NONE',  ( 0.6830127018922180770, -0.6830127018922204085, -0.2588190451025213501 ) ) ;
#6724 = ORIENTED_EDGE ( 'NONE', *, *, #119414, .T. ) ;
#6725 = LINE ( 'NONE', #20486, #99640 ) ;
#6726 = ADVANCED_FACE ( 'NONE', ( #121334 ), #12570, .F. ) ;
#6727 = ORIENTED_EDGE ( 'NONE', *, *, #135802, .F. ) ;
#6728 = EDGE_CURVE ( 'NONE', #91342, #126947, #111153, .T. ) ;
#6729 = ORIENTED_EDGE ( 'NONE', *, *, #89457, .T. ) ;
#6730 = CARTESIAN_POINT ( 'NONE',  ( -27.29974487139158512, -27.71228299555225405, 4.000000000000000000 ) ) ;
#6731 =( GEOMETRIC_REPRESENTATION_CONTEXT ( 3 ) GLOBAL_UNCERTAINTY_ASSIGNED_CONTEXT ( ( #30139 ) ) GLOBAL_UNIT_ASSIGNED_CONTEXT ( ( #121693, #97057, #63788 ) ) REPRESENTATION_CONTEXT ( 'NONE', 'WORKASPACE' ) );
#6732 = AXIS2_PLACEMENT_3D ( 'NONE', #80531, #79848, #124023 ) ;
#6733 = VECTOR ( 'NONE', #138068, 1000.000000000000000 ) ;
#6734 = CARTESIAN_POINT ( 'NONE',  ( 0.3281693992235254487, -15.74070752338412760, 4.000000000000000000 ) ) ;
#6735 = CARTESIAN_POINT ( 'NONE',  ( -38.38161509397980353, -2.240707523384260824, 13.37739548510248255 ) ) ;
#6736 = VECTOR ( 'NONE', #116530, 1000.000000000000000 ) ;
#6737 = CARTESIAN_POINT ( 'NONE',  ( 2.999999999999988898, -13.44781430457069682, 5.000000000000000000 ) ) ;
#6738 = EDGE_CURVE ( 'NONE', #97151, #75676, #99566, .T. ) ;
#6739 = FACE_OUTER_BOUND ( 'NONE', #101837, .T. ) ;
#6740 = ORIENTED_EDGE ( 'NONE', *, *, #4687, .F. ) ;
#6741 = EDGE_CURVE ( 'NONE', #123367, #31644, #17463, .T. ) ;
#6742 = DIRECTION ( 'NONE',  ( -0.7071067811865486830, -0.7071067811865464625, -0.000000000000000000 ) ) ;
#6743 = DIRECTION ( 'NONE',  ( -0.3543493200069162685, -0.000000000000000000, -0.9351131265310288487 ) ) ;
#6744 = DIRECTION ( 'NONE',  ( -0.3543493200069162685, -0.000000000000000000, -0.9351131265310288487 ) ) ;
#6745 = AXIS2_PLACEMENT_3D ( 'NONE', #56016, #80608, #124806 ) ;
#6746 = SURFACE_STYLE_FILL_AREA ( #106073 ) ;
#6747 = CARTESIAN_POINT ( 'NONE',  ( 14.99451991528749595, 28.92564299267948513, 4.000000000000000000 ) ) ;
#6748 = LINE ( 'NONE', #51029, #27258 ) ;
#6749 = CARTESIAN_POINT ( 'NONE',  ( 61.32919371712955581, -3.975000000000001865, 6.884901960086284411 ) ) ;
#6750 = CARTESIAN_POINT ( 'NONE',  ( 0.000000000000000000, 0.000000000000000000, 5.000000000000000000 ) ) ;
#6751 = ORIENTED_EDGE ( 'NONE', *, *, #96871, .F. ) ;
#6752 = ORIENTED_EDGE ( 'NONE', *, *, #29268, .T. ) ;
#6753 = CARTESIAN_POINT ( 'NONE',  ( 54.37499999999999289, 7.950000000000000178, 1.460391307983218535E-15 ) ) ;
#6754 = CARTESIAN_POINT ( 'NONE',  ( -68.99451991528748351, 28.92564299267986172, 4.000000000000000000 ) ) ;
#6755 = LINE ( 'NONE', #83691, #83317 ) ;
#6756 = AXIS2_PLACEMENT_3D ( 'NONE', #69386, #4045, #26578 ) ;
#6757 = VECTOR ( 'NONE', #66321, 1000.000000000000000 ) ;
#6758 = PRESENTATION_STYLE_ASSIGNMENT (( #63376 ) ) ;
#6759 = ORIENTED_EDGE ( 'NONE', *, *, #117336, .T. ) ;
#6760 = EDGE_CURVE ( 'NONE', #61260, #85411, #6823, .T. ) ;
#6761 =( BOUNDED_CURVE ( )  B_SPLINE_CURVE ( 3, ( #23227, #79106, #77658, #64619 ),
 .UNSPECIFIED., .F., .F. ) 
 B_SPLINE_CURVE_WITH_KNOTS ( ( 4, 4 ),
 ( 1.964434688349486979, 3.503810798801452187 ),
 .UNSPECIFIED. ) 
 CURVE ( )  GEOMETRIC_REPRESENTATION_ITEM ( )  RATIONAL_B_SPLINE_CURVE ( ( 1.000000000000000000, 0.8120851936182278408, 0.8120851936182278408, 1.000000000000000000 ) ) 
 REPRESENTATION_ITEM ( '' )  );
#6762 = LINE ( 'NONE', #95239, #58373 ) ;
#6763 = AXIS2_PLACEMENT_3D ( 'NONE', #6750, #16973, #94507 ) ;
#6764 = CARTESIAN_POINT ( 'NONE',  ( 53.95876352523143282, 0.000000000000000000, -6.110000000000001208 ) ) ;
#6765 = VERTEX_POINT ( 'NONE', #31489 ) ;
#6766 = LINE ( 'NONE', #106826, #126530 ) ;
#6767 = ORIENTED_EDGE ( 'NONE', *, *, #58442, .T. ) ;
#6768 = EDGE_LOOP ( 'NONE', ( #133406, #49375, #138591, #88145 ) ) ;
#6769 = DIRECTION ( 'NONE',  ( -0.6830127018922181881, 0.6830127018922202975, -0.2588190451025214056 ) ) ;
#6770 = AXIS2_PLACEMENT_3D ( 'NONE', #82820, #103124, #139358 ) ;
#6771 = AXIS2_PLACEMENT_3D ( 'NONE', #84893, #28387, #8022 ) ;
#6772 = DIRECTION ( 'NONE',  ( -0.000000000000000000, -0.3543493200069152693, 0.9351131265310292928 ) ) ;
#6773 = DIRECTION ( 'NONE',  ( 0.7071067811865486830, -0.7071067811865464625, -0.000000000000000000 ) ) ;
#6774 = VECTOR ( 'NONE', #126244, 1000.000000000000000 ) ;
#6775 = LINE ( 'NONE', #61265, #88050 ) ;
#6776 = CARTESIAN_POINT ( 'NONE',  ( 44.99451991528749772, 28.92564299267969474, 4.000000000000000000 ) ) ;
#6778 = ORIENTED_EDGE ( 'NONE', *, *, #65610, .T. ) ;
#6777 = DIRECTION ( 'NONE',  ( -0.000000000000000000, -0.3543493200069152693, 0.9351131265310292928 ) ) ;
#6779 = AXIS2_PLACEMENT_3D ( 'NONE', #137329, #104677, #19098 ) ;
#6780 = CARTESIAN_POINT ( 'NONE',  ( 2.000000000000000000, -2.375000000000000000, -0.000000000000000000 ) ) ;
#6781 = CARTESIAN_POINT ( 'NONE',  ( -29.20666063542132207, 21.75929247661549226, 4.998822639870711626 ) ) ;
#6782 = DIRECTION ( 'NONE',  ( 0.7071067811865487940, 0.7071067811865463515, 0.000000000000000000 ) ) ;
#6783 = VECTOR ( 'NONE', #136771, 1000.000000000000227 ) ;
#6784 = CARTESIAN_POINT ( 'NONE',  ( 23.99999999999983658, 7.552185695429090906, 5.000000000000000000 ) ) ;
#6785 = CARTESIAN_POINT ( 'NONE',  ( 16.49999999999988276, -4.216083040037233332, -7.486842126848696211 ) ) ;
#6786 = VECTOR ( 'NONE', #76288, 999.9999999999998863 ) ;
#6787 = EDGE_LOOP ( 'NONE', ( #84850, #67843, #87072, #134403 ) ) ;
#6788 = EDGE_CURVE ( 'NONE', #39740, #42277, #108283, .T. ) ;
#6789 = ORIENTED_EDGE ( 'NONE', *, *, #51613, .T. ) ;
#6790 = SURFACE_STYLE_USAGE ( .BOTH. , #41604 ) ;
#6791 = CARTESIAN_POINT ( 'NONE',  ( 74.43293019189810877, 1.637169565754156508, 6.110000000000000320 ) ) ;
#6792 = EDGE_CURVE ( 'NONE', #1646, #63895, #109020, .T. ) ;
#6793 = DIRECTION ( 'NONE',  ( -0.6830127018922180770, 0.6830127018922202975, -0.2588190451025213501 ) ) ;
#6794 = LINE ( 'NONE', #135927, #27118 ) ;
#6795 = CARTESIAN_POINT ( 'NONE',  ( 29.28242261357413057, -21.73023691814492864, 5.000000000000000888 ) ) ;
#6796 = FACE_OUTER_BOUND ( 'NONE', #143496, .T. ) ;
#6797 = EDGE_LOOP ( 'NONE', ( #15955, #70142, #26620, #15043 ) ) ;
#6798 = ORIENTED_EDGE ( 'NONE', *, *, #18450, .T. ) ;
#6799 = VECTOR ( 'NONE', #44639, 1000.000000000000000 ) ;
#6800 = CARTESIAN_POINT ( 'NONE',  ( 30.72281430457039875, -21.72499999999999432, 5.000000000000000000 ) ) ;
#6801 = SURFACE_SIDE_STYLE ('',( #72151 ) ) ;
#6802 = ORIENTED_EDGE ( 'NONE', *, *, #57956, .F. ) ;
#6803 = EDGE_CURVE ( 'NONE', #111332, #9354, #95010, .T. ) ;
#6804 = ADVANCED_FACE ( 'NONE', ( #19875 ), #40248, .F. ) ;
#6805 = ORIENTED_EDGE ( 'NONE', *, *, #51882, .T. ) ;
#6806 = LINE ( 'NONE', #50368, #139402 ) ;
#6807 = ORIENTED_EDGE ( 'NONE', *, *, #125783, .F. ) ;
#6808 = CARTESIAN_POINT ( 'NONE',  ( 62.20419371712955581, -6.884901960086285300, -3.975000000000000089 ) ) ;
#6809 = ADVANCED_FACE ( 'NONE', ( #86596 ), #119881, .T. ) ;
#6810 = FACE_BOUND ( 'NONE', #33951, .T. ) ;
#6811 = EDGE_CURVE ( 'NONE', #18156, #68806, #76431, .T. ) ;
#6812 = PLANE ( 'NONE',  #80382 ) ;
#6813 = PLANE ( 'NONE',  #11928 ) ;
#6814 = CARTESIAN_POINT ( 'NONE',  ( 17.07999999999999829, 9.521314400968980422E-16, 0.000000000000000000 ) ) ;
#6816 = VERTEX_POINT ( 'NONE', #7564 ) ;
#6815 = CARTESIAN_POINT ( 'NONE',  ( 44.99451991528749772, 28.92564299267969474, 4.000000000000000000 ) ) ;
#6817 = CARTESIAN_POINT ( 'NONE',  ( -3.489213562373097322, -27.52281430457057709, 5.000000000000000000 ) ) ;
#6818 = ADVANCED_FACE ( 'NONE', ( #107605 ), #51826, .F. ) ;
#6819 = VERTEX_POINT ( 'NONE', #83220 ) ;
#6820 = EDGE_LOOP ( 'NONE', ( #50785, #100314, #95659, #64139, #78496 ) ) ;
#6821 = CARTESIAN_POINT ( 'NONE',  ( 92.51626352523145158, -4.472830434245838482, 4.472830434245838482 ) ) ;
#6822 = EDGE_LOOP ( 'NONE', ( #17724, #122473, #53304, #36701 ) ) ;
#6823 = LINE ( 'NONE', #128654, #98499 ) ;
#6824 = CARTESIAN_POINT ( 'NONE',  ( -27.18398860626900060, 28.73617430169806042, 5.000000000000000000 ) ) ;
#6825 = CARTESIAN_POINT ( 'NONE',  ( 0.000000000000000000, 9.735942053221458872E-16, -7.950000000000000178 ) ) ;
#6826 = EDGE_CURVE ( 'NONE', #134910, #28590, #44875, .T. ) ;
#6827 = DIRECTION ( 'NONE',  ( 0.7071067811865487940, 0.7071067811865463515, 0.000000000000000000 ) ) ;
#6828 = CARTESIAN_POINT ( 'NONE',  ( 12.69999999999999574, -60.26999999999998892, -39.50000000000000000 ) ) ;
#6829 = ORIENTED_EDGE ( 'NONE', *, *, #68226, .T. ) ;
#6830 = DIRECTION ( 'NONE',  ( -0.7071067811865486830, -0.7071067811865464625, 0.000000000000000000 ) ) ;
#6831 = CARTESIAN_POINT ( 'NONE',  ( 22.49999999999984723, 8.319652575858409449, -8.582050562765775936 ) ) ;
#6832 = CARTESIAN_POINT ( 'NONE',  ( -6.758600742197917732, 21.72500000000000142, 5.000000000000000000 ) ) ;
#6833 = DIRECTION ( 'NONE',  ( 0.000000000000000000, 0.000000000000000000, 1.000000000000000000 ) ) ;
#6834 = CARTESIAN_POINT ( 'NONE',  ( 2.999999999999999112, -5.520864266206504263E-14, 0.000000000000000000 ) ) ;
#6835 = CARTESIAN_POINT ( 'NONE',  ( 31.49999999999977973, 1.030536316426536203, -5.498701923753874787 ) ) ;
#6836 = EDGE_CURVE ( 'NONE', #134440, #41017, #40448, .T. ) ;
#6837 = AXIS2_PLACEMENT_3D ( 'NONE', #108678, #17419, #94966 ) ;
#6838 = AXIS2_PLACEMENT_3D ( 'NONE', #22591, #66861, #111031 ) ;
#6839 = CARTESIAN_POINT ( 'NONE',  ( -10.17183060077640100, 9.759292476615614831, 4.000000000000000000 ) ) ;
#6840 = VECTOR ( 'NONE', #129676, 1000.000000000000000 ) ;
#6841 = ORIENTED_EDGE ( 'NONE', *, *, #27016, .F. ) ;
#6842 = DIRECTION ( 'NONE',  ( -0.7071067811865487940, 0.7071067811865463515, -0.000000000000000000 ) ) ;
#6843 = CARTESIAN_POINT ( 'NONE',  ( -11.99999999999991296, 17.58746187583907172, 4.000000000000000000 ) ) ;
#6844 = AXIS2_PLACEMENT_3D ( 'NONE', #118490, #19190, #83029 ) ;
#6845 = ORIENTED_EDGE ( 'NONE', *, *, #35653, .F. ) ;
#6846 = ORIENTED_EDGE ( 'NONE', *, *, #141064, .T. ) ;
#6847 = VERTEX_POINT ( 'NONE', #49182 ) ;
#6848 = ADVANCED_FACE ( 'NONE', ( #71638 ), #139029, .T. ) ;
#6849 = CARTESIAN_POINT ( 'NONE',  ( 46.66709685856476852, -3.055000000000000160, -5.291415217122921177 ) ) ;
#6850 = EDGE_CURVE ( 'NONE', #68379, #5793, #107094, .T. ) ;
#6851 = VERTEX_POINT ( 'NONE', #28122 ) ;
#6852 = MECHANICAL_DESIGN_GEOMETRIC_PRESENTATION_REPRESENTATION (  '', ( #134096 ), #141099 ) ;
#6853 = ADVANCED_FACE ( 'NONE', ( #138312 ), #70934, .F. ) ;
#6854 = VECTOR ( 'NONE', #22586, 1000.000000000000000 ) ;
#6855 = CARTESIAN_POINT ( 'NONE',  ( 16.23330628287043353, -6.094999999999989981, -1.633150327867689100 ) ) ;
#6856 = CARTESIAN_POINT ( 'NONE',  ( -16.03282571951856283, 6.618735317068870749, -28.66949109531741158 ) ) ;
#6857 = ORIENTED_EDGE ( 'NONE', *, *, #48779, .T. ) ;
#6858 = DIRECTION ( 'NONE',  ( 1.000000000000000000, 0.000000000000000000, 0.000000000000000000 ) ) ;
#6859 = ORIENTED_EDGE ( 'NONE', *, *, #134161, .T. ) ;
#6860 = DIRECTION ( 'NONE',  ( 0.7071067811865486830, -0.7071067811865464625, -0.000000000000000000 ) ) ;
#6861 = CIRCLE ( 'NONE', #87938, 3.000000000000000000 ) ;
#6862 = VECTOR ( 'NONE', #30608, 1000.000000000000000 ) ;
#6863 = LINE ( 'NONE', #27948, #63752 ) ;
#6865 = ORIENTED_EDGE ( 'NONE', *, *, #83552, .F. ) ;
#6864 = DIRECTION ( 'NONE',  ( 0.3543493200069162685, -0.000000000000000000, -0.9351131265310288487 ) ) ;
#6866 = EDGE_LOOP ( 'NONE', ( #47517, #22984, #11957, #58195 ) ) ;
#6867 = PLANE ( 'NONE',  #134914 ) ;
#6868 = ORIENTED_EDGE ( 'NONE', *, *, #27303, .T. ) ;
#6869 = AXIS2_PLACEMENT_3D ( 'NONE', #79624, #89720, #111470 ) ;
#6870 = CARTESIAN_POINT ( 'NONE',  ( -47.99451991528749062, 28.92564299267971251, 4.000000000000000000 ) ) ;
#6871 = ORIENTED_EDGE ( 'NONE', *, *, #141831, .F. ) ;
#6872 = ORIENTED_EDGE ( 'NONE', *, *, #31646, .F. ) ;
#6873 = ORIENTED_EDGE ( 'NONE', *, *, #90651, .T. ) ;
#6874 = ORIENTED_EDGE ( 'NONE', *, *, #63655, .F. ) ;
#6875 = CARTESIAN_POINT ( 'NONE',  ( 31.82816939922331656, -17.24070752338409918, 4.000000000000000000 ) ) ;
#6876 = AXIS2_PLACEMENT_3D ( 'NONE', #30913, #142528, #107723 ) ;
#6877 = AXIS2_PLACEMENT_3D ( 'NONE', #99312, #63878, #140689 ) ;
#6878 = LINE ( 'NONE', #50443, #16737 ) ;
#6879 = CARTESIAN_POINT ( 'NONE',  ( 11.99451991528749417, 28.92564299267946382, 4.000000000000000000 ) ) ;
#6880 = CARTESIAN_POINT ( 'NONE',  ( -13.17183060077637968, -5.240707523384225297, 4.000000000000000000 ) ) ;
#6881 = EDGE_LOOP ( 'NONE', ( #121944, #11650, #31354, #87855, #10531 ) ) ;
#6882 = AXIS2_PLACEMENT_3D ( 'NONE', #126182, #115989, #71823 ) ;
#6883 = CARTESIAN_POINT ( 'NONE',  ( -24.00548008471250938, 28.92564299267921513, 4.000000000000000000 ) ) ;
#6884 = VERTEX_POINT ( 'NONE', #93375 ) ;
#6885 = AXIS2_PLACEMENT_3D ( 'NONE', #112716, #135218, #134486 ) ;
#6886 = CARTESIAN_POINT ( 'NONE',  ( -1.499999999999984013, -20.94781430457061333, 5.000000000000000000 ) ) ;
#6887 = CARTESIAN_POINT ( 'NONE',  ( -28.49999999999980460, -5.568876922607759461, 4.000000000000000000 ) ) ;
#6888 = DIRECTION ( 'NONE',  ( 0.6830127018922181881, 0.6830127018922202975, -0.2588190451025214056 ) ) ;
#6889 = ORIENTED_EDGE ( 'NONE', *, *, #95363, .T. ) ;
#6890 = CARTESIAN_POINT ( 'NONE',  ( -48.18398860626899705, 28.73617430169820608, 5.000000000000000000 ) ) ;
#6891 = FACE_OUTER_BOUND ( 'NONE', #66405, .T. ) ;
#6892 = ORIENTED_EDGE ( 'NONE', *, *, #108414, .T. ) ;
#6893 = EDGE_LOOP ( 'NONE', ( #142897, #113266, #101994, #109541 ) ) ;
#6894 = ORIENTED_EDGE ( 'NONE', *, *, #65304, .F. ) ;
#6895 = FACE_OUTER_BOUND ( 'NONE', #19454, .T. ) ;
#6896 = CARTESIAN_POINT ( 'NONE',  ( -13.84116387061258457, 6.089959206779446355, 4.000000000000000000 ) ) ;
#6897 = AXIS2_PLACEMENT_3D ( 'NONE', #115506, #126414, #27105 ) ;
#6898 = CARTESIAN_POINT ( 'NONE',  ( -12.18398860626900060, 28.73617430169795739, 5.000000000000000000 ) ) ;
#6899 = CARTESIAN_POINT ( 'NONE',  ( -25.39999999999996305, 0.000000000000000000, 2.500000000000000000 ) ) ;
#6900 = CARTESIAN_POINT ( 'NONE',  ( 74.43293019189810877, 1.637169565754156730, 6.110000000000001208 ) ) ;
#6901 = LINE ( 'NONE', #50466, #71834 ) ;
#6902 = CARTESIAN_POINT ( 'NONE',  ( 2.999999999999985345, -4.447814304570786526, 5.000000000000000000 ) ) ;
#6903 = PLANE ( 'NONE',  #14058 ) ;
#6904 = CARTESIAN_POINT ( 'NONE',  ( -1.499999999999977129, 13.08746187583910725, 4.000000000000000000 ) ) ;
#6905 = DIRECTION ( 'NONE',  ( 0.3543493200069162685, -0.000000000000000000, -0.9351131265310288487 ) ) ;
#6906 = ORIENTED_EDGE ( 'NONE', *, *, #96993, .F. ) ;
#6907 = VECTOR ( 'NONE', #56874, 1000.000000000000000 ) ;
#6908 = CARTESIAN_POINT ( 'NONE',  ( 17.54601624070869548, -3.246904730846185583, -35.78195362552649783 ) ) ;
#6909 = VERTEX_POINT ( 'NONE', #6304 ) ;
#6910 = DIRECTION ( 'NONE',  ( -0.6830127018922180770, -0.6830127018922204085, -0.2588190451025213501 ) ) ;
#6912 = ORIENTED_EDGE ( 'NONE', *, *, #121789, .T. ) ;
#6911 = DIRECTION ( 'NONE',  ( -1.000000000000000000, -1.224606353822377258E-16, -0.000000000000000000 ) ) ;
#6913 = EDGE_CURVE ( 'NONE', #69972, #30925, #94074, .T. ) ;
#6914 = LINE ( 'NONE', #5509, #16241 ) ;
#6915 = CARTESIAN_POINT ( 'NONE',  ( 27.29974487139158512, -27.71228299555225405, 4.000000000000000000 ) ) ;
#6916 = ORIENTED_EDGE ( 'NONE', *, *, #110836, .F. ) ;
#6917 = EDGE_CURVE ( 'NONE', #82553, #40629, #91577, .T. ) ;
#6918 = ORIENTED_EDGE ( 'NONE', *, *, #99925, .T. ) ;
#6919 = CARTESIAN_POINT ( 'NONE',  ( 34.92499999999998295, -21.72500000000000142, 5.000000000000000000 ) ) ;
#6920 = CARTESIAN_POINT ( 'NONE',  ( -11.95341186370447950, 14.25929247661557753, 18.84478104361330963 ) ) ;
#6921 = VECTOR ( 'NONE', #67987, 1000.000000000000000 ) ;
#6922 = AXIS2_PLACEMENT_3D ( 'NONE', #59554, #94286, #137090 ) ;
#6923 = CARTESIAN_POINT ( 'NONE',  ( 32.99999999999976552, 5.966399257802198264, 5.000000000000000000 ) ) ;
#6924 = CARTESIAN_POINT ( 'NONE',  ( 94.72502705046289861, 5.819803920172573086, -5.819803920172572198 ) ) ;
#6925 = CARTESIAN_POINT ( 'NONE',  ( 6.278254515685692816, 8.259292476615637923, 11.78515199841151784 ) ) ;
#6926 = ORIENTED_EDGE ( 'NONE', *, *, #46304, .F. ) ;
#6927 = EDGE_CURVE ( 'NONE', #2946, #9514, #139535, .T. ) ;
#6928 = PLANE ( 'NONE',  #70113 ) ;
#6929 = CARTESIAN_POINT ( 'NONE',  ( 21.59770000000000323, 3.130000000000007887, -22.35000000000000142 ) ) ;
#6930 = CARTESIAN_POINT ( 'NONE',  ( 34.41666666666667140, 5.278424836066147208, 3.047499999999990550 ) ) ;
#6931 = CYLINDRICAL_SURFACE ( 'NONE', #14364, 7.950000000000000178 ) ;
#6932 = ORIENTED_EDGE ( 'NONE', *, *, #33885, .F. ) ;
#6933 = ADVANCED_FACE ( 'NONE', ( #16503 ), #72387, .F. ) ;
#6934 = LINE ( 'NONE', #115698, #28310 ) ;
#6935 = ORIENTED_EDGE ( 'NONE', *, *, #62584, .F. ) ;
#6936 = CIRCLE ( 'NONE', #88013, 4.607329295533711289 ) ;
#6937 = CARTESIAN_POINT ( 'NONE',  ( 80.64626352523141861, -4.472830434245840259, 4.472830434245839371 ) ) ;
#6938 = DIRECTION ( 'NONE',  ( -0.6830127018922180770, -0.6830127018922204085, -0.2588190451025213501 ) ) ;
#6939 = VECTOR ( 'NONE', #112574, 1000.000000000000000 ) ;
#6940 = LINE ( 'NONE', #30161, #2931 ) ;
#6941 = FACE_OUTER_BOUND ( 'NONE', #140067, .T. ) ;
#6942 = ORIENTED_EDGE ( 'NONE', *, *, #54087, .T. ) ;
#6943 = ADVANCED_FACE ( 'NONE', ( #128848 ), #17913, .F. ) ;
#6944 = AXIS2_PLACEMENT_3D ( 'NONE', #38508, #14609, #2264 ) ;
#6945 = CONICAL_SURFACE ( 'NONE', #34855, 2.500000000000000444, 0.9599310885968830309 ) ;
#6946 = PLANE ( 'NONE',  #14125 ) ;
#6947 = CARTESIAN_POINT ( 'NONE',  ( 13.49999999999991118, 7.466399257802187606, 5.000000000000000000 ) ) ;
#6949 = VERTEX_POINT ( 'NONE', #105648 ) ;
#6948 = DIRECTION ( 'NONE',  ( 0.000000000000000000, -0.000000000000000000, 1.000000000000000000 ) ) ;
#6950 = CARTESIAN_POINT ( 'NONE',  ( 17.22560490425083657, 3.821174125832445049E-16, 0.000000000000000000 ) ) ;
#6951 = CARTESIAN_POINT ( 'NONE',  ( -23.67183060077630330, -9.740707523384187994, 4.000000000000000000 ) ) ;
#6952 = CARTESIAN_POINT ( 'NONE',  ( 1.573529187797693574, -2.874494765961987497, 5.856845438429902018 ) ) ;
#6953 = VECTOR ( 'NONE', #73667, 999.9999999999998863 ) ;
#6954 =( BOUNDED_CURVE ( )  B_SPLINE_CURVE ( 2, ( #5496, #60666, #15632, #125891, #26563, #72260, #49773, #93953, #70806, #38868, #7644, #63512, #8337 ),
 .UNSPECIFIED., .F., .T. ) 
 B_SPLINE_CURVE_WITH_KNOTS ( ( 3, 2, 2, 2, 2, 2, 3 ),
 ( 0.5166666666666667185, 0.5194444444444444864, 0.5222222222222222543, 0.5250000000000000222, 0.5277777777777777901, 0.5305555555555555580, 0.5333333333333333259 ),
 .UNSPECIFIED. ) 
 CURVE ( )  GEOMETRIC_REPRESENTATION_ITEM ( )  RATIONAL_B_SPLINE_CURVE ( ( 1.000000000000000000, 0.9659258262890683122, 1.000000000000000000, 0.9659258262890683122, 1.000000000000000000, 0.9659258262890683122, 1.000000000000000000, 0.9659258262890683122, 1.000000000000000000, 0.9659258262890683122, 1.000000000000000000, 0.9659258262890683122, 1.000000000000000000 ) ) 
 REPRESENTATION_ITEM ( '' )  );
#6955 = FACE_OUTER_BOUND ( 'NONE', #44327, .T. ) ;
#6956 = ORIENTED_EDGE ( 'NONE', *, *, #11537, .F. ) ;
#6957 = ORIENTED_EDGE ( 'NONE', *, *, #116488, .F. ) ;
#6958 = CARTESIAN_POINT ( 'NONE',  ( 71.75043019189811844, 3.055000000000002824, -5.291415217122919401 ) ) ;
#6959 = ORIENTED_EDGE ( 'NONE', *, *, #129952, .T. ) ;
#6960 = EDGE_CURVE ( 'NONE', #23280, #76403, #60793, .T. ) ;
#6961 = CARTESIAN_POINT ( 'NONE',  ( 24.61500991739762512, 5.335133370053847912, 4.556819239218476980 ) ) ;
#6962 = DIRECTION ( 'NONE',  ( 0.7071067811865486830, -0.7071067811865464625, -0.000000000000000000 ) ) ;
#6963 = ORIENTED_EDGE ( 'NONE', *, *, #108799, .T. ) ;
#6964 = LINE ( 'NONE', #38231, #23597 ) ;
#6965 = CARTESIAN_POINT ( 'NONE',  ( -34.92500000000001137, 4.701930566820959001, 4.500000000000000888 ) ) ;
#6966 = EDGE_CURVE ( 'NONE', #126576, #120537, #90574, .T. ) ;
#6967 = EDGE_CURVE ( 'NONE', #19931, #42357, #58876, .T. ) ;
#6968 = VECTOR ( 'NONE', #11977, 1000.000000000000000 ) ;
#6969 = ORIENTED_EDGE ( 'NONE', *, *, #108372, .T. ) ;
#6970 = VECTOR ( 'NONE', #133661, 1000.000000000000000 ) ;
#6971 = LINE ( 'NONE', #52660, #51317 ) ;
#6972 = AXIS2_PLACEMENT_3D ( 'NONE', #72983, #127310, #72280 ) ;
#6973 = CARTESIAN_POINT ( 'NONE',  ( 34.49586038379622011, -3.974999999999998312, -6.884901960086286188 ) ) ;
#6974 = CARTESIAN_POINT ( 'NONE',  ( -15.69326993309589824, -3.740707523384244837, 12.88036043432871303 ) ) ;
#6976 = EDGE_CURVE ( 'NONE', #34897, #123482, #90752, .T. ) ;
#6975 = CIRCLE ( 'NONE', #6877, 2.500000000000000444 ) ;
#6977 = VERTEX_POINT ( 'NONE', #134982 ) ;
#6978 = VERTEX_POINT ( 'NONE', #33526 ) ;
#6979 = EDGE_CURVE ( 'NONE', #131599, #107344, #24753, .T. ) ;
#6980 = AXIS2_PLACEMENT_3D ( 'NONE', #51173, #74358, #118547 ) ;
#6981 = EDGE_CURVE ( 'NONE', #35420, #42357, #10618, .T. ) ;
#6982 = DIRECTION ( 'NONE',  ( -0.5735764363510507113, 0.8191520442889885789, 1.003171929053520926E-16 ) ) ;
#6983 = CARTESIAN_POINT ( 'NONE',  ( 8.816011393731004731, 28.73617430169781173, 5.000000000000000000 ) ) ;
#6984 = LINE ( 'NONE', #51268, #115916 ) ;
#6985 = LINE ( 'NONE', #19166, #10845 ) ;
#6986 = CARTESIAN_POINT ( 'NONE',  ( -29.29289321881325137, 11.25929247661560773, 5.000000000000000000 ) ) ;
#6987 = CARTESIAN_POINT ( 'NONE',  ( -34.92500000000001137, 8.454535441273645091, -0.2181437882982119325 ) ) ;
#6988 = CARTESIAN_POINT ( 'NONE',  ( -18.00548008471250583, 28.92564299267925776, 4.000000000000000000 ) ) ;
#6989 = SHAPE_REPRESENTATION_RELATIONSHIP ( 'NONE' , 'NONE' ,  #428, #53301 ) ;
#6990 = ORIENTED_EDGE ( 'NONE', *, *, #62319, .F. ) ;
#6991 = VECTOR ( 'NONE', #135949, 1000.000000000000000 ) ;
#6992 = EDGE_LOOP ( 'NONE', ( #77970, #136678, #113297, #52716 ) ) ;
#6993 = VERTEX_POINT ( 'NONE', #25452 ) ;
#6994 = EDGE_CURVE ( 'NONE', #62992, #119600, #73181, .T. ) ;
#6995 = EDGE_LOOP ( 'NONE', ( #18463, #60264, #47235, #77607 ) ) ;
#6996 = AXIS2_PLACEMENT_3D ( 'NONE', #132727, #45014, #66720 ) ;
#6997 = ADVANCED_FACE ( 'NONE', ( #26895 ), #138522, .F. ) ;
#6998 = CARTESIAN_POINT ( 'NONE',  ( 25.39999999999999858, -5.520864266206504263E-14, 0.000000000000000000 ) ) ;
#6999 = EDGE_LOOP ( 'NONE', ( #136960, #90877, #109230, #54714 ) ) ;
#7000 = DIRECTION ( 'NONE',  ( -0.7071067811865487940, 0.7071067811865463515, -0.000000000000000000 ) ) ;
#7001 = LINE ( 'NONE', #138286, #123633 ) ;
#7002 = CARTESIAN_POINT ( 'NONE',  ( -11.99999999999991651, -21.84840872380825516, 2.849755605029579808 ) ) ;
#7003 = CARTESIAN_POINT ( 'NONE',  ( -30.48921356237309510, -27.52281430457076894, 5.000000000000000000 ) ) ;
#7004 = VECTOR ( 'NONE', #110129, 1000.000000000000000 ) ;
#7005 = FACE_OUTER_BOUND ( 'NONE', #56984, .T. ) ;
#7006 = VERTEX_POINT ( 'NONE', #50797 ) ;
#7007 = DIRECTION ( 'NONE',  ( -0.3543493200069163240, 4.681814790819596721E-17, -0.9351131265310288487 ) ) ;
#7008 = DIRECTION ( 'NONE',  ( -0.7071067811865487940, 0.7071067811865463515, 0.000000000000000000 ) ) ;
#7009 = ORIENTED_EDGE ( 'NONE', *, *, #4630, .T. ) ;
#7010 = FACE_OUTER_BOUND ( 'NONE', #56009, .T. ) ;
#7011 = ORIENTED_EDGE ( 'NONE', *, *, #14340, .F. ) ;
#7012 = CARTESIAN_POINT ( 'NONE',  ( -9.516654386410381861, 22.22500000000000142, 4.500000000000000888 ) ) ;
#7013 = ORIENTED_EDGE ( 'NONE', *, *, #14904, .T. ) ;
#7014 = CARTESIAN_POINT ( 'NONE',  ( 74.66709685856476142, -3.055000000000000160, -5.291415217122921177 ) ) ;
#7015 = EDGE_CURVE ( 'NONE', #87517, #66916, #85704, .T. ) ;
#7017 = ORIENTED_EDGE ( 'NONE', *, *, #132423, .T. ) ;
#7016 = VECTOR ( 'NONE', #87919, 1000.000000000000000 ) ;
#7018 = VECTOR ( 'NONE', #139968, 1000.000000000000227 ) ;
#7019 = EDGE_CURVE ( 'NONE', #88713, #22841, #17438, .T. ) ;
#7020 = DIRECTION ( 'NONE',  ( -0.7071067811865487940, 0.7071067811865463515, -0.000000000000000000 ) ) ;
#7021 = ADVANCED_FACE ( 'NONE', ( #137092 ), #60268, .F. ) ;
#7022 = DIRECTION ( 'NONE',  ( 0.7071067811865486830, -0.7071067811865464625, -0.000000000000000000 ) ) ;
#7023 = CARTESIAN_POINT ( 'NONE',  ( 109.6670968585647756, -3.055000000000000160, -5.291415217122921177 ) ) ;
#7024 = DIRECTION ( 'NONE',  ( -0.7071067811865486830, -0.7071067811865464625, 0.000000000000000000 ) ) ;
#7025 = DIRECTION ( 'NONE',  ( 0.7071067811865487940, -0.7071067811865463515, 0.000000000000000000 ) ) ;
#7026 = CARTESIAN_POINT ( 'NONE',  ( -33.18398860626899705, 28.73617430169810305, 5.000000000000000000 ) ) ;
#7027 = CARTESIAN_POINT ( 'NONE',  ( -14.97558742549547617, -1.187250289053312979, 4.247958624336151345 ) ) ;
#7029 = ADVANCED_FACE ( 'NONE', ( #129773 ), #42796, .F. ) ;
#7028 = VECTOR ( 'NONE', #87830, 1000.000000000000000 ) ;
#7030 = CARTESIAN_POINT ( 'NONE',  ( 19.10840764549667270, 9.139736423841732040E-16, 0.000000000000000000 ) ) ;
#7031 = FACE_BOUND ( 'NONE', #121992, .T. ) ;
#7033 = DIRECTION ( 'NONE',  ( -0.7071067811865486830, 0.7071067811865463515, 0.000000000000000000 ) ) ;
#7032 = PRESENTATION_LAYER_ASSIGNMENT (  '', '', ( #81205 ) ) ;
#7035 = ORIENTED_EDGE ( 'NONE', *, *, #22890, .F. ) ;
#7034 = VECTOR ( 'NONE', #90270, 1000.000000000000000 ) ;
#7036 = CARTESIAN_POINT ( 'NONE',  ( 16.82816939922341604, 15.75929247661555088, 4.000000000000000000 ) ) ;
#7037 = CARTESIAN_POINT ( 'NONE',  ( -9.707106781186469746, -9.740707523384184441, 5.000000000000000000 ) ) ;
#7038 = ORIENTED_EDGE ( 'NONE', *, *, #30062, .F. ) ;
#7039 = EDGE_LOOP ( 'NONE', ( #33735, #30643, #65578, #33320 ) ) ;
#7040 = CARTESIAN_POINT ( 'NONE',  ( 62.99451991528749772, 28.92564299267982264, 4.000000000000000000 ) ) ;
#7041 = AXIS2_PLACEMENT_3D ( 'NONE', #121586, #143345, #53497 ) ;
#7042 = ORIENTED_EDGE ( 'NONE', *, *, #102614, .T. ) ;
#7043 = VECTOR ( 'NONE', #72254, 1000.000000000000000 ) ;
#7044 = CIRCLE ( 'NONE', #88135, 5.999999999999998224 ) ;
#7045 = VECTOR ( 'NONE', #39559, 999.9999999999998863 ) ;
#7046 = DIRECTION ( 'NONE',  ( 0.3543493200069163240, 0.000000000000000000, 0.9351131265310288487 ) ) ;
#7047 = CARTESIAN_POINT ( 'NONE',  ( -13.82816939922344091, -17.24070752338409918, 4.000000000000000000 ) ) ;
#7048 = CARTESIAN_POINT ( 'NONE',  ( -42.48921356237308800, -27.52281430457085065, 5.000000000000000000 ) ) ;
#7049 = DIRECTION ( 'NONE',  ( -0.3543493200069162685, -0.000000000000000000, -0.9351131265310288487 ) ) ;
#7050 = ORIENTED_EDGE ( 'NONE', *, *, #128520, .F. ) ;
#7051 = CARTESIAN_POINT ( 'NONE',  ( 3.010427959778288365, -48.08977582060914813, 37.49964900842618931 ) ) ;
#7053 = VERTEX_POINT ( 'NONE', #56554 ) ;
#7052 = CIRCLE ( 'NONE', #25614, 9.119999999999999218 ) ;
#7054 = CARTESIAN_POINT ( 'NONE',  ( 5.228736474768552078, 5.808823158059031044, -5.808823158059038150 ) ) ;
#7055 = CARTESIAN_POINT ( 'NONE',  ( -11.20666063542143753, 21.75929247661549937, 4.998822639870708073 ) ) ;
#7056 = CARTESIAN_POINT ( 'NONE',  ( 63.18398860626900415, 28.73617430169831621, 5.000000000000000000 ) ) ;
#7057 = CARTESIAN_POINT ( 'NONE',  ( 10.49999999999993072, 15.05218569542901896, 5.000000000000000000 ) ) ;
#7058 = EDGE_LOOP ( 'NONE', ( #28381, #142275, #4915, #27729 ) ) ;
#7059 = VERTEX_POINT ( 'NONE', #88431 ) ;
#7060 = EDGE_CURVE ( 'NONE', #64733, #14309, #31892, .T. ) ;
#7061 = ORIENTED_EDGE ( 'NONE', *, *, #44700, .F. ) ;
#7063 = VECTOR ( 'NONE', #56221, 1000.000000000000000 ) ;
#7062 = CARTESIAN_POINT ( 'NONE',  ( 15.83159235450332147, -2.500000000000000444, 3.061616997868384620E-16 ) ) ;
#7064 = LINE ( 'NONE', #41160, #136742 ) ;
#7065 = CARTESIAN_POINT ( 'NONE',  ( 13.49999999999990763, 8.900465351122162971, -2.516491619111544953 ) ) ;
#7066 = CARTESIAN_POINT ( 'NONE',  ( -12.49289321881345494, -22.06289321881344634, -1.793453714559299607E-17 ) ) ;
#7067 = FACE_OUTER_BOUND ( 'NONE', #97351, .T. ) ;
#7068 = DIRECTION ( 'NONE',  ( -0.7071067811865486830, -0.7071067811865464625, 0.000000000000000000 ) ) ;
#7069 = CARTESIAN_POINT ( 'NONE',  ( 5.700255128608413102, -27.71228299555201957, 4.000000000000000000 ) ) ;
#7070 = VECTOR ( 'NONE', #110395, 1000.000000000000000 ) ;
#7071 = VECTOR ( 'NONE', #80141, 1000.000000000000227 ) ;
#7072 = CARTESIAN_POINT ( 'NONE',  ( 20.99065804761471199, 3.061616997868383634E-16, -2.500000000000000444 ) ) ;
#7073 = FACE_OUTER_BOUND ( 'NONE', #99253, .T. ) ;
#7074 = LINE ( 'NONE', #7813, #141478 ) ;
#7075 = VECTOR ( 'NONE', #3045, 1000.000000000000114 ) ;
#7076 = VERTEX_POINT ( 'NONE', #120281 ) ;
#7077 = DIRECTION ( 'NONE',  ( -0.000000000000000000, 0.3543493200069153248, 0.9351131265310292928 ) ) ;
#7078 = CARTESIAN_POINT ( 'NONE',  ( 54.18398860626899705, 28.73617430169825226, 5.000000000000000000 ) ) ;
#7079 = ORIENTED_EDGE ( 'NONE', *, *, #113747, .F. ) ;
#7080 = ADVANCED_FACE ( 'NONE', ( #20998 ), #10129, .T. ) ;
#7081 = CARTESIAN_POINT ( 'NONE',  ( -0.2997448713915885632, -27.71228299555206220, 4.000000000000000000 ) ) ;
#7083 = ORIENTED_EDGE ( 'NONE', *, *, #132071, .F. ) ;
#7082 = CARTESIAN_POINT ( 'NONE',  ( 4.930039745135884388, -0.7407075233842770334, 13.87443053587610109 ) ) ;
#7084 = EDGE_CURVE ( 'NONE', #141344, #142044, #54643, .T. ) ;
#7085 = PRESENTATION_LAYER_ASSIGNMENT (  '', '', ( #69668 ) ) ;
#7086 = LINE ( 'NONE', #38340, #116349 ) ;
#7087 = FACE_OUTER_BOUND ( 'NONE', #54296, .T. ) ;
#7088 = ORIENTED_EDGE ( 'NONE', *, *, #100826, .F. ) ;
#7089 = DIRECTION ( 'NONE',  ( -0.7071067811865486830, -0.7071067811865464625, 0.000000000000000000 ) ) ;
#7090 = UNCERTAINTY_MEASURE_WITH_UNIT (LENGTH_MEASURE( 1.000000000000000082E-05 ), #95434, 'distance_accuracy_value', 'NONE');
#7091 = EDGE_LOOP ( 'NONE', ( #110812, #131178, #76099, #72331 ) ) ;
#7092 = EDGE_CURVE ( 'NONE', #74581, #53159, #86811, .T. ) ;
#7093 = EDGE_CURVE ( 'NONE', #138830, #18068, #10746, .T. ) ;
#7094 = FACE_OUTER_BOUND ( 'NONE', #46231, .T. ) ;
#7095 = CARTESIAN_POINT ( 'NONE',  ( 121.5583603837962130, -7.949999999999997513, -2.130196079827425759 ) ) ;
#7096 = LINE ( 'NONE', #4213, #120270 ) ;
#7097 = VECTOR ( 'NONE', #98256, 1000.000000000000000 ) ;
#7098 = CARTESIAN_POINT ( 'NONE',  ( 30.29974487139158867, -27.71228299555227537, 4.000000000000000000 ) ) ;
#7099 = EDGE_CURVE ( 'NONE', #53161, #80396, #97792, .T. ) ;
#7100 = LINE ( 'NONE', #107158, #132505 ) ;
#7101 = DIRECTION ( 'NONE',  ( 0.7071067811865487940, 0.7071067811865463515, 0.000000000000000000 ) ) ;
#7103 = AXIS2_PLACEMENT_3D ( 'NONE', #130941, #125596, #26271 ) ;
#7102 = CARTESIAN_POINT ( 'NONE',  ( 7.583333333333333925, -5.278424836066144543, 3.047499999999995879 ) ) ;
#7104 = CARTESIAN_POINT ( 'NONE',  ( 10.18706980810188512, -2.126176841940956130, 7.934999999999990727 ) ) ;
#7105 = DIRECTION ( 'NONE',  ( -0.7071067811865486830, -0.7071067811865464625, 0.000000000000000000 ) ) ;
#7106 = CARTESIAN_POINT ( 'NONE',  ( 7.171830600776425868, 3.759292476615681888, 4.000000000000000000 ) ) ;
#7107 = VERTEX_POINT ( 'NONE', #119511 ) ;
#7108 = ORIENTED_EDGE ( 'NONE', *, *, #142417, .T. ) ;
#7110 = EDGE_CURVE ( 'NONE', #89257, #37221, #120220, .T. ) ;
#7109 = CARTESIAN_POINT ( 'NONE',  ( 85.87500000000000000, 7.950000000000000178, 1.460391307983218535E-15 ) ) ;
#7111 = CARTESIAN_POINT ( 'NONE',  ( 0.000000000000000000, 0.000000000000000000, 5.000000000000000000 ) ) ;
#7112 = VERTEX_POINT ( 'NONE', #108633 ) ;
#7113 = DIRECTION ( 'NONE',  ( -0.7071067811865487940, 0.7071067811865463515, -0.000000000000000000 ) ) ;
#7114 = CARTESIAN_POINT ( 'NONE',  ( 3.398789304146613510, 2.055000000000001048, 2.516649172247811554E-16 ) ) ;
#7115 = AXIS2_PLACEMENT_3D ( 'NONE', #136900, #70271, #2058 ) ;
#7116 = LINE ( 'NONE', #126103, #6048 ) ;
#7117 = ORIENTED_EDGE ( 'NONE', *, *, #138129, .F. ) ;
#7118 = EDGE_CURVE ( 'NONE', #136547, #23940, #74638, .T. ) ;
#7119 = CARTESIAN_POINT ( 'NONE',  ( 31.17183060077625356, -5.240707523384228850, 4.000000000000000000 ) ) ;
#7120 = CARTESIAN_POINT ( 'NONE',  ( 14.70025512860841133, -27.71228299555195917, 4.000000000000000000 ) ) ;
#7121 = CARTESIAN_POINT ( 'NONE',  ( 39.29974487139159578, -27.71228299555233576, 4.000000000000000000 ) ) ;
#7122 = LINE ( 'NONE', #73857, #90994 ) ;
#7123 = DIRECTION ( 'NONE',  ( 0.7071067811865486830, -0.7071067811865464625, -0.000000000000000000 ) ) ;
#7124 = ADVANCED_FACE ( 'NONE', ( #44144 ), #65197, .F. ) ;
#7125 = FACE_OUTER_BOUND ( 'NONE', #67752, .T. ) ;
#7126 = AXIS2_PLACEMENT_3D ( 'NONE', #121087, #57304, #111657 ) ;
#7127 = CARTESIAN_POINT ( 'NONE',  ( 0.000000000000000000, 0.000000000000000000, 5.000000000000000000 ) ) ;
#7128 = FACE_OUTER_BOUND ( 'NONE', #43965, .T. ) ;
#7129 = DIRECTION ( 'NONE',  ( -0.7071067811865487940, 0.7071067811865463515, 0.000000000000000000 ) ) ;
#7130 = CARTESIAN_POINT ( 'NONE',  ( 55.64345981607718272, -48.97294124528174564, 39.12804664298385404 ) ) ;
#7131 = ORIENTED_EDGE ( 'NONE', *, *, #67255, .T. ) ;
#7132 = EDGE_LOOP ( 'NONE', ( #126882, #93561, #23473, #96035 ) ) ;
#7133 = CARTESIAN_POINT ( 'NONE',  ( 100.7712635252314328, 4.472830434245839371, 4.472830434245842035 ) ) ;
#7134 = ORIENTED_EDGE ( 'NONE', *, *, #91906, .F. ) ;
#7135 = EDGE_CURVE ( 'NONE', #130377, #58822, #131142, .T. ) ;
#7136 = CARTESIAN_POINT ( 'NONE',  ( 26.12514619309218133, -14.24070752338413470, 9.401115078912598122 ) ) ;
#7137 = CARTESIAN_POINT ( 'NONE',  ( -23.81601139373100295, 28.73617430169770870, 5.000000000000000000 ) ) ;
#7138 = ORIENTED_EDGE ( 'NONE', *, *, #26163, .F. ) ;
#7139 = COLOUR_RGB ( '', 0.09019608, 0.27058824, 0.51372549) ;
#7140 = CARTESIAN_POINT ( 'NONE',  ( 38.99451991528749062, 28.92564299267965211, 4.000000000000000000 ) ) ;
#7141 = CARTESIAN_POINT ( 'NONE',  ( 60.48921356237309510, -27.52281430457097500, 5.000000000000000000 ) ) ;
#7143 = EDGE_CURVE ( 'NONE', #128780, #91002, #132607, .T. ) ;
#7142 = CONICAL_SURFACE ( 'NONE', #2498, 2.055000000000001048, 0.9599310885968758145 ) ;
#7144 = AXIS2_PLACEMENT_3D ( 'NONE', #110066, #122367, #61793 ) ;
#7145 = CARTESIAN_POINT ( 'NONE',  ( 92.66209685856479439, -5.291415217122919401, 3.054999999999997939 ) ) ;
#7146 = ORIENTED_EDGE ( 'NONE', *, *, #68056, .T. ) ;
#7147 = EDGE_CURVE ( 'NONE', #81467, #102769, #9307, .T. ) ;
#7148 = LINE ( 'NONE', #63036, #18788 ) ;
#7149 = ORIENTED_EDGE ( 'NONE', *, *, #29776, .F. ) ;
#7150 = DIRECTION ( 'NONE',  ( 1.000000000000000000, 0.000000000000000000, 0.000000000000000000 ) ) ;
#7151 = VECTOR ( 'NONE', #124616, 1000.000000000000000 ) ;
#7152 = VECTOR ( 'NONE', #52600, 1000.000000000000000 ) ;
#7153 = DIRECTION ( 'NONE',  ( 0.2419218955996628451, 0.000000000000000000, 0.9702957262759975832 ) ) ;
#7154 = VECTOR ( 'NONE', #67798, 1000.000000000000000 ) ;
#7155 = AXIS2_PLACEMENT_3D ( 'NONE', #37702, #79084, #113083 ) ;
#7156 = CARTESIAN_POINT ( 'NONE',  ( 0.2997448713915885632, -27.71228299555206220, 4.000000000000000000 ) ) ;
#7157 = EDGE_CURVE ( 'NONE', #103619, #82336, #66609, .T. ) ;
#7158 = VECTOR ( 'NONE', #55983, 1000.000000000000000 ) ;
#7159 = VERTEX_POINT ( 'NONE', #98507 ) ;
#7160 = ORIENTED_EDGE ( 'NONE', *, *, #59069, .T. ) ;
#7161 = ORIENTED_EDGE ( 'NONE', *, *, #113885, .T. ) ;
#7162 = DIRECTION ( 'NONE',  ( 0.3543493200069162685, -0.000000000000000000, -0.9351131265310288487 ) ) ;
#7163 = DIRECTION ( 'NONE',  ( -0.7071067811865486830, -0.7071067811865464625, -0.000000000000000000 ) ) ;
#7164 = CARTESIAN_POINT ( 'NONE',  ( 4.587903141435219823, 6.871911579029515771, 3.967499999999989146 ) ) ;
#7165 = AXIS2_PLACEMENT_3D ( 'NONE', #30168, #74415, #20712 ) ;
#7166 = LINE ( 'NONE', #50017, #87316 ) ;
#7167 = ORIENTED_EDGE ( 'NONE', *, *, #103846, .F. ) ;
#7168 = VERTEX_POINT ( 'NONE', #63762 ) ;
#7170 = ADVANCED_FACE ( 'NONE', ( #121668 ), #142731, .T. ) ;
#7169 = CIRCLE ( 'NONE', #88245, 6.450000000000025047 ) ;
#7171 = LINE ( 'NONE', #115945, #68719 ) ;
#7172 = ORIENTED_EDGE ( 'NONE', *, *, #121256, .T. ) ;
#7173 = ORIENTED_EDGE ( 'NONE', *, *, #117622, .F. ) ;
#7174 =( GEOMETRIC_REPRESENTATION_CONTEXT ( 3 ) GLOBAL_UNCERTAINTY_ASSIGNED_CONTEXT ( ( #56403 ) ) GLOBAL_UNIT_ASSIGNED_CONTEXT ( ( #331, #33734, #67058 ) ) REPRESENTATION_CONTEXT ( 'NONE', 'WORKASPACE' ) );
#7175 = EDGE_CURVE ( 'NONE', #109845, #94724, #99943, .T. ) ;
#7176 = VECTOR ( 'NONE', #133618, 1000.000000000000000 ) ;
#7177 = CARTESIAN_POINT ( 'NONE',  ( 6.328169399223492420, -0.7407075233842735917, 4.000000000000000000 ) ) ;
#7178 = DIRECTION ( 'NONE',  ( 0.000000000000000000, -1.000000000000000000, 0.000000000000000000 ) ) ;
#7179 = ORIENTED_EDGE ( 'NONE', *, *, #89538, .T. ) ;
#7180 = FACE_OUTER_BOUND ( 'NONE', #107301, .T. ) ;
#7181 = AXIS2_PLACEMENT_3D ( 'NONE', #85491, #53617, #88393 ) ;
#7182 = CARTESIAN_POINT ( 'NONE',  ( 25.39999999999999858, -1.600000000000060929, 28.92500000000001847 ) ) ;
#7183 = DIRECTION ( 'NONE',  ( -0.000000000000000000, -0.3543493200069152693, 0.9351131265310292928 ) ) ;
#7184 = VECTOR ( 'NONE', #12473, 999.9999999999998863 ) ;
#7185 = SURFACE_SIDE_STYLE ('',( #73217 ) ) ;
#7186 = ORIENTED_EDGE ( 'NONE', *, *, #17084, .T. ) ;
#7187 = PLANE ( 'NONE',  #85719 ) ;
#7188 = LINE ( 'NONE', #118838, #50045 ) ;
#7189 = VERTEX_POINT ( 'NONE', #110084 ) ;
#7190 = LINE ( 'NONE', #84792, #4017 ) ;
#7191 = PLANE ( 'NONE',  #142982 ) ;
#7192 = VECTOR ( 'NONE', #137849, 1000.000000000000000 ) ;
#7193 = DIRECTION ( 'NONE',  ( -0.7071067811865487940, 0.7071067811865463515, -0.000000000000000000 ) ) ;
#7194 = EDGE_CURVE ( 'NONE', #116279, #141681, #52837, .T. ) ;
#7195 = ORIENTED_EDGE ( 'NONE', *, *, #92385, .T. ) ;
#7196 = LINE ( 'NONE', #107250, #73664 ) ;
#7197 = EDGE_LOOP ( 'NONE', ( #22983, #18619, #5587, #136048, #141619 ) ) ;
#7198 = EDGE_LOOP ( 'NONE', ( #80305, #4114, #115885, #110226 ) ) ;
#7199 = EDGE_LOOP ( 'NONE', ( #78162, #11306, #41333, #68225 ) ) ;
#7200 = EDGE_CURVE ( 'NONE', #12371, #81437, #21669, .T. ) ;
#7201 = DIRECTION ( 'NONE',  ( 0.7071067811865487940, 0.7071067811865463515, 0.000000000000000000 ) ) ;
#7202 = VECTOR ( 'NONE', #12015, 1000.000000000000000 ) ;
#7203 = DIRECTION ( 'NONE',  ( -0.7071067811865486830, -0.7071067811865464625, -0.000000000000000000 ) ) ;
#7204 = PLANE ( 'NONE',  #10119 ) ;
#7205 = CARTESIAN_POINT ( 'NONE',  ( 45.48921356237309510, -27.52281430457087197, 5.000000000000000000 ) ) ;
#7206 = FACE_OUTER_BOUND ( 'NONE', #134097, .T. ) ;
#7207 = CARTESIAN_POINT ( 'NONE',  ( 17.99999999999987210, -6.108550654416944781, -3.114665004254924430 ) ) ;
#7209 = CARTESIAN_POINT ( 'NONE',  ( 30.48921356237309510, -27.52281430457076894, 5.000000000000000000 ) ) ;
#7208 = AXIS2_PLACEMENT_3D ( 'NONE', #52626, #121455, #109873 ) ;
#7210 = CIRCLE ( 'NONE', #92939, 2.055000000000000604 ) ;
#7211 = LINE ( 'NONE', #62364, #35293 ) ;
#7212 = EDGE_CURVE ( 'NONE', #128869, #90647, #76793, .T. ) ;
#7213 = LINE ( 'NONE', #84812, #8835 ) ;
#7214 = LINE ( 'NONE', #126183, #126919 ) ;
#7215 = DIRECTION ( 'NONE',  ( 1.000000000000000000, -0.000000000000000000, 0.000000000000000000 ) ) ;
#7216 = CIRCLE ( 'NONE', #134568, 6.094999999999989093 ) ;
#7217 = VERTEX_POINT ( 'NONE', #42729 ) ;
#7218 = ORIENTED_EDGE ( 'NONE', *, *, #27467, .T. ) ;
#7219 = ORIENTED_EDGE ( 'NONE', *, *, #133389, .F. ) ;
#7220 = AXIS2_PLACEMENT_3D ( 'NONE', #22072, #88068, #120664 ) ;
#7221 = ORIENTED_EDGE ( 'NONE', *, *, #58596, .F. ) ;
#7222 = CARTESIAN_POINT ( 'NONE',  ( 23.63159235450331863, 9.902892378096218942E-16, 0.000000000000000000 ) ) ;
#7223 = VERTEX_POINT ( 'NONE', #31827 ) ;
#7224 =( BOUNDED_CURVE ( )  B_SPLINE_CURVE ( 2, ( #104630, #27067, #48129 ),
 .UNSPECIFIED., .F., .F. ) 
 B_SPLINE_CURVE_WITH_KNOTS ( ( 3, 3 ),
 ( 0.01429413858638482922, 0.01666666666666668031 ),
 .UNSPECIFIED. ) 
 CURVE ( )  GEOMETRIC_REPRESENTATION_ITEM ( )  RATIONAL_B_SPLINE_CURVE ( ( 0.9915083049239679092, 0.9708969037810285529, 1.000000000000000222 ) ) 
 REPRESENTATION_ITEM ( '' )  );
#7225 = VERTEX_POINT ( 'NONE', #65918 ) ;
#7226 = FACE_OUTER_BOUND ( 'NONE', #96435, .T. ) ;
#7227 = SURFACE_STYLE_USAGE ( .BOTH. , #142773 ) ;
#7228 = DIRECTION ( 'NONE',  ( 0.7071067811865487940, 0.7071067811865463515, 0.000000000000000000 ) ) ;
#7229 = EDGE_CURVE ( 'NONE', #13435, #99726, #100692, .T. ) ;
#7230 = PLANE ( 'NONE',  #27787 ) ;
#7231 = ORIENTED_EDGE ( 'NONE', *, *, #91310, .T. ) ;
#7232 = DIRECTION ( 'NONE',  ( 0.7071067811865487940, -0.7071067811865463515, 0.000000000000000000 ) ) ;
#7233 = AXIS2_PLACEMENT_3D ( 'NONE', #123636, #122888, #13383 ) ;
#7234 = EDGE_LOOP ( 'NONE', ( #132066, #31674, #84211, #26323 ) ) ;
#7235 = LINE ( 'NONE', #98554, #72217 ) ;
#7236 = CARTESIAN_POINT ( 'NONE',  ( 7.122370700763592133, -39.92999999999999972, 19.06900128115122328 ) ) ;
#7237 = CARTESIAN_POINT ( 'NONE',  ( 5.171236474768553748, 0.000000000000000000, 7.934999999999990727 ) ) ;
#7238 = VERTEX_POINT ( 'NONE', #42004 ) ;
#7239 = CARTESIAN_POINT ( 'NONE',  ( 93.09959685856479439, -6.109999999999998543, -1.637169565754160727 ) ) ;
#7240 = LINE ( 'NONE', #139960, #76024 ) ;
#7241 = DIRECTION ( 'NONE',  ( -0.7071067811865486830, -0.7071067811865464625, -0.000000000000000000 ) ) ;
#7242 = LINE ( 'NONE', #95709, #129914 ) ;
#7243 = VERTEX_POINT ( 'NONE', #86220 ) ;
#7244 = VERTEX_POINT ( 'NONE', #75349 ) ;
#7245 = LINE ( 'NONE', #42792, #31142 ) ;
#7246 = ORIENTED_EDGE ( 'NONE', *, *, #18565, .T. ) ;
#7247 = CARTESIAN_POINT ( 'NONE',  ( -9.183988606268997046, 28.73617430169793607, 5.000000000000000000 ) ) ;
#7248 = CARTESIAN_POINT ( 'NONE',  ( 60.29974487139158867, -27.71228299555248142, 4.000000000000000000 ) ) ;
#7249 = AXIS2_PLACEMENT_3D ( 'NONE', #93403, #28151, #26012 ) ;
#7250 = CARTESIAN_POINT ( 'NONE',  ( -24.18398860626899705, 28.73617430169804265, 5.000000000000000000 ) ) ;
#7251 = CARTESIAN_POINT ( 'NONE',  ( -9.098435806082317612, 11.25929247661560240, 10.79108189686405161 ) ) ;
#7252 = ORIENTED_EDGE ( 'NONE', *, *, #48260, .F. ) ;
#7253 = AXIS2_PLACEMENT_3D ( 'NONE', #93018, #69881, #57559 ) ;
#7254 = CARTESIAN_POINT ( 'NONE',  ( -35.99451991528749772, 28.92564299267963079, 4.000000000000000000 ) ) ;
#7255 = VECTOR ( 'NONE', #118645, 999.9999999999998863 ) ;
#7256 = B_SPLINE_CURVE_WITH_KNOTS ( 'NONE', 1,
 ( #2140, #46450 ),
 .UNSPECIFIED., .F., .F.,
 ( 2, 2 ),
 ( 0.8695652173913019922, 1.000000000000000000 ),
 .UNSPECIFIED. ) ;
#7257 = LINE ( 'NONE', #130522, #109113 ) ;
#7258 = LINE ( 'NONE', #142116, #118271 ) ;
#7259 = EDGE_CURVE ( 'NONE', #8140, #91460, #80358, .T. ) ;
#7260 = ORIENTED_EDGE ( 'NONE', *, *, #67317, .F. ) ;
#7261 = FACE_OUTER_BOUND ( 'NONE', #50879, .T. ) ;
#7262 = VECTOR ( 'NONE', #92512, 1000.000000000000000 ) ;
#7263 = PRESENTATION_LAYER_ASSIGNMENT (  '', '', ( #35064 ) ) ;
#7264 = VECTOR ( 'NONE', #52657, 1000.000000000000000 ) ;
#7265 = LINE ( 'NONE', #61705, #738 ) ;
#7267 = VERTEX_POINT ( 'NONE', #122384 ) ;
#7266 = VECTOR ( 'NONE', #105847, 1000.000000000000000 ) ;
#7269 = EDGE_LOOP ( 'NONE', ( #2372, #106241, #31717, #97864 ) ) ;
#7268 = CARTESIAN_POINT ( 'NONE',  ( 22.53999999999999915, -2.055000000000000160, 0.000000000000000000 ) ) ;
#7270 = EDGE_CURVE ( 'NONE', #64780, #54692, #24515, .T. ) ;
#7271 = ADVANCED_FACE ( 'NONE', ( #89763 ), #57897, .F. ) ;
#7272 = CARTESIAN_POINT ( 'NONE',  ( -9.693269933095928437, -3.740707523384244837, 12.88036043432869882 ) ) ;
#7273 = AXIS2_PLACEMENT_3D ( 'NONE', #47529, #72129, #114153 ) ;
#7274 = DIRECTION ( 'NONE',  ( 0.7071067811865486830, -0.7071067811865464625, -0.000000000000000000 ) ) ;
#7275 = ORIENTED_EDGE ( 'NONE', *, *, #122326, .T. ) ;
#7276 = DIRECTION ( 'NONE',  ( 0.7071067811865486830, -0.7071067811865464625, -0.000000000000000000 ) ) ;
#7277 = EDGE_CURVE ( 'NONE', #15156, #71528, #107606, .T. ) ;
#7278 = ADVANCED_FACE ( 'NONE', ( #23812 ), #100666, .F. ) ;
#7279 = CARTESIAN_POINT ( 'NONE',  ( 14.20666063542142687, 21.75929247661549937, 4.998822639870700080 ) ) ;
#7280 = LINE ( 'NONE', #74003, #36803 ) ;
#7281 = EDGE_CURVE ( 'NONE', #118169, #126680, #103481, .T. ) ;
#7282 = VECTOR ( 'NONE', #2382, 1000.000000000000000 ) ;
#7283 = DIRECTION ( 'NONE',  ( 0.000000000000000000, -1.000000000000000000, 0.000000000000000000 ) ) ;
#7284 = CARTESIAN_POINT ( 'NONE',  ( -78.48921356237309510, -27.52281430457109934, 5.000000000000000000 ) ) ;
#7285 = EDGE_CURVE ( 'NONE', #23427, #56845, #34696, .T. ) ;
#7286 = LINE ( 'NONE', #129801, #11997 ) ;
#7287 = DIRECTION ( 'NONE',  ( 0.7071067811865487940, 0.7071067811865463515, 0.000000000000000000 ) ) ;
#7288 = DIRECTION ( 'NONE',  ( 0.7071067811865487940, -0.7071067811865463515, 0.000000000000000000 ) ) ;
#7289 = CARTESIAN_POINT ( 'NONE',  ( 14.99999999999990941, -19.44781430457063465, 5.000000000000000000 ) ) ;
#7290 = CARTESIAN_POINT ( 'NONE',  ( 21.11237052021067129, 8.776708805967446736, 4.202873650309270737 ) ) ;
#7291 = EDGE_CURVE ( 'NONE', #130333, #121313, #45594, .T. ) ;
#7292 = DIRECTION ( 'NONE',  ( 0.7071067811865486830, -0.7071067811865464625, -0.000000000000000000 ) ) ;
#7293 = ORIENTED_EDGE ( 'NONE', *, *, #61025, .T. ) ;
#7294 = VECTOR ( 'NONE', #108639, 1000.000000000000227 ) ;
#7295 = EDGE_LOOP ( 'NONE', ( #51413, #51817, #49134 ) ) ;
#7296 = ORIENTED_EDGE ( 'NONE', *, *, #80533, .F. ) ;
#7298 = EDGE_CURVE ( 'NONE', #64292, #85310, #38198, .T. ) ;
#7297 = CARTESIAN_POINT ( 'NONE',  ( 114.1666666666666714, 6.884901960086285300, 3.975000000000003642 ) ) ;
#7299 = VECTOR ( 'NONE', #94017, 1000.000000000000000 ) ;
#7300 = ORIENTED_EDGE ( 'NONE', *, *, #3295, .F. ) ;
#7301 = EDGE_LOOP ( 'NONE', ( #115354, #8356, #21460, #17902 ) ) ;
#7302 = CONICAL_SURFACE ( 'NONE', #11972, 2.247899999999995568, 1.029744258676650315 ) ;
#7303 = ORIENTED_EDGE ( 'NONE', *, *, #14860, .T. ) ;
#7304 = PLANE ( 'NONE',  #140451 ) ;
#7305 = CARTESIAN_POINT ( 'NONE',  ( 89.81249999999998579, 5.819803920172571310, 5.819803920172576639 ) ) ;
#7306 = VECTOR ( 'NONE', #105718, 999.9999999999998863 ) ;
#7307 = ORIENTED_EDGE ( 'NONE', *, *, #5932, .T. ) ;
#7308 = DIRECTION ( 'NONE',  ( -8.817971600062199903E-18, 0.3543493200069153248, 0.9351131265310292928 ) ) ;
#7309 = EDGE_CURVE ( 'NONE', #4615, #57316, #35439, .T. ) ;
#7310 = FACE_OUTER_BOUND ( 'NONE', #108390, .T. ) ;
#7311 = CARTESIAN_POINT ( 'NONE',  ( 25.49999999999981881, -20.56887692260760758, 4.000000000000000000 ) ) ;
#7312 = CARTESIAN_POINT ( 'NONE',  ( 25.34840764549667469, 3.061616997868380183E-16, -2.500000000000001332 ) ) ;
#7313 = CARTESIAN_POINT ( 'NONE',  ( 98.87543019189810423, -5.291415217122920289, -3.055000000000001492 ) ) ;
#7314 = ORIENTED_EDGE ( 'NONE', *, *, #6359, .T. ) ;
#7315 = LINE ( 'NONE', #84900, #64999 ) ;
#7316 = DIRECTION ( 'NONE',  ( 0.3543493200069162685, -0.000000000000000000, -0.9351131265310288487 ) ) ;
#7317 = DIRECTION ( 'NONE',  ( -0.000000000000000000, 1.000000000000000000, -0.000000000000000000 ) ) ;
#7318 = DIRECTION ( 'NONE',  ( -0.7071067811865487940, 0.7071067811865463515, -0.000000000000000000 ) ) ;
#7319 = EDGE_CURVE ( 'NONE', #1998, #35419, #96013, .T. ) ;
#7320 = AXIS2_PLACEMENT_3D ( 'NONE', #53219, #97432, #9715 ) ;
#7321 = DIRECTION ( 'NONE',  ( 0.7071067811865487940, 0.7071067811865463515, -0.000000000000000000 ) ) ;
#7322 =( NAMED_UNIT ( * ) PLANE_ANGLE_UNIT ( ) SI_UNIT ( $, .RADIAN. ) );
#7323 = CARTESIAN_POINT ( 'NONE',  ( 28.37086038379622721, 6.884901960086289741, -3.974999999999993427 ) ) ;
#7324 = CARTESIAN_POINT ( 'NONE',  ( 13.49999999999991473, -4.796895815301002841, -3.611700055028651768 ) ) ;
#7325 = ORIENTED_EDGE ( 'NONE', *, *, #97452, .F. ) ;
#7326 = VERTEX_POINT ( 'NONE', #69477 ) ;
#7327 = CARTESIAN_POINT ( 'NONE',  ( 125.4170968585647756, 3.054999999999998828, 5.291415217122922066 ) ) ;
#7328 = ORIENTED_EDGE ( 'NONE', *, *, #32406, .F. ) ;
#7329 = CARTESIAN_POINT ( 'NONE',  ( 0.4892135623730947680, -27.52281430457055578, 5.000000000000000000 ) ) ;
#7330 = VECTOR ( 'NONE', #42157, 1000.000000000000000 ) ;
#7331 = LINE ( 'NONE', #84241, #128849 ) ;
#7332 = VECTOR ( 'NONE', #113204, 1000.000000000000000 ) ;
#7333 = DIRECTION ( 'NONE',  ( -0.000000000000000000, -0.000000000000000000, 1.000000000000000000 ) ) ;
#7334 = CARTESIAN_POINT ( 'NONE',  ( -36.48921356237310221, -27.52281430457080802, 5.000000000000000000 ) ) ;
#7335 =( NAMED_UNIT ( * ) PLANE_ANGLE_UNIT ( ) SI_UNIT ( $, .RADIAN. ) );
#7336 = SURFACE_SIDE_STYLE ('',( #118970 ) ) ;
#7337 = ADVANCED_FACE ( 'NONE', ( #57185 ), #23056, .T. ) ;
#7338 = CARTESIAN_POINT ( 'NONE',  ( 126.0579301918981230, 6.110000000000000320, -1.637169565754156064 ) ) ;
#7339 = VERTEX_POINT ( 'NONE', #101360 ) ;
#7340 = VECTOR ( 'NONE', #141143, 1000.000000000000000 ) ;
#7341 = EDGE_CURVE ( 'NONE', #44042, #109431, #90498, .T. ) ;
#7342 = LINE ( 'NONE', #73360, #105817 ) ;
#7343 = ORIENTED_EDGE ( 'NONE', *, *, #88408, .T. ) ;
#7344 = VECTOR ( 'NONE', #34773, 999.9999999999998863 ) ;
#7345 = PLANE ( 'NONE',  #73995 ) ;
#7346 = CARTESIAN_POINT ( 'NONE',  ( -36.48921356237310221, -27.52281430457080802, 5.000000000000000000 ) ) ;
#7348 = ADVANCED_FACE ( 'NONE', ( #58642 ), #3451, .F. ) ;
#7347 = DIRECTION ( 'NONE',  ( -0.3543493200069162685, -0.000000000000000000, -0.9351131265310288487 ) ) ;
#7349 = CARTESIAN_POINT ( 'NONE',  ( 16.49999999999989342, 19.46639925780206326, 5.000000000000000000 ) ) ;
#7350 = ORIENTED_EDGE ( 'NONE', *, *, #141290, .T. ) ;
#7351 = CARTESIAN_POINT ( 'NONE',  ( 45.50043019189810423, -3.055000000000002380, 5.291415217122920289 ) ) ;
#7352 = ORIENTED_EDGE ( 'NONE', *, *, #108613, .T. ) ;
#7353 = DIRECTION ( 'NONE',  ( 1.000000000000000000, 0.000000000000000000, 0.000000000000000000 ) ) ;
#7354 = LINE ( 'NONE', #52301, #83193 ) ;
#7355 = DIRECTION ( 'NONE',  ( -0.7071067811865486830, -0.7071067811865464625, 0.000000000000000000 ) ) ;
#7356 = CARTESIAN_POINT ( 'NONE',  ( -7.940000000000007496, -60.26999999999998892, -12.24790000000000312 ) ) ;
#7357 = CIRCLE ( 'NONE', #102294, 2.500000000000000444 ) ;
#7358 =( BOUNDED_CURVE ( )  B_SPLINE_CURVE ( 3, ( #91355, #9638, #53916, #68200 ),
 .UNSPECIFIED., .F., .T. ) 
 B_SPLINE_CURVE_WITH_KNOTS ( ( 4, 4 ),
 ( 1.862445515227526771, 1.909667095125055392 ),
 .UNSPECIFIED. ) 
 CURVE ( )  GEOMETRIC_REPRESENTATION_ITEM ( )  RATIONAL_B_SPLINE_CURVE ( ( 1.000000000000000000, 0.9998141854983972898, 0.9998141854983972898, 1.000000000000000000 ) ) 
 REPRESENTATION_ITEM ( '' )  );
#7359 = CARTESIAN_POINT ( 'NONE',  ( 36.37043019189811588, -3.055000000000001492, 5.291415217122917625 ) ) ;
#7360 = ORIENTED_EDGE ( 'NONE', *, *, #46994, .T. ) ;
#7361 = CARTESIAN_POINT ( 'NONE',  ( -54.48921356237310221, -27.52281430457093236, 5.000000000000000000 ) ) ;
#7362 = ADVANCED_FACE ( 'NONE', ( #36814 ), #81061, .F. ) ;
#7363 = CARTESIAN_POINT ( 'NONE',  ( 57.48921356237308800, -27.52281430457095368, 5.000000000000000000 ) ) ;
#7364 = ORIENTED_EDGE ( 'NONE', *, *, #110406, .F. ) ;
#7365 = VERTEX_POINT ( 'NONE', #15050 ) ;
#7366 = VERTEX_POINT ( 'NONE', #59329 ) ;
#7367 = AXIS2_PLACEMENT_3D ( 'NONE', #57361, #101536, #46512 ) ;
#7368 = LINE ( 'NONE', #137924, #34971 ) ;
#7369 = ADVANCED_FACE ( 'NONE', ( #48410 ), #92609, .F. ) ;
#7370 = EDGE_LOOP ( 'NONE', ( #6290, #122072, #101683, #27540 ) ) ;
#7371 = CARTESIAN_POINT ( 'NONE',  ( 43.97502705046288440, -5.819803920172573086, 5.819803920172573086 ) ) ;
#7373 = FACE_OUTER_BOUND ( 'NONE', #5237, .T. ) ;
#7372 = VECTOR ( 'NONE', #93983, 1000.000000000000000 ) ;
#7374 = VECTOR ( 'NONE', #74391, 1000.000000000000000 ) ;
#7375 = VECTOR ( 'NONE', #3938, 999.9999999999998863 ) ;
#7376 = CARTESIAN_POINT ( 'NONE',  ( 34.42500000000002558, -22.26999999999999247, -0.5000000000000000000 ) ) ;
#7377 = EDGE_CURVE ( 'NONE', #141023, #100787, #51284, .T. ) ;
#7378 = FACE_BOUND ( 'NONE', #60718, .T. ) ;
#7379 = CARTESIAN_POINT ( 'NONE',  ( -57.48921356237308800, -27.52281430457095368, 5.000000000000000000 ) ) ;
#7380 = CARTESIAN_POINT ( 'NONE',  ( 3.730677800976790248, -49.14999999999999147, 40.92499999999998295 ) ) ;
#7381 = EDGE_CURVE ( 'NONE', #55035, #135278, #81791, .T. ) ;
#7382 = ORIENTED_EDGE ( 'NONE', *, *, #7986, .F. ) ;
#7383 = CARTESIAN_POINT ( 'NONE',  ( 181.1500000000000057, -43.14999999999999147, -40.92499999999998295 ) ) ;
#7384 = ORIENTED_EDGE ( 'NONE', *, *, #33496, .F. ) ;
#7385 = ORIENTED_EDGE ( 'NONE', *, *, #116968, .F. ) ;
#7386 = DIRECTION ( 'NONE',  ( -0.000000000000000000, 0.3543493200069153248, 0.9351131265310292928 ) ) ;
#7387 = EDGE_LOOP ( 'NONE', ( #51138, #139168, #4723, #28131 ) ) ;
#7388 = ADVANCED_FACE ( 'NONE', ( #117207 ), #50553, .F. ) ;
#7389 = CARTESIAN_POINT ( 'NONE',  ( 53.43293019189810167, 1.637169565754156508, 6.110000000000000320 ) ) ;
#7390 = VERTEX_POINT ( 'NONE', #104185 ) ;
#7391 = LINE ( 'NONE', #116178, #4676 ) ;
#7392 = LINE ( 'NONE', #105984, #12548 ) ;
#7393 = ORIENTED_EDGE ( 'NONE', *, *, #11779, .F. ) ;
#7394 = FACE_OUTER_BOUND ( 'NONE', #94620, .T. ) ;
#7395 = EDGE_CURVE ( 'NONE', #26993, #67807, #60019, .T. ) ;
#7396 = VECTOR ( 'NONE', #133839, 1000.000000000000000 ) ;
#7397 = VECTOR ( 'NONE', #69274, 1000.000000000000227 ) ;
#7398 = ADVANCED_FACE ( 'NONE', ( #73054 ), #116524, .T. ) ;
#7399 = DIRECTION ( 'NONE',  ( -0.7071067811865486830, 0.7071067811865464625, 0.000000000000000000 ) ) ;
#7400 = DIRECTION ( 'NONE',  ( -0.7071067811865486830, -0.7071067811865464625, 0.000000000000000000 ) ) ;
#7401 = CARTESIAN_POINT ( 'NONE',  ( -8.953411863704499041, 14.25929247661557753, 18.84478104361330253 ) ) ;
#7402 = AXIS2_PLACEMENT_3D ( 'NONE', #71651, #94087, #138325 ) ;
#7403 = LINE ( 'NONE', #37939, #28416 ) ;
#7404 = DIRECTION ( 'NONE',  ( 0.7071067811865487940, -0.7071067811865463515, 0.000000000000000000 ) ) ;
#7405 = ORIENTED_EDGE ( 'NONE', *, *, #48896, .F. ) ;
#7406 = EDGE_LOOP ( 'NONE', ( #114356, #128447, #47214, #75460 ) ) ;
#7407 = VECTOR ( 'NONE', #23376, 1000.000000000000000 ) ;
#7408 = CARTESIAN_POINT ( 'NONE',  ( 5.999999999999963585, 14.96639925780211122, 5.000000000000000000 ) ) ;
#7409 = DIRECTION ( 'NONE',  ( 0.7071067811865487940, 0.7071067811865463515, 0.000000000000000000 ) ) ;
#7410 = ORIENTED_EDGE ( 'NONE', *, *, #21282, .F. ) ;
#7411 = ORIENTED_EDGE ( 'NONE', *, *, #135225, .T. ) ;
#7412 = EDGE_LOOP ( 'NONE', ( #72394, #102553, #137467, #29584 ) ) ;
#7413 = CARTESIAN_POINT ( 'NONE',  ( -11.99451991528749417, 28.92564299267946382, 4.000000000000000000 ) ) ;
#7414 = EDGE_CURVE ( 'NONE', #25495, #34714, #94745, .T. ) ;
#7415 = DIRECTION ( 'NONE',  ( 0.000000000000000000, 1.000000000000000000, 0.000000000000000000 ) ) ;
#7416 = EDGE_LOOP ( 'NONE', ( #96973, #2614, #49904, #143296 ) ) ;
#7417 = DIRECTION ( 'NONE',  ( 0.7071067811865487940, 0.7071067811865463515, 0.000000000000000000 ) ) ;
#7418 = VECTOR ( 'NONE', #79864, 1000.000000000000227 ) ;
#7419 = DIRECTION ( 'NONE',  ( 0.6830127018922180770, -0.6830127018922204085, -0.2588190451025213501 ) ) ;
#7420 = CARTESIAN_POINT ( 'NONE',  ( 16.10873647476855552, -5.808823158059033709, 5.808823158059035485 ) ) ;
#7421 = PLANE ( 'NONE',  #35664 ) ;
#7422 = EDGE_LOOP ( 'NONE', ( #12684, #52595, #107687, #10267 ) ) ;
#7423 = CARTESIAN_POINT ( 'NONE',  ( 128.6829301918981230, -1.637169565754159173, -6.109999999999999432 ) ) ;
#7424 = CARTESIAN_POINT ( 'NONE',  ( 9.183988606268997046, 28.73617430169793607, 5.000000000000000000 ) ) ;
#7425 = AXIS2_PLACEMENT_3D ( 'NONE', #61604, #107206, #84752 ) ;
#7426 = FACE_OUTER_BOUND ( 'NONE', #99400, .T. ) ;
#7428 = VERTEX_POINT ( 'NONE', #106323 ) ;
#7427 = LINE ( 'NONE', #140130, #17045 ) ;
#7429 = FACE_OUTER_BOUND ( 'NONE', #110944, .T. ) ;
#7430 = VERTEX_POINT ( 'NONE', #139738 ) ;
#7431 = DIRECTION ( 'NONE',  ( 0.5735764363510453823, -0.8191520442889923537, 1.003171929053525486E-16 ) ) ;
#7432 = LINE ( 'NONE', #119064, #9958 ) ;
#7433 = CARTESIAN_POINT ( 'NONE',  ( 0.1161069444170876597, 0.000000000000000000, 0.000000000000000000 ) ) ;
#7434 = VERTEX_POINT ( 'NONE', #84619 ) ;
#7435 = DIRECTION ( 'NONE',  ( -0.7071067811865486830, -0.7071067811865464625, 0.000000000000000000 ) ) ;
#7436 = DIRECTION ( 'NONE',  ( -0.7071067811865487940, 0.7071067811865463515, 0.000000000000000000 ) ) ;
#7438 = ADVANCED_FACE ( 'NONE', ( #7738 ), #88192, .F. ) ;
#7437 = DIRECTION ( 'NONE',  ( 0.000000000000000000, 1.000000000000000000, 0.000000000000000000 ) ) ;
#7439 = VECTOR ( 'NONE', #138530, 1000.000000000000000 ) ;
#7440 = ORIENTED_EDGE ( 'NONE', *, *, #126186, .T. ) ;
#7441 = CARTESIAN_POINT ( 'NONE',  ( -39.48921356237310221, -27.52281430457082934, 5.000000000000000000 ) ) ;
#7442 = CARTESIAN_POINT ( 'NONE',  ( 14.51078643762690490, -27.52281430457045275, 5.000000000000000000 ) ) ;
#7443 = LINE ( 'NONE', #52391, #123312 ) ;
#7444 = LINE ( 'NONE', #6000, #121250 ) ;
#7445 = DIRECTION ( 'NONE',  ( -0.7071067811865486830, -0.7071067811865464625, -0.000000000000000000 ) ) ;
#7446 = ORIENTED_EDGE ( 'NONE', *, *, #29306, .F. ) ;
#7447 = ADVANCED_FACE ( 'NONE', ( #31665 ), #32383, .T. ) ;
#7448 = ORIENTED_EDGE ( 'NONE', *, *, #35784, .T. ) ;
#7449 = VECTOR ( 'NONE', #80986, 1000.000000000000000 ) ;
#7450 = CARTESIAN_POINT ( 'NONE',  ( 51.18398860626899705, 28.73617430169823095, 5.000000000000000000 ) ) ;
#7451 = LINE ( 'NONE', #142981, #124684 ) ;
#7452 = CARTESIAN_POINT ( 'NONE',  ( 16.02040314143522082, 7.934999999999989839, -2.126176841940961904 ) ) ;
#7453 = PLANE ( 'NONE',  #18056 ) ;
#7454 = EDGE_CURVE ( 'NONE', #127371, #95284, #100551, .T. ) ;
#7455 = DIRECTION ( 'NONE',  ( -0.000000000000000000, 0.000000000000000000, 1.000000000000000000 ) ) ;
#7456 = LINE ( 'NONE', #129981, #14319 ) ;
#7457 = ADVANCED_FACE ( 'NONE', ( #109925 ), #19354, .F. ) ;
#7458 = ORIENTED_EDGE ( 'NONE', *, *, #114540, .T. ) ;
#7459 = DIRECTION ( 'NONE',  ( 0.000000000000000000, 1.000000000000000000, 0.000000000000000000 ) ) ;
#7460 = EDGE_CURVE ( 'NONE', #65672, #20317, #9891, .T. ) ;
#7461 = CARTESIAN_POINT ( 'NONE',  ( 34.92499999999998295, -6.183345613589489531, 4.500000000000000888 ) ) ;
#7462 = LINE ( 'NONE', #64020, #130366 ) ;
#7463 = VECTOR ( 'NONE', #6360, 1000.000000000000000 ) ;
#7464 = VECTOR ( 'NONE', #76490, 1000.000000000000227 ) ;
#7465 = VECTOR ( 'NONE', #76950, 1000.000000000000000 ) ;
#7466 = CARTESIAN_POINT ( 'NONE',  ( 71.99451991528749772, 28.92564299267988304, 4.000000000000000000 ) ) ;
#7467 = EDGE_CURVE ( 'NONE', #142939, #4917, #77345, .T. ) ;
#7468 = CARTESIAN_POINT ( 'NONE',  ( 38.99543019189812298, 5.291415217122917625, 3.055000000000002380 ) ) ;
#7469 = CARTESIAN_POINT ( 'NONE',  ( 16.00193056682086379, -22.22500000000000142, 4.500000000000000888 ) ) ;
#7470 = VECTOR ( 'NONE', #68471, 1000.000000000000000 ) ;
#7471 = VECTOR ( 'NONE', #37741, 1000.000000000000000 ) ;
#7472 = ORIENTED_EDGE ( 'NONE', *, *, #118936, .T. ) ;
#7473 = CARTESIAN_POINT ( 'NONE',  ( -18.72281430457046270, -21.72500000000000142, 5.000000000000000000 ) ) ;
#7474 = ORIENTED_EDGE ( 'NONE', *, *, #37089, .F. ) ;
#7475 = EDGE_CURVE ( 'NONE', #57193, #75539, #20769, .T. ) ;
#7476 = EDGE_LOOP ( 'NONE', ( #45369, #64873, #133284, #73093, #26038 ) ) ;
#7477 = VECTOR ( 'NONE', #73354, 1000.000000000000000 ) ;
#7478 =( GEOMETRIC_REPRESENTATION_CONTEXT ( 3 ) GLOBAL_UNCERTAINTY_ASSIGNED_CONTEXT ( ( #130361 ) ) GLOBAL_UNIT_ASSIGNED_CONTEXT ( ( #90232, #54777, #33049 ) ) REPRESENTATION_CONTEXT ( 'NONE', 'WORKASPACE' ) );
#7479 = CARTESIAN_POINT ( 'NONE',  ( 18.29974487139159223, -27.71228299555219010, 4.000000000000000000 ) ) ;
#7480 = MECHANICAL_DESIGN_GEOMETRIC_PRESENTATION_REPRESENTATION (  '', ( #7580 ), #65486 ) ;
#7481 = DIRECTION ( 'NONE',  ( -0.7071067811865486830, -0.7071067811865464625, -0.000000000000000000 ) ) ;
#7482 = DIRECTION ( 'NONE',  ( 0.7071067811865487940, 0.7071067811865463515, 0.000000000000000000 ) ) ;
#7483 = DIRECTION ( 'NONE',  ( 0.000000000000000000, -1.000000000000000000, 0.000000000000000000 ) ) ;
#7484 = EDGE_CURVE ( 'NONE', #72549, #30937, #132443, .T. ) ;
#7485 = DIRECTION ( 'NONE',  ( 0.3543493200069162685, -0.000000000000000000, -0.9351131265310288487 ) ) ;
#7486 = ADVANCED_FACE ( 'NONE', ( #41103 ), #63606, .F. ) ;
#7487 = DIRECTION ( 'NONE',  ( -0.000000000000000000, 0.3543493200069153248, 0.9351131265310292928 ) ) ;
#7488 = LINE ( 'NONE', #74936, #94016 ) ;
#7489 = ORIENTED_EDGE ( 'NONE', *, *, #8888, .T. ) ;
#7490 = DIRECTION ( 'NONE',  ( 0.3543493200069162685, -0.000000000000000000, -0.9351131265310288487 ) ) ;
#7491 = DIRECTION ( 'NONE',  ( -1.000000000000000000, -1.224606353822377258E-16, -0.000000000000000000 ) ) ;
#7492 = DIRECTION ( 'NONE',  ( -0.3543493200069163240, 0.000000000000000000, 0.9351131265310288487 ) ) ;
#7493 = DIRECTION ( 'NONE',  ( 1.000000000000000000, 0.000000000000000000, 0.000000000000000000 ) ) ;
#7494 = CARTESIAN_POINT ( 'NONE',  ( 32.29289321881324071, 17.25929247661554911, 5.000000000000000000 ) ) ;
#7495 = EDGE_CURVE ( 'NONE', #137044, #55653, #118661, .T. ) ;
#7496 = CARTESIAN_POINT ( 'NONE',  ( 103.6208603837962272, -6.884901960086286188, 3.974999999999997424 ) ) ;
#7497 = CARTESIAN_POINT ( 'NONE',  ( 63.80836038379621300, 7.949999999999997513, 2.130196079827431088 ) ) ;
#7498 = PLANE ( 'NONE',  #22918 ) ;
#7499 = ORIENTED_EDGE ( 'NONE', *, *, #35203, .T. ) ;
#7500 = ORIENTED_EDGE ( 'NONE', *, *, #122510, .F. ) ;
#7501 = CARTESIAN_POINT ( 'NONE',  ( 53.93750000000000000, 5.819803920172573974, -5.819803920172572198 ) ) ;
#7502 = CARTESIAN_POINT ( 'NONE',  ( 0.000000000000000000, 0.000000000000000000, 5.000000000000000000 ) ) ;
#7503 = LINE ( 'NONE', #129285, #64798 ) ;
#7504 = DIRECTION ( 'NONE',  ( 0.6830127018922181881, 0.6830127018922202975, -0.2588190451025214056 ) ) ;
#7505 = VERTEX_POINT ( 'NONE', #75194 ) ;
#7506 = VECTOR ( 'NONE', #38109, 1000.000000000000227 ) ;
#7507 = DIRECTION ( 'NONE',  ( -0.7071067811865486830, 0.7071067811865464625, 0.000000000000000000 ) ) ;
#7508 = CARTESIAN_POINT ( 'NONE',  ( 45.93793019189810423, -6.110000000000001208, 1.637169565754158951 ) ) ;
#7509 = AXIS2_PLACEMENT_3D ( 'NONE', #140453, #141159, #119394 ) ;
#7510 = ORIENTED_EDGE ( 'NONE', *, *, #18748, .T. ) ;
#7511 = EDGE_CURVE ( 'NONE', #72734, #30899, #142576, .T. ) ;
#7512 = DIRECTION ( 'NONE',  ( -0.000000000000000000, 0.3543493200069153248, 0.9351131265310292928 ) ) ;
#7513 = ORIENTED_EDGE ( 'NONE', *, *, #76592, .T. ) ;
#7514 = ORIENTED_EDGE ( 'NONE', *, *, #55601, .F. ) ;
#7515 = VECTOR ( 'NONE', #56621, 1000.000000000000000 ) ;
#7516 = LINE ( 'NONE', #127913, #28455 ) ;
#7517 = LINE ( 'NONE', #53168, #104463 ) ;
#7518 = CARTESIAN_POINT ( 'NONE',  ( 9.299744871391588674, -27.71228299555212971, 4.000000000000000000 ) ) ;
#7519 = DIRECTION ( 'NONE',  ( -0.7071067811865486830, -0.7071067811865464625, 0.000000000000000000 ) ) ;
#7521 = ORIENTED_EDGE ( 'NONE', *, *, #95955, .T. ) ;
#7520 = PLANE ( 'NONE',  #10483 ) ;
#7522 = CARTESIAN_POINT ( 'NONE',  ( 0.000000000000000000, 9.735942053221458872E-16, -7.950000000000000178 ) ) ;
#7523 = DIRECTION ( 'NONE',  ( -0.3543493200069162685, -0.000000000000000000, -0.9351131265310288487 ) ) ;
#7524 = SURFACE_SIDE_STYLE ('',( #131478 ) ) ;
#7525 = LINE ( 'NONE', #42346, #74156 ) ;
#7526 = LINE ( 'NONE', #39484, #25294 ) ;
#7527 = EDGE_CURVE ( 'NONE', #49206, #120930, #140413, .T. ) ;
#7528 = ORIENTED_EDGE ( 'NONE', *, *, #20157, .F. ) ;
#7529 = ORIENTED_EDGE ( 'NONE', *, *, #80269, .F. ) ;
#7530 = CARTESIAN_POINT ( 'NONE',  ( 57.18398860626899705, 28.73617430169827358, 5.000000000000000000 ) ) ;
#7531 = CARTESIAN_POINT ( 'NONE',  ( 79.97459685856479439, 1.637169565754164058, -6.109999999999996767 ) ) ;
#7532 = FACE_OUTER_BOUND ( 'NONE', #66327, .T. ) ;
#7533 = ADVANCED_FACE ( 'NONE', ( #141114 ), #85298, .F. ) ;
#7534 = VECTOR ( 'NONE', #43236, 1000.000000000000227 ) ;
#7535 = CARTESIAN_POINT ( 'NONE',  ( -20.29298673570681544, -21.74070752338406720, 4.999753212805217117 ) ) ;
#7536 = CARTESIAN_POINT ( 'NONE',  ( 153.4000000000000057, -1.600000000000094458, 33.92499999999998295 ) ) ;
#7537 = ORIENTED_EDGE ( 'NONE', *, *, #8071, .T. ) ;
#7538 = VERTEX_POINT ( 'NONE', #86041 ) ;
#7539 = VECTOR ( 'NONE', #100426, 1000.000000000000000 ) ;
#7540 = CARTESIAN_POINT ( 'NONE',  ( 11.70025512860841133, -27.71228299555198049, 4.000000000000000000 ) ) ;
#7541 = SURFACE_STYLE_FILL_AREA ( #18402 ) ;
#7542 = ORIENTED_EDGE ( 'NONE', *, *, #58205, .T. ) ;
#7543 = EDGE_LOOP ( 'NONE', ( #143060, #110285, #140679, #17538 ) ) ;
#7544 = EDGE_CURVE ( 'NONE', #97811, #60787, #141872, .T. ) ;
#7545 = DIRECTION ( 'NONE',  ( -0.7071067811865486830, -0.7071067811865464625, -0.000000000000000000 ) ) ;
#7546 = ORIENTED_EDGE ( 'NONE', *, *, #63364, .F. ) ;
#7547 = LINE ( 'NONE', #108999, #110465 ) ;
#7548 = AXIS2_PLACEMENT_3D ( 'NONE', #43243, #32354, #77321 ) ;
#7549 = FACE_OUTER_BOUND ( 'NONE', #135720, .T. ) ;
#7550 = EDGE_CURVE ( 'NONE', #116840, #20377, #42567, .T. ) ;
#7551 = FACE_BOUND ( 'NONE', #34431, .T. ) ;
#7552 = CARTESIAN_POINT ( 'NONE',  ( -69.18398860626899705, 28.73617430169835529, 5.000000000000000000 ) ) ;
#7553 = CARTESIAN_POINT ( 'NONE',  ( 21.32816939922338406, -9.740707523384177335, 4.000000000000000000 ) ) ;
#7554 = CIRCLE ( 'NONE', #107112, 2.500000000000000888 ) ;
#7555 = CARTESIAN_POINT ( 'NONE',  ( -34.92500000000001137, -4.298069433178936194, 4.500000000000000888 ) ) ;
#7557 = VERTEX_POINT ( 'NONE', #86767 ) ;
#7556 = DIRECTION ( 'NONE',  ( 4.681814790819592407E-17, 0.3543493200069153248, 0.9351131265310292928 ) ) ;
#7558 = CARTESIAN_POINT ( 'NONE',  ( 10.94186803553636977, -2.500000000000001776, 0.000000000000000000 ) ) ;
#7559 = SHAPE_DEFINITION_REPRESENTATION ( #43228, #54265 ) ;
#7560 = ORIENTED_EDGE ( 'NONE', *, *, #106648, .T. ) ;
#7561 = ORIENTED_EDGE ( 'NONE', *, *, #107033, .T. ) ;
#7562 = CARTESIAN_POINT ( 'NONE',  ( 85.51626352523145158, -4.472830434245838482, 4.472830434245838482 ) ) ;
#7563 = EDGE_LOOP ( 'NONE', ( #32025, #104865, #36140, #57891 ) ) ;
#7564 = CARTESIAN_POINT ( 'NONE',  ( 29.20710678118633652, 15.75929247661555443, 5.000000000000000000 ) ) ;
#7565 = FACE_OUTER_BOUND ( 'NONE', #103019, .T. ) ;
#7566 = CARTESIAN_POINT ( 'NONE',  ( 20.36747333860806819, 3.821174125832445049E-16, 0.000000000000000000 ) ) ;
#7567 = VECTOR ( 'NONE', #129232, 1000.000000000000227 ) ;
#7568 = AXIS2_PLACEMENT_3D ( 'NONE', #129958, #64704, #100886 ) ;
#7569 = VECTOR ( 'NONE', #13633, 999.9999999999998863 ) ;
#7570 = CARTESIAN_POINT ( 'NONE',  ( -1.499999999999987566, -17.91344420646042934, 1.358650452708460854 ) ) ;
#7571 = DIRECTION ( 'NONE',  ( 0.7071067811865487940, -0.7071067811865463515, 0.000000000000000000 ) ) ;
#7572 = ADVANCED_FACE ( 'NONE', ( #130989 ), #33131, .T. ) ;
#7573 = DIRECTION ( 'NONE',  ( 0.7071067811865487940, 0.7071067811865463515, 0.000000000000000000 ) ) ;
#7574 = CARTESIAN_POINT ( 'NONE',  ( -32.67183060077623935, -3.740707523384244837, 4.000000000000000000 ) ) ;
#7575 = CARTESIAN_POINT ( 'NONE',  ( -16.82816939922340893, 18.75929247661553134, 4.000000000000000000 ) ) ;
#7576 = DIRECTION ( 'NONE',  ( 0.7071067811865487940, 0.7071067811865463515, 0.000000000000000000 ) ) ;
#7577 = PLANE ( 'NONE',  #43950 ) ;
#7578 = VECTOR ( 'NONE', #52367, 1000.000000000000000 ) ;
#7579 = VECTOR ( 'NONE', #77450, 1000.000000000000000 ) ;
#7580 = STYLED_ITEM ( 'NONE', ( #91899 ), #15274 ) ;
#7581 = DIRECTION ( 'NONE',  ( -0.7071067811865486830, -0.7071067811865464625, -0.000000000000000000 ) ) ;
#7582 = ORIENTED_EDGE ( 'NONE', *, *, #1854, .T. ) ;
#7583 = CARTESIAN_POINT ( 'NONE',  ( 38.99451991528749062, 28.92564299267965211, 4.000000000000000000 ) ) ;
#7584 = LINE ( 'NONE', #20604, #104447 ) ;
#7585 = ORIENTED_EDGE ( 'NONE', *, *, #76580, .F. ) ;
#7586 = ORIENTED_EDGE ( 'NONE', *, *, #30309, .T. ) ;
#7587 = ADVANCED_FACE ( 'NONE', ( #101186 ), #12031, .F. ) ;
#7588 = ORIENTED_EDGE ( 'NONE', *, *, #129288, .T. ) ;
#7589 = CARTESIAN_POINT ( 'NONE',  ( 31.50043019189810423, -3.055000000000002380, 5.291415217122920289 ) ) ;
#7590 = ORIENTED_EDGE ( 'NONE', *, *, #57217, .T. ) ;
#7591 = DIRECTION ( 'NONE',  ( 0.7071067811865487940, 0.7071067811865463515, 0.000000000000000000 ) ) ;
#7592 = VECTOR ( 'NONE', #121405, 1000.000000000000000 ) ;
#7593 = CARTESIAN_POINT ( 'NONE',  ( 15.64997294953710671, -4.461849672132299105, 4.461849672132299993 ) ) ;
#7594 = CARTESIAN_POINT ( 'NONE',  ( 13.55929415207057076, 9.045080515339410709, -27.46719384617228243 ) ) ;
#7595 = VERTEX_POINT ( 'NONE', #13441 ) ;
#7596 = CARTESIAN_POINT ( 'NONE',  ( 36.18398860626899705, 28.73617430169812437, 5.000000000000000000 ) ) ;
#7597 = ORIENTED_EDGE ( 'NONE', *, *, #93848, .F. ) ;
#7598 = PLANE ( 'NONE',  #78941 ) ;
#7599 = DIRECTION ( 'NONE',  ( -1.000000000000000000, 0.000000000000000000, -0.000000000000000000 ) ) ;
#7601 = ORIENTED_EDGE ( 'NONE', *, *, #20023, .T. ) ;
#7600 = CARTESIAN_POINT ( 'NONE',  ( 9.299744871391588674, -27.71228299555212971, 4.000000000000000000 ) ) ;
#7602 = VERTEX_POINT ( 'NONE', #102643 ) ;
#7603 = EDGE_CURVE ( 'NONE', #125282, #62063, #70046, .T. ) ;
#7604 = DIRECTION ( 'NONE',  ( -0.7071067811865486830, -0.7071067811865464625, 0.000000000000000000 ) ) ;
#7605 = VECTOR ( 'NONE', #41858, 999.9999999999998863 ) ;
#7606 = ORIENTED_EDGE ( 'NONE', *, *, #6615, .T. ) ;
#7607 = LINE ( 'NONE', #13315, #119864 ) ;
#7608 = VERTEX_POINT ( 'NONE', #45423 ) ;
#7609 = PRODUCT ( '1.1 Sliding Jaw', '1.1 Sliding Jaw', '', ( #61303 ) ) ;
#7610 = ORIENTED_EDGE ( 'NONE', *, *, #84921, .F. ) ;
#7611 = VECTOR ( 'NONE', #127844, 1000.000000000000000 ) ;
#7612 = EDGE_LOOP ( 'NONE', ( #38070, #57452, #10904, #31312 ) ) ;
#7613 = CARTESIAN_POINT ( 'NONE',  ( 2.999999999999999112, 3.061616997868383141E-16, -2.500000000000000000 ) ) ;
#7614 = LINE ( 'NONE', #119237, #53810 ) ;
#7615 = CARTESIAN_POINT ( 'NONE',  ( 34.47516574401891631, 0.02806734111581514132, 4.998110765256834398 ) ) ;
#7616 = DIRECTION ( 'NONE',  ( -0.7071067811865486830, -0.7071067811865464625, 0.000000000000000000 ) ) ;
#7617 = DIRECTION ( 'NONE',  ( -0.7071067811865487940, 0.7071067811865463515, -0.000000000000000000 ) ) ;
#7618 = ORIENTED_EDGE ( 'NONE', *, *, #116171, .F. ) ;
#7619 = LINE ( 'NONE', #140301, #90475 ) ;
#7620 = ORIENTED_EDGE ( 'NONE', *, *, #139462, .T. ) ;
#7621 = DIRECTION ( 'NONE',  ( 0.6830127018922180770, -0.6830127018922204085, -0.2588190451025213501 ) ) ;
#7622 = AXIS2_PLACEMENT_3D ( 'NONE', #98586, #142815, #41344 ) ;
#7623 = CARTESIAN_POINT ( 'NONE',  ( 30.02040314143521726, 7.934999999999989839, -2.126176841940961904 ) ) ;
#7624 = LINE ( 'NONE', #10309, #113355 ) ;
#7625 = EDGE_CURVE ( 'NONE', #84565, #129451, #56316, .T. ) ;
#7626 = VERTEX_POINT ( 'NONE', #112781 ) ;
#7627 = CARTESIAN_POINT ( 'NONE',  ( -51.29974487139158867, -27.71228299555242103, 4.000000000000000000 ) ) ;
#7628 = CARTESIAN_POINT ( 'NONE',  ( -30.32816939922330945, 5.259292476615672562, 4.000000000000000000 ) ) ;
#7629 = ORIENTED_EDGE ( 'NONE', *, *, #57360, .T. ) ;
#7630 = EDGE_CURVE ( 'NONE', #130905, #110484, #99761, .T. ) ;
#7631 = ORIENTED_EDGE ( 'NONE', *, *, #11156, .T. ) ;
#7632 = VECTOR ( 'NONE', #125080, 1000.000000000000000 ) ;
#7633 = ORIENTED_EDGE ( 'NONE', *, *, #11134, .T. ) ;
#7634 = CARTESIAN_POINT ( 'NONE',  ( -48.48921356237309510, -27.52281430457089328, 5.000000000000000000 ) ) ;
#7635 = DIRECTION ( 'NONE',  ( -0.6830127018922180770, -0.6830127018922204085, -0.2588190451025213501 ) ) ;
#7636 = DIRECTION ( 'NONE',  ( -0.7071067811865487940, 0.7071067811865463515, -0.000000000000000000 ) ) ;
#7637 = AXIS2_PLACEMENT_3D ( 'NONE', #26080, #92734, #128251 ) ;
#7638 = DIRECTION ( 'NONE',  ( -0.3543493200069162685, -0.000000000000000000, -0.9351131265310288487 ) ) ;
#7639 = CARTESIAN_POINT ( 'NONE',  ( 0.5414528859221161561, -52.10163751122234999, -40.43817685073778279 ) ) ;
#7640 = EDGE_CURVE ( 'NONE', #77421, #129881, #80190, .T. ) ;
#7642 = ADVANCED_FACE ( 'NONE', ( #23633 ), #78741, .F. ) ;
#7641 = CARTESIAN_POINT ( 'NONE',  ( 73.26626352523143737, 4.472830434245839371, -4.472830434245839371 ) ) ;
#7643 =( BOUNDED_CURVE ( )  B_SPLINE_CURVE ( 3, ( #20874, #109329, #44087, #41206 ),
 .UNSPECIFIED., .F., .F. ) 
 B_SPLINE_CURVE_WITH_KNOTS ( ( 4, 4 ),
 ( 1.208578181583236821, 1.359146454359482892 ),
 .UNSPECIFIED. ) 
 CURVE ( )  GEOMETRIC_REPRESENTATION_ITEM ( )  RATIONAL_B_SPLINE_CURVE ( ( 1.000000000000000000, 0.9981116584018941973, 0.9981116584018941973, 1.000000000000000000 ) ) 
 REPRESENTATION_ITEM ( '' )  );
#7644 = CARTESIAN_POINT ( 'NONE',  ( 73.57919371712957002, 3.975000000000002753, -6.884901960086283523 ) ) ;
#7645 = CARTESIAN_POINT ( 'NONE',  ( -25.49999999999982236, -2.947814304570797184, 5.000000000000000000 ) ) ;
#7646 = DIRECTION ( 'NONE',  ( -0.000000000000000000, 0.3543493200069153248, 0.9351131265310292928 ) ) ;
#7647 = DIRECTION ( 'NONE',  ( 0.000000000000000000, -2.556434596176436521E-15, -1.000000000000000000 ) ) ;
#7648 = ORIENTED_EDGE ( 'NONE', *, *, #120810, .T. ) ;
#7649 = CARTESIAN_POINT ( 'NONE',  ( -17.82446237275610201, 9.017796866808286183, 4.672399651904014739 ) ) ;
#7650 = ORIENTED_EDGE ( 'NONE', *, *, #17910, .F. ) ;
#7651 = COLOUR_RGB ( '', 0.08235294, 0.09019608, 0.10196078) ;
#7652 = LINE ( 'NONE', #48496, #119516 ) ;
#7653 = DIRECTION ( 'NONE',  ( -0.6830127018922180770, -0.6830127018922204085, -0.2588190451025213501 ) ) ;
#7654 = ORIENTED_EDGE ( 'NONE', *, *, #95997, .F. ) ;
#7655 =( BOUNDED_CURVE ( )  B_SPLINE_CURVE ( 3, ( #34854, #14505, #124695, #135590 ),
 .UNSPECIFIED., .F., .F. ) 
 B_SPLINE_CURVE_WITH_KNOTS ( ( 4, 4 ),
 ( 5.106027341939272546, 6.645403452391245303 ),
 .UNSPECIFIED. ) 
 CURVE ( )  GEOMETRIC_REPRESENTATION_ITEM ( )  RATIONAL_B_SPLINE_CURVE ( ( 1.000000000000000000, 0.8120851936182260644, 0.8120851936182260644, 1.000000000000000000 ) ) 
 REPRESENTATION_ITEM ( '' )  );
#7656 = LINE ( 'NONE', #117131, #120198 ) ;
#7658 = VERTEX_POINT ( 'NONE', #133831 ) ;
#7657 = CARTESIAN_POINT ( 'NONE',  ( -34.49999999999974420, -17.94567065516885762, 4.994342998332165884 ) ) ;
#7659 = ADVANCED_FACE ( 'NONE', ( #89599 ), #137426, .T. ) ;
#7660 = ADVANCED_FACE ( 'NONE', ( #123692 ), #57717, .T. ) ;
#7661 = DIRECTION ( 'NONE',  ( 1.000000000000000000, 0.000000000000000000, 0.000000000000000000 ) ) ;
#7662 = CARTESIAN_POINT ( 'NONE',  ( 0.000000000000000000, 0.000000000000000000, 0.000000000000000000 ) ) ;
#7663 = ORIENTED_EDGE ( 'NONE', *, *, #89794, .F. ) ;
#7665 = ORIENTED_EDGE ( 'NONE', *, *, #113714, .F. ) ;
#7664 = VECTOR ( 'NONE', #126113, 999.9999999999998863 ) ;
#7666 = FILL_AREA_STYLE_COLOUR ( '', #90669 ) ;
#7667 = DIRECTION ( 'NONE',  ( -3.166071393695993333E-32, 1.016133275908817741E-16, -1.000000000000000000 ) ) ;
#7668 = CARTESIAN_POINT ( 'NONE',  ( -24.18398860626899705, 28.73617430169804265, 5.000000000000000000 ) ) ;
#7669 = EDGE_CURVE ( 'NONE', #64185, #81832, #33817, .T. ) ;
#7670 = CARTESIAN_POINT ( 'NONE',  ( 93.41252705046289861, -7.949999999999998401, -4.867971026610728450E-16 ) ) ;
#7671 = CARTESIAN_POINT ( 'NONE',  ( 9.792893218813391698, -11.24070752338417201, 5.000000000000000000 ) ) ;
#7672 = CARTESIAN_POINT ( 'NONE',  ( 34.75611968250419181, -10.29434930147584737, 4.955485411084881164 ) ) ;
#7673 = ORIENTED_EDGE ( 'NONE', *, *, #37426, .F. ) ;
#7674 = DIRECTION ( 'NONE',  ( -0.7071067811865487940, 0.7071067811865463515, -0.000000000000000000 ) ) ;
#7675 = CARTESIAN_POINT ( 'NONE',  ( 24.79333936457830134, 21.75929247661549226, 4.998822639870711626 ) ) ;
#7676 = CARTESIAN_POINT ( 'NONE',  ( 28.43750000000000355, -4.461849672132299105, 4.461849672132299993 ) ) ;
#7677 = EDGE_CURVE ( 'NONE', #10831, #136292, #112090, .T. ) ;
#7678 = CARTESIAN_POINT ( 'NONE',  ( 1.001930566820972812, -22.22500000000000142, 4.500000000000000888 ) ) ;
#7679 = ORIENTED_EDGE ( 'NONE', *, *, #62664, .T. ) ;
#7680 = VECTOR ( 'NONE', #110991, 1000.000000000000227 ) ;
#7681 = CARTESIAN_POINT ( 'NONE',  ( -18.18398860626898994, 28.73617430169800002, 5.000000000000000000 ) ) ;
#7682 = ORIENTED_EDGE ( 'NONE', *, *, #128705, .T. ) ;
#7683 = CARTESIAN_POINT ( 'NONE',  ( 82.97959685856476142, 6.109999999999999432, 1.637169565754164280 ) ) ;
#7684 = FACE_OUTER_BOUND ( 'NONE', #66904, .T. ) ;
#7685 = ADVANCED_FACE ( 'NONE', ( #3290 ), #78038, .F. ) ;
#7687 = CARTESIAN_POINT ( 'NONE',  ( -32.99999999999977263, -2.904428200921339354, -6.989807076074864511 ) ) ;
#7686 = CIRCLE ( 'NONE', #125798, 5.999999999999998224 ) ;
#7688 = STYLED_ITEM ( 'NONE', ( #107757 ), #129565 ) ;
#7689 = ORIENTED_EDGE ( 'NONE', *, *, #140447, .T. ) ;
#7690 = FACE_OUTER_BOUND ( 'NONE', #19599, .T. ) ;
#7691 = AXIS2_PLACEMENT_3D ( 'NONE', #71116, #49376, #60239 ) ;
#7692 = CARTESIAN_POINT ( 'NONE',  ( 31.49999999999977973, 22.01701374228158059, 2.453858888625559231 ) ) ;
#7693 = CARTESIAN_POINT ( 'NONE',  ( 27.18398860626900060, 28.73617430169806042, 5.000000000000000000 ) ) ;
#7695 = ORIENTED_EDGE ( 'NONE', *, *, #54600, .T. ) ;
#7694 = CARTESIAN_POINT ( 'NONE',  ( -14.56453960929607128, -0.7633378608190106718, 4.223415947001583959 ) ) ;
#7696 = DIRECTION ( 'NONE',  ( 0.7071067811865487940, 0.7071067811865463515, 0.000000000000000000 ) ) ;
#7697 = CARTESIAN_POINT ( 'NONE',  ( 15.96626304157554266, 4.202752102959690472E-16, 0.000000000000000000 ) ) ;
#7698 = DIRECTION ( 'NONE',  ( 1.000000000000000000, 0.000000000000000000, 0.000000000000000000 ) ) ;
#7699 = CARTESIAN_POINT ( 'NONE',  ( 60.50000000000000000, 0.000000000000000000, -7.950000000000000178 ) ) ;
#7700 = ORIENTED_EDGE ( 'NONE', *, *, #105022, .F. ) ;
#7701 = EDGE_CURVE ( 'NONE', #93695, #25745, #34513, .T. ) ;
#7702 = ORIENTED_EDGE ( 'NONE', *, *, #78552, .T. ) ;
#7703 = CARTESIAN_POINT ( 'NONE',  ( 69.27126352523144703, 4.472830434245839371, 4.472830434245842035 ) ) ;
#7704 = AXIS2_PLACEMENT_3D ( 'NONE', #139289, #97135, #138553 ) ;
#7705 = ORIENTED_EDGE ( 'NONE', *, *, #115101, .T. ) ;
#7706 = FACE_OUTER_BOUND ( 'NONE', #28715, .T. ) ;
#7707 = DIRECTION ( 'NONE',  ( -1.000000000000000000, -0.000000000000000000, -0.000000000000000000 ) ) ;
#7708 = CARTESIAN_POINT ( 'NONE',  ( 33.29974487139158867, -27.71228299555229313, 4.000000000000000000 ) ) ;
#7709 = FACE_OUTER_BOUND ( 'NONE', #68074, .T. ) ;
#7710 = VERTEX_POINT ( 'NONE', #47576 ) ;
#7711 = CARTESIAN_POINT ( 'NONE',  ( -12.69999999999998153, 0.000000000000000000, 2.500000000000000444 ) ) ;
#7712 = CARTESIAN_POINT ( 'NONE',  ( 36.29974487139159578, -27.71228299555231445, 4.000000000000000000 ) ) ;
#7713 = VECTOR ( 'NONE', #122807, 1000.000000000000114 ) ;
#7714 = ORIENTED_EDGE ( 'NONE', *, *, #38022, .F. ) ;
#7715 = AXIS2_PLACEMENT_3D ( 'NONE', #14527, #68243, #113111 ) ;
#7716 = EDGE_CURVE ( 'NONE', #134224, #88846, #12739, .T. ) ;
#7717 = PLANE ( 'NONE',  #69869 ) ;
#7718 = DIRECTION ( 'NONE',  ( -1.000000000000000000, -1.224606353822377258E-16, -0.000000000000000000 ) ) ;
#7719 = DIRECTION ( 'NONE',  ( -0.6830127018922181881, 0.6830127018922202975, -0.2588190451025214056 ) ) ;
#7720 = ORIENTED_EDGE ( 'NONE', *, *, #126600, .F. ) ;
#7722 = ORIENTED_EDGE ( 'NONE', *, *, #12563, .F. ) ;
#7721 = VECTOR ( 'NONE', #102528, 1000.000000000000000 ) ;
#7723 = EDGE_CURVE ( 'NONE', #61774, #140269, #90312, .T. ) ;
#7724 = FACE_BOUND ( 'NONE', #57182, .T. ) ;
#7725 = DIRECTION ( 'NONE',  ( 0.3543493200069162685, -0.000000000000000000, -0.9351131265310288487 ) ) ;
#7726 = DIRECTION ( 'NONE',  ( -0.7071067811865486830, -0.7071067811865464625, 0.000000000000000000 ) ) ;
#7727 = CYLINDRICAL_SURFACE ( 'NONE', #82768, 0.5000000000000004441 ) ;
#7728 = VECTOR ( 'NONE', #67904, 1000.000000000000000 ) ;
#7729 = CARTESIAN_POINT ( 'NONE',  ( -3.589048004105921397E-14, -0.6000000000000001998, 3.226849613583692822 ) ) ;
#7730 = ORIENTED_EDGE ( 'NONE', *, *, #124158, .T. ) ;
#7731 = VECTOR ( 'NONE', #141753, 1000.000000000000227 ) ;
#7732 = ORIENTED_EDGE ( 'NONE', *, *, #135394, .T. ) ;
#7733 = ORIENTED_EDGE ( 'NONE', *, *, #80802, .T. ) ;
#7734 = ORIENTED_EDGE ( 'NONE', *, *, #61915, .F. ) ;
#7735 = AXIS2_PLACEMENT_3D ( 'NONE', #137526, #59280, #4799 ) ;
#7736 = CARTESIAN_POINT ( 'NONE',  ( 180.4193221990230143, -49.14999999999999147, 40.92499999999998295 ) ) ;
#7737 = DIRECTION ( 'NONE',  ( -0.7071067811865486830, -0.7071067811865464625, 0.000000000000000000 ) ) ;
#7738 = FACE_OUTER_BOUND ( 'NONE', #44858, .T. ) ;
#7739 = ORIENTED_EDGE ( 'NONE', *, *, #122105, .F. ) ;
#7740 = DIRECTION ( 'NONE',  ( 0.7071067811865487940, 0.7071067811865463515, -0.000000000000000000 ) ) ;
#7741 = LINE ( 'NONE', #76623, #79776 ) ;
#7742 = EDGE_CURVE ( 'NONE', #92118, #78177, #91062, .T. ) ;
#7743 = LINE ( 'NONE', #96176, #73525 ) ;
#7744 = DIRECTION ( 'NONE',  ( -0.000000000000000000, -0.000000000000000000, 1.000000000000000000 ) ) ;
#7745 = AXIS2_PLACEMENT_3D ( 'NONE', #132305, #75763, #98908 ) ;
#7746 = CARTESIAN_POINT ( 'NONE',  ( 27.00000000000001421, -7.661656307529537635, -1.660001620851698112 ) ) ;
#7747 = ORIENTED_EDGE ( 'NONE', *, *, #24735, .T. ) ;
#7748 = CARTESIAN_POINT ( 'NONE',  ( 122.6835989386367345, -57.15000000000009095, 34.92499999999998295 ) ) ;
#7749 = DIRECTION ( 'NONE',  ( 1.000000000000000000, 0.000000000000000000, 0.000000000000000000 ) ) ;
#7750 = EDGE_LOOP ( 'NONE', ( #114604, #82815, #61346, #128148 ) ) ;
#7751 = EDGE_CURVE ( 'NONE', #32796, #72863, #135283, .T. ) ;
#7752 = CARTESIAN_POINT ( 'NONE',  ( -34.75611968250420603, 20.81293425470715519, 4.955485411084898040 ) ) ;
#7753 = ORIENTED_EDGE ( 'NONE', *, *, #21670, .F. ) ;
#7755 = EDGE_CURVE ( 'NONE', #96557, #93700, #93879, .T. ) ;
#7754 = FACE_OUTER_BOUND ( 'NONE', #7785, .T. ) ;
#7756 = ORIENTED_EDGE ( 'NONE', *, *, #44182, .F. ) ;
#7757 = AXIS2_PLACEMENT_3D ( 'NONE', #135921, #79454, #24304 ) ;
#7758 = CARTESIAN_POINT ( 'NONE',  ( 64.16709685856476142, -3.055000000000000160, -5.291415217122921177 ) ) ;
#7759 = VERTEX_POINT ( 'NONE', #14890 ) ;
#7760 = ORIENTED_EDGE ( 'NONE', *, *, #117657, .F. ) ;
#7761 = CARTESIAN_POINT ( 'NONE',  ( -34.42500000000001137, -7.458600742197909916, 5.000000000000000000 ) ) ;
#7762 = ADVANCED_FACE ( 'NONE', ( #81614 ), #60586, .F. ) ;
#7763 = AXIS2_PLACEMENT_3D ( 'NONE', #60790, #83215, #104951 ) ;
#7764 = CARTESIAN_POINT ( 'NONE',  ( -32.99999999999977263, 1.761378380278653344, -6.096875308897330648 ) ) ;
#7765 = CARTESIAN_POINT ( 'NONE',  ( 103.6879301918981042, 6.110000000000002984, -1.637169565754156730 ) ) ;
#7766 = EDGE_CURVE ( 'NONE', #120604, #47491, #17723, .T. ) ;
#7767 = DIRECTION ( 'NONE',  ( 1.000000000000000000, 0.000000000000000000, 0.000000000000000000 ) ) ;
#7768 = DIRECTION ( 'NONE',  ( -0.7071067811865487940, 0.7071067811865463515, 0.000000000000000000 ) ) ;
#7769 = DIRECTION ( 'NONE',  ( -0.6830127018922181881, 0.6830127018922202975, -0.2588190451025214056 ) ) ;
#7770 = CARTESIAN_POINT ( 'NONE',  ( -54.29974487139159578, -27.71228299555243879, 4.000000000000000000 ) ) ;
#7771 = EDGE_CURVE ( 'NONE', #70901, #70593, #37375, .T. ) ;
#7772 = AXIS2_PLACEMENT_3D ( 'NONE', #89803, #55779, #56526 ) ;
#7773 = LINE ( 'NONE', #120824, #102307 ) ;
#7774 = LINE ( 'NONE', #129562, #116916 ) ;
#7775 = VERTEX_POINT ( 'NONE', #26495 ) ;
#7776 =( LENGTH_UNIT ( ) NAMED_UNIT ( * ) SI_UNIT ( .MILLI., .METRE. ) );
#7777 = CARTESIAN_POINT ( 'NONE',  ( 0.7307956238753654521, 0.4000000000000001887, -2.467792535850613866 ) ) ;
#7778 = ORIENTED_EDGE ( 'NONE', *, *, #37463, .F. ) ;
#7779 = ORIENTED_EDGE ( 'NONE', *, *, #81065, .T. ) ;
#7780 = ORIENTED_EDGE ( 'NONE', *, *, #26217, .T. ) ;
#7781 = EDGE_LOOP ( 'NONE', ( #123137, #2024, #58597, #97637 ) ) ;
#7782 = LINE ( 'NONE', #73094, #134749 ) ;
#7783 = FACE_OUTER_BOUND ( 'NONE', #3489, .T. ) ;
#7784 = CARTESIAN_POINT ( 'NONE',  ( 6.707106781186501721, -0.7407075233842770334, 5.000000000000000000 ) ) ;
#7785 = EDGE_LOOP ( 'NONE', ( #14242, #138122, #111563, #82137 ) ) ;
#7786 = CARTESIAN_POINT ( 'NONE',  ( 3.100164867288737636, -48.63026969829241608, 38.45492102172730142 ) ) ;
#7787 = VERTEX_POINT ( 'NONE', #61315 ) ;
#7788 = VECTOR ( 'NONE', #14367, 999.9999999999998863 ) ;
#7789 = VECTOR ( 'NONE', #47150, 1000.000000000000000 ) ;
#7790 = CARTESIAN_POINT ( 'NONE',  ( 8.291236474768552966, -9.717572351234235426E-16, -7.934999999999990727 ) ) ;
#7791 = DIRECTION ( 'NONE',  ( -0.7071067811865486830, -0.7071067811865464625, 0.000000000000000000 ) ) ;
#7792 = EDGE_CURVE ( 'NONE', #1886, #40019, #59162, .T. ) ;
#7793 = PLANE ( 'NONE',  #122359 ) ;
#7794 = CARTESIAN_POINT ( 'NONE',  ( 34.49999999999975131, 9.054329344830847504, 4.994342998332164107 ) ) ;
#7795 = ORIENTED_EDGE ( 'NONE', *, *, #111759, .F. ) ;
#7796 = EDGE_CURVE ( 'NONE', #62812, #81522, #51754, .T. ) ;
#7797 = VERTEX_POINT ( 'NONE', #128659 ) ;
#7798 = ORIENTED_EDGE ( 'NONE', *, *, #133031, .F. ) ;
#7799 = CARTESIAN_POINT ( 'NONE',  ( 0.000000000000000000, 0.000000000000000000, 5.000000000000000000 ) ) ;
#7800 = CARTESIAN_POINT ( 'NONE',  ( 10.06000000000000050, 9.521314400968980422E-16, 0.000000000000000000 ) ) ;
#7801 = DIRECTION ( 'NONE',  ( -0.7071067811865486830, -0.7071067811865464625, 0.000000000000000000 ) ) ;
#7802 =( NAMED_UNIT ( * ) SI_UNIT ( $, .STERADIAN. ) SOLID_ANGLE_UNIT ( ) );
#7803 = AXIS2_PLACEMENT_3D ( 'NONE', #62563, #49568, #50260 ) ;
#7804 = PLANE ( 'NONE',  #106104 ) ;
#7805 = EDGE_CURVE ( 'NONE', #106932, #35816, #93175, .T. ) ;
#7806 = EDGE_CURVE ( 'NONE', #70774, #125073, #29331, .T. ) ;
#7807 = CARTESIAN_POINT ( 'NONE',  ( -36.29974487139159578, -27.71228299555231445, 4.000000000000000000 ) ) ;
#7808 = DIRECTION ( 'NONE',  ( 0.7071067811865487940, 0.7071067811865463515, 0.000000000000000000 ) ) ;
#7809 = DIRECTION ( 'NONE',  ( -0.7071067811865486830, 0.7071067811865464625, 0.000000000000000000 ) ) ;
#7810 = VECTOR ( 'NONE', #71141, 1000.000000000000000 ) ;
#7811 = CARTESIAN_POINT ( 'NONE',  ( 25.95876352523143638, 0.000000000000000000, -6.110000000000001208 ) ) ;
#7812 = SURFACE_STYLE_USAGE ( .BOTH. , #139074 ) ;
#7813 = CARTESIAN_POINT ( 'NONE',  ( -17.99451991528748351, 28.92564299267950645, 4.000000000000000000 ) ) ;
#7814 = VERTEX_POINT ( 'NONE', #28652 ) ;
#7815 = CARTESIAN_POINT ( 'NONE',  ( 11.51078643762690490, -27.52281430457047406, 5.000000000000000000 ) ) ;
#7816 = CARTESIAN_POINT ( 'NONE',  ( -23.79027397808395250, -22.22500000000000142, 9.219363927620312538 ) ) ;
#7817 = EDGE_LOOP ( 'NONE', ( #25721, #109358, #12975, #18997 ) ) ;
#7818 = AXIS2_PLACEMENT_3D ( 'NONE', #93770, #106765, #116234 ) ;
#7819 = CARTESIAN_POINT ( 'NONE',  ( 27.18398860626900060, 28.73617430169806042, 5.000000000000000000 ) ) ;
#7821 = VERTEX_POINT ( 'NONE', #72905 ) ;
#7820 = CARTESIAN_POINT ( 'NONE',  ( 56.00844637038503748, -48.60795469097138977, -38.18754904900253422 ) ) ;
#7822 = ADVANCED_FACE ( 'NONE', ( #62001 ), #106157, .F. ) ;
#7823 = VECTOR ( 'NONE', #115282, 1000.000000000000000 ) ;
#7824 = EDGE_CURVE ( 'NONE', #28405, #12698, #116354, .T. ) ;
#7825 = CARTESIAN_POINT ( 'NONE',  ( 15.29974487139158867, -27.71228299555216879, 4.000000000000000000 ) ) ;
#7826 = LINE ( 'NONE', #73820, #62400 ) ;
#7827 = ORIENTED_EDGE ( 'NONE', *, *, #39811, .T. ) ;
#7828 = CARTESIAN_POINT ( 'NONE',  ( -19.40370036533107978, 9.134293891043357760, 4.529189151624868792 ) ) ;
#7829 = ORIENTED_EDGE ( 'NONE', *, *, #34468, .T. ) ;
#7830 =( BOUNDED_CURVE ( )  B_SPLINE_CURVE ( 2, ( #118274, #18981, #63246, #8075, #52317, #75513, #119683, #64627, #53775, #97976, #135604, #44331, #113113 ),
 .UNSPECIFIED., .F., .T. ) 
 B_SPLINE_CURVE_WITH_KNOTS ( ( 3, 2, 2, 2, 2, 2, 3 ),
 ( 0.4666666666666666741, 0.4694444444444444420, 0.4722222222222222099, 0.4749999999999999778, 0.4777777777777778012, 0.4805555555555555691, 0.4833333333333333370 ),
 .UNSPECIFIED. ) 
 CURVE ( )  GEOMETRIC_REPRESENTATION_ITEM ( )  RATIONAL_B_SPLINE_CURVE ( ( 1.000000000000000000, 0.9659258262890683122, 1.000000000000000000, 0.9659258262890683122, 1.000000000000000000, 0.9659258262890683122, 1.000000000000000000, 0.9659258262890683122, 1.000000000000000000, 0.9659258262890683122, 1.000000000000000000, 0.9659258262890683122, 1.000000000000000000 ) ) 
 REPRESENTATION_ITEM ( '' )  );
#7831 = VECTOR ( 'NONE', #119538, 1000.000000000000000 ) ;
#7832 = CARTESIAN_POINT ( 'NONE',  ( -16.49999999999988276, -2.568876922607790103, 4.000000000000000000 ) ) ;
#7833 = CARTESIAN_POINT ( 'NONE',  ( 121.1208603837962272, -6.884901960086286188, 3.974999999999997424 ) ) ;
#7835 = AXIS2_PLACEMENT_3D ( 'NONE', #110119, #33341, #123180 ) ;
#7834 = CARTESIAN_POINT ( 'NONE',  ( 7.499999999999954703, 13.08746187583911080, 4.000000000000000000 ) ) ;
#7836 = EDGE_CURVE ( 'NONE', #80414, #99670, #92430, .T. ) ;
#7837 = DIRECTION ( 'NONE',  ( -0.6830127018922180770, -0.6830127018922204085, -0.2588190451025213501 ) ) ;
#7838 = CARTESIAN_POINT ( 'NONE',  ( -1.968364840778075830, 2.259292476615697876, 13.77329220150636679 ) ) ;
#7839 = DIRECTION ( 'NONE',  ( -0.3543493200069162685, -0.000000000000000000, -0.9351131265310288487 ) ) ;
#7840 = CARTESIAN_POINT ( 'NONE',  ( 3.500000000000000444, 0.000000000000000000, 6.094999999999989981 ) ) ;
#7841 = CARTESIAN_POINT ( 'NONE',  ( 7.416236474768552078, -7.934999999999990727, 4.858786175617117713E-16 ) ) ;
#7842 = VECTOR ( 'NONE', #140337, 1000.000000000000000 ) ;
#7843 = EDGE_CURVE ( 'NONE', #64319, #22146, #125819, .T. ) ;
#7844 = CARTESIAN_POINT ( 'NONE',  ( 0.000000000000000000, 0.000000000000000000, 5.000000000000000000 ) ) ;
#7845 = FACE_OUTER_BOUND ( 'NONE', #99963, .T. ) ;
#7846 = ORIENTED_EDGE ( 'NONE', *, *, #46607, .F. ) ;
#7847 = EDGE_LOOP ( 'NONE', ( #125342, #6942, #130844, #99135 ) ) ;
#7848 = DIRECTION ( 'NONE',  ( 0.000000000000000000, 0.000000000000000000, 1.000000000000000000 ) ) ;
#7849 = ORIENTED_EDGE ( 'NONE', *, *, #10496, .T. ) ;
#7850 = DIRECTION ( 'NONE',  ( 0.7071067811865486830, -0.7071067811865464625, -0.000000000000000000 ) ) ;
#7851 = DIRECTION ( 'NONE',  ( -0.7071067811865486830, -0.7071067811865464625, 0.000000000000000000 ) ) ;
#7853 = EDGE_CURVE ( 'NONE', #58791, #30060, #70307, .T. ) ;
#7852 = AXIS2_PLACEMENT_3D ( 'NONE', #51344, #60824, #86106 ) ;
#7854 = CARTESIAN_POINT ( 'NONE',  ( 9.489213562373095101, -27.52281430457062328, 5.000000000000000000 ) ) ;
#7855 = ORIENTED_EDGE ( 'NONE', *, *, #65775, .F. ) ;
#7856 = CARTESIAN_POINT ( 'NONE',  ( 54.18398860626899705, 28.73617430169825226, 5.000000000000000000 ) ) ;
#7857 = LINE ( 'NONE', #107871, #81325 ) ;
#7858 = DIRECTION ( 'NONE',  ( -0.7071067811865487940, 0.7071067811865463515, -0.000000000000000000 ) ) ;
#7859 = CARTESIAN_POINT ( 'NONE',  ( 15.48921356237309510, -27.52281430457066236, 5.000000000000000000 ) ) ;
#7861 = ORIENTED_EDGE ( 'NONE', *, *, #134555, .F. ) ;
#7860 = CARTESIAN_POINT ( 'NONE',  ( 22.49999999999984368, 12.43112307739206024, 4.000000000000000000 ) ) ;
#7862 = EDGE_CURVE ( 'NONE', #33632, #30495, #104012, .T. ) ;
#7863 = CARTESIAN_POINT ( 'NONE',  ( -27.48921356237309155, -27.52281430457074762, 5.000000000000000000 ) ) ;
#7864 = DIRECTION ( 'NONE',  ( 0.7071067811865487940, -0.7071067811865463515, 0.000000000000000000 ) ) ;
#7865 = FACE_OUTER_BOUND ( 'NONE', #45675, .T. ) ;
#7866 = PLANE ( 'NONE',  #1196 ) ;
#7867 = CARTESIAN_POINT ( 'NONE',  ( 59.09089496824217491, -46.71325913968129129, 35.40428284070832632 ) ) ;
#7868 = ORIENTED_EDGE ( 'NONE', *, *, #78693, .T. ) ;
#7869 = EDGE_CURVE ( 'NONE', #109630, #139077, #139572, .T. ) ;
#7870 = ORIENTED_EDGE ( 'NONE', *, *, #96785, .F. ) ;
#7871 = VERTEX_POINT ( 'NONE', #50396 ) ;
#7872 = CARTESIAN_POINT ( 'NONE',  ( 97.27126352523143282, 4.472830434245839371, 4.472830434245842035 ) ) ;
#7873 = VECTOR ( 'NONE', #82886, 1000.000000000000000 ) ;
#7874 = ORIENTED_EDGE ( 'NONE', *, *, #129606, .F. ) ;
#7875 = CARTESIAN_POINT ( 'NONE',  ( 21.52400138585433709, 22.03583458319438293, 4.979811245910091166 ) ) ;
#7876 = CARTESIAN_POINT ( 'NONE',  ( -48.18398860626899705, 28.73617430169820608, 5.000000000000000000 ) ) ;
#7877 = ORIENTED_EDGE ( 'NONE', *, *, #85540, .T. ) ;
#7878 = ADVANCED_FACE ( 'NONE', ( #38099 ), #40255, .F. ) ;
#7879 = PLANE ( 'NONE',  #134773 ) ;
#7881 = VECTOR ( 'NONE', #94415, 1000.000000000000000 ) ;
#7880 = LINE ( 'NONE', #84753, #76770 ) ;
#7882 = CARTESIAN_POINT ( 'NONE',  ( 96.59959685856476597, -6.109999999999997655, -1.637169565754160283 ) ) ;
#7883 = ORIENTED_EDGE ( 'NONE', *, *, #73302, .F. ) ;
#7884 = DIRECTION ( 'NONE',  ( 0.6830127018922180770, -0.6830127018922204085, -0.2588190451025213501 ) ) ;
#7885 = PLANE ( 'NONE',  #117069 ) ;
#7886 = CARTESIAN_POINT ( 'NONE',  ( -24.79333936457829779, 21.75929247661549581, 4.998822639870701856 ) ) ;
#7887 = DIRECTION ( 'NONE',  ( -0.7071067811865487940, 0.7071067811865463515, -0.000000000000000000 ) ) ;
#7888 = ORIENTED_EDGE ( 'NONE', *, *, #106156, .T. ) ;
#7889 = ORIENTED_EDGE ( 'NONE', *, *, #34512, .F. ) ;
#7890 = VERTEX_POINT ( 'NONE', #27189 ) ;
#7891 = DIRECTION ( 'NONE',  ( -0.3543493200069162685, -0.000000000000000000, -0.9351131265310288487 ) ) ;
#7892 = CARTESIAN_POINT ( 'NONE',  ( 31.49999999999979039, -7.912538124160673370, 4.000000000000000000 ) ) ;
#7893 = CARTESIAN_POINT ( 'NONE',  ( 7.942069808101886785, 7.934999999999992504, 2.126176841940951689 ) ) ;
#7894 = AXIS2_PLACEMENT_3D ( 'NONE', #67916, #57728, #33144 ) ;
#7895 = LINE ( 'NONE', #130431, #85024 ) ;
#7896 =( LENGTH_UNIT ( ) NAMED_UNIT ( * ) SI_UNIT ( .MILLI., .METRE. ) );
#7897 = VECTOR ( 'NONE', #44825, 999.9999999999998863 ) ;
#7898 = VERTEX_POINT ( 'NONE', #71432 ) ;
#7899 = ORIENTED_EDGE ( 'NONE', *, *, #59113, .T. ) ;
#7900 = VECTOR ( 'NONE', #6208, 1000.000000000000114 ) ;
#7901 = CARTESIAN_POINT ( 'NONE',  ( 24.18398860626899705, 28.73617430169804265, 5.000000000000000000 ) ) ;
#7903 = EDGE_CURVE ( 'NONE', #138539, #44911, #16290, .T. ) ;
#7902 = ORIENTED_EDGE ( 'NONE', *, *, #35649, .T. ) ;
#7904 = ORIENTED_EDGE ( 'NONE', *, *, #127521, .T. ) ;
#7905 =( NAMED_UNIT ( * ) PLANE_ANGLE_UNIT ( ) SI_UNIT ( $, .RADIAN. ) );
#7906 = CARTESIAN_POINT ( 'NONE',  ( -60.48921356237309510, -27.52281430457097500, 5.000000000000000000 ) ) ;
#7907 = ORIENTED_EDGE ( 'NONE', *, *, #61365, .T. ) ;
#7908 = AXIS2_PLACEMENT_3D ( 'NONE', #106381, #84678, #141939 ) ;
#7909 = CARTESIAN_POINT ( 'NONE',  ( 0.000000000000000000, 0.000000000000000000, 5.000000000000000000 ) ) ;
#7910 = EDGE_CURVE ( 'NONE', #16291, #20377, #109027, .T. ) ;
#7911 = LINE ( 'NONE', #50030, #59475 ) ;
#7912 = CARTESIAN_POINT ( 'NONE',  ( 36.18398860626899705, 28.73617430169812437, 5.000000000000000000 ) ) ;
#7913 =( LENGTH_UNIT ( ) NAMED_UNIT ( * ) SI_UNIT ( .MILLI., .METRE. ) );
#7914 = ORIENTED_EDGE ( 'NONE', *, *, #7986, .T. ) ;
#7915 = DIRECTION ( 'NONE',  ( 0.7071067811865486830, -0.7071067811865464625, -0.000000000000000000 ) ) ;
#7916 = CARTESIAN_POINT ( 'NONE',  ( -8.206660635421469507, 21.75929247661548516, 4.998822639870715179 ) ) ;
#7918 = ORIENTED_EDGE ( 'NONE', *, *, #34544, .T. ) ;
#7917 = VECTOR ( 'NONE', #36015, 1000.000000000000000 ) ;
#7919 = CARTESIAN_POINT ( 'NONE',  ( 7.939999999999994174, -60.26999999999998892, -12.24789999999999957 ) ) ;
#7920 = EDGE_CURVE ( 'NONE', #137750, #102574, #10025, .T. ) ;
#7921 = CARTESIAN_POINT ( 'NONE',  ( 19.61884355727922014, -0.8539424794488987835, -31.56759919030367101 ) ) ;
#7922 = ORIENTED_EDGE ( 'NONE', *, *, #80131, .F. ) ;
#7924 = EDGE_CURVE ( 'NONE', #13610, #122891, #32208, .T. ) ;
#7923 = CYLINDRICAL_SURFACE ( 'NONE', #20438, 2.500000000000000000 ) ;
#7925 = VERTEX_POINT ( 'NONE', #85860 ) ;
#7926 = ORIENTED_EDGE ( 'NONE', *, *, #50869, .F. ) ;
#7927 = ORIENTED_EDGE ( 'NONE', *, *, #130387, .T. ) ;
#7929 = ADVANCED_FACE ( 'NONE', ( #141690 ), #63440, .T. ) ;
#7928 = VECTOR ( 'NONE', #54382, 999.9999999999998863 ) ;
#7930 = PLANE ( 'NONE',  #7181 ) ;
#7931 = VECTOR ( 'NONE', #3158, 1000.000000000000000 ) ;
#7932 = AXIS2_PLACEMENT_3D ( 'NONE', #7250, #42080, #41326 ) ;
#7933 = DIRECTION ( 'NONE',  ( -0.7071067811865486830, -0.7071067811865464625, -0.000000000000000000 ) ) ;
#7934 = PLANE ( 'NONE',  #86625 ) ;
#7935 = FACE_BOUND ( 'NONE', #73889, .T. ) ;
#7936 = CARTESIAN_POINT ( 'NONE',  ( -9.524999999999995026, -4.870000000000014317, -40.00000000000000000 ) ) ;
#7937 = EDGE_CURVE ( 'NONE', #118585, #103206, #130099, .T. ) ;
#7938 = DIRECTION ( 'NONE',  ( 0.6830127018922180770, -0.6830127018922204085, -0.2588190451025213501 ) ) ;
#7939 = CARTESIAN_POINT ( 'NONE',  ( -22.49999999999984723, -14.94781430457067195, 5.000000000000000000 ) ) ;
#7940 = EDGE_CURVE ( 'NONE', #78254, #98954, #19879, .T. ) ;
#7941 = STYLED_ITEM ( 'NONE', ( #13280 ), #2383 ) ;
#7942 = DIRECTION ( 'NONE',  ( -0.7071067811865486830, -0.7071067811865464625, 0.000000000000000000 ) ) ;
#7943 = FACE_OUTER_BOUND ( 'NONE', #3747, .T. ) ;
#7944 = CARTESIAN_POINT ( 'NONE',  ( 34.92499999999998295, -21.72500000000000142, 5.000000000000000000 ) ) ;
#7945 = ORIENTED_EDGE ( 'NONE', *, *, #49468, .T. ) ;
#7946 = ORIENTED_EDGE ( 'NONE', *, *, #108964, .F. ) ;
#7947 = ORIENTED_EDGE ( 'NONE', *, *, #124276, .F. ) ;
#7948 = EDGE_LOOP ( 'NONE', ( #96073, #52877, #84012, #18772 ) ) ;
#7949 = CARTESIAN_POINT ( 'NONE',  ( 0.000000000000000000, 0.000000000000000000, 0.000000000000000000 ) ) ;
#7950 = EDGE_CURVE ( 'NONE', #139004, #127787, #143102, .T. ) ;
#7951 = ORIENTED_EDGE ( 'NONE', *, *, #136975, .T. ) ;
#7952 = ORIENTED_EDGE ( 'NONE', *, *, #129255, .F. ) ;
#7953 = LINE ( 'NONE', #31175, #120832 ) ;
#7954 = DIRECTION ( 'NONE',  ( 0.000000000000000000, 0.000000000000000000, -1.000000000000000000 ) ) ;
#7955 = DIRECTION ( 'NONE',  ( -0.7071067811865487940, 0.7071067811865463515, -0.000000000000000000 ) ) ;
#7956 = EDGE_LOOP ( 'NONE', ( #97977, #83457, #5561, #108629 ) ) ;
#7957 = CARTESIAN_POINT ( 'NONE',  ( 14.99999999999989697, -18.03360074219755660, 5.000000000000000000 ) ) ;
#7958 = EDGE_CURVE ( 'NONE', #82847, #49011, #65588, .T. ) ;
#7959 = ORIENTED_EDGE ( 'NONE', *, *, #47900, .T. ) ;
#7960 = FACE_OUTER_BOUND ( 'NONE', #132463, .T. ) ;
#7961 = CARTESIAN_POINT ( 'NONE',  ( -11.01088028653940576, -22.02621442084247860, 4.990779571109222879 ) ) ;
#7962 = CARTESIAN_POINT ( 'NONE',  ( 8.087903141435219823, 6.871911579029515771, 3.967499999999989146 ) ) ;
#7963 = ORIENTED_EDGE ( 'NONE', *, *, #70023, .T. ) ;
#7964 = CARTESIAN_POINT ( 'NONE',  ( 87.84959685856476597, 6.109999999999997655, 1.637169565754163836 ) ) ;
#7965 = DIRECTION ( 'NONE',  ( -0.3543493200069162685, -0.000000000000000000, -0.9351131265310288487 ) ) ;
#7966 = PLANE ( 'NONE',  #14226 ) ;
#7967 = CARTESIAN_POINT ( 'NONE',  ( -11.29289321881336861, -12.74070752338415247, 5.000000000000000000 ) ) ;
#7968 = ORIENTED_EDGE ( 'NONE', *, *, #10546, .F. ) ;
#7969 = EDGE_CURVE ( 'NONE', #79775, #53362, #53220, .T. ) ;
#7970 = VERTEX_POINT ( 'NONE', #52515 ) ;
#7971 = FACE_OUTER_BOUND ( 'NONE', #46397, .T. ) ;
#7972 = VERTEX_POINT ( 'NONE', #120608 ) ;
#7973 = CARTESIAN_POINT ( 'NONE',  ( 25.65999999999999659, 9.521314400968980422E-16, 0.000000000000000000 ) ) ;
#7974 = CARTESIAN_POINT ( 'NONE',  ( 9.516654386410381861, 22.22500000000000142, 4.500000000000000888 ) ) ;
#7975 = CARTESIAN_POINT ( 'NONE',  ( -11.99999999999991651, 7.931123077392104648, 4.000000000000000000 ) ) ;
#7976 = LINE ( 'NONE', #63829, #81967 ) ;
#7978 = VERTEX_POINT ( 'NONE', #109757 ) ;
#7977 = VECTOR ( 'NONE', #94245, 1000.000000000000000 ) ;
#7979 = EDGE_CURVE ( 'NONE', #108003, #35148, #142410, .T. ) ;
#7980 = EDGE_CURVE ( 'NONE', #29089, #122015, #20591, .T. ) ;
#7981 = PLANE ( 'NONE',  #90071 ) ;
#7982 = PLANE ( 'NONE',  #56147 ) ;
#7983 = EDGE_LOOP ( 'NONE', ( #79443, #2245, #129630, #14927 ) ) ;
#7984 = DIRECTION ( 'NONE',  ( 1.000000000000000000, 0.000000000000000000, 0.000000000000000000 ) ) ;
#7986 = EDGE_CURVE ( 'NONE', #28861, #45664, #8961, .T. ) ;
#7985 = PLANE ( 'NONE',  #95641 ) ;
#7987 = ORIENTED_EDGE ( 'NONE', *, *, #1098, .F. ) ;
#7989 = EDGE_LOOP ( 'NONE', ( #36420, #10079, #129452, #12956 ) ) ;
#7988 = LINE ( 'NONE', #71875, #138952 ) ;
#7991 = ORIENTED_EDGE ( 'NONE', *, *, #51924, .F. ) ;
#7990 = ADVANCED_FACE ( 'NONE', ( #106891 ), #9717, .F. ) ;
#7992 = LINE ( 'NONE', #18137, #9913 ) ;
#7993 = LINE ( 'NONE', #18887, #64555 ) ;
#7994 = ORIENTED_EDGE ( 'NONE', *, *, #122358, .T. ) ;
#7995 = DIRECTION ( 'NONE',  ( 0.7071067811865487940, 0.7071067811865463515, 0.000000000000000000 ) ) ;
#7996 = CARTESIAN_POINT ( 'NONE',  ( -6.328169399223481761, -3.740707523384243505, 4.000000000000000000 ) ) ;
#7997 = AXIS2_PLACEMENT_3D ( 'NONE', #89198, #45019, #34111 ) ;
#7998 = LINE ( 'NONE', #32649, #76246 ) ;
#7999 = EDGE_CURVE ( 'NONE', #48100, #79180, #43796, .T. ) ;
#8000 = DIRECTION ( 'NONE',  ( 0.6830127018922180770, -0.6830127018922204085, -0.2588190451025213501 ) ) ;
#8002 = CARTESIAN_POINT ( 'NONE',  ( 34.92499999999998295, 16.80009451602700210, 4.759050581649325373 ) ) ;
#8001 = VECTOR ( 'NONE', #21950, 1000.000000000000000 ) ;
#8003 = DIRECTION ( 'NONE',  ( -0.6830127018922181881, 0.6830127018922202975, -0.2588190451025214056 ) ) ;
#8004 = DIRECTION ( 'NONE',  ( 0.7071067811865486830, -0.7071067811865464625, -0.000000000000000000 ) ) ;
#8005 = CARTESIAN_POINT ( 'NONE',  ( -5.816011393731002066, 28.73617430169783304, 5.000000000000000000 ) ) ;
#8006 = DIRECTION ( 'NONE',  ( 0.3543493200069162685, -0.000000000000000000, -0.9351131265310288487 ) ) ;
#8007 = LINE ( 'NONE', #29074, #76845 ) ;
#8008 = CARTESIAN_POINT ( 'NONE',  ( -33.18398860626899705, 28.73617430169810305, 5.000000000000000000 ) ) ;
#8009 = ADVANCED_FACE ( 'NONE', ( #129358 ), #42393, .F. ) ;
#8010 = LINE ( 'NONE', #74014, #21091 ) ;
#8011 = DIRECTION ( 'NONE',  ( 0.000000000000000000, 1.000000000000000000, 0.000000000000000000 ) ) ;
#8012 = EDGE_LOOP ( 'NONE', ( #71243, #72278, #123249, #135978 ) ) ;
#8013 = ORIENTED_EDGE ( 'NONE', *, *, #32007, .T. ) ;
#8014 = VERTEX_POINT ( 'NONE', #8268 ) ;
#8015 = CARTESIAN_POINT ( 'NONE',  ( 109.5000000000000000, 0.000000000000000000, -7.950000000000000178 ) ) ;
#8016 = ORIENTED_EDGE ( 'NONE', *, *, #37641, .F. ) ;
#8017 = VERTEX_POINT ( 'NONE', #130830 ) ;
#8018 = ORIENTED_EDGE ( 'NONE', *, *, #83115, .T. ) ;
#8019 = DIRECTION ( 'NONE',  ( 0.7071067811865487940, 0.7071067811865463515, 0.000000000000000000 ) ) ;
#8020 = FACE_OUTER_BOUND ( 'NONE', #86538, .T. ) ;
#8021 = ORIENTED_EDGE ( 'NONE', *, *, #19804, .T. ) ;
#8022 = DIRECTION ( 'NONE',  ( 0.000000000000000000, -1.000000000000000000, 0.000000000000000000 ) ) ;
#8023 = DIRECTION ( 'NONE',  ( 0.7071067811865487940, 0.7071067811865463515, 0.000000000000000000 ) ) ;
#8024 = CARTESIAN_POINT ( 'NONE',  ( -33.12147316337127023, -20.24070752338407075, 7.412974875817869069 ) ) ;
#8025 = DIRECTION ( 'NONE',  ( -0.000000000000000000, -0.3543493200069152693, 0.9351131265310292928 ) ) ;
#8026 = CARTESIAN_POINT ( 'NONE',  ( 100.9170968585647756, 3.054999999999998828, 5.291415217122922066 ) ) ;
#8027 = ORIENTED_EDGE ( 'NONE', *, *, #87812, .F. ) ;
#8028 = CARTESIAN_POINT ( 'NONE',  ( -3.753437965960260136, 12.18814048229829261, -27.09591142044626011 ) ) ;
#8029 = CARTESIAN_POINT ( 'NONE',  ( -6.684521246590537480, -34.56135169103111338, 17.98619725537731995 ) ) ;
#8030 = DIRECTION ( 'NONE',  ( 0.3543493200069162685, -0.000000000000000000, -0.9351131265310288487 ) ) ;
#8031 = FACE_OUTER_BOUND ( 'NONE', #103682, .T. ) ;
#8032 = DIRECTION ( 'NONE',  ( -1.000000000000000000, -1.224606353822377258E-16, -0.000000000000000000 ) ) ;
#8033 = CARTESIAN_POINT ( 'NONE',  ( -17.81601139373099940, 28.73617430169775133, 5.000000000000000000 ) ) ;
#8034 = FACE_OUTER_BOUND ( 'NONE', #29804, .T. ) ;
#8035 = CARTESIAN_POINT ( 'NONE',  ( 32.01669371712954160, 7.950000000000001066, -2.130196079827421318 ) ) ;
#8036 = VECTOR ( 'NONE', #14825, 1000.000000000000114 ) ;
#8037 = CARTESIAN_POINT ( 'NONE',  ( 16.49999999999988987, 21.05218569542895679, 5.000000000000000000 ) ) ;
#8038 = EDGE_CURVE ( 'NONE', #69227, #121031, #64841, .T. ) ;
#8039 = VECTOR ( 'NONE', #3676, 1000.000000000000000 ) ;
#8040 = ORIENTED_EDGE ( 'NONE', *, *, #39045, .F. ) ;
#8041 = ORIENTED_EDGE ( 'NONE', *, *, #47807, .F. ) ;
#8042 = VECTOR ( 'NONE', #112322, 1000.000000000000000 ) ;
#8043 = CARTESIAN_POINT ( 'NONE',  ( 29.43749999999998579, 5.819803920172573974, -5.819803920172572198 ) ) ;
#8044 = EDGE_LOOP ( 'NONE', ( #69150, #85237, #100776 ) ) ;
#8045 =( GEOMETRIC_REPRESENTATION_CONTEXT ( 3 ) GLOBAL_UNCERTAINTY_ASSIGNED_CONTEXT ( ( #105876 ) ) GLOBAL_UNIT_ASSIGNED_CONTEXT ( ( #104927, #115764, #17884 ) ) REPRESENTATION_CONTEXT ( 'NONE', 'WORKASPACE' ) );
#8046 = DIRECTION ( 'NONE',  ( -0.7071067811865486830, 0.7071067811865464625, 0.000000000000000000 ) ) ;
#8047 = FACE_OUTER_BOUND ( 'NONE', #96688, .T. ) ;
#8048 = CARTESIAN_POINT ( 'NONE',  ( 13.96000000000000085, 9.521314400968980422E-16, 0.000000000000000000 ) ) ;
#8049 = CARTESIAN_POINT ( 'NONE',  ( -51.29974487139158867, -27.71228299555242103, 4.000000000000000000 ) ) ;
#8050 = CARTESIAN_POINT ( 'NONE',  ( 24.79289321881328689, -17.24070752338409918, 5.000000000000000000 ) ) ;
#8051 =( LENGTH_UNIT ( ) NAMED_UNIT ( * ) SI_UNIT ( .MILLI., .METRE. ) );
#8052 = CARTESIAN_POINT ( 'NONE',  ( 124.4537635252314516, -6.109999999999998543, -3.741295971395162543E-16 ) ) ;
#8053 = VERTEX_POINT ( 'NONE', #87302 ) ;
#8054 = LINE ( 'NONE', #571, #85045 ) ;
#8055 = ORIENTED_EDGE ( 'NONE', *, *, #101657, .F. ) ;
#8056 = LINE ( 'NONE', #126991, #130699 ) ;
#8057 = PLANE ( 'NONE',  #15366 ) ;
#8058 = FACE_OUTER_BOUND ( 'NONE', #120417, .T. ) ;
#8059 = CARTESIAN_POINT ( 'NONE',  ( -19.78678096696629041, 12.75929247661559351, 10.29404684609030696 ) ) ;
#8060 = ORIENTED_EDGE ( 'NONE', *, *, #130943, .F. ) ;
#8061 = CARTESIAN_POINT ( 'NONE',  ( 45.79209685856476852, -5.291415217122921177, 3.054999999999999272 ) ) ;
#8062 = EDGE_LOOP ( 'NONE', ( #111725, #14219, #27039, #77689 ) ) ;
#8063 = DIRECTION ( 'NONE',  ( 1.000000000000000000, 0.000000000000000000, 0.000000000000000000 ) ) ;
#8064 = CARTESIAN_POINT ( 'NONE',  ( -24.18398860626899705, 28.73617430169804265, 5.000000000000000000 ) ) ;
#8065 = CARTESIAN_POINT ( 'NONE',  ( 12.40000000000000213, 9.521314400968980422E-16, 0.000000000000000000 ) ) ;
#8066 = LINE ( 'NONE', #41428, #2080 ) ;
#8067 = CARTESIAN_POINT ( 'NONE',  ( 37.68293019189810167, -1.637169565754158951, -6.109999999999998543 ) ) ;
#8068 = ORIENTED_EDGE ( 'NONE', *, *, #44662, .T. ) ;
#8069 = DIRECTION ( 'NONE',  ( 0.7071067811865486830, -0.7071067811865464625, -0.000000000000000000 ) ) ;
#8071 = EDGE_CURVE ( 'NONE', #56522, #75711, #25585, .T. ) ;
#8070 = ORIENTED_EDGE ( 'NONE', *, *, #107199, .T. ) ;
#8072 = EDGE_LOOP ( 'NONE', ( #74486, #117067, #47553, #62042, #86616, #35873, #19633, #1364, #55333, #142617, #117900, #89041, #96499, #38836, #66152, #122881, #87505, #81982 ) ) ;
#8073 = ORIENTED_EDGE ( 'NONE', *, *, #84301, .T. ) ;
#8074 = DIRECTION ( 'NONE',  ( 1.000000000000000000, 0.000000000000000000, 0.000000000000000000 ) ) ;
#8075 = CARTESIAN_POINT ( 'NONE',  ( 79.85002705046289861, -5.819803920172573086, -5.819803920172573086 ) ) ;
#8076 = ORIENTED_EDGE ( 'NONE', *, *, #139424, .F. ) ;
#8077 = CARTESIAN_POINT ( 'NONE',  ( 2.301729841053981485, 3.061616997868383141E-16, -2.500000000000000444 ) ) ;
#8078 = CARTESIAN_POINT ( 'NONE',  ( -1.499999999999987566, 6.052185695429108669, 5.000000000000000000 ) ) ;
#8079 = CARTESIAN_POINT ( 'NONE',  ( 21.29974487139158512, -27.71228299555221142, 4.000000000000000000 ) ) ;
#8080 = EDGE_CURVE ( 'NONE', #24706, #128126, #40442, .T. ) ;
#8081 = FACE_BOUND ( 'NONE', #41959, .T. ) ;
#8082 = ORIENTED_EDGE ( 'NONE', *, *, #110078, .T. ) ;
#8083 = LINE ( 'NONE', #141490, #133659 ) ;
#8084 = EDGE_CURVE ( 'NONE', #95696, #109538, #111918, .T. ) ;
#8085 = EDGE_CURVE ( 'NONE', #64063, #69181, #89431, .T. ) ;
#8086 = CARTESIAN_POINT ( 'NONE',  ( 12.00548008471251293, 28.92564299267929684, 4.000000000000000000 ) ) ;
#8087 = LINE ( 'NONE', #52328, #108698 ) ;
#8088 = VERTEX_POINT ( 'NONE', #13991 ) ;
#8089 = SURFACE_STYLE_FILL_AREA ( #64646 ) ;
#8090 = EDGE_LOOP ( 'NONE', ( #47374, #124652, #3641, #110715 ) ) ;
#8091 = VERTEX_POINT ( 'NONE', #55399 ) ;
#8092 = CARTESIAN_POINT ( 'NONE',  ( -3.183988606268992161, 28.73617430169789699, 5.000000000000000000 ) ) ;
#8093 = ORIENTED_EDGE ( 'NONE', *, *, #31216, .T. ) ;
#8094 = ADVANCED_FACE ( 'NONE', ( #11121 ), #47416, .F. ) ;
#8095 = EDGE_CURVE ( 'NONE', #79128, #68609, #57548, .T. ) ;
#8096 = CARTESIAN_POINT ( 'NONE',  ( 60.14126352523143737, 4.472830434245835818, 4.472830434245840259 ) ) ;
#8097 = ORIENTED_EDGE ( 'NONE', *, *, #41856, .F. ) ;
#8098 = CARTESIAN_POINT ( 'NONE',  ( -19.22850677138653452, 20.25929247661551713, 7.808871592221724001 ) ) ;
#8099 = AXIS2_PLACEMENT_3D ( 'NONE', #24109, #75993, #120164 ) ;
#8100 = DIRECTION ( 'NONE',  ( -0.3543493200069162685, -0.000000000000000000, -0.9351131265310288487 ) ) ;
#8101 = EDGE_CURVE ( 'NONE', #112793, #52592, #250, .T. ) ;
#8102 = ORIENTED_EDGE ( 'NONE', *, *, #500, .T. ) ;
#8103 = FACE_OUTER_BOUND ( 'NONE', #39898, .T. ) ;
#8104 = EDGE_CURVE ( 'NONE', #50012, #99801, #90143, .T. ) ;
#8105 = CARTESIAN_POINT ( 'NONE',  ( 11.81601139373100651, 28.73617430169779041, 5.000000000000000000 ) ) ;
#8106 = COLOUR_RGB ( '', 0.09019608, 0.27058824, 0.51372549) ;
#8107 = CARTESIAN_POINT ( 'NONE',  ( 34.42499999999998295, -15.02281430457044742, 5.000000000000000000 ) ) ;
#8108 = LINE ( 'NONE', #140772, #94438 ) ;
#8109 = CARTESIAN_POINT ( 'NONE',  ( 0.000000000000000000, 0.000000000000000000, 0.000000000000000000 ) ) ;
#8110 = PLANE ( 'NONE',  #44052 ) ;
#8111 = EDGE_LOOP ( 'NONE', ( #34052, #2670, #17268, #15931, #101188, #18714, #75186, #125162 ) ) ;
#8112 = EDGE_CURVE ( 'NONE', #127403, #49277, #46709, .T. ) ;
#8113 = EDGE_LOOP ( 'NONE', ( #2525, #96399, #92241, #112138 ) ) ;
#8114 = CARTESIAN_POINT ( 'NONE',  ( 37.78501580275787575, -3.740707523384248390, 15.76143240460133121 ) ) ;
#8115 = CARTESIAN_POINT ( 'NONE',  ( 62.99451991528749772, 28.92564299267982264, 4.000000000000000000 ) ) ;
#8116 = ORIENTED_EDGE ( 'NONE', *, *, #24005, .T. ) ;
#8117 = ORIENTED_EDGE ( 'NONE', *, *, #25842, .F. ) ;
#8118 = ORIENTED_EDGE ( 'NONE', *, *, #124383, .F. ) ;
#8119 = CARTESIAN_POINT ( 'NONE',  ( -26.99451991528749417, 28.92564299267956685, 4.000000000000000000 ) ) ;
#8120 = DIRECTION ( 'NONE',  ( 0.7071067811865487940, 0.7071067811865463515, 0.000000000000000000 ) ) ;
#8121 = LINE ( 'NONE', #75564, #25388 ) ;
#8122 = ORIENTED_EDGE ( 'NONE', *, *, #127489, .T. ) ;
#8123 = DIRECTION ( 'NONE',  ( 0.7071067811865486830, -0.7071067811865464625, -0.000000000000000000 ) ) ;
#8124 = EDGE_CURVE ( 'NONE', #33017, #117585, #112618, .T. ) ;
#8125 = DIRECTION ( 'NONE',  ( 0.7071067811865487940, -0.7071067811865463515, 0.000000000000000000 ) ) ;
#8126 = VECTOR ( 'NONE', #126366, 999.9999999999998863 ) ;
#8127 = CARTESIAN_POINT ( 'NONE',  ( 22.37956980810188767, 3.967499999999998916, 6.871911579029510442 ) ) ;
#8128 = AXIS2_PLACEMENT_3D ( 'NONE', #97653, #74507, #1861 ) ;
#8129 = DIRECTION ( 'NONE',  ( -0.000000000000000000, 0.000000000000000000, 1.000000000000000000 ) ) ;
#8130 = EDGE_LOOP ( 'NONE', ( #50108, #56244, #12565, #5862 ) ) ;
#8131 = CARTESIAN_POINT ( 'NONE',  ( 116.8704301918981230, -3.055000000000001936, 5.291415217122918513 ) ) ;
#8132 = VECTOR ( 'NONE', #22366, 1000.000000000000000 ) ;
#8133 = CIRCLE ( 'NONE', #40574, 2.337593264352433753 ) ;
#8134 = DIRECTION ( 'NONE',  ( -1.000000000000000000, -0.000000000000000000, -0.000000000000000000 ) ) ;
#8135 = EDGE_CURVE ( 'NONE', #42962, #37411, #132977, .T. ) ;
#8136 = CARTESIAN_POINT ( 'NONE',  ( -8.671830600776409881, 5.259292476615659240, 4.000000000000000000 ) ) ;
#8138 = ORIENTED_EDGE ( 'NONE', *, *, #12810, .T. ) ;
#8137 = CARTESIAN_POINT ( 'NONE',  ( 5.994519915287488843, 28.92564299267942118, 4.000000000000000000 ) ) ;
#8139 = CARTESIAN_POINT ( 'NONE',  ( 0.000000000000000000, 0.000000000000000000, 5.000000000000000000 ) ) ;
#8140 = VERTEX_POINT ( 'NONE', #56138 ) ;
#8141 = CARTESIAN_POINT ( 'NONE',  ( 75.62086038379622721, -6.884901960086286188, 3.974999999999997424 ) ) ;
#8142 = PLANE ( 'NONE',  #63210 ) ;
#8143 = DIRECTION ( 'NONE',  ( -1.000000000000000000, -1.224606353822377258E-16, -0.000000000000000000 ) ) ;
#8144 = EDGE_LOOP ( 'NONE', ( #45874, #39153 ) ) ;
#8145 = EDGE_CURVE ( 'NONE', #116931, #52182, #2389, .T. ) ;
#8146 = EDGE_CURVE ( 'NONE', #16679, #143518, #122042, .T. ) ;
#8147 = DIRECTION ( 'NONE',  ( 0.7071067811865486830, -0.7071067811865464625, -0.000000000000000000 ) ) ;
#8148 = CARTESIAN_POINT ( 'NONE',  ( -18.18398860626898994, 28.73617430169800002, 5.000000000000000000 ) ) ;
#8149 = CARTESIAN_POINT ( 'NONE',  ( -19.49368896717581023, -0.02969617003380616710, -31.02254237922252500 ) ) ;
#8150 = ORIENTED_EDGE ( 'NONE', *, *, #45348, .F. ) ;
#8151 = DIRECTION ( 'NONE',  ( 0.7071067811865487940, 0.7071067811865463515, 0.000000000000000000 ) ) ;
#8153 = ADVANCED_FACE ( 'NONE', ( #80034 ), #66982, .F. ) ;
#8152 = FACE_OUTER_BOUND ( 'NONE', #19129, .T. ) ;
#8154 = CARTESIAN_POINT ( 'NONE',  ( 4.812500000000000000, -4.461849672132299993, -4.461849672132299105 ) ) ;
#8155 = PLANE ( 'NONE',  #143331 ) ;
#8156 = ORIENTED_EDGE ( 'NONE', *, *, #10276, .T. ) ;
#8157 = VERTEX_POINT ( 'NONE', #45261 ) ;
#8158 = FACE_OUTER_BOUND ( 'NONE', #136308, .T. ) ;
#8159 = DIRECTION ( 'NONE',  ( 0.000000000000000000, 1.000000000000000000, 0.000000000000000000 ) ) ;
#8160 = ADVANCED_FACE ( 'NONE', ( #133665 ), #34346, .F. ) ;
#8161 = CARTESIAN_POINT ( 'NONE',  ( 13.39540314143521904, 2.126176841940962348, 7.934999999999989839 ) ) ;
#8162 = DIRECTION ( 'NONE',  ( -0.000000000000000000, -1.000000000000000000, -0.000000000000000000 ) ) ;
#8163 = CARTESIAN_POINT ( 'NONE',  ( 12.69999999999999574, -35.15000000000000568, -40.00000000000000000 ) ) ;
#8164 = DIRECTION ( 'NONE',  ( -1.000000000000000000, -0.000000000000000000, -0.000000000000000000 ) ) ;
#8165 = ORIENTED_EDGE ( 'NONE', *, *, #101928, .T. ) ;
#8166 = EDGE_CURVE ( 'NONE', #5483, #97574, #128328, .T. ) ;
#8167 = DIRECTION ( 'NONE',  ( 0.7071067811865487940, 0.7071067811865463515, -0.000000000000000000 ) ) ;
#8168 = FACE_OUTER_BOUND ( 'NONE', #72873, .T. ) ;
#8169 = DIRECTION ( 'NONE',  ( -0.000000000000000000, -0.3543493200069152693, 0.9351131265310292928 ) ) ;
#8170 = PLANE ( 'NONE',  #133933 ) ;
#8171 = CARTESIAN_POINT ( 'NONE',  ( 39.43293019189811588, 1.637169565754156730, 6.110000000000001208 ) ) ;
#8172 = DIRECTION ( 'NONE',  ( -0.000000000000000000, -0.000000000000000000, 1.000000000000000000 ) ) ;
#8173 = VERTEX_POINT ( 'NONE', #14731 ) ;
#8174 = FILL_AREA_STYLE_COLOUR ( '', #125320 ) ;
#8175 = ORIENTED_EDGE ( 'NONE', *, *, #42029, .T. ) ;
#8176 = ORIENTED_EDGE ( 'NONE', *, *, #130934, .T. ) ;
#8177 = DIRECTION ( 'NONE',  ( 0.000000000000000000, -1.000000000000000000, 0.000000000000000000 ) ) ;
#8178 = LINE ( 'NONE', #41536, #60224 ) ;
#8179 = EDGE_LOOP ( 'NONE', ( #80359, #130720, #28171, #780 ) ) ;
#8180 =( LENGTH_UNIT ( ) NAMED_UNIT ( * ) SI_UNIT ( .MILLI., .METRE. ) );
#8181 = LINE ( 'NONE', #143012, #51189 ) ;
#8182 = CARTESIAN_POINT ( 'NONE',  ( 69.18398860626899705, 28.73617430169835529, 5.000000000000000000 ) ) ;
#8183 = EDGE_CURVE ( 'NONE', #88988, #47967, #59007, .T. ) ;
#8184 = CARTESIAN_POINT ( 'NONE',  ( 82.81250000000000000, 5.819803920172571310, 5.819803920172576639 ) ) ;
#8185 = CARTESIAN_POINT ( 'NONE',  ( -45.48921356237309510, -27.52281430457087197, 5.000000000000000000 ) ) ;
#8186 = EDGE_LOOP ( 'NONE', ( #87949, #100295, #96738, #7739 ) ) ;
#8187 = CARTESIAN_POINT ( 'NONE',  ( -27.48921356237309155, -27.52281430457074762, 5.000000000000000000 ) ) ;
#8188 = DIRECTION ( 'NONE',  ( -0.3543493200069162685, -0.000000000000000000, -0.9351131265310288487 ) ) ;
#8189 = CARTESIAN_POINT ( 'NONE',  ( -33.79289321881321939, -5.240707523384230626, 5.000000000000000000 ) ) ;
#8190 = CARTESIAN_POINT ( 'NONE',  ( -29.99451991528749417, 28.92564299267958816, 4.000000000000000000 ) ) ;
#8191 = DIRECTION ( 'NONE',  ( -0.7071067811865486830, 0.7071067811865464625, 0.000000000000000000 ) ) ;
#8192 = CARTESIAN_POINT ( 'NONE',  ( 60.16252705046289151, 7.949999999999998401, 1.460391307983218338E-15 ) ) ;
#8193 = VECTOR ( 'NONE', #121460, 1000.000000000000227 ) ;
#8194 = ADVANCED_FACE ( 'NONE', ( #103163 ), #7934, .F. ) ;
#8195 = CARTESIAN_POINT ( 'NONE',  ( 10.50000000000000000, 0.000000000000000000, 6.094999999999989981 ) ) ;
#8196 = VERTEX_POINT ( 'NONE', #25590 ) ;
#8197 = ORIENTED_EDGE ( 'NONE', *, *, #117320, .T. ) ;
#8198 = CARTESIAN_POINT ( 'NONE',  ( 50.87499999999999289, 7.950000000000000178, 1.460391307983218535E-15 ) ) ;
#8199 = CARTESIAN_POINT ( 'NONE',  ( -18.54365462162017408, -22.22500000000000142, 11.20750413071516860 ) ) ;
#8200 = VECTOR ( 'NONE', #66408, 1000.000000000000227 ) ;
#8201 = DIRECTION ( 'NONE',  ( 0.3543493200069162685, -0.000000000000000000, -0.9351131265310288487 ) ) ;
#8202 = PLANE ( 'NONE',  #15869 ) ;
#8203 = ORIENTED_EDGE ( 'NONE', *, *, #12379, .T. ) ;
#8204 = EDGE_CURVE ( 'NONE', #32743, #47525, #6473, .T. ) ;
#8205 = CARTESIAN_POINT ( 'NONE',  ( -24.79289321881328334, -5.240707523384232402, 5.000000000000000000 ) ) ;
#8206 = EDGE_CURVE ( 'NONE', #141465, #124724, #80725, .T. ) ;
#8207 = AXIS2_PLACEMENT_3D ( 'NONE', #34607, #66530, #1921 ) ;
#8208 = CARTESIAN_POINT ( 'NONE',  ( 47.10459685856477563, 1.637169565754164946, -6.109999999999999432 ) ) ;
#8209 = EDGE_LOOP ( 'NONE', ( #129631, #49857, #123730, #64388 ) ) ;
#8210 = CARTESIAN_POINT ( 'NONE',  ( 7.176659101599685009, 5.259292476615659240, 15.86257073897096070 ) ) ;
#8211 = ORIENTED_EDGE ( 'NONE', *, *, #65018, .T. ) ;
#8212 = ORIENTED_EDGE ( 'NONE', *, *, #87043, .T. ) ;
#8213 = CARTESIAN_POINT ( 'NONE',  ( -42.48921356237308800, -27.52281430457085065, 5.000000000000000000 ) ) ;
#8214 = CARTESIAN_POINT ( 'NONE',  ( 13.49999999999990763, 13.56627193232216477, -10.57019076586065687 ) ) ;
#8215 = DIRECTION ( 'NONE',  ( -0.6830127018922181881, 0.6830127018922202975, -0.2588190451025214056 ) ) ;
#8216 = ORIENTED_EDGE ( 'NONE', *, *, #78718, .T. ) ;
#8217 = EDGE_CURVE ( 'NONE', #43879, #60787, #40602, .T. ) ;
#8218 = CARTESIAN_POINT ( 'NONE',  ( -34.49999999999976552, 3.073033219394595505, -6.593910359671048660 ) ) ;
#8220 = EDGE_LOOP ( 'NONE', ( #127151, #108096, #64112, #93756 ) ) ;
#8219 = LINE ( 'NONE', #82273, #142461 ) ;
#8221 = CARTESIAN_POINT ( 'NONE',  ( 23.60898926630779826, -0.6778661889157658882, 4.000000000000000000 ) ) ;
#8222 = DIRECTION ( 'NONE',  ( -0.7071067811865486830, -0.7071067811865464625, 0.000000000000000000 ) ) ;
#8223 = DIRECTION ( 'NONE',  ( -0.6830127018922180770, -0.6830127018922204085, -0.2588190451025213501 ) ) ;
#8224 = FACE_OUTER_BOUND ( 'NONE', #31463, .T. ) ;
#8225 = VECTOR ( 'NONE', #5552, 1000.000000000000000 ) ;
#8226 = EDGE_LOOP ( 'NONE', ( #43644, #77141, #125012, #42026 ) ) ;
#8227 = VECTOR ( 'NONE', #104321, 1000.000000000000000 ) ;
#8228 = VERTEX_POINT ( 'NONE', #97056 ) ;
#8229 = AXIS2_PLACEMENT_3D ( 'NONE', #70448, #35668, #79893 ) ;
#8230 = CARTESIAN_POINT ( 'NONE',  ( -17.99999999999986855, 20.96639925780204905, 5.000000000000000000 ) ) ;
#8231 = CARTESIAN_POINT ( 'NONE',  ( 70.05793019189812298, 6.110000000000000320, -1.637169565754156064 ) ) ;
#8232 = LINE ( 'NONE', #120561, #97284 ) ;
#8233 = DIRECTION ( 'NONE',  ( -0.7071067811865486830, -0.7071067811865464625, -0.000000000000000000 ) ) ;
#8234 = CARTESIAN_POINT ( 'NONE',  ( 25.49999999999982592, 6.277155672890295079, -3.510561720659000962 ) ) ;
#8235 = ORIENTED_EDGE ( 'NONE', *, *, #33880, .T. ) ;
#8236 = ORIENTED_EDGE ( 'NONE', *, *, #28139, .F. ) ;
#8237 = VECTOR ( 'NONE', #41908, 1000.000000000000000 ) ;
#8238 = DIRECTION ( 'NONE',  ( -0.000000000000000000, -0.3543493200069152693, 0.9351131265310292928 ) ) ;
#8239 = PLANE ( 'NONE',  #23645 ) ;
#8240 = VERTEX_POINT ( 'NONE', #39167 ) ;
#8241 = EDGE_LOOP ( 'NONE', ( #128185, #116395, #126319, #96183 ) ) ;
#8242 = PLANE ( 'NONE',  #120828 ) ;
#8243 = ORIENTED_EDGE ( 'NONE', *, *, #66429, .F. ) ;
#8244 = CARTESIAN_POINT ( 'NONE',  ( 64.29166666666665719, 3.975000000000003642, -6.884901960086285300 ) ) ;
#8245 = EDGE_CURVE ( 'NONE', #134120, #99796, #139926, .T. ) ;
#8246 = DIRECTION ( 'NONE',  ( -0.7071067811865486830, -0.7071067811865464625, -0.000000000000000000 ) ) ;
#8247 = PLANE ( 'NONE',  #9467 ) ;
#8248 = FACE_BOUND ( 'NONE', #131821, .T. ) ;
#8249 = CARTESIAN_POINT ( 'NONE',  ( -7.499999999999947597, -16.91253812416058011, 4.000000000000000000 ) ) ;
#8250 = EDGE_CURVE ( 'NONE', #63037, #14142, #29002, .T. ) ;
#8251 = CARTESIAN_POINT ( 'NONE',  ( 26.90840764549667696, 9.139736423841732040E-16, 0.000000000000000000 ) ) ;
#8252 = FACE_OUTER_BOUND ( 'NONE', #92686, .T. ) ;
#8254 = EDGE_LOOP ( 'NONE', ( #67768, #138531, #123832 ) ) ;
#8253 = CARTESIAN_POINT ( 'NONE',  ( 54.29974487139159578, -27.71228299555243879, 4.000000000000000000 ) ) ;
#8255 = CARTESIAN_POINT ( 'NONE',  ( 20.99999999999985079, 12.83542986846998879, -1.025386466790417561 ) ) ;
#8256 = VERTEX_POINT ( 'NONE', #72557 ) ;
#8257 = EDGE_CURVE ( 'NONE', #63984, #124237, #110663, .T. ) ;
#8258 = EDGE_CURVE ( 'NONE', #88739, #75266, #116720, .T. ) ;
#8259 = ORIENTED_EDGE ( 'NONE', *, *, #23507, .F. ) ;
#8260 = CARTESIAN_POINT ( 'NONE',  ( 85.95376352523145158, -6.109999999999998543, -3.741295971395162543E-16 ) ) ;
#8261 = ORIENTED_EDGE ( 'NONE', *, *, #61575, .F. ) ;
#8262 = DIRECTION ( 'NONE',  ( 0.7071067811865487940, -0.7071067811865463515, 0.000000000000000000 ) ) ;
#8263 = ADVANCED_FACE ( 'NONE', ( #29689 ), #94943, .F. ) ;
#8264 = DIRECTION ( 'NONE',  ( 0.6830127018922180770, -0.6830127018922204085, -0.2588190451025213501 ) ) ;
#8265 = EDGE_CURVE ( 'NONE', #100067, #19260, #18073, .T. ) ;
#8266 = CARTESIAN_POINT ( 'NONE',  ( 5.700255128608413102, -27.71228299555201957, 4.000000000000000000 ) ) ;
#8267 = ADVANCED_FACE ( 'NONE', ( #106520 ), #7204, .F. ) ;
#8268 = CARTESIAN_POINT ( 'NONE',  ( -27.79289321881325847, 6.759292476615649470, 5.000000000000000000 ) ) ;
#8269 = CARTESIAN_POINT ( 'NONE',  ( 66.48921356237309510, -27.52281430457101763, 5.000000000000000000 ) ) ;
#8270 = EDGE_CURVE ( 'NONE', #91367, #116472, #51476, .T. ) ;
#8271 = CARTESIAN_POINT ( 'NONE',  ( 30.29974487139158867, -27.71228299555227537, 4.000000000000000000 ) ) ;
#8272 = DIRECTION ( 'NONE',  ( -0.7071067811865486830, -0.7071067811865464625, -0.000000000000000000 ) ) ;
#8273 = PLANE ( 'NONE',  #61222 ) ;
#8274 = DIRECTION ( 'NONE',  ( -1.000000000000000000, -1.224606353822377258E-16, -0.000000000000000000 ) ) ;
#8275 = FACE_OUTER_BOUND ( 'NONE', #8226, .T. ) ;
#8276 = ORIENTED_EDGE ( 'NONE', *, *, #74717, .F. ) ;
#8277 =( NAMED_UNIT ( * ) PLANE_ANGLE_UNIT ( ) SI_UNIT ( $, .RADIAN. ) );
#8278 = VERTEX_POINT ( 'NONE', #30431 ) ;
#8279 = CARTESIAN_POINT ( 'NONE',  ( -26.99451991528749417, 28.92564299267956685, 4.000000000000000000 ) ) ;
#8280 = DIRECTION ( 'NONE',  ( 0.000000000000000000, -1.000000000000000000, 0.000000000000000000 ) ) ;
#8281 = EDGE_CURVE ( 'NONE', #20176, #46795, #74665, .T. ) ;
#8282 = ORIENTED_EDGE ( 'NONE', *, *, #117272, .T. ) ;
#8283 = EDGE_LOOP ( 'NONE', ( #52578, #8176, #30633, #98962 ) ) ;
#8284 = ORIENTED_EDGE ( 'NONE', *, *, #32742, .F. ) ;
#8285 = CARTESIAN_POINT ( 'NONE',  ( 40.10459685856476852, 1.637169565754164946, -6.109999999999999432 ) ) ;
#8286 = ORIENTED_EDGE ( 'NONE', *, *, #141206, .F. ) ;
#8287 = DIRECTION ( 'NONE',  ( 0.5735764363510453823, -0.8191520442889923537, 1.003171929053525486E-16 ) ) ;
#8288 = EDGE_CURVE ( 'NONE', #26834, #50573, #47239, .T. ) ;
#8289 = AXIS2_PLACEMENT_3D ( 'NONE', #118642, #65745, #20750 ) ;
#8290 = CARTESIAN_POINT ( 'NONE',  ( 26.44163961620376924, -6.094999999999989093, 1.633150327867691765 ) ) ;
#8291 = CARTESIAN_POINT ( 'NONE',  ( -4.595688708094440855, 11.98067335678676670, -27.27784815589622980 ) ) ;
#8292 = ORIENTED_EDGE ( 'NONE', *, *, #3439, .T. ) ;
#8293 = AXIS2_PLACEMENT_3D ( 'NONE', #38413, #49316, #93503 ) ;
#8294 = LINE ( 'NONE', #95332, #115140 ) ;
#8295 = ORIENTED_EDGE ( 'NONE', *, *, #46016, .T. ) ;
#8296 = DIRECTION ( 'NONE',  ( 0.6830127018922181881, 0.6830127018922202975, -0.2588190451025214056 ) ) ;
#8297 = DIRECTION ( 'NONE',  ( -0.3543493200069162685, -0.000000000000000000, -0.9351131265310288487 ) ) ;
#8299 = ORIENTED_EDGE ( 'NONE', *, *, #73425, .T. ) ;
#8298 = DIRECTION ( 'NONE',  ( -0.7071067811865486830, 0.7071067811865464625, 0.000000000000000000 ) ) ;
#8300 = ORIENTED_EDGE ( 'NONE', *, *, #106751, .T. ) ;
#8301 = DIRECTION ( 'NONE',  ( -0.6830127018922181881, 0.6830127018922202975, -0.2588190451025214056 ) ) ;
#8302 = DIRECTION ( 'NONE',  ( -0.7071067811865487940, 0.7071067811865463515, 0.000000000000000000 ) ) ;
#8303 = EDGE_LOOP ( 'NONE', ( #51416, #41280, #113016 ) ) ;
#8304 = CARTESIAN_POINT ( 'NONE',  ( 109.1625270504628986, 7.949999999999998401, 1.460391307983218338E-15 ) ) ;
#8305 = EDGE_LOOP ( 'NONE', ( #44939, #106234, #43319, #43706 ) ) ;
#8306 = ORIENTED_EDGE ( 'NONE', *, *, #118474, .F. ) ;
#8307 = ORIENTED_EDGE ( 'NONE', *, *, #117298, .T. ) ;
#8308 = VECTOR ( 'NONE', #8354, 1000.000000000000000 ) ;
#8309 = EDGE_CURVE ( 'NONE', #23928, #16647, #44172, .T. ) ;
#8310 = LINE ( 'NONE', #120654, #24022 ) ;
#8311 = DIRECTION ( 'NONE',  ( -0.7071067811865486830, 0.7071067811865464625, 0.000000000000000000 ) ) ;
#8312 = EDGE_CURVE ( 'NONE', #113821, #56274, #34007, .T. ) ;
#8313 = CARTESIAN_POINT ( 'NONE',  ( 34.45011844616453800, 0.002304141593939786677, 5.000000000000001776 ) ) ;
#8314 = CARTESIAN_POINT ( 'NONE',  ( 62.99451991528749772, 28.92564299267982264, 4.000000000000000000 ) ) ;
#8315 = DIRECTION ( 'NONE',  ( -0.6830127018922180770, -0.6830127018922204085, -0.2588190451025213501 ) ) ;
#8316 = ORIENTED_EDGE ( 'NONE', *, *, #33135, .F. ) ;
#8317 = PLANE ( 'NONE',  #297 ) ;
#8318 = VERTEX_POINT ( 'NONE', #12224 ) ;
#8319 = DIRECTION ( 'NONE',  ( 0.7071067811865486830, -0.7071067811865464625, -0.000000000000000000 ) ) ;
#8320 = ADVANCED_FACE ( 'NONE', ( #56514 ), #21692, .F. ) ;
#8321 = VECTOR ( 'NONE', #80676, 999.9999999999998863 ) ;
#8322 = CARTESIAN_POINT ( 'NONE',  ( 32.35373647476855297, -5.808823158059035485, -5.808823158059033709 ) ) ;
#8323 = VECTOR ( 'NONE', #123475, 999.9999999999998863 ) ;
#8324 = ORIENTED_EDGE ( 'NONE', *, *, #62035, .T. ) ;
#8325 = DIRECTION ( 'NONE',  ( -0.000000000000000000, -0.3543493200069152693, 0.9351131265310292928 ) ) ;
#8326 = CARTESIAN_POINT ( 'NONE',  ( 11.67183060077639212, -18.74070752338409207, 4.000000000000000000 ) ) ;
#8327 = ORIENTED_EDGE ( 'NONE', *, *, #64477, .F. ) ;
#8328 = VERTEX_POINT ( 'NONE', #42032 ) ;
#8329 = EDGE_CURVE ( 'NONE', #66627, #118938, #81985, .T. ) ;
#8330 = CARTESIAN_POINT ( 'NONE',  ( 25.49999999999983302, 16.08746187583908238, 4.000000000000000000 ) ) ;
#8331 = UNCERTAINTY_MEASURE_WITH_UNIT (LENGTH_MEASURE( 1.000000000000000082E-05 ), #50018, 'distance_accuracy_value', 'NONE');
#8332 = CARTESIAN_POINT ( 'NONE',  ( -3.489213562373097322, -27.52281430457057709, 5.000000000000000000 ) ) ;
#8333 = AXIS2_PLACEMENT_3D ( 'NONE', #122128, #114638, #25485 ) ;
#8334 = CARTESIAN_POINT ( 'NONE',  ( 34.17183060077621803, -2.240707523384275035, 4.000000000000000000 ) ) ;
#8335 = FACE_OUTER_BOUND ( 'NONE', #97810, .T. ) ;
#8336 = CARTESIAN_POINT ( 'NONE',  ( 69.18293019189809456, -1.637169565754159173, -6.109999999999999432 ) ) ;
#8337 = CARTESIAN_POINT ( 'NONE',  ( 73.28752705046288440, 0.000000000000000000, -7.949999999999998401 ) ) ;
#8338 = DIRECTION ( 'NONE',  ( 0.7071067811865487940, 0.7071067811865463515, 0.000000000000000000 ) ) ;
#8339 = PLANE ( 'NONE',  #39553 ) ;
#8340 = ADVANCED_FACE ( 'NONE', ( #44925 ), #77529, .F. ) ;
#8341 = CARTESIAN_POINT ( 'NONE',  ( -29.99451991528749417, 28.92564299267958816, 4.000000000000000000 ) ) ;
#8342 = ORIENTED_EDGE ( 'NONE', *, *, #67563, .T. ) ;
#8343 = CARTESIAN_POINT ( 'NONE',  ( -17.61782366839360847, 8.969638207445433054, 4.000000000000000000 ) ) ;
#8344 = ORIENTED_EDGE ( 'NONE', *, *, #45209, .F. ) ;
#8345 = DIRECTION ( 'NONE',  ( 1.000000000000000000, 0.000000000000000000, 0.000000000000000000 ) ) ;
#8346 = FACE_OUTER_BOUND ( 'NONE', #58279, .T. ) ;
#8347 = ORIENTED_EDGE ( 'NONE', *, *, #119887, .T. ) ;
#8348 = CARTESIAN_POINT ( 'NONE',  ( 11.99999999999991651, -21.03360074219752462, 5.000000000000000000 ) ) ;
#8350 = VERTEX_POINT ( 'NONE', #109407 ) ;
#8349 = DIRECTION ( 'NONE',  ( 0.6830127018922180770, -0.6830127018922204085, -0.2588190451025213501 ) ) ;
#8351 = FACE_OUTER_BOUND ( 'NONE', #45483, .T. ) ;
#8352 = ADVANCED_FACE ( 'NONE', ( #108655 ), #120241, .T. ) ;
#8353 = CARTESIAN_POINT ( 'NONE',  ( -12.18398860626900060, 28.73617430169795739, 5.000000000000000000 ) ) ;
#8354 = DIRECTION ( 'NONE',  ( -0.7071067811865486830, -0.7071067811865464625, 0.000000000000000000 ) ) ;
#8355 = ORIENTED_EDGE ( 'NONE', *, *, #75912, .T. ) ;
#8356 = ORIENTED_EDGE ( 'NONE', *, *, #50718, .F. ) ;
#8357 = DIRECTION ( 'NONE',  ( 0.7071067811865487940, -0.7071067811865463515, 0.000000000000000000 ) ) ;
#8358 = CARTESIAN_POINT ( 'NONE',  ( 16.75173015016484968, 4.202752102959690472E-16, 0.000000000000000000 ) ) ;
#8359 = CARTESIAN_POINT ( 'NONE',  ( 86.70419371712955581, -6.884901960086285300, -3.975000000000000089 ) ) ;
#8360 = CARTESIAN_POINT ( 'NONE',  ( 7.499999999999947597, -17.91344420646041513, 1.358650452708480838 ) ) ;
#8361 = EDGE_CURVE ( 'NONE', #9887, #19214, #65946, .T. ) ;
#8362 = CARTESIAN_POINT ( 'NONE',  ( -48.18398860626899705, 28.73617430169820608, 5.000000000000000000 ) ) ;
#8363 = ORIENTED_EDGE ( 'NONE', *, *, #11562, .F. ) ;
#8364 = CARTESIAN_POINT ( 'NONE',  ( 42.18398860626899705, 28.73617430169816700, 5.000000000000000000 ) ) ;
#8365 = CARTESIAN_POINT ( 'NONE',  ( -36.18398860626899705, 28.73617430169812437, 5.000000000000000000 ) ) ;
#8366 = CARTESIAN_POINT ( 'NONE',  ( 30.62500000000000355, 6.094999999999989981, -1.119633336120465690E-15 ) ) ;
#8367 = VECTOR ( 'NONE', #80656, 1000.000000000000000 ) ;
#8368 = ORIENTED_EDGE ( 'NONE', *, *, #54023, .T. ) ;
#8369 = EDGE_CURVE ( 'NONE', #95585, #117852, #120989, .T. ) ;
#8370 = LINE ( 'NONE', #52620, #7372 ) ;
#8371 = ORIENTED_EDGE ( 'NONE', *, *, #127305, .T. ) ;
#8372 = EDGE_CURVE ( 'NONE', #66020, #30015, #9336, .T. ) ;
#8373 = CARTESIAN_POINT ( 'NONE',  ( 78.60459685856477563, 1.637169565754164946, -6.109999999999999432 ) ) ;
#8374 = LINE ( 'NONE', #96812, #105649 ) ;
#8375 = VECTOR ( 'NONE', #128567, 1000.000000000000000 ) ;
#8376 = CYLINDRICAL_SURFACE ( 'NONE', #111927, 0.5000000000000004441 ) ;
#8377 = ORIENTED_EDGE ( 'NONE', *, *, #86002, .F. ) ;
#8378 = CARTESIAN_POINT ( 'NONE',  ( -6.938893903907228378E-15, -22.22500000000000142, 4.412002311790018894 ) ) ;
#8379 = CARTESIAN_POINT ( 'NONE',  ( 13.29826936130429260, 2.500000000000003109, 3.061616997868386592E-16 ) ) ;
#8380 = LINE ( 'NONE', #143222, #99507 ) ;
#8381 = ADVANCED_FACE ( 'NONE', ( #20959 ), #32581, .F. ) ;
#8382 = DIRECTION ( 'NONE',  ( 1.000000000000000000, 0.000000000000000000, 0.000000000000000000 ) ) ;
#8384 = EDGE_LOOP ( 'NONE', ( #62204, #81962, #115931, #2503 ) ) ;
#8383 = CARTESIAN_POINT ( 'NONE',  ( 8.671830600776408104, -18.74070752338409562, 4.000000000000000000 ) ) ;
#8385 = CARTESIAN_POINT ( 'NONE',  ( 131.8806778009766276, -49.14999999999999147, -40.92499999999998295 ) ) ;
#8386 = DIRECTION ( 'NONE',  ( -0.7071067811865487940, 0.7071067811865463515, -0.000000000000000000 ) ) ;
#8387 = CARTESIAN_POINT ( 'NONE',  ( 6.792893218813412126, -17.24070752338409918, 5.000000000000000000 ) ) ;
#8388 = LINE ( 'NONE', #63566, #51635 ) ;
#8389 = ORIENTED_EDGE ( 'NONE', *, *, #15356, .F. ) ;
#8390 = CIRCLE ( 'NONE', #135730, 2.500000000000000888 ) ;
#8391 = EDGE_LOOP ( 'NONE', ( #102492, #58422, #60287, #71616, #12586 ) ) ;
#8392 = CARTESIAN_POINT ( 'NONE',  ( 73.79209685856477563, -5.291415217122921177, 3.054999999999999272 ) ) ;
#8393 = ORIENTED_EDGE ( 'NONE', *, *, #52343, .F. ) ;
#8394 = VECTOR ( 'NONE', #41085, 1000.000000000000000 ) ;
#8395 = DIRECTION ( 'NONE',  ( 0.3543493200069162685, -0.000000000000000000, -0.9351131265310288487 ) ) ;
#8396 = DIRECTION ( 'NONE',  ( -1.000000000000000000, -1.224606353822377258E-16, -0.000000000000000000 ) ) ;
#8397 = PLANE ( 'NONE',  #124477 ) ;
#8398 = ORIENTED_EDGE ( 'NONE', *, *, #117361, .F. ) ;
#8399 = CARTESIAN_POINT ( 'NONE',  ( -7.499999999999947597, 21.43112307739195899, 4.000000000000000000 ) ) ;
#8400 = DIRECTION ( 'NONE',  ( 0.7071067811865487940, -0.7071067811865463515, 0.000000000000000000 ) ) ;
#8401 = ORIENTED_EDGE ( 'NONE', *, *, #50698, .T. ) ;
#8402 = AXIS2_PLACEMENT_3D ( 'NONE', #98352, #87474, #129520 ) ;
#8403 = CARTESIAN_POINT ( 'NONE',  ( 0.8137007348675845408, -1.054356994394161307, 3.918334772610103212 ) ) ;
#8404 = CARTESIAN_POINT ( 'NONE',  ( -17.99999999999986855, -9.412538124160658271, 4.000000000000000000 ) ) ;
#8405 = DIRECTION ( 'NONE',  ( 0.7071067811865486830, -0.7071067811865464625, -0.000000000000000000 ) ) ;
#8406 = ORIENTED_EDGE ( 'NONE', *, *, #12714, .T. ) ;
#8407 = ORIENTED_EDGE ( 'NONE', *, *, #95323, .T. ) ;
#8408 = STYLED_ITEM ( 'NONE', ( #109723 ), #111305 ) ;
#8409 = FACE_BOUND ( 'NONE', #141749, .T. ) ;
#8410 = DIRECTION ( 'NONE',  ( -0.7071067811865486830, 0.7071067811865464625, 0.000000000000000000 ) ) ;
#8411 = CARTESIAN_POINT ( 'NONE',  ( 128.1594355792471163, -6.349999999999998757, -1.701477371937630378 ) ) ;
#8412 = SURFACE_STYLE_FILL_AREA ( #41087 ) ;
#8413 = VECTOR ( 'NONE', #142553, 1000.000000000000000 ) ;
#8414 = AXIS2_PLACEMENT_3D ( 'NONE', #103982, #135929, #36607 ) ;
#8415 = DIRECTION ( 'NONE',  ( -0.000000000000000000, 0.000000000000000000, 1.000000000000000000 ) ) ;
#8416 = ORIENTED_EDGE ( 'NONE', *, *, #35686, .F. ) ;
#8418 = EDGE_CURVE ( 'NONE', #79752, #126576, #128219, .T. ) ;
#8417 = AXIS2_PLACEMENT_3D ( 'NONE', #44307, #141459, #63907 ) ;
#8420 = ORIENTED_EDGE ( 'NONE', *, *, #88850, .T. ) ;
#8419 = AXIS2_PLACEMENT_3D ( 'NONE', #94653, #48313, #38172 ) ;
#8421 = ORIENTED_EDGE ( 'NONE', *, *, #72908, .T. ) ;
#8422 = EDGE_CURVE ( 'NONE', #56693, #69078, #65223, .T. ) ;
#8423 = VERTEX_POINT ( 'NONE', #54356 ) ;
#8424 = ADVANCED_FACE ( 'NONE', ( #11487 ), #110105, .F. ) ;
#8425 = AXIS2_PLACEMENT_3D ( 'NONE', #119138, #74224, #86539 ) ;
#8426 = EDGE_CURVE ( 'NONE', #95580, #110421, #133326, .T. ) ;
#8427 = PLANE ( 'NONE',  #80294 ) ;
#8428 = DIRECTION ( 'NONE',  ( -0.6830127018922180770, -0.6830127018922204085, -0.2588190451025213501 ) ) ;
#8429 = ORIENTED_EDGE ( 'NONE', *, *, #139279, .T. ) ;
#8430 = CARTESIAN_POINT ( 'NONE',  ( 5.999999999999956479, 10.21212019023809425, -2.019456568337813618 ) ) ;
#8431 = FACE_OUTER_BOUND ( 'NONE', #37648, .T. ) ;
#8432 = CARTESIAN_POINT ( 'NONE',  ( 54.18398860626899705, 28.73617430169825226, 5.000000000000000000 ) ) ;
#8433 = CARTESIAN_POINT ( 'NONE',  ( 19.82816939922339827, -11.24070752338416490, 4.000000000000000000 ) ) ;
#8434 = CARTESIAN_POINT ( 'NONE',  ( 0.6638242047990419170, 1.145087188747829554, 3.945200277712134884 ) ) ;
#8435 = ORIENTED_EDGE ( 'NONE', *, *, #54856, .T. ) ;
#8436 = DIRECTION ( 'NONE',  ( 1.000000000000000000, 0.000000000000000000, 0.000000000000000000 ) ) ;
#8437 = CARTESIAN_POINT ( 'NONE',  ( -34.92500000000001137, 22.22500000000000142, 4.500000000000000888 ) ) ;
#8438 = ADVANCED_FACE ( 'NONE', ( #10779 ), #143455, .F. ) ;
#8439 = EDGE_LOOP ( 'NONE', ( #116205, #40188, #80561, #1678, #48501, #54430, #75050, #32377, #85686, #67372, #12732, #117488, #77270, #45063, #78163, #45850, #56486, #59786, #34834, #87725, #18343, #45859, #85137, #78966, #90063, #129037, #104834, #25897, #120091, #99854, #49346, #34602, #89588, #93558, #25627, #136956, #135091, #19962, #101101, #128821, #55730, #14420, #103492, #133848, #91553, #108559, #79515, #49077, #17830, #81463, #45027, #100112, #132014, #115819, #67460, #70467, #79197, #89364, #93014, #96089, #88001, #69804, #116746, #3975, #131956, #56600, #65930, #137007, #92932, #39828, #111856, #114689, #92312, #65058, #95664, #82493, #80044, #73536, #29085, #124784, #82603, #124503, #109596, #85096, #31050, #96321, #13328, #11755, #55763, #132687, #19155, #51883, #47116, #83134, #61645, #84972, #94015, #17633, #100447, #104628, #88695, #15426, #21846, #88106, #39479, #30980, #8564, #19916, #92589, #15684, #140590, #129596, #130954, #40036, #69127, #84861, #51632, #2218, #64516, #73874, #39572, #50448, #55420, #23522, #141251, #110761, #87642, #20053, #18326, #76101, #104419, #9856, #53450, #11339, #136908, #22862, #62081, #80292, #654, #80061, #118677, #60620, #134783, #3446, #103285, #127752, #3790, #16988, #90342, #7947, #132801, #93874, #115537, #73124, #79819, #140944, #105162, #110819, #119872, #31043, #10860, #85177, #109564, #140235, #87789 ) ) ;
#8440 = CARTESIAN_POINT ( 'NONE',  ( -34.92500000000001137, 20.71849043720401795, 4.759050581649336920 ) ) ;
#8441 = ORIENTED_EDGE ( 'NONE', *, *, #73373, .T. ) ;
#8442 = VERTEX_POINT ( 'NONE', #630 ) ;
#8443 = EDGE_CURVE ( 'NONE', #104684, #49293, #23077, .T. ) ;
#8444 = ORIENTED_EDGE ( 'NONE', *, *, #142641, .T. ) ;
#8445 = CARTESIAN_POINT ( 'NONE',  ( 67.52126352523144703, -4.472830434245838482, -4.472830434245840259 ) ) ;
#8446 = ORIENTED_EDGE ( 'NONE', *, *, #122013, .F. ) ;
#8447 = EDGE_LOOP ( 'NONE', ( #17832, #98399, #47790, #23353 ) ) ;
#8448 = EDGE_CURVE ( 'NONE', #57879, #93602, #25977, .T. ) ;
#8449 = LINE ( 'NONE', #52702, #113707 ) ;
#8450 = VECTOR ( 'NONE', #116568, 1000.000000000000227 ) ;
#8451 = DIRECTION ( 'NONE',  ( -0.6830127018922180770, -0.6830127018922204085, -0.2588190451025213501 ) ) ;
#8452 = CARTESIAN_POINT ( 'NONE',  ( 97.27126352523143282, 4.472830434245838482, 4.472830434245842035 ) ) ;
#8453 = LINE ( 'NONE', #20793, #77571 ) ;
#8454 = FACE_OUTER_BOUND ( 'NONE', #27915, .T. ) ;
#8455 = VERTEX_POINT ( 'NONE', #68792 ) ;
#8456 = LINE ( 'NONE', #83218, #99586 ) ;
#8457 = EDGE_CURVE ( 'NONE', #60173, #89845, #1336, .T. ) ;
#8458 = VECTOR ( 'NONE', #2893, 1000.000000000000114 ) ;
#8459 = LINE ( 'NONE', #128850, #137307 ) ;
#8460 =( BOUNDED_CURVE ( )  B_SPLINE_CURVE ( 3, ( #127243, #75053, #51139, #27946 ),
 .UNSPECIFIED., .F., .F. ) 
 B_SPLINE_CURVE_WITH_KNOTS ( ( 4, 4 ),
 ( 1.864375635226928729, 1.933014472006540752 ),
 .UNSPECIFIED. ) 
 CURVE ( )  GEOMETRIC_REPRESENTATION_ITEM ( )  RATIONAL_B_SPLINE_CURVE ( ( 1.000000000000000000, 0.9996074310407765395, 0.9996074310407765395, 1.000000000000000000 ) ) 
 REPRESENTATION_ITEM ( '' )  );
#8461 = DIRECTION ( 'NONE',  ( 0.7071067811865487940, 0.7071067811865463515, -0.000000000000000000 ) ) ;
#8462 = ORIENTED_EDGE ( 'NONE', *, *, #124054, .F. ) ;
#8463 = DIRECTION ( 'NONE',  ( 0.6830127018922181881, 0.6830127018922202975, -0.2588190451025214056 ) ) ;
#8464 = EDGE_LOOP ( 'NONE', ( #134851, #124825, #8327 ) ) ;
#8465 = ORIENTED_EDGE ( 'NONE', *, *, #41221, .F. ) ;
#8466 = ORIENTED_EDGE ( 'NONE', *, *, #112375, .F. ) ;
#8467 = EDGE_CURVE ( 'NONE', #139864, #78508, #69502, .T. ) ;
#8469 = AXIS2_PLACEMENT_3D ( 'NONE', #93796, #27822, #72088 ) ;
#8468 = CARTESIAN_POINT ( 'NONE',  ( 126.4954301918981230, 5.291415217122916737, 3.055000000000001936 ) ) ;
#8470 = VERTEX_POINT ( 'NONE', #3475 ) ;
#8471 =( BOUNDED_CURVE ( )  B_SPLINE_CURVE ( 3, ( #98040, #121197, #10983, #130687 ),
 .UNSPECIFIED., .F., .T. ) 
 B_SPLINE_CURVE_WITH_KNOTS ( ( 4, 4 ),
 ( 2.001653308786168317, 3.503810798801451742 ),
 .UNSPECIFIED. ) 
 CURVE ( )  GEOMETRIC_REPRESENTATION_ITEM ( )  RATIONAL_B_SPLINE_CURVE ( ( 1.000000000000000000, 0.8206354192515236123, 0.8206354192515236123, 1.000000000000000000 ) ) 
 REPRESENTATION_ITEM ( '' )  );
#8472 = CARTESIAN_POINT ( 'NONE',  ( 57.29974487139158157, -27.71228299555246011, 4.000000000000000000 ) ) ;
#8473 = DIRECTION ( 'NONE',  ( 0.6830127018922180770, -0.6830127018922204085, -0.2588190451025213501 ) ) ;
#8474 = VECTOR ( 'NONE', #135778, 1000.000000000000000 ) ;
#8475 = CARTESIAN_POINT ( 'NONE',  ( -9.489213562373095101, -27.52281430457062328, 5.000000000000000000 ) ) ;
#8476 = EDGE_LOOP ( 'NONE', ( #137256, #115609, #113109, #142312 ) ) ;
#8477 = CARTESIAN_POINT ( 'NONE',  ( 0.7113915074196556221, -49.19295221407733010, 41.21232802153977559 ) ) ;
#8478 = VERTEX_POINT ( 'NONE', #12932 ) ;
#8479 = CIRCLE ( 'NONE', #3821, 2.500000000000000888 ) ;
#8480 = CARTESIAN_POINT ( 'NONE',  ( 2.457903141435219485, 6.871911579029515771, 3.967499999999989146 ) ) ;
#8481 = CARTESIAN_POINT ( 'NONE',  ( 15.05159235450332034, 9.902892378096218942E-16, 0.000000000000000000 ) ) ;
#8482 = AXIS2_PLACEMENT_3D ( 'NONE', #10408, #64826, #52497 ) ;
#8483 = CARTESIAN_POINT ( 'NONE',  ( 38.47916666666665719, -7.950000000000000178, 2.130196079827424427 ) ) ;
#8484 = VERTEX_POINT ( 'NONE', #114402 ) ;
#8485 = EDGE_LOOP ( 'NONE', ( #112428, #92301, #140328, #102609 ) ) ;
#8486 = EDGE_CURVE ( 'NONE', #745, #130461, #58664, .T. ) ;
#8487 = VECTOR ( 'NONE', #66194, 999.9999999999998863 ) ;
#8488 = ORIENTED_EDGE ( 'NONE', *, *, #98197, .F. ) ;
#8489 = DIRECTION ( 'NONE',  ( -0.000000000000000000, 0.3543493200069153248, 0.9351131265310292928 ) ) ;
#8490 = DIRECTION ( 'NONE',  ( -0.7071067811865486830, -0.7071067811865464625, 0.000000000000000000 ) ) ;
#8491 = CARTESIAN_POINT ( 'NONE',  ( -8.510786437626906675, -27.52281430457049183, 5.000000000000000000 ) ) ;
#8492 = DIRECTION ( 'NONE',  ( -1.084202172485504434E-16, 1.000000000000000000, -0.000000000000000000 ) ) ;
#8493 = CARTESIAN_POINT ( 'NONE',  ( 0.000000000000000000, 0.000000000000000000, 5.000000000000000000 ) ) ;
#8494 = DIRECTION ( 'NONE',  ( -0.7071067811865486830, -0.7071067811865464625, 0.000000000000000000 ) ) ;
#8495 = CARTESIAN_POINT ( 'NONE',  ( 32.95876352523143282, 0.000000000000000000, -6.110000000000001208 ) ) ;
#8496 = ADVANCED_FACE ( 'NONE', ( #68100 ), #79697, .F. ) ;
#8497 = FACE_OUTER_BOUND ( 'NONE', #1428, .T. ) ;
#8498 = DIRECTION ( 'NONE',  ( -0.7071067811865487940, 0.7071067811865463515, 0.000000000000000000 ) ) ;
#8499 = ORIENTED_EDGE ( 'NONE', *, *, #7937, .F. ) ;
#8500 = DIRECTION ( 'NONE',  ( 0.7071067811865486830, -0.7071067811865464625, -0.000000000000000000 ) ) ;
#8501 = CARTESIAN_POINT ( 'NONE',  ( -24.29974487139158867, -27.71228299555223273, 4.000000000000000000 ) ) ;
#8502 = VERTEX_POINT ( 'NONE', #36150 ) ;
#8503 = CARTESIAN_POINT ( 'NONE',  ( 34.00193056682073944, -22.22500000000000142, 4.500000000000000888 ) ) ;
#8505 = ORIENTED_EDGE ( 'NONE', *, *, #93613, .T. ) ;
#8504 = CARTESIAN_POINT ( 'NONE',  ( 55.47138350052864553, -49.14501756083437556, -40.36361034346621324 ) ) ;
#8506 = EDGE_CURVE ( 'NONE', #21745, #29986, #48437, .T. ) ;
#8507 = DIRECTION ( 'NONE',  ( 0.7071067811865486830, -0.7071067811865464625, -0.000000000000000000 ) ) ;
#8508 = ORIENTED_EDGE ( 'NONE', *, *, #108832, .F. ) ;
#8509 = DIRECTION ( 'NONE',  ( -0.7071067811865487940, 0.7071067811865463515, -0.000000000000000000 ) ) ;
#8510 = ORIENTED_EDGE ( 'NONE', *, *, #121695, .T. ) ;
#8511 = CARTESIAN_POINT ( 'NONE',  ( -19.30725242247703122, 9.139235811853158253, 4.261625515810906428 ) ) ;
#8512 = ORIENTED_EDGE ( 'NONE', *, *, #137782, .T. ) ;
#8513 = AXIS2_PLACEMENT_3D ( 'NONE', #17703, #136642, #103293 ) ;
#8514 = VECTOR ( 'NONE', #19681, 1000.000000000000000 ) ;
#8516 = CARTESIAN_POINT ( 'NONE',  ( 119.5166937171295558, 7.950000000000001066, -2.130196079827421318 ) ) ;
#8515 = VECTOR ( 'NONE', #142675, 1000.000000000000000 ) ;
#8517 = CARTESIAN_POINT ( 'NONE',  ( 27.00000000000000355, -4.083527258847093222, -4.862849486279972488 ) ) ;
#8518 =( LENGTH_UNIT ( ) NAMED_UNIT ( * ) SI_UNIT ( .MILLI., .METRE. ) );
#8519 = PLANE ( 'NONE',  #60700 ) ;
#8520 = DIRECTION ( 'NONE',  ( 0.000000000000000000, 0.000000000000000000, -1.000000000000000000 ) ) ;
#8521 = AXIS2_PLACEMENT_3D ( 'NONE', #35391, #99894, #44854 ) ;
#8522 = CARTESIAN_POINT ( 'NONE',  ( 3.791666666666666963, -3.047499999999994547, 5.278424836066145431 ) ) ;
#8523 = CARTESIAN_POINT ( 'NONE',  ( 13.10373647476855297, 5.808823158059035485, 5.808823158059032821 ) ) ;
#8524 = VECTOR ( 'NONE', #111857, 1000.000000000000227 ) ;
#8525 = CARTESIAN_POINT ( 'NONE',  ( -33.48921356237309510, -27.52281430457078670, 5.000000000000000000 ) ) ;
#8526 = CARTESIAN_POINT ( 'NONE',  ( 34.47516574401890921, 15.02806734111565490, 4.998110765256834398 ) ) ;
#8527 = ORIENTED_EDGE ( 'NONE', *, *, #137713, .T. ) ;
#8528 = VERTEX_POINT ( 'NONE', #46339 ) ;
#8529 = LINE ( 'NONE', #73840, #9538 ) ;
#8530 = ORIENTED_EDGE ( 'NONE', *, *, #37133, .T. ) ;
#8531 = ADVANCED_FACE ( 'NONE', ( #91931 ), #124572, .F. ) ;
#8532 = CARTESIAN_POINT ( 'NONE',  ( 21.48921356237309155, -27.52281430457070499, 5.000000000000000000 ) ) ;
#8533 = CARTESIAN_POINT ( 'NONE',  ( 16.49999999999989697, 5.696342897626525570, -7.587980461218362116 ) ) ;
#8534 =( NAMED_UNIT ( * ) SI_UNIT ( $, .STERADIAN. ) SOLID_ANGLE_UNIT ( ) );
#8535 = CARTESIAN_POINT ( 'NONE',  ( 131.3130295073068226, -48.90295371244954481, -39.18578444878617262 ) ) ;
#8536 = ORIENTED_EDGE ( 'NONE', *, *, #33672, .T. ) ;
#8537 = PLANE ( 'NONE',  #104292 ) ;
#8538 = CARTESIAN_POINT ( 'NONE',  ( 93.02083333333331439, 7.949999999999998401, 2.130196079827431532 ) ) ;
#8539 = CARTESIAN_POINT ( 'NONE',  ( -9.005480084712511157, 28.92564299267931816, 4.000000000000000000 ) ) ;
#8540 = EDGE_CURVE ( 'NONE', #93434, #68280, #91259, .T. ) ;
#8541 = ADVANCED_FACE ( 'NONE', ( #123880 ), #113687, .F. ) ;
#8542 = CARTESIAN_POINT ( 'NONE',  ( -1.807144792967049773E-15, -50.24077216217763464, 35.40405119785170029 ) ) ;
#8544 = ORIENTED_EDGE ( 'NONE', *, *, #58790, .T. ) ;
#8543 = DIRECTION ( 'NONE',  ( -0.7071067811865486830, -0.7071067811865464625, 0.000000000000000000 ) ) ;
#8545 = CARTESIAN_POINT ( 'NONE',  ( 0.000000000000000000, 0.000000000000000000, 5.000000000000000000 ) ) ;
#8546 = VECTOR ( 'NONE', #91279, 1000.000000000000114 ) ;
#8547 = CARTESIAN_POINT ( 'NONE',  ( -55.65468426143998215, -25.33999999999998565, 0.000000000000000000 ) ) ;
#8548 = CARTESIAN_POINT ( 'NONE',  ( -42.18398860626899705, 28.73617430169816700, 5.000000000000000000 ) ) ;
#8549 = CARTESIAN_POINT ( 'NONE',  ( 54.24578869845078088, -47.96374157527325366, 37.32649486623284929 ) ) ;
#8550 = ORIENTED_EDGE ( 'NONE', *, *, #60724, .T. ) ;
#8551 = EDGE_LOOP ( 'NONE', ( #102201, #135215, #82789, #34334 ) ) ;
#8552 = ORIENTED_EDGE ( 'NONE', *, *, #41213, .F. ) ;
#8553 = CARTESIAN_POINT ( 'NONE',  ( 105.4379301918981042, -6.110000000000001208, 1.637169565754158951 ) ) ;
#8554 = AXIS2_PLACEMENT_3D ( 'NONE', #67115, #1109, #134523 ) ;
#8555 = ORIENTED_EDGE ( 'NONE', *, *, #6486, .T. ) ;
#8556 = CARTESIAN_POINT ( 'NONE',  ( 130.9531400719712906, -48.66302742222553235, 38.53170190052306054 ) ) ;
#8557 = AXIS2_PLACEMENT_3D ( 'NONE', #104149, #4092, #49116 ) ;
#8558 = DIRECTION ( 'NONE',  ( -0.000000000000000000, -0.3543493200069152693, 0.9351131265310292928 ) ) ;
#8559 = EDGE_LOOP ( 'NONE', ( #35310, #126674, #102379, #21360 ) ) ;
#8560 = EDGE_CURVE ( 'NONE', #126893, #65352, #14381, .T. ) ;
#8561 = DIRECTION ( 'NONE',  ( 1.000000000000000000, 1.224606353822377258E-16, 0.000000000000000000 ) ) ;
#8562 = DIRECTION ( 'NONE',  ( 0.7071067811865487940, 0.7071067811865463515, -0.000000000000000000 ) ) ;
#8563 = CARTESIAN_POINT ( 'NONE',  ( 96.74543019189810877, -5.291415217122918513, -3.055000000000000160 ) ) ;
#8564 = ORIENTED_EDGE ( 'NONE', *, *, #44736, .T. ) ;
#8565 = CARTESIAN_POINT ( 'NONE',  ( 33.29974487139158867, -27.71228299555229313, 4.000000000000000000 ) ) ;
#8566 = DIRECTION ( 'NONE',  ( -0.7071067811865487940, 0.7071067811865463515, 0.000000000000000000 ) ) ;
#8567 = VECTOR ( 'NONE', #102211, 1000.000000000000000 ) ;
#8568 = DIRECTION ( 'NONE',  ( -0.7071067811865486830, -0.7071067811865464625, 0.000000000000000000 ) ) ;
#8569 = CARTESIAN_POINT ( 'NONE',  ( -28.49999999999980460, -20.53675388469233098, 2.352720554255826713 ) ) ;
#8570 = ORIENTED_EDGE ( 'NONE', *, *, #3217, .T. ) ;
#8571 = ORIENTED_EDGE ( 'NONE', *, *, #129435, .T. ) ;
#8572 = ORIENTED_EDGE ( 'NONE', *, *, #15620, .F. ) ;
#8573 = DIRECTION ( 'NONE',  ( -1.000000000000000000, -0.000000000000000000, -0.000000000000000000 ) ) ;
#8574 = CARTESIAN_POINT ( 'NONE',  ( 4.499999999999967137, -17.91344420646041868, 1.358650452708475287 ) ) ;
#8575 = CARTESIAN_POINT ( 'NONE',  ( 15.96290314143521805, -3.967499999999994476, 6.871911579029513106 ) ) ;
#8576 = CARTESIAN_POINT ( 'NONE',  ( 16.56687199751246808, -21.74070752338406720, 6.915939825044033817 ) ) ;
#8577 = CARTESIAN_POINT ( 'NONE',  ( 34.92499999999998295, 4.701930566820937685, 4.500000000000000888 ) ) ;
#8578 = SHAPE_REPRESENTATION_RELATIONSHIP ( 'NONE' , 'NONE' ,  #9754, #74116 ) ;
#8579 = ADVANCED_FACE ( 'NONE', ( #4144 ), #92632, .F. ) ;
#8580 = VERTEX_POINT ( 'NONE', #37577 ) ;
#8581 = VECTOR ( 'NONE', #4476, 999.9999999999998863 ) ;
#8582 = EDGE_LOOP ( 'NONE', ( #43104, #76849, #66591, #112566, #8550 ) ) ;
#8583 = ADVANCED_FACE ( 'NONE', ( #126014 ), #26684, .T. ) ;
#8584 = CARTESIAN_POINT ( 'NONE',  ( -69.48921356237309510, -27.52281430457103895, 5.000000000000000000 ) ) ;
#8585 = ORIENTED_EDGE ( 'NONE', *, *, #100344, .F. ) ;
#8586 = VERTEX_POINT ( 'NONE', #123163 ) ;
#8587 = EDGE_CURVE ( 'NONE', #105943, #130911, #135172, .T. ) ;
#8588 = EDGE_CURVE ( 'NONE', #61667, #11699, #2779, .T. ) ;
#8589 = DIRECTION ( 'NONE',  ( 1.000000000000000000, 0.000000000000000000, 0.000000000000000000 ) ) ;
#8590 = DIRECTION ( 'NONE',  ( 0.6830127018922181881, 0.6830127018922202975, -0.2588190451025214056 ) ) ;
#8591 = ORIENTED_EDGE ( 'NONE', *, *, #137345, .T. ) ;
#8592 = CARTESIAN_POINT ( 'NONE',  ( -24.64318742751724045, -20.24070752338407786, 21.22881796311207481 ) ) ;
#8593 = DIRECTION ( 'NONE',  ( 0.5735764363510451602, 0.8191520442889924647, 0.000000000000000000 ) ) ;
#8594 = DIRECTION ( 'NONE',  ( -0.7071067811865486830, -0.7071067811865464625, 0.000000000000000000 ) ) ;
#8595 = CARTESIAN_POINT ( 'NONE',  ( 24.89279686680829329, 1.949462372756121775, 4.672399651904028062 ) ) ;
#8596 = DIRECTION ( 'NONE',  ( 0.000000000000000000, -1.000000000000000000, 0.000000000000000000 ) ) ;
#8597 = VERTEX_POINT ( 'NONE', #13643 ) ;
#8598 = SURFACE_STYLE_FILL_AREA ( #31141 ) ;
#8599 = EDGE_CURVE ( 'NONE', #34187, #5268, #57925, .T. ) ;
#8600 = ORIENTED_EDGE ( 'NONE', *, *, #71170, .F. ) ;
#8601 = CARTESIAN_POINT ( 'NONE',  ( 25.39999999999999858, 4.836323036001208386, -6.294117125145909597 ) ) ;
#8602 = CARTESIAN_POINT ( 'NONE',  ( 8.524873872149486331, 14.25929247661557575, 9.797011795316656446 ) ) ;
#8603 = ORIENTED_EDGE ( 'NONE', *, *, #73097, .T. ) ;
#8604 = ADVANCED_FACE ( 'NONE', ( #17905 ), #62912, .F. ) ;
#8605 = EDGE_LOOP ( 'NONE', ( #57290, #17016, #31214, #81577 ) ) ;
#8606 = LINE ( 'NONE', #63077, #136152 ) ;
#8607 = ORIENTED_EDGE ( 'NONE', *, *, #66440, .F. ) ;
#8608 = ORIENTED_EDGE ( 'NONE', *, *, #53571, .F. ) ;
#8609 = CIRCLE ( 'NONE', #27177, 1.000000000000000888 ) ;
#8610 = EDGE_LOOP ( 'NONE', ( #106091, #21603, #110535 ) ) ;
#8611 = AXIS2_PLACEMENT_3D ( 'NONE', #22693, #100308, #55382 ) ;
#8612 = EDGE_CURVE ( 'NONE', #92353, #8845, #104949, .T. ) ;
#8613 = VECTOR ( 'NONE', #31968, 1000.000000000000000 ) ;
#8614 = CARTESIAN_POINT ( 'NONE',  ( 29.51626352523143737, -4.472830434245838482, 4.472830434245838482 ) ) ;
#8615 = DIRECTION ( 'NONE',  ( 0.3543493200069162685, -0.000000000000000000, -0.9351131265310288487 ) ) ;
#8616 = DIRECTION ( 'NONE',  ( -1.000000000000000000, -0.000000000000000000, -0.000000000000000000 ) ) ;
#8617 = CARTESIAN_POINT ( 'NONE',  ( 124.3962635252314470, 4.472830434245840259, -4.472830434245838482 ) ) ;
#8618 = PLANE ( 'NONE',  #5697 ) ;
#8619 = LINE ( 'NONE', #140600, #4185 ) ;
#8621 = DIRECTION ( 'NONE',  ( 0.5735764363510451602, 0.8191520442889924647, 0.000000000000000000 ) ) ;
#8620 = LINE ( 'NONE', #140601, #87554 ) ;
#8622 = AXIS2_PLACEMENT_3D ( 'NONE', #41792, #84591, #73700 ) ;
#8623 = ADVANCED_FACE ( 'NONE', ( #96196 ), #139024, .T. ) ;
#8624 = CARTESIAN_POINT ( 'NONE',  ( -18.79289321881332597, 18.75929247661552068, 5.000000000000000000 ) ) ;
#8625 = LINE ( 'NONE', #18826, #76061 ) ;
#8626 = CARTESIAN_POINT ( 'NONE',  ( -48.29974487139158867, -27.71228299555239971, 4.000000000000000000 ) ) ;
#8627 = CARTESIAN_POINT ( 'NONE',  ( 34.92499999999998295, 18.85612307739221549, 4.000000000000000000 ) ) ;
#8628 = ORIENTED_EDGE ( 'NONE', *, *, #137477, .T. ) ;
#8629 = EDGE_LOOP ( 'NONE', ( #114537, #102043, #6619, #114165 ) ) ;
#8631 = ORIENTED_EDGE ( 'NONE', *, *, #135943, .F. ) ;
#8630 = EDGE_CURVE ( 'NONE', #79017, #101826, #40440, .T. ) ;
#8632 = ORIENTED_EDGE ( 'NONE', *, *, #28784, .F. ) ;
#8633 = FACE_OUTER_BOUND ( 'NONE', #54306, .T. ) ;
#8634 = ORIENTED_EDGE ( 'NONE', *, *, #72710, .F. ) ;
#8635 = EDGE_LOOP ( 'NONE', ( #101924, #114969, #92999, #103 ) ) ;
#8636 = CARTESIAN_POINT ( 'NONE',  ( -33.48921356237309510, -27.52281430457078670, 5.000000000000000000 ) ) ;
#8637 = PLANE ( 'NONE',  #108015 ) ;
#8638 = DIRECTION ( 'NONE',  ( -0.7071067811865486830, -0.7071067811865464625, 0.000000000000000000 ) ) ;
#8639 = EDGE_CURVE ( 'NONE', #139082, #39184, #60788, .T. ) ;
#8640 = VERTEX_POINT ( 'NONE', #17233 ) ;
#8642 = ADVANCED_FACE ( 'NONE', ( #128159 ), #16496, .F. ) ;
#8641 = VECTOR ( 'NONE', #33138, 999.9999999999998863 ) ;
#8643 = CARTESIAN_POINT ( 'NONE',  ( 22.78501580275796101, -3.740707523384248390, 15.76143240460129569 ) ) ;
#8644 = EDGE_LOOP ( 'NONE', ( #129095, #201 ) ) ;
#8645 =( BOUNDED_CURVE ( )  B_SPLINE_CURVE ( 3, ( #24199, #46721, #135130, #80042 ),
 .UNSPECIFIED., .F., .T. ) 
 B_SPLINE_CURVE_WITH_KNOTS ( ( 4, 4 ),
 ( 3.996889577052295195, 4.025035655492698261 ),
 .UNSPECIFIED. ) 
 CURVE ( )  GEOMETRIC_REPRESENTATION_ITEM ( )  RATIONAL_B_SPLINE_CURVE ( ( 1.000000000000000000, 0.9999339842785831545, 0.9999339842785831545, 1.000000000000000000 ) ) 
 REPRESENTATION_ITEM ( '' )  );
#8646 = FACE_OUTER_BOUND ( 'NONE', #139703, .T. ) ;
#8647 = EDGE_CURVE ( 'NONE', #48148, #55125, #45055, .T. ) ;
#8648 = PLANE ( 'NONE',  #14878 ) ;
#8649 = VECTOR ( 'NONE', #105832, 999.9999999999998863 ) ;
#8650 = CARTESIAN_POINT ( 'NONE',  ( 12.46290314143521982, -3.967499999999994476, 6.871911579029513106 ) ) ;
#8651 = ORIENTED_EDGE ( 'NONE', *, *, #52306, .F. ) ;
#8652 = CARTESIAN_POINT ( 'NONE',  ( 89.16209685856478018, -5.291415217122919401, 3.054999999999998384 ) ) ;
#8653 = PLANE ( 'NONE',  #126907 ) ;
#8654 = DIRECTION ( 'NONE',  ( -0.6830127018922180770, -0.6830127018922204085, -0.2588190451025213501 ) ) ;
#8655 = DIRECTION ( 'NONE',  ( -0.7071067811865486830, -0.7071067811865464625, 0.000000000000000000 ) ) ;
#8656 = EDGE_LOOP ( 'NONE', ( #43170, #108169, #52223, #67919 ) ) ;
#8657 = ORIENTED_EDGE ( 'NONE', *, *, #128077, .T. ) ;
#8658 = CARTESIAN_POINT ( 'NONE',  ( 131.7507865773015681, -49.14999999999999147, -40.57473644908944266 ) ) ;
#8659 = ORIENTED_EDGE ( 'NONE', *, *, #20126, .T. ) ;
#8660 = LINE ( 'NONE', #119583, #138953 ) ;
#8661 = DIRECTION ( 'NONE',  ( -0.7071067811865487940, 0.7071067811865463515, 0.000000000000000000 ) ) ;
#8662 = CARTESIAN_POINT ( 'NONE',  ( -15.48921356237309510, -27.52281430457066236, 5.000000000000000000 ) ) ;
#8663 = CARTESIAN_POINT ( 'NONE',  ( 61.46640106136302961, -43.14999999999999147, -34.92499999999998295 ) ) ;
#8664 = ORIENTED_EDGE ( 'NONE', *, *, #30388, .T. ) ;
#8665 = DIRECTION ( 'NONE',  ( -0.000000000000000000, -0.3543493200069152693, 0.9351131265310292928 ) ) ;
#8666 = FACE_OUTER_BOUND ( 'NONE', #18161, .T. ) ;
#8667 = LINE ( 'NONE', #108707, #505 ) ;
#8668 = ORIENTED_EDGE ( 'NONE', *, *, #100693, .F. ) ;
#8669 = DIRECTION ( 'NONE',  ( -0.000000000000000000, 0.000000000000000000, 1.000000000000000000 ) ) ;
#8670 = DIRECTION ( 'NONE',  ( 0.5735764363510453823, -0.8191520442889923537, 1.003171929053525486E-16 ) ) ;
#8671 = EDGE_LOOP ( 'NONE', ( #42075, #124395, #43182, #127356 ) ) ;
#8673 = VERTEX_POINT ( 'NONE', #60046 ) ;
#8672 = CARTESIAN_POINT ( 'NONE',  ( 0.000000000000000000, 0.000000000000000000, 7.950000000000000178 ) ) ;
#8674 = ORIENTED_EDGE ( 'NONE', *, *, #128477, .T. ) ;
#8675 = LINE ( 'NONE', #52921, #74843 ) ;
#8676 = PLANE ( 'NONE',  #6655 ) ;
#8677 = ORIENTED_EDGE ( 'NONE', *, *, #3903, .T. ) ;
#8678 = DIRECTION ( 'NONE',  ( -0.000000000000000000, -0.3543493200069152693, 0.9351131265310292928 ) ) ;
#8679 = DIRECTION ( 'NONE',  ( -0.7071067811865486830, -0.7071067811865464625, 0.000000000000000000 ) ) ;
#8680 = DIRECTION ( 'NONE',  ( 0.7071067811865486830, -0.7071067811865464625, -0.000000000000000000 ) ) ;
#8681 = AXIS2_PLACEMENT_3D ( 'NONE', #135288, #123696, #134567 ) ;
#8682 = CARTESIAN_POINT ( 'NONE',  ( 44.99451991528749772, 28.92564299267969474, 4.000000000000000000 ) ) ;
#8683 = CARTESIAN_POINT ( 'NONE',  ( 29.87852683662835318, -20.24070752338406720, 7.412974875817723408 ) ) ;
#8684 = DIRECTION ( 'NONE',  ( -0.7071067811865486830, -0.7071067811865464625, 0.000000000000000000 ) ) ;
#8685 = CARTESIAN_POINT ( 'NONE',  ( 27.68840764549667455, 2.499999999999998224, 3.061616997868380183E-16 ) ) ;
#8686 = DIRECTION ( 'NONE',  ( 0.000000000000000000, 0.000000000000000000, 1.000000000000000000 ) ) ;
#8687 = DIRECTION ( 'NONE',  ( 0.000000000000000000, 0.000000000000000000, -1.000000000000000000 ) ) ;
#8688 = LINE ( 'NONE', #120319, #90701 ) ;
#8689 = CARTESIAN_POINT ( 'NONE',  ( -30.18398860626900060, 28.73617430169808173, 5.000000000000000000 ) ) ;
#8690 = LINE ( 'NONE', #30514, #14150 ) ;
#8691 = CARTESIAN_POINT ( 'NONE',  ( 30.48921356237309510, -27.52281430457076894, 5.000000000000000000 ) ) ;
#8692 = VERTEX_POINT ( 'NONE', #39728 ) ;
#8693 = ORIENTED_EDGE ( 'NONE', *, *, #139898, .F. ) ;
#8694 = EDGE_LOOP ( 'NONE', ( #18744, #61084, #111096, #23073, #125773, #60748 ) ) ;
#8695 = CARTESIAN_POINT ( 'NONE',  ( 106.7291666666666430, 7.950000000000001954, -2.130196079827421762 ) ) ;
#8696 = AXIS2_PLACEMENT_3D ( 'NONE', #119124, #105386, #8191 ) ;
#8697 = ORIENTED_EDGE ( 'NONE', *, *, #21759, .T. ) ;
#8698 = ORIENTED_EDGE ( 'NONE', *, *, #48886, .F. ) ;
#8699 = EDGE_CURVE ( 'NONE', #33874, #94223, #104211, .T. ) ;
#8700 = EDGE_LOOP ( 'NONE', ( #48876, #104785, #30455, #86391 ) ) ;
#8701 = CARTESIAN_POINT ( 'NONE',  ( 10.49999999999992184, 19.39370406404967895, 1.459788787078177830 ) ) ;
#8702 = LINE ( 'NONE', #51571, #43966 ) ;
#8703 = ORIENTED_EDGE ( 'NONE', *, *, #86153, .F. ) ;
#8704 = VECTOR ( 'NONE', #24384, 1000.000000000000000 ) ;
#8705 = DIRECTION ( 'NONE',  ( 0.000000000000000000, 1.000000000000000000, -0.000000000000000000 ) ) ;
#8706 = LINE ( 'NONE', #116084, #76617 ) ;
#8707 = AXIS2_PLACEMENT_3D ( 'NONE', #115576, #103999, #94568 ) ;
#8708 = DIRECTION ( 'NONE',  ( -0.7071067811865486830, -0.7071067811865464625, -0.000000000000000000 ) ) ;
#8709 = DIRECTION ( 'NONE',  ( 0.7071067811865486830, -0.7071067811865464625, -0.000000000000000000 ) ) ;
#8710 = CARTESIAN_POINT ( 'NONE',  ( 106.0212635252314470, -4.472830434245839371, -4.472830434245840259 ) ) ;
#8711 = EDGE_CURVE ( 'NONE', #142010, #33645, #1443, .T. ) ;
#8712 = ORIENTED_EDGE ( 'NONE', *, *, #1520, .F. ) ;
#8713 = DIRECTION ( 'NONE',  ( 0.000000000000000000, -1.000000000000000000, 0.000000000000000000 ) ) ;
#8714 = EDGE_CURVE ( 'NONE', #8442, #11462, #85327, .T. ) ;
#8715 = DIRECTION ( 'NONE',  ( 0.000000000000000000, 0.000000000000000000, 1.000000000000000000 ) ) ;
#8717 = DIRECTION ( 'NONE',  ( -0.000000000000000000, 0.3543493200069153248, 0.9351131265310292928 ) ) ;
#8716 = VECTOR ( 'NONE', #140671, 999.9999999999998863 ) ;
#8718 = CARTESIAN_POINT ( 'NONE',  ( -45.48921356237309510, -27.52281430457087197, 5.000000000000000000 ) ) ;
#8719 = CARTESIAN_POINT ( 'NONE',  ( 63.29974487139158867, -27.71228299555250274, 4.000000000000000000 ) ) ;
#8720 = CARTESIAN_POINT ( 'NONE',  ( 33.03752705046289151, -9.735942053221456900E-16, 7.949999999999998401 ) ) ;
#8721 = CARTESIAN_POINT ( 'NONE',  ( -1.251544128675743828, -11.24070752338416845, 10.39518518046009632 ) ) ;
#8722 = ORIENTED_EDGE ( 'NONE', *, *, #112900, .T. ) ;
#8723 = VERTEX_POINT ( 'NONE', #29518 ) ;
#8724 = CARTESIAN_POINT ( 'NONE',  ( 27.10416666666666785, 2.130196079827422206, 7.950000000000001954 ) ) ;
#8725 = VERTEX_POINT ( 'NONE', #6298 ) ;
#8726 = EDGE_CURVE ( 'NONE', #75249, #6819, #49175, .T. ) ;
#8727 = DIRECTION ( 'NONE',  ( -0.3543493200069163240, -0.000000000000000000, -0.9351131265310288487 ) ) ;
#8728 = DIRECTION ( 'NONE',  ( 0.6830127018922181881, 0.6830127018922202975, -0.2588190451025214056 ) ) ;
#8729 = CARTESIAN_POINT ( 'NONE',  ( -34.92500000000001137, 22.22500000000000142, 4.000000000000000000 ) ) ;
#8730 = CARTESIAN_POINT ( 'NONE',  ( -15.92034494338828665, -22.22500000000000142, 12.20157423226259397 ) ) ;
#8731 = EDGE_CURVE ( 'NONE', #87168, #32802, #38283, .T. ) ;
#8732 = LINE ( 'NONE', #141448, #30435 ) ;
#8733 = DIRECTION ( 'NONE',  ( 0.7071067811865487940, 0.7071067811865463515, 0.000000000000000000 ) ) ;
#8734 = CARTESIAN_POINT ( 'NONE',  ( 120.9537635252314658, -6.109999999999998543, -3.741295971395162543E-16 ) ) ;
#8735 = ORIENTED_EDGE ( 'NONE', *, *, #63175, .T. ) ;
#8736 = DIRECTION ( 'NONE',  ( -0.6830127018922181881, 0.6830127018922202975, -0.2588190451025214056 ) ) ;
#8737 = ORIENTED_EDGE ( 'NONE', *, *, #93219, .F. ) ;
#8738 = LINE ( 'NONE', #109536, #36935 ) ;
#8739 = EDGE_CURVE ( 'NONE', #91902, #120409, #82500, .T. ) ;
#8740 = EDGE_CURVE ( 'NONE', #132281, #19758, #105642, .T. ) ;
#8741 = LINE ( 'NONE', #17520, #4651 ) ;
#8742 = PLANE ( 'NONE',  #88164 ) ;
#8743 = ORIENTED_EDGE ( 'NONE', *, *, #119718, .F. ) ;
#8744 = CARTESIAN_POINT ( 'NONE',  ( 44.77126352523143282, 4.472830434245839371, 4.472830434245842035 ) ) ;
#8745 = ORIENTED_EDGE ( 'NONE', *, *, #127501, .F. ) ;
#8746 = PLANE ( 'NONE',  #28524 ) ;
#8747 = LINE ( 'NONE', #74070, #32293 ) ;
#8748 = CARTESIAN_POINT ( 'NONE',  ( 15.79289321881334907, -20.24070752338407431, 5.000000000000000000 ) ) ;
#8749 = AXIS2_PLACEMENT_3D ( 'NONE', #81267, #103672, #127610 ) ;
#8750 = DIRECTION ( 'NONE',  ( -0.000000000000000000, -0.3543493200069153248, -0.9351131265310291818 ) ) ;
#8751 = CARTESIAN_POINT ( 'NONE',  ( 40.59959685856476597, -6.109999999999997655, -1.637169565754160283 ) ) ;
#8752 = VERTEX_POINT ( 'NONE', #49889 ) ;
#8753 = ADVANCED_FACE ( 'NONE', ( #129550 ), #94068, .F. ) ;
#8754 = DIRECTION ( 'NONE',  ( 0.7071067811865487940, 0.7071067811865463515, 0.000000000000000000 ) ) ;
#8755 = ORIENTED_EDGE ( 'NONE', *, *, #9622, .F. ) ;
#8756 = EDGE_LOOP ( 'NONE', ( #6229, #133803, #45795 ) ) ;
#8757 = VERTEX_POINT ( 'NONE', #94772 ) ;
#8759 = ADVANCED_FACE ( 'NONE', ( #78059 ), #107789, .F. ) ;
#8758 = AXIS2_PLACEMENT_3D ( 'NONE', #56911, #4564, #35876 ) ;
#8760 = EDGE_CURVE ( 'NONE', #76190, #106463, #33455, .T. ) ;
#8761 = CARTESIAN_POINT ( 'NONE',  ( -5.816011393731002066, 28.73617430169783304, 5.000000000000000000 ) ) ;
#8762 = EDGE_LOOP ( 'NONE', ( #128751, #38826, #102910, #1522 ) ) ;
#8763 = DIRECTION ( 'NONE',  ( 0.7071067811865486830, -0.7071067811865464625, -0.000000000000000000 ) ) ;
#8764 = CARTESIAN_POINT ( 'NONE',  ( 12.00548008471251293, 28.92564299267929684, 4.000000000000000000 ) ) ;
#8765 = ADVANCED_FACE ( 'NONE', ( #52703 ), #141897, .F. ) ;
#8766 = CARTESIAN_POINT ( 'NONE',  ( -25.82816939922334853, -11.24070752338417201, 4.000000000000000000 ) ) ;
#8767 = FACE_BOUND ( 'NONE', #128720, .T. ) ;
#8768 = EDGE_CURVE ( 'NONE', #34652, #28496, #42591, .T. ) ;
#8769 = ORIENTED_EDGE ( 'NONE', *, *, #134186, .F. ) ;
#8770 = CARTESIAN_POINT ( 'NONE',  ( 20.99451991528748707, 28.92564299267952777, 4.000000000000000000 ) ) ;
#8771 = PLANE ( 'NONE',  #81521 ) ;
#8772 = FACE_OUTER_BOUND ( 'NONE', #133917, .T. ) ;
#8773 = ADVANCED_FACE ( 'NONE', ( #19375 ), #74469, .T. ) ;
#8774 = ORIENTED_EDGE ( 'NONE', *, *, #13487, .F. ) ;
#8775 = LINE ( 'NONE', #107428, #89785 ) ;
#8776 = VERTEX_POINT ( 'NONE', #27581 ) ;
#8777 = EDGE_LOOP ( 'NONE', ( #48900, #58557, #87689, #133171 ) ) ;
#8778 = DIRECTION ( 'NONE',  ( -0.6830127018922181881, 0.6830127018922202975, -0.2588190451025214056 ) ) ;
#8779 = ORIENTED_EDGE ( 'NONE', *, *, #33104, .F. ) ;
#8780 = CARTESIAN_POINT ( 'NONE',  ( 56.49543019189812298, 5.291415217122916737, 3.055000000000001936 ) ) ;
#8781 = EDGE_LOOP ( 'NONE', ( #50927, #29912, #86541, #77466 ) ) ;
#8782 = AXIS2_PLACEMENT_3D ( 'NONE', #116187, #93726, #126344 ) ;
#8783 = ADVANCED_FACE ( 'NONE', ( #105154 ), #17425, .F. ) ;
#8784 = CARTESIAN_POINT ( 'NONE',  ( 18.48921356237309510, -27.52281430457068367, 5.000000000000000000 ) ) ;
#8785 = LINE ( 'NONE', #23261, #105169 ) ;
#8786 = ORIENTED_EDGE ( 'NONE', *, *, #44381, .T. ) ;
#8787 = CARTESIAN_POINT ( 'NONE',  ( 39.18398860626899705, 28.73617430169814568, 5.000000000000000000 ) ) ;
#8788 = CARTESIAN_POINT ( 'NONE',  ( 2.700255128608413990, -27.71228299555204089, 4.000000000000000000 ) ) ;
#8789 = EDGE_CURVE ( 'NONE', #136335, #23129, #26182, .T. ) ;
#8790 = DIRECTION ( 'NONE',  ( 0.9843059135694992579, 0.000000000000000000, -0.1764705882353009014 ) ) ;
#8791 = SURFACE_SIDE_STYLE ('',( #63277 ) ) ;
#8792 = FACE_OUTER_BOUND ( 'NONE', #115300, .T. ) ;
#8793 = DIRECTION ( 'NONE',  ( 0.000000000000000000, 0.000000000000000000, 1.000000000000000000 ) ) ;
#8794 = CARTESIAN_POINT ( 'NONE',  ( 13.49999999999990763, 10.94296225409028089, -9.576120664313226172 ) ) ;
#8795 = VERTEX_POINT ( 'NONE', #126202 ) ;
#8796 = VERTEX_POINT ( 'NONE', #103022 ) ;
#8797 = CARTESIAN_POINT ( 'NONE',  ( -7.954842266633281866, -21.74070752338405299, 21.72585301388582479 ) ) ;
#8799 = LINE ( 'NONE', #74124, #88338 ) ;
#8798 = AXIS2_PLACEMENT_3D ( 'NONE', #46377, #56551, #111584 ) ;
#8800 = ORIENTED_EDGE ( 'NONE', *, *, #19312, .T. ) ;
#8801 = VERTEX_POINT ( 'NONE', #71846 ) ;
#8803 = ORIENTED_EDGE ( 'NONE', *, *, #106297, .T. ) ;
#8802 = VECTOR ( 'NONE', #130262, 1000.000000000000227 ) ;
#8804 = CARTESIAN_POINT ( 'NONE',  ( -34.92500000000001137, 22.22500000000000142, 4.500000000000000888 ) ) ;
#8805 = CARTESIAN_POINT ( 'NONE',  ( 11.70025512860841133, -27.71228299555198049, 4.000000000000000000 ) ) ;
#8806 = ORIENTED_EDGE ( 'NONE', *, *, #17645, .F. ) ;
#8807 = LINE ( 'NONE', #41488, #37064 ) ;
#8808 = VECTOR ( 'NONE', #126000, 999.9999999999998863 ) ;
#8809 = VECTOR ( 'NONE', #89780, 1000.000000000000000 ) ;
#8810 = EDGE_CURVE ( 'NONE', #129287, #72440, #50082, .T. ) ;
#8811 = LINE ( 'NONE', #42950, #137053 ) ;
#8812 = EDGE_CURVE ( 'NONE', #80652, #31146, #92844, .T. ) ;
#8813 = CARTESIAN_POINT ( 'NONE',  ( 15.52540314143522160, 2.126176841940962348, 7.934999999999989839 ) ) ;
#8814 = DIRECTION ( 'NONE',  ( -0.6830127018922180770, -0.6830127018922204085, -0.2588190451025213501 ) ) ;
#8815 = ORIENTED_EDGE ( 'NONE', *, *, #29172, .F. ) ;
#8816 = CARTESIAN_POINT ( 'NONE',  ( 122.5579301918981088, 6.110000000000001208, -1.637169565754156286 ) ) ;
#8817 = FACE_OUTER_BOUND ( 'NONE', #42027, .T. ) ;
#8818 = DIRECTION ( 'NONE',  ( 1.000000000000000000, 0.000000000000000000, 0.000000000000000000 ) ) ;
#8819 = VERTEX_POINT ( 'NONE', #103697 ) ;
#8820 = AXIS2_PLACEMENT_3D ( 'NONE', #31378, #20471, #98750 ) ;
#8821 = CARTESIAN_POINT ( 'NONE',  ( -26.24139925780185578, 21.72500000000000142, 5.000000000000000000 ) ) ;
#8822 = VERTEX_POINT ( 'NONE', #69708 ) ;
#8823 = CARTESIAN_POINT ( 'NONE',  ( 75.18336038379622721, -2.130196079827426203, 7.949999999999996625 ) ) ;
#8824 = DIRECTION ( 'NONE',  ( -0.7071067811865486830, -0.7071067811865464625, 0.000000000000000000 ) ) ;
#8825 = DIRECTION ( 'NONE',  ( -0.6830127018922181881, 0.6830127018922202975, -0.2588190451025214056 ) ) ;
#8826 = EDGE_LOOP ( 'NONE', ( #119878, #29970, #138476, #57453 ) ) ;
#8827 = DIRECTION ( 'NONE',  ( 1.734723475976806848E-16, -1.000000000000000000, 0.000000000000000000 ) ) ;
#8828 = DIRECTION ( 'NONE',  ( -0.3543493200069163240, 4.681814790819596721E-17, -0.9351131265310288487 ) ) ;
#8829 = ORIENTED_EDGE ( 'NONE', *, *, #61521, .F. ) ;
#8830 = VECTOR ( 'NONE', #104294, 999.9999999999998863 ) ;
#8831 = DIRECTION ( 'NONE',  ( -0.7071067811865487940, 0.7071067811865463515, 0.000000000000000000 ) ) ;
#8833 = STYLED_ITEM ( 'NONE', ( #98753 ), #57613 ) ;
#8832 = DIRECTION ( 'NONE',  ( -1.000000000000000000, -0.000000000000000000, -0.000000000000000000 ) ) ;
#8834 = VERTEX_POINT ( 'NONE', #5090 ) ;
#8835 = VECTOR ( 'NONE', #86957, 999.9999999999998863 ) ;
#8836 = CARTESIAN_POINT ( 'NONE',  ( 3.500000000000000444, 0.000000000000000000, 6.094999999999989981 ) ) ;
#8837 = FACE_OUTER_BOUND ( 'NONE', #52166, .T. ) ;
#8838 = ORIENTED_EDGE ( 'NONE', *, *, #133355, .F. ) ;
#8839 = ORIENTED_EDGE ( 'NONE', *, *, #94197, .F. ) ;
#8840 = DIRECTION ( 'NONE',  ( -0.7071067811865486830, 0.7071067811865464625, 0.000000000000000000 ) ) ;
#8841 = LINE ( 'NONE', #132134, #82991 ) ;
#8842 = CARTESIAN_POINT ( 'NONE',  ( 14.56206980810188334, -7.934999999999991616, -2.126176841940955242 ) ) ;
#8843 = LINE ( 'NONE', #11732, #87820 ) ;
#8844 = DIRECTION ( 'NONE',  ( 0.7071067811865487940, 0.7071067811865463515, 0.000000000000000000 ) ) ;
#8845 = VERTEX_POINT ( 'NONE', #136353 ) ;
#8846 = DIRECTION ( 'NONE',  ( 0.000000000000000000, 1.000000000000000000, 0.000000000000000000 ) ) ;
#8847 = DIRECTION ( 'NONE',  ( 0.7071067811865486830, -0.7071067811865464625, -0.000000000000000000 ) ) ;
#8848 = CARTESIAN_POINT ( 'NONE',  ( 8.999999999999937828, -18.41253812416056590, 4.000000000000000000 ) ) ;
#8849 = VECTOR ( 'NONE', #19546, 1000.000000000000227 ) ;
#8850 = DIRECTION ( 'NONE',  ( 0.6830127018922180770, -0.6830127018922204085, -0.2588190451025213501 ) ) ;
#8851 = CARTESIAN_POINT ( 'NONE',  ( 37.09959685856476597, -6.109999999999998543, -1.637169565754160727 ) ) ;
#8852 = VECTOR ( 'NONE', #97313, 1000.000000000000000 ) ;
#8853 = VERTEX_POINT ( 'NONE', #49390 ) ;
#8854 = LINE ( 'NONE', #28553, #55704 ) ;
#8855 = ORIENTED_EDGE ( 'NONE', *, *, #42669, .T. ) ;
#8856 = ORIENTED_EDGE ( 'NONE', *, *, #116781, .T. ) ;
#8857 = CARTESIAN_POINT ( 'NONE',  ( 13.49999999999990585, 15.05218569542901186, 5.000000000000000000 ) ) ;
#8858 = CARTESIAN_POINT ( 'NONE',  ( 0.000000000000000000, 0.000000000000000000, 5.000000000000000000 ) ) ;
#8859 = ORIENTED_EDGE ( 'NONE', *, *, #139058, .F. ) ;
#8860 = CARTESIAN_POINT ( 'NONE',  ( 7.499999999999951150, -4.216083040037250207, -7.486842126848674894 ) ) ;
#8861 = EDGE_CURVE ( 'NONE', #34748, #31094, #58861, .T. ) ;
#8862 = LINE ( 'NONE', #63355, #85677 ) ;
#8863 = LINE ( 'NONE', #62616, #27972 ) ;
#8864 = DIRECTION ( 'NONE',  ( -0.7071067811865487940, 0.7071067811865463515, -0.000000000000000000 ) ) ;
#8865 = EDGE_CURVE ( 'NONE', #20167, #64959, #126884, .T. ) ;
#8866 = ADVANCED_FACE ( 'NONE', ( #6502 ), #114589, .T. ) ;
#8867 = ORIENTED_EDGE ( 'NONE', *, *, #126387, .F. ) ;
#8868 = DIRECTION ( 'NONE',  ( -0.000000000000000000, 0.3543493200069153248, 0.9351131265310292928 ) ) ;
#8869 = CARTESIAN_POINT ( 'NONE',  ( 14.99999999999989519, -8.151047557385055597, -8.977947279169832484 ) ) ;
#8870 = CARTESIAN_POINT ( 'NONE',  ( 79.74999999999998579, -9.735942053221458872E-16, 7.950000000000000178 ) ) ;
#8871 = LINE ( 'NONE', #132169, #133561 ) ;
#8872 = DIRECTION ( 'NONE',  ( -0.7071067811865486830, -0.7071067811865464625, 0.000000000000000000 ) ) ;
#8873 = SURFACE_STYLE_FILL_AREA ( #50495 ) ;
#8874 = LINE ( 'NONE', #143027, #80592 ) ;
#8875 = EDGE_CURVE ( 'NONE', #83448, #74127, #130203, .T. ) ;
#8877 = ADVANCED_FACE ( 'NONE', ( #39939 ), #104429, .F. ) ;
#8876 = CARTESIAN_POINT ( 'NONE',  ( 56.22502705046289151, 5.819803920172573086, -5.819803920172572198 ) ) ;
#8878 = CARTESIAN_POINT ( 'NONE',  ( 14.99451991528749595, 28.92564299267948513, 4.000000000000000000 ) ) ;
#8879 = ORIENTED_EDGE ( 'NONE', *, *, #87587, .T. ) ;
#8880 = EDGE_LOOP ( 'NONE', ( #135748, #8150, #90347, #90355 ) ) ;
#8881 = CARTESIAN_POINT ( 'NONE',  ( 53.49999999999999289, 0.000000000000000000, -7.950000000000000178 ) ) ;
#8882 = DIRECTION ( 'NONE',  ( -1.000000000000000000, -1.224606353822377258E-16, -0.000000000000000000 ) ) ;
#8883 = EDGE_CURVE ( 'NONE', #41257, #33380, #116744, .T. ) ;
#8884 = LINE ( 'NONE', #64054, #76391 ) ;
#8885 = FACE_OUTER_BOUND ( 'NONE', #36025, .T. ) ;
#8886 = ORIENTED_EDGE ( 'NONE', *, *, #88573, .F. ) ;
#8887 = LINE ( 'NONE', #43725, #81622 ) ;
#8888 = EDGE_CURVE ( 'NONE', #99466, #40629, #137807, .T. ) ;
#8889 = VECTOR ( 'NONE', #105171, 1000.000000000000000 ) ;
#8890 = CARTESIAN_POINT ( 'NONE',  ( 47.25043019189810423, 3.055000000000002824, -5.291415217122919401 ) ) ;
#8891 = ORIENTED_EDGE ( 'NONE', *, *, #49728, .F. ) ;
#8892 = CARTESIAN_POINT ( 'NONE',  ( 48.48921356237309510, -27.52281430457089328, 5.000000000000000000 ) ) ;
#8893 = ORIENTED_EDGE ( 'NONE', *, *, #56610, .T. ) ;
#8894 = EDGE_LOOP ( 'NONE', ( #94877, #4419, #8203, #105936 ) ) ;
#8895 = LINE ( 'NONE', #141633, #26372 ) ;
#8897 = EDGE_CURVE ( 'NONE', #24205, #38741, #28775, .T. ) ;
#8896 = AXIS2_PLACEMENT_3D ( 'NONE', #129697, #86222, #96329 ) ;
#8898 = VECTOR ( 'NONE', #86099, 1000.000000000000000 ) ;
#8899 = AXIS2_PLACEMENT_3D ( 'NONE', #109558, #142903, #74827 ) ;
#8900 = CARTESIAN_POINT ( 'NONE',  ( 24.48921356237309510, -27.52281430457072631, 5.000000000000000000 ) ) ;
#8901 = DIRECTION ( 'NONE',  ( -1.000000000000000000, -0.000000000000000000, -0.000000000000000000 ) ) ;
#8902 = CONICAL_SURFACE ( 'NONE', #110760, 2.055000000000001048, 0.9599310885968758145 ) ;
#8903 = DIRECTION ( 'NONE',  ( -0.7071067811865487940, 0.7071067811865463515, -0.000000000000000000 ) ) ;
#8904 = ORIENTED_EDGE ( 'NONE', *, *, #31105, .F. ) ;
#8905 = CARTESIAN_POINT ( 'NONE',  ( 20.67906569311139009, 4.202752102959690472E-16, 0.000000000000000000 ) ) ;
#8907 = ORIENTED_EDGE ( 'NONE', *, *, #102156, .F. ) ;
#8906 = CARTESIAN_POINT ( 'NONE',  ( 9.524972949537108491, -4.461849672132299993, -4.461849672132299105 ) ) ;
#8908 = CARTESIAN_POINT ( 'NONE',  ( 79.62543019189810423, 5.291415217122919401, 3.055000000000002824 ) ) ;
#8909 = DIRECTION ( 'NONE',  ( 0.7071067811865486830, -0.7071067811865464625, -0.000000000000000000 ) ) ;
#8910 = LINE ( 'NONE', #108975, #52335 ) ;
#8911 = FILL_AREA_STYLE_COLOUR ( '', #67955 ) ;
#8912 = EDGE_CURVE ( 'NONE', #9095, #112404, #115271, .T. ) ;
#8913 = VECTOR ( 'NONE', #13814, 1000.000000000000000 ) ;
#8914 = VECTOR ( 'NONE', #9591, 1000.000000000000000 ) ;
#8915 = ORIENTED_EDGE ( 'NONE', *, *, #39966, .T. ) ;
#8916 = CARTESIAN_POINT ( 'NONE',  ( 64.66209685856478018, -5.291415217122919401, 3.054999999999997939 ) ) ;
#8917 = CARTESIAN_POINT ( 'NONE',  ( 30.48921356237309510, -27.52281430457076894, 5.000000000000000000 ) ) ;
#8918 = ADVANCED_FACE ( 'NONE', ( #15961 ), #82704, .T. ) ;
#8919 = CARTESIAN_POINT ( 'NONE',  ( 12.71159235450332048, 2.500000000000001332, 0.000000000000000000 ) ) ;
#8920 = CARTESIAN_POINT ( 'NONE',  ( 21.18398860626899349, 28.73617430169802134, 5.000000000000000000 ) ) ;
#8921 = ORIENTED_EDGE ( 'NONE', *, *, #93878, .F. ) ;
#8922 = EDGE_LOOP ( 'NONE', ( #15671, #67477, #128647, #42909 ) ) ;
#8923 = AXIS2_PLACEMENT_3D ( 'NONE', #6535, #69748, #3692 ) ;
#8924 = CARTESIAN_POINT ( 'NONE',  ( 42.18398860626899705, 28.73617430169816700, 5.000000000000000000 ) ) ;
#8925 = CARTESIAN_POINT ( 'NONE',  ( 0.000000000000000000, 0.000000000000000000, 0.000000000000000000 ) ) ;
#8926 = ORIENTED_EDGE ( 'NONE', *, *, #26089, .T. ) ;
#8927 = ADVANCED_FACE ( 'NONE', ( #98557 ), #18105, .F. ) ;
#8928 = ORIENTED_EDGE ( 'NONE', *, *, #114405, .T. ) ;
#8929 = CIRCLE ( 'NONE', #41372, 2.500000000000000444 ) ;
#8930 = DIRECTION ( 'NONE',  ( -0.7071067811865486830, -0.7071067811865464625, -0.000000000000000000 ) ) ;
#8932 = EDGE_CURVE ( 'NONE', #30215, #14718, #20267, .T. ) ;
#8931 = VERTEX_POINT ( 'NONE', #119571 ) ;
#8933 = CARTESIAN_POINT ( 'NONE',  ( -18.79289321881332242, 15.75929247661555976, 5.000000000000000000 ) ) ;
#8934 = LINE ( 'NONE', #128640, #133590 ) ;
#8935 = VECTOR ( 'NONE', #52249, 1000.000000000000000 ) ;
#8936 = VECTOR ( 'NONE', #102760, 1000.000000000000000 ) ;
#8938 = EDGE_CURVE ( 'NONE', #4192, #28467, #21801, .T. ) ;
#8937 = AXIS2_PLACEMENT_3D ( 'NONE', #139817, #17283, #61546 ) ;
#8940 = AXIS2_PLACEMENT_3D ( 'NONE', #49775, #126566, #16363 ) ;
#8939 = DIRECTION ( 'NONE',  ( 0.7071067811865487940, 0.7071067811865463515, -0.000000000000000000 ) ) ;
#8941 = FACE_BOUND ( 'NONE', #18511, .T. ) ;
#8942 = CARTESIAN_POINT ( 'NONE',  ( -34.92500000000001137, 13.70193056682087196, 4.500000000000000888 ) ) ;
#8943 = CARTESIAN_POINT ( 'NONE',  ( 40.18336038379621300, -2.130196079827426203, 7.949999999999996625 ) ) ;
#8944 = DIRECTION ( 'NONE',  ( -0.000000000000000000, 0.3543493200069153248, 0.9351131265310292928 ) ) ;
#8946 = ORIENTED_EDGE ( 'NONE', *, *, #23148, .T. ) ;
#8945 = CARTESIAN_POINT ( 'NONE',  ( 28.49999999999981171, 1.030536316426539756, -5.498701923753864129 ) ) ;
#8947 = VECTOR ( 'NONE', #63860, 1000.000000000000000 ) ;
#8948 = CIRCLE ( 'NONE', #43784, 5.968999999999998529 ) ;
#8949 = FILL_AREA_STYLE ('',( #17712 ) ) ;
#8950 = CONTEXT_DEPENDENT_SHAPE_REPRESENTATION ( #109636, #75987 ) ;
#8951 = ORIENTED_EDGE ( 'NONE', *, *, #104545, .F. ) ;
#8952 = EDGE_LOOP ( 'NONE', ( #110995, #37352, #86233, #4895 ) ) ;
#8953 = CARTESIAN_POINT ( 'NONE',  ( 85.22459685856479439, -1.637169565754160949, 6.109999999999997655 ) ) ;
#8954 = ORIENTED_EDGE ( 'NONE', *, *, #31238, .F. ) ;
#8955 = ADVANCED_FACE ( 'NONE', ( #53645 ), #8648, .F. ) ;
#8956 = CARTESIAN_POINT ( 'NONE',  ( 11.99999999999991473, -16.60178936734447319, 0.8616154019347775916 ) ) ;
#8957 = VERTEX_POINT ( 'NONE', #85520 ) ;
#8958 = PLANE ( 'NONE',  #7320 ) ;
#8959 = AXIS2_PLACEMENT_3D ( 'NONE', #125705, #72788, #6002 ) ;
#8960 = EDGE_CURVE ( 'NONE', #30662, #19069, #75397, .T. ) ;
#8961 = LINE ( 'NONE', #98866, #86522 ) ;
#8962 = CARTESIAN_POINT ( 'NONE',  ( 30.18398860626900060, 28.73617430169808173, 5.000000000000000000 ) ) ;
#8963 = LINE ( 'NONE', #41643, #50154 ) ;
#8964 = CARTESIAN_POINT ( 'NONE',  ( 30.48921356237309510, -27.52281430457076894, 5.000000000000000000 ) ) ;
#8965 = CARTESIAN_POINT ( 'NONE',  ( -5.816011393731002066, 28.73617430169783304, 5.000000000000000000 ) ) ;
#8966 = LINE ( 'NONE', #120615, #639 ) ;
#8967 = CARTESIAN_POINT ( 'NONE',  ( -45.48921356237309510, -27.52281430457087197, 5.000000000000000000 ) ) ;
#8968 = ORIENTED_EDGE ( 'NONE', *, *, #89026, .T. ) ;
#8969 = DIRECTION ( 'NONE',  ( 0.000000000000000000, -1.000000000000000000, 0.000000000000000000 ) ) ;
#8970 = ORIENTED_EDGE ( 'NONE', *, *, #8080, .F. ) ;
#8971 = CARTESIAN_POINT ( 'NONE',  ( -7.499999999999951150, -1.592773361805382981, -6.492772025301212224 ) ) ;
#8972 = CARTESIAN_POINT ( 'NONE',  ( -19.69064382391260892, -2.759520746520534473, 4.000000000000000000 ) ) ;
#8973 = EDGE_LOOP ( 'NONE', ( #76087, #18538, #115063, #20846 ) ) ;
#8974 = EDGE_CURVE ( 'NONE', #117002, #55674, #100586, .T. ) ;
#8975 = ORIENTED_EDGE ( 'NONE', *, *, #54200, .T. ) ;
#8976 = DIRECTION ( 'NONE',  ( -0.6830127018922181881, 0.6830127018922202975, -0.2588190451025214056 ) ) ;
#8977 = VERTEX_POINT ( 'NONE', #131195 ) ;
#8978 = EDGE_CURVE ( 'NONE', #80320, #113825, #95702, .T. ) ;
#8979 = CARTESIAN_POINT ( 'NONE',  ( 35.14626352523143993, -4.472830434245840259, 4.472830434245838482 ) ) ;
#8980 = ORIENTED_EDGE ( 'NONE', *, *, #39841, .F. ) ;
#8981 = CARTESIAN_POINT ( 'NONE',  ( 0.2997448713915885632, -27.71228299555206220, 4.000000000000000000 ) ) ;
#8982 = EDGE_CURVE ( 'NONE', #7797, #54723, #130502, .T. ) ;
#8983 = CARTESIAN_POINT ( 'NONE',  ( 28.33747294953710849, 6.094999999999989981, -1.119633336120465690E-15 ) ) ;
#8984 = CARTESIAN_POINT ( 'NONE',  ( 0.4527155423044956772, 12.59110042198609136, -25.26827755431022027 ) ) ;
#8985 = ORIENTED_EDGE ( 'NONE', *, *, #44533, .F. ) ;
#8986 = FACE_OUTER_BOUND ( 'NONE', #34806, .T. ) ;
#8987 = ORIENTED_EDGE ( 'NONE', *, *, #109740, .F. ) ;
#8988 = LINE ( 'NONE', #141718, #48817 ) ;
#8989 = PLANE ( 'NONE',  #1193 ) ;
#8991 = ORIENTED_EDGE ( 'NONE', *, *, #19128, .F. ) ;
#8990 = LINE ( 'NONE', #140973, #77203 ) ;
#8992 = ORIENTED_EDGE ( 'NONE', *, *, #73139, .T. ) ;
#8993 = CARTESIAN_POINT ( 'NONE',  ( 25.82816939922335209, -2.240707523384257716, 4.000000000000000000 ) ) ;
#8994 = CARTESIAN_POINT ( 'NONE',  ( 33.41161490594808470, 22.22500000000000497, 4.777194822843814137 ) ) ;
#8995 = VERTEX_POINT ( 'NONE', #65253 ) ;
#8996 = EDGE_CURVE ( 'NONE', #63176, #30783, #118881, .T. ) ;
#8997 = CARTESIAN_POINT ( 'NONE',  ( 109.4541937171295558, 6.884901960086283523, 3.975000000000002753 ) ) ;
#8998 = ORIENTED_EDGE ( 'NONE', *, *, #117477, .T. ) ;
#8999 = ORIENTED_EDGE ( 'NONE', *, *, #17802, .T. ) ;
#9000 = EDGE_LOOP ( 'NONE', ( #53952, #81698, #2936, #52833 ) ) ;
#9001 = CARTESIAN_POINT ( 'NONE',  ( 20.20519093902540320, 4.584330080086930965E-16, 0.000000000000000000 ) ) ;
#9002 = VECTOR ( 'NONE', #108797, 1000.000000000000000 ) ;
#9003 = VECTOR ( 'NONE', #143103, 999.9999999999998863 ) ;
#9004 = VECTOR ( 'NONE', #1486, 999.9999999999998863 ) ;
#9005 = VECTOR ( 'NONE', #82279, 999.9999999999998863 ) ;
#9006 = DIRECTION ( 'NONE',  ( -0.7071067811865486830, 0.7071067811865464625, 0.000000000000000000 ) ) ;
#9007 =( LENGTH_UNIT ( ) NAMED_UNIT ( * ) SI_UNIT ( .MILLI., .METRE. ) );
#9008 = FACE_OUTER_BOUND ( 'NONE', #44273, .T. ) ;
#9009 = STYLED_ITEM ( 'NONE', ( #13081 ), #113213 ) ;
#9010 = DIRECTION ( 'NONE',  ( -0.000000000000000000, 0.000000000000000000, 1.000000000000000000 ) ) ;
#9011 = DIRECTION ( 'NONE',  ( -1.000000000000000000, -1.224606353822377258E-16, -0.000000000000000000 ) ) ;
#9012 = EDGE_CURVE ( 'NONE', #98151, #57105, #29029, .T. ) ;
#9013 = ORIENTED_EDGE ( 'NONE', *, *, #123635, .F. ) ;
#9014 = FACE_OUTER_BOUND ( 'NONE', #102365, .T. ) ;
#9015 = ORIENTED_EDGE ( 'NONE', *, *, #87301, .F. ) ;
#9016 = VECTOR ( 'NONE', #47308, 1000.000000000000000 ) ;
#9017 = LINE ( 'NONE', #131575, #10030 ) ;
#9018 = CARTESIAN_POINT ( 'NONE',  ( -7.294715974614694787, 22.22500000000000142, -5.470147491473989376 ) ) ;
#9019 = EDGE_LOOP ( 'NONE', ( #70328, #10169, #89993, #64466 ) ) ;
#9020 = PLANE ( 'NONE',  #136339 ) ;
#9021 =( BOUNDED_CURVE ( )  B_SPLINE_CURVE ( 2, ( #64394, #28917, #86156, #73156, #117321, #40519, #106425, #130382, #9248, #51393, #95587, #97734, #139847 ),
 .UNSPECIFIED., .F., .T. ) 
 B_SPLINE_CURVE_WITH_KNOTS ( ( 3, 2, 2, 2, 2, 2, 3 ),
 ( 0.3499999999999999778, 0.3527777777777778012, 0.3555555555555555691, 0.3583333333333333370, 0.3611111111111111049, 0.3638888888888888729, 0.3666666666666666408 ),
 .UNSPECIFIED. ) 
 CURVE ( )  GEOMETRIC_REPRESENTATION_ITEM ( )  RATIONAL_B_SPLINE_CURVE ( ( 1.000000000000000000, 0.9659258262890683122, 1.000000000000000000, 0.9659258262890683122, 1.000000000000000000, 0.9659258262890683122, 1.000000000000000000, 0.9659258262890683122, 1.000000000000000000, 0.9659258262890683122, 1.000000000000000000, 0.9659258262890683122, 1.000000000000000000 ) ) 
 REPRESENTATION_ITEM ( '' )  );
#9022 = CARTESIAN_POINT ( 'NONE',  ( -5.816011393731002066, 28.73617430169783304, 5.000000000000000000 ) ) ;
#9023 = ORIENTED_EDGE ( 'NONE', *, *, #555, .F. ) ;
#9024 = VERTEX_POINT ( 'NONE', #31882 ) ;
#9025 = LINE ( 'NONE', #119255, #99806 ) ;
#9026 = DIRECTION ( 'NONE',  ( -0.6830127018922180770, -0.6830127018922204085, -0.2588190451025213501 ) ) ;
#9027 = VECTOR ( 'NONE', #71525, 999.9999999999998863 ) ;
#9028 = VECTOR ( 'NONE', #41694, 1000.000000000000000 ) ;
#9029 = PLANE ( 'NONE',  #47419 ) ;
#9030 = CARTESIAN_POINT ( 'NONE',  ( 7.014532492589830248, 0.000000000000000000, 2.500000000000000444 ) ) ;
#9031 = CARTESIAN_POINT ( 'NONE',  ( 64.66209685856478018, -5.291415217122919401, 3.054999999999998384 ) ) ;
#9032 = PLANE ( 'NONE',  #95079 ) ;
#9034 = PLANE ( 'NONE',  #136478 ) ;
#9033 = AXIS2_PLACEMENT_3D ( 'NONE', #35010, #56786, #100944 ) ;
#9035 = CARTESIAN_POINT ( 'NONE',  ( 4.600000000000001421, 2.055000000000001492, 0.000000000000000000 ) ) ;
#9036 = CARTESIAN_POINT ( 'NONE',  ( -26.20666063542134339, 21.75929247661549226, 4.998822639870711626 ) ) ;
#9037 = ORIENTED_EDGE ( 'NONE', *, *, #117897, .F. ) ;
#9038 = DIRECTION ( 'NONE',  ( 0.000000000000000000, 9.130123557772669567E-17, -1.000000000000000000 ) ) ;
#9039 = EDGE_CURVE ( 'NONE', #94283, #16938, #84835, .T. ) ;
#9040 = ORIENTED_EDGE ( 'NONE', *, *, #118092, .T. ) ;
#9041 = PLANE ( 'NONE',  #33888 ) ;
#9042 = ORIENTED_EDGE ( 'NONE', *, *, #95731, .T. ) ;
#9043 = VECTOR ( 'NONE', #120008, 1000.000000000000000 ) ;
#9044 = AXIS2_PLACEMENT_3D ( 'NONE', #41542, #107522, #16954 ) ;
#9045 = CIRCLE ( 'NONE', #129535, 2.999999999999999112 ) ;
#9046 = CARTESIAN_POINT ( 'NONE',  ( -15.16464500931035886, 22.22500000000000142, -2.487937186831706171 ) ) ;
#9048 = ORIENTED_EDGE ( 'NONE', *, *, #139614, .T. ) ;
#9047 = DIRECTION ( 'NONE',  ( 1.000000000000000000, 1.224606353822377258E-16, 0.000000000000000000 ) ) ;
#9049 = LINE ( 'NONE', #129448, #2247 ) ;
#9050 = DIRECTION ( 'NONE',  ( -0.6830127018922181881, 0.6830127018922202975, -0.2588190451025214056 ) ) ;
#9051 = FACE_OUTER_BOUND ( 'NONE', #10367, .T. ) ;
#9052 = EDGE_CURVE ( 'NONE', #84184, #122293, #137634, .T. ) ;
#9053 = EDGE_CURVE ( 'NONE', #28495, #64833, #97089, .T. ) ;
#9054 = EDGE_LOOP ( 'NONE', ( #51162, #97972, #36292, #37376, #99045 ) ) ;
#9055 = ORIENTED_EDGE ( 'NONE', *, *, #37158, .F. ) ;
#9056 = LINE ( 'NONE', #65688, #64889 ) ;
#9057 = CARTESIAN_POINT ( 'NONE',  ( 26.20710678118636139, 6.759292476615649470, 5.000000000000000000 ) ) ;
#9058 = CIRCLE ( 'NONE', #90127, 3.999999999999996447 ) ;
#9059 = COLOUR_RGB ( '', 0.72549020, 0.75294118, 0.79215686) ;
#9060 = LINE ( 'NONE', #40345, #26457 ) ;
#9061 = CARTESIAN_POINT ( 'NONE',  ( 34.42499999999998295, 4.541399257802000378, 5.000000000000000000 ) ) ;
#9062 = EDGE_CURVE ( 'NONE', #10646, #94260, #141347, .T. ) ;
#9064 = EDGE_CURVE ( 'NONE', #29147, #1156, #45951, .T. ) ;
#9063 = CARTESIAN_POINT ( 'NONE',  ( 79.99586038379621300, -3.974999999999998312, -6.884901960086286188 ) ) ;
#9065 = DIRECTION ( 'NONE',  ( 0.7071067811865487940, -0.7071067811865463515, 0.000000000000000000 ) ) ;
#9066 = DIRECTION ( 'NONE',  ( -0.7071067811865487940, 0.7071067811865463515, 0.000000000000000000 ) ) ;
#9068 = ADVANCED_FACE ( 'NONE', ( #86278 ), #118141, .T. ) ;
#9067 = ORIENTED_EDGE ( 'NONE', *, *, #113032, .T. ) ;
#9069 = FACE_OUTER_BOUND ( 'NONE', #57568, .T. ) ;
#9070 = ADVANCED_FACE ( 'NONE', ( #43474 ), #131920, .F. ) ;
#9071 = CARTESIAN_POINT ( 'NONE',  ( -12.70000000000000462, -25.83999999999997499, -40.00000000000000711 ) ) ;
#9072 = CARTESIAN_POINT ( 'NONE',  ( 30.33333333333333570, 5.278424836066143655, -3.047499999999997655 ) ) ;
#9073 = VECTOR ( 'NONE', #7445, 1000.000000000000000 ) ;
#9074 = ADVANCED_FACE ( 'NONE', ( #57059 ), #26539, .F. ) ;
#9075 = ORIENTED_EDGE ( 'NONE', *, *, #110071, .F. ) ;
#9076 = CARTESIAN_POINT ( 'NONE',  ( 56.99451991528749062, 28.92564299267978001, 4.000000000000000000 ) ) ;
#9078 = EDGE_LOOP ( 'NONE', ( #62355, #100063, #32421, #57588 ) ) ;
#9077 = ADVANCED_FACE ( 'NONE', ( #47619 ), #134610, .F. ) ;
#9079 = CARTESIAN_POINT ( 'NONE',  ( 77.00043019189811844, -3.055000000000002380, 5.291415217122920289 ) ) ;
#9080 = CARTESIAN_POINT ( 'NONE',  ( 72.48921356237309510, -27.52281430457106026, 5.000000000000000000 ) ) ;
#9081 = FACE_OUTER_BOUND ( 'NONE', #22407, .T. ) ;
#9082 = EDGE_LOOP ( 'NONE', ( #969, #23057, #117965, #75357 ) ) ;
#9083 = CARTESIAN_POINT ( 'NONE',  ( -11.00492477221187393, -5.240707523384228850, 12.38332538355498436 ) ) ;
#9084 = EDGE_CURVE ( 'NONE', #111777, #118671, #55247, .T. ) ;
#9085 = CARTESIAN_POINT ( 'NONE',  ( -11.99999999999992006, -10.06887692260771239, 4.000000000000000000 ) ) ;
#9086 = CARTESIAN_POINT ( 'NONE',  ( 13.64840764549667540, -2.500000000000000888, 0.000000000000000000 ) ) ;
#9087 = CARTESIAN_POINT ( 'NONE',  ( -10.44665057663211449, 2.259292476615697876, 14.86850063742356909 ) ) ;
#9089 = EDGE_LOOP ( 'NONE', ( #106158, #28871, #95644, #58097 ) ) ;
#9088 = CARTESIAN_POINT ( 'NONE',  ( -32.29289321881322650, 8.259292476615637923, 5.000000000000000000 ) ) ;
#9090 = CARTESIAN_POINT ( 'NONE',  ( 5.206660635421493488, 21.75929247661549937, 4.998822639870701856 ) ) ;
#9091 = CARTESIAN_POINT ( 'NONE',  ( -13.82334089840018443, 5.259292476615659240, 15.86257073897100867 ) ) ;
#9092 = EDGE_CURVE ( 'NONE', #35675, #120153, #123733, .T. ) ;
#9093 = LINE ( 'NONE', #44680, #73851 ) ;
#9094 = ORIENTED_EDGE ( 'NONE', *, *, #35669, .F. ) ;
#9095 = VERTEX_POINT ( 'NONE', #70094 ) ;
#9096 = CARTESIAN_POINT ( 'NONE',  ( 62.85459685856477563, -1.637169565754161615, 6.110000000000000320 ) ) ;
#9097 = ORIENTED_EDGE ( 'NONE', *, *, #29054, .T. ) ;
#9098 = LINE ( 'NONE', #53366, #1277 ) ;
#9099 = CARTESIAN_POINT ( 'NONE',  ( -19.11017322888196901, -22.22499999999999432, 4.785647885939354751 ) ) ;
#9100 = DIRECTION ( 'NONE',  ( 0.7071067811865486830, -0.7071067811865464625, -0.000000000000000000 ) ) ;
#9101 = CARTESIAN_POINT ( 'NONE',  ( -59.99451991528749772, 28.92564299267980132, 4.000000000000000000 ) ) ;
#9102 = ORIENTED_EDGE ( 'NONE', *, *, #57276, .T. ) ;
#9103 = LINE ( 'NONE', #97584, #90887 ) ;
#9104 = CARTESIAN_POINT ( 'NONE',  ( 7.799999601179139042, 3.821174125832445049E-16, 0.000000000000000000 ) ) ;
#9105 = EDGE_CURVE ( 'NONE', #83522, #122249, #65640, .T. ) ;
#9106 = ORIENTED_EDGE ( 'NONE', *, *, #3851, .T. ) ;
#9107 = CARTESIAN_POINT ( 'NONE',  ( -31.49999999999977973, -19.91253812416054814, 4.000000000000000000 ) ) ;
#9108 = EDGE_CURVE ( 'NONE', #87703, #71573, #15608, .T. ) ;
#9109 = CARTESIAN_POINT ( 'NONE',  ( 5.994519915287488843, 28.92564299267942118, 4.000000000000000000 ) ) ;
#9110 = CARTESIAN_POINT ( 'NONE',  ( 26.20710678118636139, -2.240707523384257716, 5.000000000000000000 ) ) ;
#9111 = AXIS2_PLACEMENT_3D ( 'NONE', #42235, #106006, #131365 ) ;
#9112 = AXIS2_PLACEMENT_3D ( 'NONE', #91790, #113535, #58521 ) ;
#9113 = AXIS2_PLACEMENT_3D ( 'NONE', #73887, #74617, #105765 ) ;
#9114 = EDGE_CURVE ( 'NONE', #42222, #114028, #123002, .T. ) ;
#9115 = VERTEX_POINT ( 'NONE', #14930 ) ;
#9116 = ORIENTED_EDGE ( 'NONE', *, *, #76782, .F. ) ;
#9117 = CARTESIAN_POINT ( 'NONE',  ( 56.99451991528749062, 28.92564299267978001, 4.000000000000000000 ) ) ;
#9118 = CARTESIAN_POINT ( 'NONE',  ( -60.29974487139158867, -27.71228299555248142, 4.000000000000000000 ) ) ;
#9119 = LINE ( 'NONE', #66427, #127541 ) ;
#9120 = CIRCLE ( 'NONE', #106309, 2.055000000000000604 ) ;
#9121 = CARTESIAN_POINT ( 'NONE',  ( 0.2271987153435547913, -0.6000000000000000888, 3.878866322980131454 ) ) ;
#9122 = SHAPE_REPRESENTATION_RELATIONSHIP ( 'NONE' , 'NONE' ,  #118114, #129565 ) ;
#9123 = ORIENTED_EDGE ( 'NONE', *, *, #67424, .F. ) ;
#9124 = VECTOR ( 'NONE', #48850, 1000.000000000000114 ) ;
#9125 = VERTEX_POINT ( 'NONE', #37423 ) ;
#9126 = CARTESIAN_POINT ( 'NONE',  ( 111.9120968585647944, 5.291415217122921177, -3.054999999999994831 ) ) ;
#9127 = ORIENTED_EDGE ( 'NONE', *, *, #52558, .T. ) ;
#9128 = EDGE_CURVE ( 'NONE', #22009, #57196, #12782, .T. ) ;
#9129 = ORIENTED_EDGE ( 'NONE', *, *, #73652, .F. ) ;
#9130 = AXIS2_PLACEMENT_3D ( 'NONE', #42129, #52260, #142847 ) ;
#9131 = VECTOR ( 'NONE', #140754, 1000.000000000000000 ) ;
#9132 = CARTESIAN_POINT ( 'NONE',  ( 183.7681020908654261, -51.95642703808907470, 39.54367611436589414 ) ) ;
#9133 = LINE ( 'NONE', #66444, #133467 ) ;
#9134 = VECTOR ( 'NONE', #110032, 1000.000000000000114 ) ;
#9135 = DIRECTION ( 'NONE',  ( 0.7071067811865487940, -0.7071067811865463515, 0.000000000000000000 ) ) ;
#9136 = ORIENTED_EDGE ( 'NONE', *, *, #28622, .T. ) ;
#9137 = DIRECTION ( 'NONE',  ( -0.6830127018922181881, 0.6830127018922202975, -0.2588190451025214056 ) ) ;
#9138 = LINE ( 'NONE', #53410, #54197 ) ;
#9139 = EDGE_CURVE ( 'NONE', #90720, #85257, #114255, .T. ) ;
#9140 = DIRECTION ( 'NONE',  ( -0.6830127018922180770, -0.6830127018922204085, -0.2588190451025213501 ) ) ;
#9141 = CARTESIAN_POINT ( 'NONE',  ( 48.29974487139158867, -27.71228299555239971, 4.000000000000000000 ) ) ;
#9142 = AXIS2_PLACEMENT_3D ( 'NONE', #69823, #99526, #113268 ) ;
#9143 = CARTESIAN_POINT ( 'NONE',  ( -2.563198967791689764, -12.74070752338415247, 9.898150129686381860 ) ) ;
#9144 = VERTEX_POINT ( 'NONE', #2622 ) ;
#9145 = AXIS2_PLACEMENT_3D ( 'NONE', #140014, #16779, #18169 ) ;
#9146 = FACE_OUTER_BOUND ( 'NONE', #67145, .T. ) ;
#9147 = DIRECTION ( 'NONE',  ( 0.7071067811865487940, 0.7071067811865463515, 0.000000000000000000 ) ) ;
#9148 = VERTEX_POINT ( 'NONE', #91106 ) ;
#9150 = ADVANCED_FACE ( 'NONE', ( #81666 ), #3329, .F. ) ;
#9149 = CARTESIAN_POINT ( 'NONE',  ( 2.613322195557305605, 4.202752102959690472E-16, 0.000000000000000000 ) ) ;
#9151 = ORIENTED_EDGE ( 'NONE', *, *, #8038, .F. ) ;
#9152 = PLANE ( 'NONE',  #34173 ) ;
#9153 = ORIENTED_EDGE ( 'NONE', *, *, #14514, .F. ) ;
#9154 = AXIS2_PLACEMENT_3D ( 'NONE', #92681, #39777, #115841 ) ;
#9155 = ORIENTED_EDGE ( 'NONE', *, *, #62325, .F. ) ;
#9157 = VECTOR ( 'NONE', #112022, 1000.000000000000000 ) ;
#9156 = CARTESIAN_POINT ( 'NONE',  ( 60.22959685856476142, -6.110000000000000320, -1.637169565754161393 ) ) ;
#9158 = EDGE_LOOP ( 'NONE', ( #28849, #81274, #122965, #14637, #17212 ) ) ;
#9159 = ORIENTED_EDGE ( 'NONE', *, *, #57791, .F. ) ;
#9160 = DIRECTION ( 'NONE',  ( 0.7071067811865487940, -0.7071067811865463515, 0.000000000000000000 ) ) ;
#9161 = EDGE_CURVE ( 'NONE', #85868, #25060, #59893, .T. ) ;
#9162 = CARTESIAN_POINT ( 'NONE',  ( -1.558360383796227655, -6.094999999999989093, 1.633150327867691765 ) ) ;
#9163 = CARTESIAN_POINT ( 'NONE',  ( 98.43793019189811844, -6.110000000000001208, 1.637169565754158951 ) ) ;
#9164 = DIRECTION ( 'NONE',  ( 0.7071067811865487940, 0.7071067811865463515, -0.000000000000000000 ) ) ;
#9165 = EDGE_CURVE ( 'NONE', #24914, #83531, #46186, .T. ) ;
#9166 = CARTESIAN_POINT ( 'NONE',  ( 28.17183060077627488, 3.759292476615680112, 4.000000000000000000 ) ) ;
#9167 = ORIENTED_EDGE ( 'NONE', *, *, #119098, .F. ) ;
#9168 = FACE_OUTER_BOUND ( 'NONE', #114419, .T. ) ;
#9169 = VECTOR ( 'NONE', #3885, 1000.000000000000000 ) ;
#9170 = CARTESIAN_POINT ( 'NONE',  ( -5.816011393731002066, 28.73617430169783304, 5.000000000000000000 ) ) ;
#9171 = EDGE_CURVE ( 'NONE', #123192, #142351, #35305, .T. ) ;
#9172 = DIRECTION ( 'NONE',  ( 2.781805975412905890E-17, -0.3543493200069152693, 0.9351131265310292928 ) ) ;
#9173 = LINE ( 'NONE', #31001, #135469 ) ;
#9174 = ORIENTED_EDGE ( 'NONE', *, *, #31669, .F. ) ;
#9175 = EDGE_CURVE ( 'NONE', #132281, #142117, #125869, .T. ) ;
#9176 = CARTESIAN_POINT ( 'NONE',  ( -27.18398860626900060, 28.73617430169806042, 5.000000000000000000 ) ) ;
#9177 = ORIENTED_EDGE ( 'NONE', *, *, #105365, .T. ) ;
#9178 = VERTEX_POINT ( 'NONE', #80234 ) ;
#9179 = ORIENTED_EDGE ( 'NONE', *, *, #72348, .F. ) ;
#9180 = CARTESIAN_POINT ( 'NONE',  ( 120.3704301918981230, -3.055000000000001492, 5.291415217122917625 ) ) ;
#9181 = ORIENTED_EDGE ( 'NONE', *, *, #66169, .T. ) ;
#9182 = AXIS2_PLACEMENT_3D ( 'NONE', #112635, #4514, #80745 ) ;
#9183 = CARTESIAN_POINT ( 'NONE',  ( 0.000000000000000000, 0.000000000000000000, 5.000000000000000000 ) ) ;
#9184 = CARTESIAN_POINT ( 'NONE',  ( -42.18398860626899705, 28.73617430169816700, 5.000000000000000000 ) ) ;
#9185 = PLANE ( 'NONE',  #11605 ) ;
#9186 = EDGE_CURVE ( 'NONE', #100169, #56865, #36685, .T. ) ;
#9187 = VERTEX_POINT ( 'NONE', #83812 ) ;
#9188 = CARTESIAN_POINT ( 'NONE',  ( 30.18398860626900060, 28.73617430169808173, 5.000000000000000000 ) ) ;
#9189 = EDGE_LOOP ( 'NONE', ( #50606, #56404, #86175, #129009 ) ) ;
#9190 = CARTESIAN_POINT ( 'NONE',  ( 11.93706980810188689, 2.126176841940952134, -7.934999999999993392 ) ) ;
#9191 = CARTESIAN_POINT ( 'NONE',  ( -30.48921356237309510, -27.52281430457076894, 5.000000000000000000 ) ) ;
#9192 = LINE ( 'NONE', #143323, #27464 ) ;
#9193 = CARTESIAN_POINT ( 'NONE',  ( 34.42499999999998295, 2.977185695429370504, 5.000000000000000000 ) ) ;
#9194 = EDGE_LOOP ( 'NONE', ( #48404, #130165, #120221, #122182, #13890, #72824 ) ) ;
#9195 = VERTEX_POINT ( 'NONE', #63488 ) ;
#9196 = VERTEX_POINT ( 'NONE', #117789 ) ;
#9197 = FACE_OUTER_BOUND ( 'NONE', #1382, .T. ) ;
#9198 = FACE_OUTER_BOUND ( 'NONE', #74226, .T. ) ;
#9199 = CARTESIAN_POINT ( 'NONE',  ( 14.99451991528749595, 28.92564299267948513, 4.000000000000000000 ) ) ;
#9200 = CARTESIAN_POINT ( 'NONE',  ( 34.92499999999998295, -22.22500000000000142, 4.500000000000000888 ) ) ;
#9201 = DIRECTION ( 'NONE',  ( 0.7071067811865486830, -0.7071067811865464625, -0.000000000000000000 ) ) ;
#9202 = AXIS2_PLACEMENT_3D ( 'NONE', #23862, #57227, #103526 ) ;
#9203 = CARTESIAN_POINT ( 'NONE',  ( 15.29974487139158867, -27.71228299555216879, 4.000000000000000000 ) ) ;
#9204 = CARTESIAN_POINT ( 'NONE',  ( 26.39626352523143282, 4.472830434245840259, -4.472830434245839371 ) ) ;
#9205 = DIRECTION ( 'NONE',  ( 1.000000000000000000, 0.000000000000000000, 0.000000000000000000 ) ) ;
#9206 = DIRECTION ( 'NONE',  ( -0.3543493200069162685, -0.000000000000000000, -0.9351131265310288487 ) ) ;
#9207 = ORIENTED_EDGE ( 'NONE', *, *, #77113, .T. ) ;
#9208 = CARTESIAN_POINT ( 'NONE',  ( -36.48921356237310221, -27.52281430457080802, 5.000000000000000000 ) ) ;
#9209 = EDGE_LOOP ( 'NONE', ( #126002, #32613, #23661, #139940 ) ) ;
#9210 = VECTOR ( 'NONE', #139950, 1000.000000000000000 ) ;
#9211 = AXIS2_PLACEMENT_3D ( 'NONE', #76878, #45674, #88453 ) ;
#9212 = AXIS2_PLACEMENT_3D ( 'NONE', #134805, #56558, #24577 ) ;
#9213 = LINE ( 'NONE', #11364, #105524 ) ;
#9214 = ORIENTED_EDGE ( 'NONE', *, *, #36877, .T. ) ;
#9215 = VECTOR ( 'NONE', #70592, 1000.000000000000000 ) ;
#9216 = LINE ( 'NONE', #18690, #43666 ) ;
#9218 = VERTEX_POINT ( 'NONE', #128019 ) ;
#9217 = PLANE ( 'NONE',  #120465 ) ;
#9219 = PLANE ( 'NONE',  #123311 ) ;
#9220 = ORIENTED_EDGE ( 'NONE', *, *, #55235, .T. ) ;
#9221 = CARTESIAN_POINT ( 'NONE',  ( -25.03340032343007238, 6.759292476615653023, 12.28218704918516302 ) ) ;
#9222 = VERTEX_POINT ( 'NONE', #127265 ) ;
#9223 = FACE_OUTER_BOUND ( 'NONE', #136753, .T. ) ;
#9224 =( GEOMETRIC_REPRESENTATION_CONTEXT ( 3 ) GLOBAL_UNCERTAINTY_ASSIGNED_CONTEXT ( ( #24410 ) ) GLOBAL_UNIT_ASSIGNED_CONTEXT ( ( #34609, #112183, #133921 ) ) REPRESENTATION_CONTEXT ( 'NONE', 'WORKASPACE' ) );
#9225 = ORIENTED_EDGE ( 'NONE', *, *, #104797, .F. ) ;
#9227 = EDGE_CURVE ( 'NONE', #53505, #65082, #72944, .T. ) ;
#9226 = CARTESIAN_POINT ( 'NONE',  ( 108.7250270504628844, 5.819803920172573086, -5.819803920172572198 ) ) ;
#9228 = DIRECTION ( 'NONE',  ( 1.000000000000000000, 0.000000000000000000, 0.000000000000000000 ) ) ;
#9229 = DIRECTION ( 'NONE',  ( 0.000000000000000000, 0.000000000000000000, 1.000000000000000000 ) ) ;
#9230 = EDGE_CURVE ( 'NONE', #52329, #65412, #83065, .T. ) ;
#9231 = DIRECTION ( 'NONE',  ( 0.7071067811865487940, -0.7071067811865463515, 0.000000000000000000 ) ) ;
#9232 = CARTESIAN_POINT ( 'NONE',  ( -34.42500000000001137, -22.22500000000000142, 5.000000000000000000 ) ) ;
#9233 = EDGE_CURVE ( 'NONE', #31173, #25152, #117093, .T. ) ;
#9234 = CARTESIAN_POINT ( 'NONE',  ( 24.48921356237309510, -27.52281430457072631, 5.000000000000000000 ) ) ;
#9235 = CARTESIAN_POINT ( 'NONE',  ( 1.020833333333333481, -6.094999999999989981, -1.633150327867689100 ) ) ;
#9236 = CARTESIAN_POINT ( 'NONE',  ( 18.06206980810188867, -7.934999999999990727, -2.126176841940955242 ) ) ;
#9237 = VECTOR ( 'NONE', #133939, 999.9999999999998863 ) ;
#9238 = PLANE ( 'NONE',  #30410 ) ;
#9240 = ADVANCED_FACE ( 'NONE', ( #27966 ), #17771, .F. ) ;
#9239 = PLANE ( 'NONE',  #80221 ) ;
#9241 = ORIENTED_EDGE ( 'NONE', *, *, #2538, .F. ) ;
#9242 = ORIENTED_EDGE ( 'NONE', *, *, #78642, .T. ) ;
#9243 = VECTOR ( 'NONE', #115543, 1000.000000000000000 ) ;
#9244 = DIRECTION ( 'NONE',  ( -0.000000000000000000, 0.000000000000000000, 1.000000000000000000 ) ) ;
#9245 = VERTEX_POINT ( 'NONE', #62046 ) ;
#9246 = EDGE_CURVE ( 'NONE', #57093, #141023, #40987, .T. ) ;
#9247 = VECTOR ( 'NONE', #123617, 999.9999999999998863 ) ;
#9248 = CARTESIAN_POINT ( 'NONE',  ( 91.37086038379622721, 6.884901960086289741, -3.974999999999993427 ) ) ;
#9249 = CARTESIAN_POINT ( 'NONE',  ( 1.500000000000000000, 0.000000000000000000, 0.000000000000000000 ) ) ;
#9250 = DIRECTION ( 'NONE',  ( -0.7071067811865486830, -0.7071067811865464625, 0.000000000000000000 ) ) ;
#9251 = PLANE ( 'NONE',  #13098 ) ;
#9252 = ORIENTED_EDGE ( 'NONE', *, *, #56366, .T. ) ;
#9253 = CIRCLE ( 'NONE', #90322, 2.500000000000000888 ) ;
#9254 = LINE ( 'NONE', #86876, #103027 ) ;
#9255 = DIRECTION ( 'NONE',  ( -0.3543493200069162685, -0.000000000000000000, -0.9351131265310288487 ) ) ;
#9256 = EDGE_CURVE ( 'NONE', #124198, #75105, #95355, .T. ) ;
#9257 = CARTESIAN_POINT ( 'NONE',  ( 93.75000000000000000, -9.735942053221458872E-16, 7.950000000000000178 ) ) ;
#9258 = EDGE_CURVE ( 'NONE', #30612, #106170, #38846, .T. ) ;
#9259 = VECTOR ( 'NONE', #139063, 1000.000000000000114 ) ;
#9261 = VERTEX_POINT ( 'NONE', #128703 ) ;
#9260 = CARTESIAN_POINT ( 'NONE',  ( 23.99999999999982947, 10.93112307739207623, 4.000000000000000000 ) ) ;
#9262 = DIRECTION ( 'NONE',  ( 1.000000000000000000, 0.000000000000000000, 0.000000000000000000 ) ) ;
#9263 = VECTOR ( 'NONE', #113976, 1000.000000000000000 ) ;
#9264 = LINE ( 'NONE', #7863, #91571 ) ;
#9265 = CARTESIAN_POINT ( 'NONE',  ( -2.994519915287485734, 28.92564299267940342, 4.000000000000000000 ) ) ;
#9266 = PLANE ( 'NONE',  #103451 ) ;
#9267 = ADVANCED_FACE ( 'NONE', ( #93217 ), #39577, .T. ) ;
#9268 = LINE ( 'NONE', #53544, #88584 ) ;
#9269 = ORIENTED_EDGE ( 'NONE', *, *, #79857, .T. ) ;
#9270 = ORIENTED_EDGE ( 'NONE', *, *, #78902, .F. ) ;
#9271 = ORIENTED_EDGE ( 'NONE', *, *, #26447, .F. ) ;
#9272 = CARTESIAN_POINT ( 'NONE',  ( 95.08376352523144703, -6.110000000000001208, -3.741295971395164515E-16 ) ) ;
#9273 = VECTOR ( 'NONE', #118472, 1000.000000000000000 ) ;
#9274 = ORIENTED_EDGE ( 'NONE', *, *, #126637, .F. ) ;
#9275 = CARTESIAN_POINT ( 'NONE',  ( 128.5894344200537489, -52.00875322212550600, 39.86617647058824332 ) ) ;
#9276 = VECTOR ( 'NONE', #102558, 1000.000000000000000 ) ;
#9277 = DIRECTION ( 'NONE',  ( -0.6830127018922180770, -0.6830127018922204085, -0.2588190451025213501 ) ) ;
#9278 = ORIENTED_EDGE ( 'NONE', *, *, #40746, .F. ) ;
#9279 = DIRECTION ( 'NONE',  ( 0.6830127018922181881, 0.6830127018922202975, -0.2588190451025214056 ) ) ;
#9280 = CARTESIAN_POINT ( 'NONE',  ( -23.99999999999982592, -10.44781430457072346, 5.000000000000000000 ) ) ;
#9281 = CARTESIAN_POINT ( 'NONE',  ( 93.53709685856479439, -3.054999999999998828, -5.291415217122919401 ) ) ;
#9282 = ORIENTED_EDGE ( 'NONE', *, *, #127140, .F. ) ;
#9283 = CARTESIAN_POINT ( 'NONE',  ( -3.080955290695428076E-14, 0.5999999999999988676, -3.226721766443181760 ) ) ;
#9284 = EDGE_CURVE ( 'NONE', #50102, #95024, #40301, .T. ) ;
#9285 = DIRECTION ( 'NONE',  ( -1.000000000000000000, -1.224606353822377258E-16, -0.000000000000000000 ) ) ;
#9286 = AXIS2_PLACEMENT_3D ( 'NONE', #5087, #3654, #38476 ) ;
#9287 = CARTESIAN_POINT ( 'NONE',  ( 30.48921356237309510, -27.52281430457076894, 5.000000000000000000 ) ) ;
#9288 = VERTEX_POINT ( 'NONE', #116404 ) ;
#9289 = ORIENTED_EDGE ( 'NONE', *, *, #137726, .F. ) ;
#9290 = ORIENTED_EDGE ( 'NONE', *, *, #32543, .T. ) ;
#9291 = CARTESIAN_POINT ( 'NONE',  ( -18.09843580608225366, 11.25929247661560595, 10.79108189686402852 ) ) ;
#9292 = FACE_OUTER_BOUND ( 'NONE', #120453, .T. ) ;
#9293 = CARTESIAN_POINT ( 'NONE',  ( 13.92123647476855197, -9.717572351234235426E-16, -7.934999999999990727 ) ) ;
#9294 = AXIS2_PLACEMENT_3D ( 'NONE', #134468, #24267, #34428 ) ;
#9295 = CARTESIAN_POINT ( 'NONE',  ( 160.4290834833332440, 26.96999999999994913, 34.92499999999999716 ) ) ;
#9296 = DIRECTION ( 'NONE',  ( -0.7071067811865486830, -0.7071067811865464625, 0.000000000000000000 ) ) ;
#9297 = ORIENTED_EDGE ( 'NONE', *, *, #20668, .T. ) ;
#9298 = ORIENTED_EDGE ( 'NONE', *, *, #77651, .T. ) ;
#9299 = CARTESIAN_POINT ( 'NONE',  ( 1.499999999999987566, 8.900465351122152313, -2.516491619111516531 ) ) ;
#9301 = ORIENTED_EDGE ( 'NONE', *, *, #61687, .F. ) ;
#9300 = EDGE_CURVE ( 'NONE', #53394, #80081, #84507, .T. ) ;
#9302 = VERTEX_POINT ( 'NONE', #85184 ) ;
#9303 = MECHANICAL_DESIGN_GEOMETRIC_PRESENTATION_REPRESENTATION (  '', ( #111157 ), #23539 ) ;
#9304 =( BOUNDED_CURVE ( )  B_SPLINE_CURVE ( 2, ( #25773, #78749, #46887, #112786, #134570, #57723, #122962 ),
 .UNSPECIFIED., .F., .F. ) 
 B_SPLINE_CURVE_WITH_KNOTS ( ( 3, 2, 2, 3 ),
 ( 0.9666666666666666741, 0.9694444444444444420, 0.9722222222222222099, 0.9741589280471857348 ),
 .UNSPECIFIED. ) 
 CURVE ( )  GEOMETRIC_REPRESENTATION_ITEM ( )  RATIONAL_B_SPLINE_CURVE ( ( 1.000000000000000000, 0.9659258262890683122, 1.000000000000000000, 0.9659258262890683122, 1.000000000000000000, 0.9762430057455590005, 0.9856134340835827068 ) ) 
 REPRESENTATION_ITEM ( '' )  );
#9305 = VECTOR ( 'NONE', #79995, 999.9999999999998863 ) ;
#9306 = LINE ( 'NONE', #29662, #37337 ) ;
#9307 = LINE ( 'NONE', #109383, #79829 ) ;
#9308 = ORIENTED_EDGE ( 'NONE', *, *, #86393, .T. ) ;
#9309 = CARTESIAN_POINT ( 'NONE',  ( -5.207106781186502609, -5.240707523384230626, 5.000000000000000000 ) ) ;
#9310 = LINE ( 'NONE', #41262, #25254 ) ;
#9311 = EDGE_CURVE ( 'NONE', #49712, #28781, #62756, .T. ) ;
#9312 = CARTESIAN_POINT ( 'NONE',  ( -12.49816348513948761, -17.24070752338410628, 8.407044977365254468 ) ) ;
#9313 = LINE ( 'NONE', #116697, #99275 ) ;
#9314 = VECTOR ( 'NONE', #43839, 1000.000000000000000 ) ;
#9315 = AXIS2_PLACEMENT_3D ( 'NONE', #114272, #14245, #70799 ) ;
#9316 = AXIS2_PLACEMENT_3D ( 'NONE', #1619, #55343, #56082 ) ;
#9317 =( BOUNDED_CURVE ( )  B_SPLINE_CURVE ( 3, ( #11852, #56141, #978, #45263 ),
 .UNSPECIFIED., .F., .T. ) 
 B_SPLINE_CURVE_WITH_KNOTS ( ( 4, 4 ),
 ( 1.142100667999822683, 1.182775789206201411 ),
 .UNSPECIFIED. ) 
 CURVE ( )  GEOMETRIC_REPRESENTATION_ITEM ( )  RATIONAL_B_SPLINE_CURVE ( ( 1.000000000000000000, 0.9998621326283523292, 0.9998621326283523292, 1.000000000000000000 ) ) 
 REPRESENTATION_ITEM ( '' )  );
#9318 = CARTESIAN_POINT ( 'NONE',  ( 20.51159235450331764, 9.902892378096218942E-16, 0.000000000000000000 ) ) ;
#9319 = ORIENTED_EDGE ( 'NONE', *, *, #132872, .T. ) ;
#9320 = VECTOR ( 'NONE', #98705, 1000.000000000000000 ) ;
#9321 = LINE ( 'NONE', #75356, #69627 ) ;
#9322 = VERTEX_POINT ( 'NONE', #51880 ) ;
#9323 = CARTESIAN_POINT ( 'NONE',  ( 25.40000000000001279, 0.9275341018601235277, -7.891049174277950051 ) ) ;
#9325 = EDGE_CURVE ( 'NONE', #130843, #3304, #129407, .T. ) ;
#9324 = CARTESIAN_POINT ( 'NONE',  ( 60.29974487139158867, -27.71228299555248142, 4.000000000000000000 ) ) ;
#9326 = VERTEX_POINT ( 'NONE', #71479 ) ;
#9327 = DIRECTION ( 'NONE',  ( 0.7071067811865486830, -0.7071067811865464625, -0.000000000000000000 ) ) ;
#9328 = ORIENTED_EDGE ( 'NONE', *, *, #115909, .F. ) ;
#9329 = CARTESIAN_POINT ( 'NONE',  ( 60.18398860626900415, 28.73617430169829490, 5.000000000000000000 ) ) ;
#9330 = ORIENTED_EDGE ( 'NONE', *, *, #60016, .T. ) ;
#9331 = VERTEX_POINT ( 'NONE', #115644 ) ;
#9332 = VECTOR ( 'NONE', #6393, 1000.000000000000227 ) ;
#9333 = ORIENTED_EDGE ( 'NONE', *, *, #49280, .F. ) ;
#9334 = CARTESIAN_POINT ( 'NONE',  ( 27.03709685856478373, -3.054999999999998828, -5.291415217122919401 ) ) ;
#9335 = DIRECTION ( 'NONE',  ( 0.7071067811865486830, -0.7071067811865464625, -0.000000000000000000 ) ) ;
#9336 = LINE ( 'NONE', #87660, #112073 ) ;
#9337 = CARTESIAN_POINT ( 'NONE',  ( 126.8754301918981184, -5.291415217122920289, -3.055000000000001492 ) ) ;
#9338 = DIRECTION ( 'NONE',  ( 0.6830127018922181881, 0.6830127018922202975, -0.2588190451025214056 ) ) ;
#9339 = LINE ( 'NONE', #87664, #62128 ) ;
#9341 = LINE ( 'NONE', #44178, #58335 ) ;
#9340 = CARTESIAN_POINT ( 'NONE',  ( 7.828169399223474656, -2.240707523384259492, 4.000000000000000000 ) ) ;
#9342 = PRESENTATION_LAYER_ASSIGNMENT (  '', '', ( #4668 ) ) ;
#9343 = DIRECTION ( 'NONE',  ( -0.000000000000000000, -0.3543493200069152693, 0.9351131265310292928 ) ) ;
#9344 = EDGE_CURVE ( 'NONE', #130559, #45081, #17093, .T. ) ;
#9345 = VECTOR ( 'NONE', #52997, 1000.000000000000000 ) ;
#9346 = CARTESIAN_POINT ( 'NONE',  ( 5.111623618947549019, 9.759292476615607725, 17.35367589129211652 ) ) ;
#9347 = AXIS2_PLACEMENT_3D ( 'NONE', #68266, #35630, #11658 ) ;
#9348 = EDGE_CURVE ( 'NONE', #1016, #104350, #30093, .T. ) ;
#9349 = LINE ( 'NONE', #108660, #71483 ) ;
#9350 = DIRECTION ( 'NONE',  ( -0.7071067811865486830, -0.7071067811865464625, -0.000000000000000000 ) ) ;
#9351 = ORIENTED_EDGE ( 'NONE', *, *, #103705, .T. ) ;
#9352 = VECTOR ( 'NONE', #6742, 1000.000000000000000 ) ;
#9353 = ORIENTED_EDGE ( 'NONE', *, *, #122732, .F. ) ;
#9354 = VERTEX_POINT ( 'NONE', #104808 ) ;
#9355 = ORIENTED_EDGE ( 'NONE', *, *, #120662, .T. ) ;
#9356 = CARTESIAN_POINT ( 'NONE',  ( 3.489213562373097322, -27.52281430457057709, 5.000000000000000000 ) ) ;
#9357 = ORIENTED_EDGE ( 'NONE', *, *, #20410, .T. ) ;
#9358 = VECTOR ( 'NONE', #3876, 1000.000000000000000 ) ;
#9359 = ORIENTED_EDGE ( 'NONE', *, *, #116154, .T. ) ;
#9360 = CARTESIAN_POINT ( 'NONE',  ( 26.99999999999981171, 5.966399257802205369, 5.000000000000000000 ) ) ;
#9361 = CARTESIAN_POINT ( 'NONE',  ( 2.999999999999999112, 0.000000000000000000, 0.000000000000000000 ) ) ;
#9362 = ADVANCED_FACE ( 'NONE', ( #5468 ), #93926, .F. ) ;
#9363 = AXIS2_PLACEMENT_3D ( 'NONE', #16939, #40834, #138730 ) ;
#9364 = EDGE_CURVE ( 'NONE', #115521, #77672, #54732, .T. ) ;
#9365 = CARTESIAN_POINT ( 'NONE',  ( -36.29974487139159578, -27.71228299555231445, 4.000000000000000000 ) ) ;
#9366 = ORIENTED_EDGE ( 'NONE', *, *, #82333, .T. ) ;
#9367 = CARTESIAN_POINT ( 'NONE',  ( -4.499999999999968914, -14.70932175296478128, -11.46312253303836215 ) ) ;
#9368 = ORIENTED_EDGE ( 'NONE', *, *, #139949, .F. ) ;
#9369 =( LENGTH_UNIT ( ) NAMED_UNIT ( * ) SI_UNIT ( .MILLI., .METRE. ) );
#9370 = CARTESIAN_POINT ( 'NONE',  ( 7.134088674951085451, -39.93000000000000682, 19.02448003456068548 ) ) ;
#9371 = VECTOR ( 'NONE', #19258, 1000.000000000000000 ) ;
#9372 = CARTESIAN_POINT ( 'NONE',  ( 9.108736474768550195, -5.808823158059033709, 5.808823158059035485 ) ) ;
#9373 = ORIENTED_EDGE ( 'NONE', *, *, #64600, .T. ) ;
#9374 = CARTESIAN_POINT ( 'NONE',  ( 91.34959685856478018, 6.109999999999997655, 1.637169565754163836 ) ) ;
#9375 = CARTESIAN_POINT ( 'NONE',  ( 5.980202007725322844, -9.485991381305455050, 0.5885017396600767947 ) ) ;
#9376 = DIRECTION ( 'NONE',  ( 0.7071067811865487940, -0.7071067811865463515, 0.000000000000000000 ) ) ;
#9377 = DIRECTION ( 'NONE',  ( -0.000000000000000000, 0.3543493200069153248, 0.9351131265310292928 ) ) ;
#9378 = ORIENTED_EDGE ( 'NONE', *, *, #76274, .F. ) ;
#9379 = ORIENTED_EDGE ( 'NONE', *, *, #140544, .F. ) ;
#9380 = CARTESIAN_POINT ( 'NONE',  ( 0.000000000000000000, -2.375000000000000000, 4.319999999999998508 ) ) ;
#9381 = VECTOR ( 'NONE', #135559, 999.9999999999998863 ) ;
#9382 = ORIENTED_EDGE ( 'NONE', *, *, #23556, .F. ) ;
#9383 = CARTESIAN_POINT ( 'NONE',  ( 9.208651418775088970, 4.584330080086930965E-16, 0.000000000000000000 ) ) ;
#9384 = CARTESIAN_POINT ( 'NONE',  ( -23.99999999999982947, -7.447814304570756327, 5.000000000000000000 ) ) ;
#9385 = CARTESIAN_POINT ( 'NONE',  ( -34.49999999999975131, -1.912538124160733766, 4.000000000000000000 ) ) ;
#9386 = FACE_OUTER_BOUND ( 'NONE', #135309, .T. ) ;
#9387 = EDGE_CURVE ( 'NONE', #19769, #131428, #86651, .T. ) ;
#9388 = ORIENTED_EDGE ( 'NONE', *, *, #25788, .F. ) ;
#9389 = FACE_OUTER_BOUND ( 'NONE', #125906, .T. ) ;
#9390 = LINE ( 'NONE', #108706, #72121 ) ;
#9391 = CARTESIAN_POINT ( 'NONE',  ( 23.67183060077630330, -3.740707523384243505, 4.000000000000000000 ) ) ;
#9392 = ORIENTED_EDGE ( 'NONE', *, *, #47642, .F. ) ;
#9393 = DIRECTION ( 'NONE',  ( -1.000000000000000000, 0.000000000000000000, -0.000000000000000000 ) ) ;
#9394 = VECTOR ( 'NONE', #104811, 1000.000000000000227 ) ;
#9395 = FACE_OUTER_BOUND ( 'NONE', #33300, .T. ) ;
#9396 = ORIENTED_EDGE ( 'NONE', *, *, #110942, .T. ) ;
#9398 = ORIENTED_EDGE ( 'NONE', *, *, #6099, .F. ) ;
#9397 = DIRECTION ( 'NONE',  ( -0.000000000000000000, -0.9647414015272155474, 0.2631995976047525887 ) ) ;
#9399 = ORIENTED_EDGE ( 'NONE', *, *, #43491, .F. ) ;
#9400 = CARTESIAN_POINT ( 'NONE',  ( 29.99999999999979039, 1.761378380278712186, -6.096875308897186763 ) ) ;
#9401 = FACE_OUTER_BOUND ( 'NONE', #17407, .T. ) ;
#9403 = VERTEX_POINT ( 'NONE', #30845 ) ;
#9402 = AXIS2_PLACEMENT_3D ( 'NONE', #21941, #110359, #55310 ) ;
#9404 = PLANE ( 'NONE',  #25713 ) ;
#9405 = DIRECTION ( 'NONE',  ( -1.000000000000000000, -1.224606353822377258E-16, -0.000000000000000000 ) ) ;
#9406 = EDGE_CURVE ( 'NONE', #63949, #99331, #130875, .T. ) ;
#9407 = DIRECTION ( 'NONE',  ( 0.7071067811865487940, -0.7071067811865463515, 0.000000000000000000 ) ) ;
#9408 = PLANE ( 'NONE',  #94757 ) ;
#9409 = EDGE_CURVE ( 'NONE', #65559, #126328, #31542, .T. ) ;
#9410 = CARTESIAN_POINT ( 'NONE',  ( 0.1600000000000004752, -2.314171071560278126, -7.597438125929392605 ) ) ;
#9411 = PLANE ( 'NONE',  #109181 ) ;
#9412 = DIRECTION ( 'NONE',  ( 0.7071067811865486830, -0.7071067811865464625, -0.000000000000000000 ) ) ;
#9413 = FILL_AREA_STYLE_COLOUR ( '', #32192 ) ;
#9414 = DIRECTION ( 'NONE',  ( -0.7071067811865486830, -0.7071067811865464625, 0.000000000000000000 ) ) ;
#9415 = CARTESIAN_POINT ( 'NONE',  ( 8.292893218813405909, -0.7407075233842735917, 5.000000000000000000 ) ) ;
#9416 = CARTESIAN_POINT ( 'NONE',  ( -51.48921356237309510, -27.52281430457091460, 5.000000000000000000 ) ) ;
#9417 = VECTOR ( 'NONE', #43169, 1000.000000000000000 ) ;
#9418 = LINE ( 'NONE', #52939, #37246 ) ;
#9420 = ADVANCED_FACE ( 'NONE', ( #301 ), #132311, .F. ) ;
#9419 = PLANE ( 'NONE',  #105614 ) ;
#9422 = EDGE_CURVE ( 'NONE', #79985, #38905, #88064, .T. ) ;
#9421 = EDGE_LOOP ( 'NONE', ( #80099, #35495, #41797, #99407, #16065, #21186 ) ) ;
#9423 = ORIENTED_EDGE ( 'NONE', *, *, #128350, .F. ) ;
#9424 = ORIENTED_EDGE ( 'NONE', *, *, #52468, .F. ) ;
#9425 = AXIS2_PLACEMENT_3D ( 'NONE', #35276, #65774, #109937 ) ;
#9426 = CARTESIAN_POINT ( 'NONE',  ( 103.2291666666666714, 7.950000000000001954, -2.130196079827421762 ) ) ;
#9427 = VERTEX_POINT ( 'NONE', #98230 ) ;
#9428 = VERTEX_POINT ( 'NONE', #75769 ) ;
#9429 = EDGE_LOOP ( 'NONE', ( #118865, #106263, #56842, #37729, #69593 ) ) ;
#9430 = LINE ( 'NONE', #8701, #87279 ) ;
#9431 = DIRECTION ( 'NONE',  ( 0.000000000000000000, 0.000000000000000000, 1.000000000000000000 ) ) ;
#9432 = VECTOR ( 'NONE', #67591, 999.9999999999998863 ) ;
#9433 = AXIS2_PLACEMENT_3D ( 'NONE', #127126, #27826, #72091 ) ;
#9434 = VECTOR ( 'NONE', #109097, 1000.000000000000000 ) ;
#9435 = MECHANICAL_DESIGN_GEOMETRIC_PRESENTATION_REPRESENTATION (  '', ( #53452 ), #44272 ) ;
#9436 = VERTEX_POINT ( 'NONE', #109808 ) ;
#9437 = DIRECTION ( 'NONE',  ( -0.7071067811865486830, -0.7071067811865464625, 0.000000000000000000 ) ) ;
#9438 = STYLED_ITEM ( 'NONE', ( #80911 ), #115316 ) ;
#9439 = CARTESIAN_POINT ( 'NONE',  ( -3.328169399223502189, -0.7407075233842770334, 4.000000000000000000 ) ) ;
#9440 = EDGE_CURVE ( 'NONE', #104604, #138539, #122095, .T. ) ;
#9441 = DIRECTION ( 'NONE',  ( -0.6830127018922181881, 0.6830127018922202975, -0.2588190451025214056 ) ) ;
#9442 = CARTESIAN_POINT ( 'NONE',  ( 0.000000000000000000, 20.70535890316561023, 1.956823837851916714 ) ) ;
#9443 = ORIENTED_EDGE ( 'NONE', *, *, #52987, .T. ) ;
#9444 = EDGE_CURVE ( 'NONE', #10446, #109601, #53269, .T. ) ;
#9445 = CARTESIAN_POINT ( 'NONE',  ( -0.9818841892814907935, 12.58817548488941540, -26.73591915876452774 ) ) ;
#9446 = DIRECTION ( 'NONE',  ( 0.6830127018922180770, -0.6830127018922204085, -0.2588190451025213501 ) ) ;
#9447 = VECTOR ( 'NONE', #107720, 1000.000000000000000 ) ;
#9448 = CARTESIAN_POINT ( 'NONE',  ( -18.18398860626898994, 28.73617430169800002, 5.000000000000000000 ) ) ;
#9449 = CARTESIAN_POINT ( 'NONE',  ( 23.91666666666666785, 5.278424836066147208, 3.047499999999990550 ) ) ;
#9450 = CARTESIAN_POINT ( 'NONE',  ( 1.031902578047557473, -0.5999999999999992006, -4.508672757499343042 ) ) ;
#9451 = CARTESIAN_POINT ( 'NONE',  ( 30.99586038379621655, -3.974999999999998312, -6.884901960086286188 ) ) ;
#9452 = EDGE_CURVE ( 'NONE', #66483, #118907, #119933, .T. ) ;
#9453 = LINE ( 'NONE', #87057, #23576 ) ;
#9454 = VERTEX_POINT ( 'NONE', #77215 ) ;
#9455 = ORIENTED_EDGE ( 'NONE', *, *, #10680, .F. ) ;
#9456 = CARTESIAN_POINT ( 'NONE',  ( 30.75000000000000000, -9.735942053221458872E-16, 7.950000000000000178 ) ) ;
#9457 = EDGE_LOOP ( 'NONE', ( #130653, #98634, #123307, #56251 ) ) ;
#9458 = VECTOR ( 'NONE', #42900, 999.9999999999998863 ) ;
#9459 = CARTESIAN_POINT ( 'NONE',  ( 5.816011393731002066, 28.73617430169783304, 5.000000000000000000 ) ) ;
#9460 = AXIS2_PLACEMENT_3D ( 'NONE', #101983, #47649, #58541 ) ;
#9461 = CYLINDRICAL_SURFACE ( 'NONE', #57184, 0.5000000000000004441 ) ;
#9462 = EDGE_CURVE ( 'NONE', #139894, #135322, #130152, .T. ) ;
#9463 = PLANE ( 'NONE',  #124369 ) ;
#9464 = DIRECTION ( 'NONE',  ( -0.5735764363510503783, -0.8191520442889886899, 0.000000000000000000 ) ) ;
#9465 = DIRECTION ( 'NONE',  ( 0.7071067811865487940, 0.7071067811865463515, -0.000000000000000000 ) ) ;
#9466 = DIRECTION ( 'NONE',  ( -0.7071067811865486830, -0.7071067811865464625, 0.000000000000000000 ) ) ;
#9467 = AXIS2_PLACEMENT_3D ( 'NONE', #64097, #60009, #104172 ) ;
#9468 = VECTOR ( 'NONE', #96304, 1000.000000000000000 ) ;
#9469 = CARTESIAN_POINT ( 'NONE',  ( 121.8287635252314516, 0.000000000000000000, -6.109999999999998543 ) ) ;
#9470 = ORIENTED_EDGE ( 'NONE', *, *, #91636, .T. ) ;
#9471 = VECTOR ( 'NONE', #44749, 1000.000000000000000 ) ;
#9472 = ORIENTED_EDGE ( 'NONE', *, *, #27720, .F. ) ;
#9473 = EDGE_CURVE ( 'NONE', #108316, #104393, #76491, .T. ) ;
#9474 = FACE_OUTER_BOUND ( 'NONE', #118525, .T. ) ;
#9475 = AXIS2_PLACEMENT_3D ( 'NONE', #55295, #45159, #121937 ) ;
#9476 = CARTESIAN_POINT ( 'NONE',  ( -12.79289321881336150, 0.7592924766157052030, 5.000000000000000000 ) ) ;
#9477 = CARTESIAN_POINT ( 'NONE',  ( 2.994519915287485734, 28.92564299267940342, 4.000000000000000000 ) ) ;
#9478 = LINE ( 'NONE', #20364, #139071 ) ;
#9479 = ORIENTED_EDGE ( 'NONE', *, *, #20367, .T. ) ;
#9480 = CARTESIAN_POINT ( 'NONE',  ( 45.35459685856476852, -1.637169565754161615, 6.110000000000000320 ) ) ;
#9481 = ORIENTED_EDGE ( 'NONE', *, *, #125888, .F. ) ;
#9482 = AXIS2_PLACEMENT_3D ( 'NONE', #78294, #90597, #89857 ) ;
#9483 = CARTESIAN_POINT ( 'NONE',  ( 33.29974487139158867, -27.71228299555229313, 4.000000000000000000 ) ) ;
#9484 = DIRECTION ( 'NONE',  ( -0.3543493200069163240, -0.000000000000000000, -0.9351131265310288487 ) ) ;
#9485 = CARTESIAN_POINT ( 'NONE',  ( 24.48921356237309510, -27.52281430457072631, 5.000000000000000000 ) ) ;
#9486 = EDGE_CURVE ( 'NONE', #63259, #71467, #107654, .T. ) ;
#9487 = ADVANCED_FACE ( 'NONE', ( #121387 ), #142454, .T. ) ;
#9488 = VECTOR ( 'NONE', #28079, 1000.000000000000227 ) ;
#9489 = CARTESIAN_POINT ( 'NONE',  ( 43.66209685856478728, -5.291415217122919401, 3.054999999999997939 ) ) ;
#9490 = ORIENTED_EDGE ( 'NONE', *, *, #130933, .T. ) ;
#9491 = DIRECTION ( 'NONE',  ( 0.7071067811865486830, -0.7071067811865464625, -0.000000000000000000 ) ) ;
#9492 = EDGE_LOOP ( 'NONE', ( #131528, #32597, #58872, #136148 ) ) ;
#9493 = ORIENTED_EDGE ( 'NONE', *, *, #81334, .T. ) ;
#9494 = CIRCLE ( 'NONE', #28058, 34.92999999999999261 ) ;
#9495 = EDGE_LOOP ( 'NONE', ( #115487, #33363, #508, #26146 ) ) ;
#9496 = AXIS2_PLACEMENT_3D ( 'NONE', #30299, #31034, #74542 ) ;
#9497 = CARTESIAN_POINT ( 'NONE',  ( 156.1500000000000057, -49.14999999999999147, -53.92499999999968452 ) ) ;
#9498 = ORIENTED_EDGE ( 'NONE', *, *, #25668, .F. ) ;
#9499 = CARTESIAN_POINT ( 'NONE',  ( -34.42500000000001137, 5.977185695429358958, 5.000000000000000000 ) ) ;
#9500 = ADVANCED_FACE ( 'NONE', ( #52563 ), #22755, .F. ) ;
#9501 = DIRECTION ( 'NONE',  ( -0.6830127018922181881, 0.6830127018922202975, -0.2588190451025214056 ) ) ;
#9502 = CIRCLE ( 'NONE', #81276, 2.500000000000000888 ) ;
#9503 = CARTESIAN_POINT ( 'NONE',  ( 16.49999999999989342, 16.46639925780208813, 5.000000000000000000 ) ) ;
#9504 = DIRECTION ( 'NONE',  ( -0.6830127018922180770, -0.6830127018922204085, -0.2588190451025213501 ) ) ;
#9505 = FACE_BOUND ( 'NONE', #45247, .T. ) ;
#9506 = EDGE_LOOP ( 'NONE', ( #34029, #127191, #118906, #25606 ) ) ;
#9507 = CARTESIAN_POINT ( 'NONE',  ( -1.499999999999989120, -13.91253812416061564, 4.000000000000000000 ) ) ;
#9508 = EDGE_CURVE ( 'NONE', #116772, #128234, #110493, .T. ) ;
#9509 = DIRECTION ( 'NONE',  ( -0.7071067811865486830, 0.7071067811865464625, 0.000000000000000000 ) ) ;
#9510 = CARTESIAN_POINT ( 'NONE',  ( 17.70025512860841488, -27.71228299555193786, 4.000000000000000000 ) ) ;
#9511 = ORIENTED_EDGE ( 'NONE', *, *, #29386, .F. ) ;
#9512 = FACE_OUTER_BOUND ( 'NONE', #24619, .T. ) ;
#9513 = ORIENTED_EDGE ( 'NONE', *, *, #116309, .T. ) ;
#9514 = VERTEX_POINT ( 'NONE', #109078 ) ;
#9515 = AXIS2_PLACEMENT_3D ( 'NONE', #40004, #107359, #96448 ) ;
#9516 = CARTESIAN_POINT ( 'NONE',  ( 19.05000000000000071, 3.174999999999997158, 0.000000000000000000 ) ) ;
#9517 =( BOUNDED_CURVE ( )  B_SPLINE_CURVE ( 3, ( #123115, #134719, #113635, #81770 ),
 .UNSPECIFIED., .F., .F. ) 
 B_SPLINE_CURVE_WITH_KNOTS ( ( 4, 4 ),
 ( 4.874499669516390910, 4.920172610314182293 ),
 .UNSPECIFIED. ) 
 CURVE ( )  GEOMETRIC_REPRESENTATION_ITEM ( )  RATIONAL_B_SPLINE_CURVE ( ( 1.000000000000000000, 0.9998261727610758820, 0.9998261727610758820, 1.000000000000000000 ) ) 
 REPRESENTATION_ITEM ( '' )  );
#9518 = ORIENTED_EDGE ( 'NONE', *, *, #72885, .T. ) ;
#9519 = CARTESIAN_POINT ( 'NONE',  ( 59.84959685856476597, 6.109999999999996767, 1.637169565754163836 ) ) ;
#9520 = EDGE_LOOP ( 'NONE', ( #84992, #119631, #79342, #10026 ) ) ;
#9521 = FACE_OUTER_BOUND ( 'NONE', #73903, .T. ) ;
#9522 = ORIENTED_EDGE ( 'NONE', *, *, #20555, .T. ) ;
#9523 = DIRECTION ( 'NONE',  ( -0.000000000000000000, 1.000000000000000000, -0.000000000000000000 ) ) ;
#9524 = ORIENTED_EDGE ( 'NONE', *, *, #13878, .F. ) ;
#9525 = EDGE_CURVE ( 'NONE', #89076, #84967, #9773, .T. ) ;
#9526 = LINE ( 'NONE', #63272, #132493 ) ;
#9527 = VECTOR ( 'NONE', #57402, 1000.000000000000000 ) ;
#9528 = VECTOR ( 'NONE', #84479, 1000.000000000000227 ) ;
#9529 = VECTOR ( 'NONE', #87462, 1000.000000000000000 ) ;
#9530 = CARTESIAN_POINT ( 'NONE',  ( -21.18398860626899349, 28.73617430169802134, 5.000000000000000000 ) ) ;
#9531 = CYLINDRICAL_SURFACE ( 'NONE', #29626, 2.999999999999999112 ) ;
#9532 = EDGE_CURVE ( 'NONE', #29201, #118149, #12381, .T. ) ;
#9533 = PLANE ( 'NONE',  #108476 ) ;
#9534 = DIRECTION ( 'NONE',  ( 0.6830127018922181881, 0.6830127018922202975, -0.2588190451025214056 ) ) ;
#9535 = DIRECTION ( 'NONE',  ( -0.7071067811865486830, -0.7071067811865464625, 0.000000000000000000 ) ) ;
#9536 = EDGE_LOOP ( 'NONE', ( #3452, #82198, #55651, #6315 ) ) ;
#9537 = VECTOR ( 'NONE', #139264, 999.9999999999998863 ) ;
#9538 = VECTOR ( 'NONE', #128237, 1000.000000000000000 ) ;
#9539 = ORIENTED_EDGE ( 'NONE', *, *, #71326, .F. ) ;
#9540 = VECTOR ( 'NONE', #15816, 1000.000000000000000 ) ;
#9541 = VERTEX_POINT ( 'NONE', #48136 ) ;
#9542 = CARTESIAN_POINT ( 'NONE',  ( -13.49999999999990052, -19.91253812416055524, 4.000000000000000000 ) ) ;
#9543 = DIRECTION ( 'NONE',  ( 0.7071067811865486830, -0.7071067811865464625, -0.000000000000000000 ) ) ;
#9544 = ORIENTED_EDGE ( 'NONE', *, *, #39977, .T. ) ;
#9545 = VECTOR ( 'NONE', #831, 999.9999999999998863 ) ;
#9546 = ORIENTED_EDGE ( 'NONE', *, *, #141244, .F. ) ;
#9547 = LINE ( 'NONE', #8119, #99947 ) ;
#9548 = CARTESIAN_POINT ( 'NONE',  ( -12.69999999999998153, 0.4000000000000001887, -2.467792535850613866 ) ) ;
#9549 = EDGE_CURVE ( 'NONE', #17021, #49295, #136544, .T. ) ;
#9550 = EDGE_CURVE ( 'NONE', #106128, #44075, #79376, .T. ) ;
#9551 = DIRECTION ( 'NONE',  ( 0.7071067811865486830, -0.7071067811865464625, -0.000000000000000000 ) ) ;
#9552 = ORIENTED_EDGE ( 'NONE', *, *, #9175, .T. ) ;
#9553 = VECTOR ( 'NONE', #140886, 1000.000000000000227 ) ;
#9554 = CARTESIAN_POINT ( 'NONE',  ( 7.828169399223474656, -20.24070752338407431, 4.000000000000000000 ) ) ;
#9555 = LINE ( 'NONE', #10282, #102305 ) ;
#9556 = CARTESIAN_POINT ( 'NONE',  ( 17.71290314143521982, 3.967499999999992699, -6.871911579029513994 ) ) ;
#9557 = LINE ( 'NONE', #53830, #141043 ) ;
#9558 = ORIENTED_EDGE ( 'NONE', *, *, #63356, .T. ) ;
#9559 = CARTESIAN_POINT ( 'NONE',  ( 120.2245968585648086, -1.637169565754161171, 6.109999999999998543 ) ) ;
#9560 = EDGE_CURVE ( 'NONE', #6090, #23067, #112662, .T. ) ;
#9561 = COLOUR_RGB ( '', 0.09019608, 0.27058824, 0.51372549) ;
#9562 = DIRECTION ( 'NONE',  ( -0.3543493200069163240, -0.000000000000000000, 0.9351131265310288487 ) ) ;
#9563 = CARTESIAN_POINT ( 'NONE',  ( -3.183988606268992161, 28.73617430169789699, 5.000000000000000000 ) ) ;
#9565 = ORIENTED_EDGE ( 'NONE', *, *, #74113, .F. ) ;
#9564 = CARTESIAN_POINT ( 'NONE',  ( -69.18398860626899705, 28.73617430169835529, 5.000000000000000000 ) ) ;
#9566 = CARTESIAN_POINT ( 'NONE',  ( 1.827855086967997478, 2.055000000000001048, 2.516649172247811554E-16 ) ) ;
#9567 = EDGE_LOOP ( 'NONE', ( #80120, #35216, #91779, #80750 ) ) ;
#9568 = DIRECTION ( 'NONE',  ( -1.000000000000000000, 0.000000000000000000, 0.000000000000000000 ) ) ;
#9569 = CARTESIAN_POINT ( 'NONE',  ( 0.000000000000000000, 0.000000000000000000, 5.000000000000000000 ) ) ;
#9570 = FACE_OUTER_BOUND ( 'NONE', #135441, .T. ) ;
#9571 = EDGE_CURVE ( 'NONE', #65516, #65242, #122829, .T. ) ;
#9572 = EDGE_LOOP ( 'NONE', ( #99934, #105720, #135150, #75962 ) ) ;
#9573 = PRESENTATION_LAYER_ASSIGNMENT (  '', '', ( #67586 ) ) ;
#9574 = VECTOR ( 'NONE', #77318, 1000.000000000000227 ) ;
#9575 = VECTOR ( 'NONE', #53821, 1000.000000000000000 ) ;
#9576 = DIRECTION ( 'NONE',  ( 0.7071067811865487940, -0.7071067811865463515, 0.000000000000000000 ) ) ;
#9577 = CARTESIAN_POINT ( 'NONE',  ( 18.32840764549667512, 2.499999999999998224, 3.061616997868380183E-16 ) ) ;
#9578 = ORIENTED_EDGE ( 'NONE', *, *, #13778, .T. ) ;
#9579 = EDGE_CURVE ( 'NONE', #40143, #133726, #92316, .T. ) ;
#9580 = FACE_OUTER_BOUND ( 'NONE', #28645, .T. ) ;
#9581 = VECTOR ( 'NONE', #81723, 1000.000000000000000 ) ;
#9582 = CARTESIAN_POINT ( 'NONE',  ( -3.792893218813429446, 18.75929247661552779, 5.000000000000000000 ) ) ;
#9583 = VERTEX_POINT ( 'NONE', #124963 ) ;
#9584 = DIRECTION ( 'NONE',  ( -0.3543493200069162685, -0.000000000000000000, -0.9351131265310288487 ) ) ;
#9585 = CARTESIAN_POINT ( 'NONE',  ( 6.299744871391586898, -27.71228299555210484, 4.000000000000000000 ) ) ;
#9586 = ORIENTED_EDGE ( 'NONE', *, *, #55998, .T. ) ;
#9587 = AXIS2_PLACEMENT_3D ( 'NONE', #35705, #92163, #103065 ) ;
#9588 = VERTEX_POINT ( 'NONE', #80770 ) ;
#9589 = CARTESIAN_POINT ( 'NONE',  ( 3.489213562373097322, -27.52281430457057709, 5.000000000000000000 ) ) ;
#9590 = DIRECTION ( 'NONE',  ( 0.6830127018922180770, -0.6830127018922204085, -0.2588190451025213501 ) ) ;
#9591 = DIRECTION ( 'NONE',  ( -0.000000000000000000, 0.3543493200069153248, 0.9351131265310292928 ) ) ;
#9592 = FACE_OUTER_BOUND ( 'NONE', #117514, .T. ) ;
#9593 = ORIENTED_EDGE ( 'NONE', *, *, #34526, .T. ) ;
#9594 = EDGE_CURVE ( 'NONE', #126646, #20150, #11904, .T. ) ;
#9595 = CARTESIAN_POINT ( 'NONE',  ( 19.05000000000000071, 3.174999999999997158, 5.000000000000000000 ) ) ;
#9596 = LINE ( 'NONE', #53872, #113831 ) ;
#9597 = VECTOR ( 'NONE', #131284, 1000.000000000000227 ) ;
#9598 = FACE_OUTER_BOUND ( 'NONE', #28762, .T. ) ;
#9599 = VECTOR ( 'NONE', #114633, 1000.000000000000000 ) ;
#9600 = CARTESIAN_POINT ( 'NONE',  ( 42.18398860626899705, 28.73617430169816700, 5.000000000000000000 ) ) ;
#9601 = CARTESIAN_POINT ( 'NONE',  ( 40.59959685856476597, -6.109999999999998543, -1.637169565754160727 ) ) ;
#9602 = PLANE ( 'NONE',  #141338 ) ;
#9603 = EDGE_CURVE ( 'NONE', #114032, #121130, #100374, .T. ) ;
#9604 = EDGE_CURVE ( 'NONE', #114250, #5707, #67783, .T. ) ;
#9605 = ORIENTED_EDGE ( 'NONE', *, *, #18051, .T. ) ;
#9606 = VERTEX_POINT ( 'NONE', #90190 ) ;
#9607 = DIRECTION ( 'NONE',  ( 0.7071067811865487940, -0.7071067811865463515, 0.000000000000000000 ) ) ;
#9608 = ORIENTED_EDGE ( 'NONE', *, *, #21387, .F. ) ;
#9609 = ORIENTED_EDGE ( 'NONE', *, *, #15540, .T. ) ;
#9610 = VECTOR ( 'NONE', #92866, 1000.000000000000000 ) ;
#9611 = DIRECTION ( 'NONE',  ( -1.000000000000000000, -1.224606353822377258E-16, -0.000000000000000000 ) ) ;
#9612 = CARTESIAN_POINT ( 'NONE',  ( -34.92500000000001137, 22.22500000000000142, 4.000000000000000000 ) ) ;
#9613 = EDGE_CURVE ( 'NONE', #94686, #1885, #139717, .T. ) ;
#9614 = ORIENTED_EDGE ( 'NONE', *, *, #139692, .T. ) ;
#9615 = DIRECTION ( 'NONE',  ( -0.000000000000000000, 0.2631995976047526442, 0.9647414015272156584 ) ) ;
#9616 = CARTESIAN_POINT ( 'NONE',  ( 30.18398860626900060, 28.73617430169808173, 5.000000000000000000 ) ) ;
#9617 = FACE_OUTER_BOUND ( 'NONE', #119504, .T. ) ;
#9618 = EDGE_CURVE ( 'NONE', #102027, #57345, #91629, .T. ) ;
#9619 = FACE_OUTER_BOUND ( 'NONE', #45078, .T. ) ;
#9620 = DIRECTION ( 'NONE',  ( 0.6830127018922180770, -0.6830127018922204085, -0.2588190451025213501 ) ) ;
#9621 = ORIENTED_EDGE ( 'NONE', *, *, #117477, .F. ) ;
#9622 = EDGE_CURVE ( 'NONE', #139467, #70462, #14777, .T. ) ;
#9623 = CARTESIAN_POINT ( 'NONE',  ( 30.61838490601977725, -2.240707523384260824, 13.37739548510232268 ) ) ;
#9624 = DIRECTION ( 'NONE',  ( 0.7071067811865487940, 0.7071067811865463515, -0.000000000000000000 ) ) ;
#9626 = AXIS2_PLACEMENT_3D ( 'NONE', #30512, #75444, #121066 ) ;
#9625 = CARTESIAN_POINT ( 'NONE',  ( 79.16666666666665719, 6.884901960086285300, 3.975000000000003642 ) ) ;
#9627 = CARTESIAN_POINT ( 'NONE',  ( -10.49999999999992184, 16.46639925780209524, 5.000000000000000000 ) ) ;
#9628 = DIRECTION ( 'NONE',  ( -0.000000000000000000, 0.000000000000000000, 1.000000000000000000 ) ) ;
#9629 = CARTESIAN_POINT ( 'NONE',  ( 5.281315875828549444, 2.500000000000000888, 0.000000000000000000 ) ) ;
#9630 = LINE ( 'NONE', #11771, #117574 ) ;
#9631 = CARTESIAN_POINT ( 'NONE',  ( 57.53752705046289151, -9.735942053221456900E-16, 7.949999999999998401 ) ) ;
#9632 = EDGE_CURVE ( 'NONE', #25081, #14507, #69922, .T. ) ;
#9633 = CARTESIAN_POINT ( 'NONE',  ( -9.489213562373095101, -27.52281430457062328, 5.000000000000000000 ) ) ;
#9634 = EDGE_LOOP ( 'NONE', ( #92215, #32995, #139085, #62177 ) ) ;
#9635 = ORIENTED_EDGE ( 'NONE', *, *, #79584, .T. ) ;
#9636 = CARTESIAN_POINT ( 'NONE',  ( 58.45833333333333570, 3.974999999999997424, 6.884901960086288852 ) ) ;
#9637 = ADVANCED_FACE ( 'NONE', ( #46756 ), #36532, .T. ) ;
#9638 = CARTESIAN_POINT ( 'NONE',  ( 21.79614956108759216, 8.475608720613170277, 4.664130618528504080 ) ) ;
#9639 = FACE_OUTER_BOUND ( 'NONE', #140004, .T. ) ;
#9640 = CARTESIAN_POINT ( 'NONE',  ( -54.48921356237310221, -27.52281430457093236, 5.000000000000000000 ) ) ;
#9641 = VERTEX_POINT ( 'NONE', #3852 ) ;
#9643 = EDGE_CURVE ( 'NONE', #95326, #25399, #101058, .T. ) ;
#9642 = CIRCLE ( 'NONE', #53662, 1.500000000000000000 ) ;
#9644 = VECTOR ( 'NONE', #75393, 1000.000000000000227 ) ;
#9645 = DIRECTION ( 'NONE',  ( -0.000000000000000000, 0.3543493200069153248, 0.9351131265310292928 ) ) ;
#9646 = DIRECTION ( 'NONE',  ( 1.000000000000000000, 0.000000000000000000, 0.000000000000000000 ) ) ;
#9647 = AXIS2_PLACEMENT_3D ( 'NONE', #125297, #25987, #50590 ) ;
#9648 = AXIS2_PLACEMENT_3D ( 'NONE', #51640, #95834, #29152 ) ;
#9649 = CARTESIAN_POINT ( 'NONE',  ( 48.85459685856476142, -1.637169565754161615, 6.110000000000000320 ) ) ;
#9650 = ORIENTED_EDGE ( 'NONE', *, *, #68813, .F. ) ;
#9651 = ORIENTED_EDGE ( 'NONE', *, *, #95559, .F. ) ;
#9653 = ORIENTED_EDGE ( 'NONE', *, *, #138983, .T. ) ;
#9652 = VECTOR ( 'NONE', #10656, 1000.000000000000000 ) ;
#9654 = VECTOR ( 'NONE', #11392, 1000.000000000000000 ) ;
#9655 = EDGE_CURVE ( 'NONE', #94256, #112217, #1714, .T. ) ;
#9656 = CONICAL_SURFACE ( 'NONE', #93087, 2.500000000000000444, 0.9599310885968830309 ) ;
#9657 = AXIS2_PLACEMENT_3D ( 'NONE', #32350, #85275, #143244 ) ;
#9658 = DIRECTION ( 'NONE',  ( 0.6830127018922181881, 0.6830127018922202975, -0.2588190451025214056 ) ) ;
#9659 = VECTOR ( 'NONE', #140023, 1000.000000000000000 ) ;
#9661 = DIRECTION ( 'NONE',  ( -0.3543493200069162685, -0.000000000000000000, -0.9351131265310288487 ) ) ;
#9660 = AXIS2_PLACEMENT_3D ( 'NONE', #97862, #8654, #9376 ) ;
#9662 = CARTESIAN_POINT ( 'NONE',  ( 26.90840764549667696, 3.061616997868380183E-16, -2.500000000000001332 ) ) ;
#9663 = CARTESIAN_POINT ( 'NONE',  ( -2.999999999999971578, 10.55218569542906337, 5.000000000000000000 ) ) ;
#9664 = EDGE_LOOP ( 'NONE', ( #141310, #4968, #33670 ) ) ;
#9665 = DIRECTION ( 'NONE',  ( 0.7071067811865486830, -0.7071067811865464625, -0.000000000000000000 ) ) ;
#9667 = ORIENTED_EDGE ( 'NONE', *, *, #134730, .F. ) ;
#9666 = CARTESIAN_POINT ( 'NONE',  ( 9.233306282870437087, -6.094999999999989981, -1.633150327867689322 ) ) ;
#9668 = CARTESIAN_POINT ( 'NONE',  ( 81.81293019189810423, -1.637169565754159617, -6.110000000000001208 ) ) ;
#9669 = CARTESIAN_POINT ( 'NONE',  ( -9.489213562373095101, -27.52281430457062328, 5.000000000000000000 ) ) ;
#9670 = DIRECTION ( 'NONE',  ( -0.000000000000000000, -0.3543493200069152693, 0.9351131265310292928 ) ) ;
#9671 = LINE ( 'NONE', #43052, #65451 ) ;
#9672 = PRESENTATION_LAYER_ASSIGNMENT (  '', '', ( #28219 ) ) ;
#9673 = EDGE_CURVE ( 'NONE', #121898, #69514, #133715, .T. ) ;
#9674 = CARTESIAN_POINT ( 'NONE',  ( -20.99451991528748707, 28.92564299267952777, 4.000000000000000000 ) ) ;
#9675 = CARTESIAN_POINT ( 'NONE',  ( 25.17183060077630330, -14.24070752338413293, 4.000000000000000000 ) ) ;
#9676 = EDGE_CURVE ( 'NONE', #112076, #63804, #111213, .T. ) ;
#9677 = ORIENTED_EDGE ( 'NONE', *, *, #105221, .F. ) ;
#9678 = CARTESIAN_POINT ( 'NONE',  ( 14.70692117890024697, 4.584330080086930965E-16, 0.000000000000000000 ) ) ;
#9679 = CARTESIAN_POINT ( 'NONE',  ( 63.64126352523144448, 4.472830434245836706, 4.472830434245840259 ) ) ;
#9680 = FACE_OUTER_BOUND ( 'NONE', #24240, .T. ) ;
#9681 = DIRECTION ( 'NONE',  ( 0.7071067811865487940, 0.7071067811865463515, -0.000000000000000000 ) ) ;
#9682 = FACE_OUTER_BOUND ( 'NONE', #16125, .T. ) ;
#9683 = ORIENTED_EDGE ( 'NONE', *, *, #106663, .T. ) ;
#9684 = EDGE_LOOP ( 'NONE', ( #87362, #82904, #35603, #37501, #124588 ) ) ;
#9685 = CARTESIAN_POINT ( 'NONE',  ( 3.489213562373097322, -27.52281430457057709, 5.000000000000000000 ) ) ;
#9687 = EDGE_CURVE ( 'NONE', #140721, #129923, #56895, .T. ) ;
#9686 = FACE_OUTER_BOUND ( 'NONE', #9810, .T. ) ;
#9688 = ORIENTED_EDGE ( 'NONE', *, *, #71799, .T. ) ;
#9689 = VECTOR ( 'NONE', #67157, 1000.000000000000114 ) ;
#9690 = ORIENTED_EDGE ( 'NONE', *, *, #61925, .F. ) ;
#9691 = AXIS2_PLACEMENT_3D ( 'NONE', #214, #44519, #88719 ) ;
#9692 = DIRECTION ( 'NONE',  ( -0.7071067811865486830, 0.7071067811865464625, 0.000000000000000000 ) ) ;
#9693 = ORIENTED_EDGE ( 'NONE', *, *, #71235, .T. ) ;
#9694 = VECTOR ( 'NONE', #108675, 1000.000000000000000 ) ;
#9695 = CARTESIAN_POINT ( 'NONE',  ( 24.18398860626899705, 28.73617430169804265, 5.000000000000000000 ) ) ;
#9696 = CARTESIAN_POINT ( 'NONE',  ( -42.18398860626899705, 28.73617430169816700, 5.000000000000000000 ) ) ;
#9697 = VECTOR ( 'NONE', #123456, 1000.000000000000000 ) ;
#9698 = CARTESIAN_POINT ( 'NONE',  ( 12.04658813629536773, 14.25929247661557042, 18.84478104361324924 ) ) ;
#9699 = FACE_BOUND ( 'NONE', #92046, .T. ) ;
#9700 = DIRECTION ( 'NONE',  ( -1.000000000000000000, -1.224606353822377258E-16, -0.000000000000000000 ) ) ;
#9701 = DIRECTION ( 'NONE',  ( 0.6830127018922180770, -0.6830127018922204085, -0.2588190451025213501 ) ) ;
#9702 = CARTESIAN_POINT ( 'NONE',  ( -14.99999999999988809, -8.151047557385080466, -8.977947279169763206 ) ) ;
#9704 = ORIENTED_EDGE ( 'NONE', *, *, #102063, .T. ) ;
#9703 = PLANE ( 'NONE',  #59798 ) ;
#9705 = VECTOR ( 'NONE', #140945, 1000.000000000000000 ) ;
#9706 = CARTESIAN_POINT ( 'NONE',  ( 14.99451991528749595, 28.92564299267948513, 4.000000000000000000 ) ) ;
#9707 = VERTEX_POINT ( 'NONE', #68481 ) ;
#9708 = ORIENTED_EDGE ( 'NONE', *, *, #138313, .T. ) ;
#9709 = CARTESIAN_POINT ( 'NONE',  ( 80.55793019189810877, 6.110000000000000320, -1.637169565754156064 ) ) ;
#9710 = EDGE_LOOP ( 'NONE', ( #127931, #33466, #59497, #55446 ) ) ;
#9711 = CARTESIAN_POINT ( 'NONE',  ( 0.000000000000000000, 0.000000000000000000, 5.000000000000000000 ) ) ;
#9712 = CARTESIAN_POINT ( 'NONE',  ( 17.07999999999999829, 2.055000000000001492, 0.000000000000000000 ) ) ;
#9713 = ADVANCED_FACE ( 'NONE', ( #101784 ), #85023, .F. ) ;
#9714 = ORIENTED_EDGE ( 'NONE', *, *, #133090, .T. ) ;
#9715 = DIRECTION ( 'NONE',  ( 0.7071067811865487940, 0.7071067811865463515, 0.000000000000000000 ) ) ;
#9716 = CIRCLE ( 'NONE', #63059, 2.500000000000000444 ) ;
#9717 = PLANE ( 'NONE',  #42553 ) ;
#9718 = CARTESIAN_POINT ( 'NONE',  ( 0.000000000000000000, 0.000000000000000000, 5.000000000000000000 ) ) ;
#9719 = DIRECTION ( 'NONE',  ( 0.000000000000000000, -1.734723475976807686E-15, 1.000000000000000000 ) ) ;
#9720 = DIRECTION ( 'NONE',  ( -0.000000000000000000, 0.3543493200069153248, 0.9351131265310292928 ) ) ;
#9721 = FACE_OUTER_BOUND ( 'NONE', #9884, .T. ) ;
#9722 = DIRECTION ( 'NONE',  ( 0.000000000000000000, -1.000000000000000000, 0.000000000000000000 ) ) ;
#9723 = ORIENTED_EDGE ( 'NONE', *, *, #39513, .T. ) ;
#9724 = VECTOR ( 'NONE', #37976, 1000.000000000000000 ) ;
#9725 = LINE ( 'NONE', #43105, #14464 ) ;
#9726 = ORIENTED_EDGE ( 'NONE', *, *, #53000, .T. ) ;
#9727 = LINE ( 'NONE', #54000, #61169 ) ;
#9728 = CARTESIAN_POINT ( 'NONE',  ( 24.48921356237309510, -27.52281430457072631, 5.000000000000000000 ) ) ;
#9729 = EDGE_CURVE ( 'NONE', #98816, #96665, #140146, .T. ) ;
#9730 = EDGE_LOOP ( 'NONE', ( #9094, #136529, #100923, #31263, #98684 ) ) ;
#9731 = VERTEX_POINT ( 'NONE', #137997 ) ;
#9732 = ADVANCED_FACE ( 'NONE', ( #137288 ), #5305, .F. ) ;
#9733 = ORIENTED_EDGE ( 'NONE', *, *, #35243, .T. ) ;
#9734 = CARTESIAN_POINT ( 'NONE',  ( 36.75043019189811133, 3.055000000000002824, -5.291415217122919401 ) ) ;
#9735 = ORIENTED_EDGE ( 'NONE', *, *, #66766, .F. ) ;
#9736 = LINE ( 'NONE', #27375, #57485 ) ;
#9737 = EDGE_CURVE ( 'NONE', #129536, #76705, #29980, .T. ) ;
#9738 = ADVANCED_FACE ( 'NONE', ( #82909 ), #37981, .T. ) ;
#9739 = CARTESIAN_POINT ( 'NONE',  ( 89.47502705046288440, -5.819803920172573086, 5.819803920172573086 ) ) ;
#9740 = CARTESIAN_POINT ( 'NONE',  ( 26.73330628287044064, -6.094999999999989981, -1.633150327867689100 ) ) ;
#9741 = CARTESIAN_POINT ( 'NONE',  ( -3.453448961350486623, 12.25336827149928176, -25.50699926098112513 ) ) ;
#9742 = EDGE_LOOP ( 'NONE', ( #129045, #64031, #2471, #14722 ) ) ;
#9743 = EDGE_CURVE ( 'NONE', #46696, #40966, #127095, .T. ) ;
#9744 = FACE_OUTER_BOUND ( 'NONE', #42705, .T. ) ;
#9745 = ORIENTED_EDGE ( 'NONE', *, *, #129908, .F. ) ;
#9746 = DIRECTION ( 'NONE',  ( 0.6830127018922180770, -0.6830127018922204085, -0.2588190451025213501 ) ) ;
#9747 = VECTOR ( 'NONE', #73469, 1000.000000000000000 ) ;
#9748 = AXIS2_PLACEMENT_3D ( 'NONE', #112996, #34749, #15099 ) ;
#9750 = ORIENTED_EDGE ( 'NONE', *, *, #10040, .F. ) ;
#9749 = DIRECTION ( 'NONE',  ( -0.7071067811865487940, 0.7071067811865463515, -0.000000000000000000 ) ) ;
#9751 = AXIS2_PLACEMENT_3D ( 'NONE', #110936, #78351, #121821 ) ;
#9752 = VERTEX_POINT ( 'NONE', #27795 ) ;
#9753 = DIRECTION ( 'NONE',  ( -0.7071067811865487940, 0.7071067811865463515, -0.000000000000000000 ) ) ;
#9754 = SHAPE_REPRESENTATION ( '1.6 Slide Key', ( #127880 ), #121007 ) ;
#9755 = LINE ( 'NONE', #42429, #49223 ) ;
#9756 = AXIS2_PLACEMENT_3D ( 'NONE', #22554, #77702, #66816 ) ;
#9757 = CARTESIAN_POINT ( 'NONE',  ( -22.49999999999984013, 9.052185695429074030, 5.000000000000000000 ) ) ;
#9758 = EDGE_CURVE ( 'NONE', #33217, #100010, #138718, .T. ) ;
#9760 = ORIENTED_EDGE ( 'NONE', *, *, #60978, .T. ) ;
#9759 = VECTOR ( 'NONE', #24527, 999.9999999999998863 ) ;
#9761 = CARTESIAN_POINT ( 'NONE',  ( 108.2875270504628986, 0.000000000000000000, -7.949999999999998401 ) ) ;
#9762 = ORIENTED_EDGE ( 'NONE', *, *, #41366, .F. ) ;
#9763 = ORIENTED_EDGE ( 'NONE', *, *, #88313, .T. ) ;
#9764 = VERTEX_POINT ( 'NONE', #72060 ) ;
#9765 = CARTESIAN_POINT ( 'NONE',  ( -34.49999999999976552, 18.43112307739199451, 4.000000000000000000 ) ) ;
#9766 = DIRECTION ( 'NONE',  ( 1.000000000000000000, 0.000000000000000000, 0.000000000000000000 ) ) ;
#9767 = VECTOR ( 'NONE', #114992, 1000.000000000000000 ) ;
#9768 = VECTOR ( 'NONE', #127888, 1000.000000000000000 ) ;
#9769 = AXIS2_PLACEMENT_3D ( 'NONE', #114862, #137378, #38069 ) ;
#9770 = ADVANCED_FACE ( 'NONE', ( #61197 ), #40821, .F. ) ;
#9771 = DIRECTION ( 'NONE',  ( -0.000000000000000000, -0.000000000000000000, 1.000000000000000000 ) ) ;
#9772 = CARTESIAN_POINT ( 'NONE',  ( -3.707106781186508826, -15.74070752338412049, 5.000000000000000000 ) ) ;
#9773 = LINE ( 'NONE', #88794, #65938 ) ;
#9774 = DIRECTION ( 'NONE',  ( 0.6830127018922181881, 0.6830127018922202975, -0.2588190451025214056 ) ) ;
#9775 = VERTEX_POINT ( 'NONE', #70634 ) ;
#9776 = CARTESIAN_POINT ( 'NONE',  ( 96.91252705046289861, -7.949999999999998401, -4.867971026610728450E-16 ) ) ;
#9777 = VERTEX_POINT ( 'NONE', #103900 ) ;
#9778 = EDGE_CURVE ( 'NONE', #27605, #111099, #7444, .T. ) ;
#9779 = CARTESIAN_POINT ( 'NONE',  ( -28.41009064519814942, 9.759292476615618384, 11.28811694763772344 ) ) ;
#9780 = CARTESIAN_POINT ( 'NONE',  ( -15.32816939922341959, -12.74070752338415247, 4.000000000000000000 ) ) ;
#9781 = ORIENTED_EDGE ( 'NONE', *, *, #48078, .F. ) ;
#9782 = CARTESIAN_POINT ( 'NONE',  ( 14.67183060077636370, -18.74070752338408852, 4.000000000000000000 ) ) ;
#9783 = CARTESIAN_POINT ( 'NONE',  ( 0.4733609636421477473, -5.240707523384232402, 16.25846745537495863 ) ) ;
#9784 = ORIENTED_EDGE ( 'NONE', *, *, #25315, .T. ) ;
#9785 = ORIENTED_EDGE ( 'NONE', *, *, #41397, .T. ) ;
#9786 = EDGE_CURVE ( 'NONE', #106369, #103352, #59738, .T. ) ;
#9787 = CARTESIAN_POINT ( 'NONE',  ( -4.828169399223491531, 9.759292476615618384, 4.000000000000000000 ) ) ;
#9788 = LINE ( 'NONE', #120677, #32674 ) ;
#9789 = CARTESIAN_POINT ( 'NONE',  ( -32.29289321881322650, 14.25929247661557042, 5.000000000000000000 ) ) ;
#9790 = CARTESIAN_POINT ( 'NONE',  ( -34.75611968250419892, -21.18706574529240783, 4.955485411084905145 ) ) ;
#9791 = CARTESIAN_POINT ( 'NONE',  ( 66.70376352523143737, 6.109999999999999432, 1.122388791418549108E-15 ) ) ;
#9792 = VECTOR ( 'NONE', #108298, 1000.000000000000000 ) ;
#9793 = LINE ( 'NONE', #96764, #90433 ) ;
#9794 = ADVANCED_FACE ( 'NONE', ( #27073 ), #50276, .T. ) ;
#9795 = EDGE_CURVE ( 'NONE', #17066, #104226, #117621, .T. ) ;
#9796 = SURFACE_SIDE_STYLE ('',( #97512 ) ) ;
#9797 = DIRECTION ( 'NONE',  ( -0.7071067811865487940, 0.7071067811865463515, -0.000000000000000000 ) ) ;
#9798 = DIRECTION ( 'NONE',  ( 1.000000000000000000, 0.000000000000000000, 0.000000000000000000 ) ) ;
#9799 = VECTOR ( 'NONE', #42609, 999.9999999999998863 ) ;
#9800 = EDGE_LOOP ( 'NONE', ( #81298, #61337, #51087, #4171 ) ) ;
#9801 = DIRECTION ( 'NONE',  ( 0.000000000000000000, 0.000000000000000000, -1.000000000000000000 ) ) ;
#9802 = EDGE_LOOP ( 'NONE', ( #71288, #6805, #110044, #32127 ) ) ;
#9803 = CARTESIAN_POINT ( 'NONE',  ( -26.99999999999980815, -15.41253812416059432, 4.000000000000000000 ) ) ;
#9805 = CIRCLE ( 'NONE', #77006, 2.500000000000000888 ) ;
#9804 = SURFACE_SIDE_STYLE ('',( #107686 ) ) ;
#9806 = ORIENTED_EDGE ( 'NONE', *, *, #77823, .T. ) ;
#9807 = EDGE_CURVE ( 'NONE', #44162, #79780, #115475, .T. ) ;
#9808 = FACE_OUTER_BOUND ( 'NONE', #27780, .T. ) ;
#9810 = EDGE_LOOP ( 'NONE', ( #88364, #3939, #102750, #23216 ) ) ;
#9809 = CARTESIAN_POINT ( 'NONE',  ( 21.48921356237309155, -27.52281430457070499, 5.000000000000000000 ) ) ;
#9811 = DIRECTION ( 'NONE',  ( 0.6830127018922180770, -0.6830127018922204085, -0.2588190451025213501 ) ) ;
#9812 = ADVANCED_FACE ( 'NONE', ( #94466 ), #39406, .F. ) ;
#9813 = DIRECTION ( 'NONE',  ( 0.7071067811865487940, -0.7071067811865463515, 0.000000000000000000 ) ) ;
#9814 = CARTESIAN_POINT ( 'NONE',  ( -39.48921356237310221, -27.52281430457082934, 5.000000000000000000 ) ) ;
#9815 = VERTEX_POINT ( 'NONE', #17609 ) ;
#9816 = ORIENTED_EDGE ( 'NONE', *, *, #38312, .T. ) ;
#9817 = DIRECTION ( 'NONE',  ( -0.7071067811865486830, -0.7071067811865464625, -0.000000000000000000 ) ) ;
#9818 = CARTESIAN_POINT ( 'NONE',  ( -16.49999999999988276, -10.53360074219763121, 5.000000000000000000 ) ) ;
#9819 = LINE ( 'NONE', #134478, #100661 ) ;
#9820 = DIRECTION ( 'NONE',  ( -0.6830127018922181881, 0.6830127018922202975, -0.2588190451025214056 ) ) ;
#9821 = CARTESIAN_POINT ( 'NONE',  ( 87.72502705046291283, 5.819803920172573086, -5.819803920172572198 ) ) ;
#9822 = CARTESIAN_POINT ( 'NONE',  ( 11.29387692260795717, 22.22500000000000142, 4.000000000000000000 ) ) ;
#9823 = LINE ( 'NONE', #120719, #46070 ) ;
#9824 = ORIENTED_EDGE ( 'NONE', *, *, #140884, .F. ) ;
#9825 = CARTESIAN_POINT ( 'NONE',  ( 81.93749999999998579, 5.819803920172573974, -5.819803920172572198 ) ) ;
#9826 = EDGE_CURVE ( 'NONE', #49111, #97582, #128546, .T. ) ;
#9827 = DIRECTION ( 'NONE',  ( -0.7071067811865486830, -0.7071067811865464625, 0.000000000000000000 ) ) ;
#9828 = CARTESIAN_POINT ( 'NONE',  ( 24.78162688292477256, 21.74787736706806385, 4.999607392498049308 ) ) ;
#9830 = VECTOR ( 'NONE', #64262, 999.9999999999998863 ) ;
#9829 = CARTESIAN_POINT ( 'NONE',  ( 32.37500000000000000, -6.094999999999989981, 3.732111120401553285E-16 ) ) ;
#9831 = AXIS2_PLACEMENT_3D ( 'NONE', #72289, #49079, #104113 ) ;
#9832 = ORIENTED_EDGE ( 'NONE', *, *, #41753, .T. ) ;
#9833 = EDGE_CURVE ( 'NONE', #74099, #59626, #18308, .T. ) ;
#9834 = LINE ( 'NONE', #54794, #111608 ) ;
#9835 = ORIENTED_EDGE ( 'NONE', *, *, #58100, .F. ) ;
#9836 = CARTESIAN_POINT ( 'NONE',  ( 76.12543019189810423, 5.291415217122919401, 3.055000000000002824 ) ) ;
#9837 =( LENGTH_UNIT ( ) NAMED_UNIT ( * ) SI_UNIT ( .MILLI., .METRE. ) );
#9838 = DIRECTION ( 'NONE',  ( 0.7071067811865486830, -0.7071067811865464625, -0.000000000000000000 ) ) ;
#9839 = ORIENTED_EDGE ( 'NONE', *, *, #61997, .T. ) ;
#9840 = STYLED_ITEM ( 'NONE', ( #54637 ), #79516 ) ;
#9841 = CARTESIAN_POINT ( 'NONE',  ( -22.49999999999984723, 11.52377502935400955, -1.522421517564034543 ) ) ;
#9842 = DIRECTION ( 'NONE',  ( 0.7071067811865486830, -0.7071067811865464625, -0.000000000000000000 ) ) ;
#9843 = CARTESIAN_POINT ( 'NONE',  ( -32.67183060077623935, 2.259292476615694323, 4.000000000000000000 ) ) ;
#9844 = DIRECTION ( 'NONE',  ( 0.7071067811865487940, 0.7071067811865463515, 0.000000000000000000 ) ) ;
#9846 = ORIENTED_EDGE ( 'NONE', *, *, #35728, .F. ) ;
#9845 = CARTESIAN_POINT ( 'NONE',  ( 34.49999999999975131, -5.568876922607759461, 4.000000000000000000 ) ) ;
#9847 = CARTESIAN_POINT ( 'NONE',  ( 128.5894344200537773, -52.00875322212549179, -39.86617647058817226 ) ) ;
#9848 = CARTESIAN_POINT ( 'NONE',  ( -21.18398860626899349, 28.73617430169802134, 5.000000000000000000 ) ) ;
#9849 = AXIS2_PLACEMENT_3D ( 'NONE', #121094, #141432, #87053 ) ;
#9850 = CARTESIAN_POINT ( 'NONE',  ( 31.82816939922330945, 6.759292476615649470, 4.000000000000000000 ) ) ;
#9851 = PLANE ( 'NONE',  #57726 ) ;
#9852 = ORIENTED_EDGE ( 'NONE', *, *, #136460, .F. ) ;
#9853 = EDGE_CURVE ( 'NONE', #55021, #47967, #119074, .T. ) ;
#9854 = ORIENTED_EDGE ( 'NONE', *, *, #138768, .F. ) ;
#9855 = CARTESIAN_POINT ( 'NONE',  ( 67.37543019189810423, -5.291415217122920289, -3.055000000000001492 ) ) ;
#9856 = ORIENTED_EDGE ( 'NONE', *, *, #40724, .F. ) ;
#9857 = CARTESIAN_POINT ( 'NONE',  ( -9.498163485139505369, -17.24070752338410273, 8.407044977365249139 ) ) ;
#9858 = DIRECTION ( 'NONE',  ( -0.000000000000000000, 0.3543493200069153248, 0.9351131265310292928 ) ) ;
#9859 = CARTESIAN_POINT ( 'NONE',  ( 10.52840764549667618, -1.925929944387235853E-31, 2.500000000000001332 ) ) ;
#9860 = VERTEX_POINT ( 'NONE', #19766 ) ;
#9861 = ORIENTED_EDGE ( 'NONE', *, *, #1188, .T. ) ;
#9862 = VECTOR ( 'NONE', #84857, 1000.000000000000000 ) ;
#9863 = AXIS2_PLACEMENT_3D ( 'NONE', #4469, #57522, #125628 ) ;
#9864 = LINE ( 'NONE', #44697, #5135 ) ;
#9865 = DIRECTION ( 'NONE',  ( -0.000000000000000000, 1.000000000000000000, 0.000000000000000000 ) ) ;
#9866 = VECTOR ( 'NONE', #128692, 1000.000000000000227 ) ;
#9867 = VECTOR ( 'NONE', #27923, 1000.000000000000000 ) ;
#9868 = VERTEX_POINT ( 'NONE', #118356 ) ;
#9869 = LINE ( 'NONE', #88894, #86081 ) ;
#9871 = CARTESIAN_POINT ( 'NONE',  ( 12.19999999999999574, -34.65000000000001279, -40.00000000000000000 ) ) ;
#9870 = VECTOR ( 'NONE', #108772, 999.9999999999998863 ) ;
#9872 = LINE ( 'NONE', #20020, #47061 ) ;
#9873 = VECTOR ( 'NONE', #89713, 1000.000000000000000 ) ;
#9874 = ORIENTED_EDGE ( 'NONE', *, *, #79413, .F. ) ;
#9875 = VERTEX_POINT ( 'NONE', #96576 ) ;
#9876 = FACE_OUTER_BOUND ( 'NONE', #72613, .T. ) ;
#9877 = LINE ( 'NONE', #98337, #57107 ) ;
#9878 = DIRECTION ( 'NONE',  ( 0.6830127018922181881, 0.6830127018922202975, -0.2588190451025214056 ) ) ;
#9879 = CARTESIAN_POINT ( 'NONE',  ( 61.52083333333332149, 7.949999999999998401, 2.130196079827431532 ) ) ;
#9880 = DIRECTION ( 'NONE',  ( -0.000000000000000000, 0.000000000000000000, 1.000000000000000000 ) ) ;
#9881 = DIRECTION ( 'NONE',  ( 0.000000000000000000, 0.000000000000000000, 1.000000000000000000 ) ) ;
#9882 = VERTEX_POINT ( 'NONE', #74165 ) ;
#9883 = AXIS2_PLACEMENT_3D ( 'NONE', #11182, #88811, #46771 ) ;
#9884 = EDGE_LOOP ( 'NONE', ( #13825, #86964, #31811, #62397, #141280 ) ) ;
#9885 = CARTESIAN_POINT ( 'NONE',  ( 116.8704301918981230, -3.055000000000001492, 5.291415217122917625 ) ) ;
#9886 = ORIENTED_EDGE ( 'NONE', *, *, #138597, .F. ) ;
#9887 = VERTEX_POINT ( 'NONE', #64003 ) ;
#9888 = SURFACE_STYLE_FILL_AREA ( #121044 ) ;
#9889 = AXIS2_PLACEMENT_3D ( 'NONE', #25255, #23843, #3482 ) ;
#9890 = DIRECTION ( 'NONE',  ( -0.7071067811865486830, -0.7071067811865464625, -0.000000000000000000 ) ) ;
#9891 = LINE ( 'NONE', #30222, #21629 ) ;
#9892 = ADVANCED_FACE ( 'NONE', ( #52392 ), #29919, .T. ) ;
#9893 = ORIENTED_EDGE ( 'NONE', *, *, #101893, .T. ) ;
#9894 = LINE ( 'NONE', #8430, #48281 ) ;
#9895 = CARTESIAN_POINT ( 'NONE',  ( -32.99999999999976552, 14.87792677143806230, -11.06722581663447791 ) ) ;
#9896 = CIRCLE ( 'NONE', #19226, 0.5000000000000004441 ) ;
#9897 = CARTESIAN_POINT ( 'NONE',  ( -30.18398860626900060, 28.73617430169808173, 5.000000000000000000 ) ) ;
#9898 = DIRECTION ( 'NONE',  ( -0.7071067811865486830, -0.7071067811865464625, -0.000000000000000000 ) ) ;
#9899 = VECTOR ( 'NONE', #186, 1000.000000000000000 ) ;
#9900 = AXIS2_PLACEMENT_3D ( 'NONE', #99895, #76745, #21628 ) ;
#9901 = CARTESIAN_POINT ( 'NONE',  ( 1.277919311390762758, 0.3448754841691806794, 3.790415138944262186 ) ) ;
#9902 = EDGE_LOOP ( 'NONE', ( #121830, #60802, #62152, #63968 ) ) ;
#9903 = LINE ( 'NONE', #29505, #3247 ) ;
#9904 = LINE ( 'NONE', #142586, #18755 ) ;
#9905 = EDGE_CURVE ( 'NONE', #108536, #33945, #41513, .T. ) ;
#9906 = VERTEX_POINT ( 'NONE', #97297 ) ;
#9907 = ORIENTED_EDGE ( 'NONE', *, *, #17531, .F. ) ;
#9908 = EDGE_CURVE ( 'NONE', #26733, #80864, #135693, .T. ) ;
#9909 = EDGE_CURVE ( 'NONE', #121879, #112076, #31372, .T. ) ;
#9910 = VERTEX_POINT ( 'NONE', #39880 ) ;
#9911 = CARTESIAN_POINT ( 'NONE',  ( 66.79209685856477563, -5.291415217122921177, 3.054999999999999272 ) ) ;
#9912 = VERTEX_POINT ( 'NONE', #84780 ) ;
#9914 = EDGE_CURVE ( 'NONE', #71118, #8088, #61632, .T. ) ;
#9913 = VECTOR ( 'NONE', #31915, 1000.000000000000114 ) ;
#9915 = EDGE_CURVE ( 'NONE', #76248, #30378, #106490, .T. ) ;
#9916 = DIRECTION ( 'NONE',  ( 0.7071067811865487940, 0.7071067811865463515, 0.000000000000000000 ) ) ;
#9918 =( BOUNDED_CURVE ( )  B_SPLINE_CURVE ( 2, ( #122836, #100379, #112667, #14782, #35867, #13331, #68486 ),
 .UNSPECIFIED., .F., .T. ) 
 B_SPLINE_CURVE_WITH_KNOTS ( ( 3, 2, 2, 3 ),
 ( 0.000000000000000000, 0.002777777777777780052, 0.005555555555555560104, 0.008333333333333340157 ),
 .UNSPECIFIED. ) 
 CURVE ( )  GEOMETRIC_REPRESENTATION_ITEM ( )  RATIONAL_B_SPLINE_CURVE ( ( 1.000000000000000000, 0.9659258262890683122, 1.000000000000000000, 0.9659258262890683122, 1.000000000000000000, 0.9659258262890678681, 1.000000000000000444 ) ) 
 REPRESENTATION_ITEM ( '' )  );
#9917 = CARTESIAN_POINT ( 'NONE',  ( 103.1045968585647614, 1.637169565754164946, -6.109999999999999432 ) ) ;
#9919 = CARTESIAN_POINT ( 'NONE',  ( 12.82439460721831104, 2.055000000000001048, 2.516649172247811554E-16 ) ) ;
#9920 = EDGE_CURVE ( 'NONE', #31242, #127932, #41259, .T. ) ;
#9921 = AXIS2_PLACEMENT_3D ( 'NONE', #3962, #59843, #104010 ) ;
#9922 = ORIENTED_EDGE ( 'NONE', *, *, #51040, .F. ) ;
#9923 = CARTESIAN_POINT ( 'NONE',  ( 2.301729841053981485, 3.821174125832445049E-16, 0.000000000000000000 ) ) ;
#9924 = AXIS2_PLACEMENT_3D ( 'NONE', #60888, #40528, #118029 ) ;
#9925 = EDGE_CURVE ( 'NONE', #3772, #27504, #70103, .T. ) ;
#9926 = CARTESIAN_POINT ( 'NONE',  ( 2.994519915287485734, 28.92564299267940342, 4.000000000000000000 ) ) ;
#9927 = CARTESIAN_POINT ( 'NONE',  ( 18.18398860626898994, 28.73617430169800002, 5.000000000000000000 ) ) ;
#9928 = CARTESIAN_POINT ( 'NONE',  ( 60.18398860626900415, 28.73617430169829490, 5.000000000000000000 ) ) ;
#9929 = ADVANCED_FACE ( 'NONE', ( #129695 ), #49333, .F. ) ;
#9930 = ORIENTED_EDGE ( 'NONE', *, *, #139893, .F. ) ;
#9931 = ORIENTED_EDGE ( 'NONE', *, *, #6302, .F. ) ;
#9932 = ORIENTED_EDGE ( 'NONE', *, *, #111355, .F. ) ;
#9933 = VERTEX_POINT ( 'NONE', #60941 ) ;
#9934 = CARTESIAN_POINT ( 'NONE',  ( 121.0995968585647802, -6.109999999999997655, -1.637169565754160283 ) ) ;
#9936 = ORIENTED_EDGE ( 'NONE', *, *, #90310, .F. ) ;
#9935 = AXIS2_PLACEMENT_3D ( 'NONE', #134722, #3433, #135429 ) ;
#9937 = CARTESIAN_POINT ( 'NONE',  ( -12.18398860626900060, 28.73617430169795739, 5.000000000000000000 ) ) ;
#9938 = EDGE_CURVE ( 'NONE', #129447, #16801, #6449, .T. ) ;
#9939 = DIRECTION ( 'NONE',  ( -0.6830127018922181881, 0.6830127018922202975, -0.2588190451025214056 ) ) ;
#9940 = VERTEX_POINT ( 'NONE', #73906 ) ;
#9941 = CARTESIAN_POINT ( 'NONE',  ( 33.48921356237309510, -27.52281430457078670, 5.000000000000000000 ) ) ;
#9942 = VECTOR ( 'NONE', #111478, 1000.000000000000000 ) ;
#9943 = EDGE_LOOP ( 'NONE', ( #69719, #67387, #12799, #123595 ) ) ;
#9944 = EDGE_CURVE ( 'NONE', #79175, #14571, #139899, .T. ) ;
#9945 = CARTESIAN_POINT ( 'NONE',  ( 17.18706980810188867, -2.126176841940956130, 7.934999999999991616 ) ) ;
#9946 = DIRECTION ( 'NONE',  ( 0.7071067811865486830, -0.7071067811865464625, -0.000000000000000000 ) ) ;
#9947 = CARTESIAN_POINT ( 'NONE',  ( 28.00000000000002487, -49.14999999999999147, -34.92499999999976978 ) ) ;
#9948 = CARTESIAN_POINT ( 'NONE',  ( 11.74750898584326464, -8.547897970587566618, -4.147060425997655564 ) ) ;
#9949 = ORIENTED_EDGE ( 'NONE', *, *, #108303, .F. ) ;
#9950 = VERTEX_POINT ( 'NONE', #140572 ) ;
#9952 = VERTEX_POINT ( 'NONE', #84103 ) ;
#9951 = ADVANCED_FACE ( 'NONE', ( #83362 ), #38430, .F. ) ;
#9953 = CARTESIAN_POINT ( 'NONE',  ( 19.97916666666666785, 6.094999999999988205, -1.633150327867694651 ) ) ;
#9954 = FILL_AREA_STYLE ('',( #20106 ) ) ;
#9955 = UNCERTAINTY_MEASURE_WITH_UNIT (LENGTH_MEASURE( 1.000000000000000082E-05 ), #59728, 'distance_accuracy_value', 'NONE');
#9956 = FACE_OUTER_BOUND ( 'NONE', #10775, .T. ) ;
#9957 = PLANE ( 'NONE',  #59896 ) ;
#9958 = VECTOR ( 'NONE', #116929, 1000.000000000000227 ) ;
#9959 = VECTOR ( 'NONE', #24888, 999.9999999999998863 ) ;
#9960 = EDGE_CURVE ( 'NONE', #70528, #58012, #107234, .T. ) ;
#9961 = CARTESIAN_POINT ( 'NONE',  ( -5.207106781186506161, -17.24070752338410628, 5.000000000000000000 ) ) ;
#9962 = CARTESIAN_POINT ( 'NONE',  ( 31.20876352523144348, -7.482591942790329030E-16, 6.110000000000001208 ) ) ;
#9963 = DIRECTION ( 'NONE',  ( 0.7071067811865487940, -0.7071067811865463515, 0.000000000000000000 ) ) ;
#9964 = DIRECTION ( 'NONE',  ( 0.000000000000000000, 0.000000000000000000, -1.000000000000000000 ) ) ;
#9965 = EDGE_CURVE ( 'NONE', #73925, #97534, #115954, .T. ) ;
#9966 = VERTEX_POINT ( 'NONE', #105098 ) ;
#9967 = LINE ( 'NONE', #7815, #120384 ) ;
#9968 = VECTOR ( 'NONE', #118329, 1000.000000000000000 ) ;
#9969 = VECTOR ( 'NONE', #16830, 1000.000000000000000 ) ;
#9971 = ORIENTED_EDGE ( 'NONE', *, *, #84467, .T. ) ;
#9970 =( GEOMETRIC_REPRESENTATION_CONTEXT ( 3 ) GLOBAL_UNCERTAINTY_ASSIGNED_CONTEXT ( ( #93698 ) ) GLOBAL_UNIT_ASSIGNED_CONTEXT ( ( #43256, #54845, #32367 ) ) REPRESENTATION_CONTEXT ( 'NONE', 'WORKASPACE' ) );
#9972 = CARTESIAN_POINT ( 'NONE',  ( 18.70710678118641468, 11.25929247661559529, 5.000000000000000000 ) ) ;
#9973 = ORIENTED_EDGE ( 'NONE', *, *, #131895, .T. ) ;
#9974 = EDGE_CURVE ( 'NONE', #76525, #126332, #98089, .T. ) ;
#9975 = FACE_OUTER_BOUND ( 'NONE', #124717, .T. ) ;
#9977 = ORIENTED_EDGE ( 'NONE', *, *, #110062, .T. ) ;
#9976 = DIRECTION ( 'NONE',  ( 0.7071067811865487940, 0.7071067811865463515, -0.000000000000000000 ) ) ;
#9978 = CARTESIAN_POINT ( 'NONE',  ( 4.658131166821905644, 3.821174125832445049E-16, 0.000000000000000000 ) ) ;
#9979 = ORIENTED_EDGE ( 'NONE', *, *, #5329, .T. ) ;
#9980 = FACE_OUTER_BOUND ( 'NONE', #96212, .T. ) ;
#9981 = VERTEX_POINT ( 'NONE', #52148 ) ;
#9982 = FACE_OUTER_BOUND ( 'NONE', #66996, .T. ) ;
#9983 = UNCERTAINTY_MEASURE_WITH_UNIT (LENGTH_MEASURE( 1.000000000000000082E-05 ), #133825, 'distance_accuracy_value', 'NONE');
#9984 = ORIENTED_EDGE ( 'NONE', *, *, #24077, .T. ) ;
#9985 = EDGE_CURVE ( 'NONE', #29352, #102792, #138456, .T. ) ;
#9986 = DIRECTION ( 'NONE',  ( 0.000000000000000000, -1.000000000000000000, 0.000000000000000000 ) ) ;
#9987 =( BOUNDED_CURVE ( )  B_SPLINE_CURVE ( 2, ( #83232, #27393, #115814, #36170, #36856, #39012, #60066, #28138, #92657, #91952, #80398, #16520, #26705 ),
 .UNSPECIFIED., .F., .T. ) 
 B_SPLINE_CURVE_WITH_KNOTS ( ( 3, 2, 2, 2, 2, 2, 3 ),
 ( 0.1166666666666666408, 0.1194444444444444225, 0.1222222222222221905, 0.1249999999999999722, 0.1277777777777777402, 0.1305555555555555358, 0.1333333333333333037 ),
 .UNSPECIFIED. ) 
 CURVE ( )  GEOMETRIC_REPRESENTATION_ITEM ( )  RATIONAL_B_SPLINE_CURVE ( ( 1.000000000000000444, 0.9659258262890679791, 1.000000000000000000, 0.9659258262890683122, 1.000000000000000000, 0.9659258262890683122, 1.000000000000000000, 0.9659258262890683122, 1.000000000000000000, 0.9659258262890683122, 1.000000000000000000, 0.9659258262890686453, 0.9999999999999996669 ) ) 
 REPRESENTATION_ITEM ( '' )  );
#9988 = CARTESIAN_POINT ( 'NONE',  ( 115.2875270504628986, 0.000000000000000000, -7.949999999999998401 ) ) ;
#9989 = CARTESIAN_POINT ( 'NONE',  ( 50.10002705046289151, 5.819803920172570422, 5.819803920172575751 ) ) ;
#9990 = VECTOR ( 'NONE', #134272, 999.9999999999998863 ) ;
#9991 = LINE ( 'NONE', #75277, #87633 ) ;
#9992 = ADVANCED_FACE ( 'NONE', ( #39145 ), #127575, .F. ) ;
#9993 = LINE ( 'NONE', #86860, #74635 ) ;
#9994 = CARTESIAN_POINT ( 'NONE',  ( -31.82816939922330235, -2.240707523384260824, 4.000000000000000000 ) ) ;
#9995 = CARTESIAN_POINT ( 'NONE',  ( -5.331532588401397099, -18.74070752338408496, 20.73178291233839943 ) ) ;
#9996 = CARTESIAN_POINT ( 'NONE',  ( 5.833333333333333925, 5.278424836066143655, -3.047499999999997655 ) ) ;
#9997 = CARTESIAN_POINT ( 'NONE',  ( 20.39540314143521726, 2.126176841940962348, 7.934999999999988951 ) ) ;
#9998 = SURFACE_STYLE_USAGE ( .BOTH. , #120150 ) ;
#9999 = DIRECTION ( 'NONE',  ( 0.6830127018922181881, 0.6830127018922202975, -0.2588190451025214056 ) ) ;
#10000 = ORIENTED_EDGE ( 'NONE', *, *, #78306, .F. ) ;
#10001 = VECTOR ( 'NONE', #128689, 1000.000000000000114 ) ;
#10002 = VERTEX_POINT ( 'NONE', #28978 ) ;
#10003 = CARTESIAN_POINT ( 'NONE',  ( 2.292986735706931345, -21.74070752338405654, 4.999753212805221558 ) ) ;
#10004 = VERTEX_POINT ( 'NONE', #117374 ) ;
#10005 = PRODUCT_DEFINITION_SHAPE ( 'NONE', 'NONE',  #104142 ) ;
#10006 = EDGE_CURVE ( 'NONE', #112008, #80926, #62338, .T. ) ;
#10007 = VECTOR ( 'NONE', #73445, 1000.000000000000000 ) ;
#10008 = LINE ( 'NONE', #30336, #96541 ) ;
#10009 = DIRECTION ( 'NONE',  ( -1.000000000000000000, -0.000000000000000000, -0.000000000000000000 ) ) ;
#10010 = CARTESIAN_POINT ( 'NONE',  ( 131.4501442085549456, -48.99436351328196082, -39.52330221398180754 ) ) ;
#10011 = VERTEX_POINT ( 'NONE', #29663 ) ;
#10012 = CARTESIAN_POINT ( 'NONE',  ( 0.1839886062690032631, 28.73617430169787568, 5.000000000000000000 ) ) ;
#10013 = FACE_OUTER_BOUND ( 'NONE', #59639, .T. ) ;
#10014 = VECTOR ( 'NONE', #28700, 999.9999999999998863 ) ;
#10015 = CARTESIAN_POINT ( 'NONE',  ( 63.18398860626900415, 28.73617430169831621, 5.000000000000000000 ) ) ;
#10016 = EDGE_CURVE ( 'NONE', #63984, #142234, #118080, .T. ) ;
#10017 = DIRECTION ( 'NONE',  ( -0.000000000000000000, -4.625929269271485322E-15, -1.000000000000000000 ) ) ;
#10019 = VERTEX_POINT ( 'NONE', #37989 ) ;
#10018 = DIRECTION ( 'NONE',  ( 1.000000000000000000, 1.224606353822377258E-16, 0.000000000000000000 ) ) ;
#10020 = FACE_OUTER_BOUND ( 'NONE', #24090, .T. ) ;
#10021 = DIRECTION ( 'NONE',  ( -0.9843059135694992579, 0.000000000000000000, -0.1764705882353013178 ) ) ;
#10022 = DIRECTION ( 'NONE',  ( 0.7071067811865486830, -0.7071067811865464625, -0.000000000000000000 ) ) ;
#10023 = CARTESIAN_POINT ( 'NONE',  ( 11.29289321881337571, 17.25929247661554200, 5.000000000000000000 ) ) ;
#10024 = FACE_OUTER_BOUND ( 'NONE', #117440, .T. ) ;
#10025 = CIRCLE ( 'NONE', #95701, 5.968999999999998529 ) ;
#10026 = ORIENTED_EDGE ( 'NONE', *, *, #5178, .T. ) ;
#10027 = VERTEX_POINT ( 'NONE', #37256 ) ;
#10028 = ORIENTED_EDGE ( 'NONE', *, *, #7940, .T. ) ;
#10029 = CARTESIAN_POINT ( 'NONE',  ( 94.64626352523143282, -4.472830434245840259, 4.472830434245839371 ) ) ;
#10030 = VECTOR ( 'NONE', #98921, 1000.000000000000000 ) ;
#10031 = ORIENTED_EDGE ( 'NONE', *, *, #39591, .T. ) ;
#10032 = CARTESIAN_POINT ( 'NONE',  ( 128.0481121284663857, -51.19676978474465301, 38.21513923100059884 ) ) ;
#10033 = MECHANICAL_DESIGN_GEOMETRIC_PRESENTATION_REPRESENTATION (  '', ( #24014 ), #63375 ) ;
#10034 = CARTESIAN_POINT ( 'NONE',  ( 16.49999999999988631, 19.39370406404968605, 1.459788787078164063 ) ) ;
#10035 = VERTEX_POINT ( 'NONE', #92321 ) ;
#10036 = CARTESIAN_POINT ( 'NONE',  ( -21.88837638105228933, 9.759292476615614831, 17.35367589129217691 ) ) ;
#10038 = ADVANCED_FACE ( 'NONE', ( #4551 ), #114781, .F. ) ;
#10037 = DIRECTION ( 'NONE',  ( 0.7071067811865486830, -0.7071067811865464625, -0.000000000000000000 ) ) ;
#10039 = CARTESIAN_POINT ( 'NONE',  ( 88.14126352523143737, 4.472830434245836706, 4.472830434245840259 ) ) ;
#10040 = EDGE_CURVE ( 'NONE', #24873, #57148, #104642, .T. ) ;
#10041 = VERTEX_POINT ( 'NONE', #139460 ) ;
#10042 = DIRECTION ( 'NONE',  ( 0.7071067811865486830, -0.7071067811865464625, -0.000000000000000000 ) ) ;
#10043 = DIRECTION ( 'NONE',  ( 0.7071067811865487940, 0.7071067811865463515, -0.000000000000000000 ) ) ;
#10044 = ORIENTED_EDGE ( 'NONE', *, *, #135848, .F. ) ;
#10045 = ORIENTED_EDGE ( 'NONE', *, *, #6613, .T. ) ;
#10046 = VERTEX_POINT ( 'NONE', #82219 ) ;
#10047 = CARTESIAN_POINT ( 'NONE',  ( -20.99451991528748707, 28.92564299267952777, 4.000000000000000000 ) ) ;
#10048 = EDGE_CURVE ( 'NONE', #1418, #54913, #28534, .T. ) ;
#10049 = CARTESIAN_POINT ( 'NONE',  ( 26.66989781452719299, 17.25929247661554555, 19.83885114516065329 ) ) ;
#10050 = VECTOR ( 'NONE', #136619, 1000.000000000000000 ) ;
#10051 = CARTESIAN_POINT ( 'NONE',  ( 9.299744871391588674, -27.71228299555212971, 4.000000000000000000 ) ) ;
#10052 = DIRECTION ( 'NONE',  ( -1.000000000000000000, -0.000000000000000000, -0.000000000000000000 ) ) ;
#10053 = FACE_OUTER_BOUND ( 'NONE', #40201, .T. ) ;
#10054 = PRESENTATION_LAYER_ASSIGNMENT (  '', '', ( #14724 ) ) ;
#10055 = ORIENTED_EDGE ( 'NONE', *, *, #43353, .F. ) ;
#10056 = VERTEX_POINT ( 'NONE', #103208 ) ;
#10057 = DIRECTION ( 'NONE',  ( -0.000000000000000000, 0.000000000000000000, 1.000000000000000000 ) ) ;
#10058 = ORIENTED_EDGE ( 'NONE', *, *, #3567, .F. ) ;
#10059 = ORIENTED_EDGE ( 'NONE', *, *, #74856, .F. ) ;
#10060 = AXIS2_PLACEMENT_3D ( 'NONE', #807, #112454, #121871 ) ;
#10061 = CARTESIAN_POINT ( 'NONE',  ( 15.13014816246815109, 7.677378749015542070, 4.326165144404741092 ) ) ;
#10062 = EDGE_CURVE ( 'NONE', #122249, #14269, #79621, .T. ) ;
#10063 = ORIENTED_EDGE ( 'NONE', *, *, #32221, .F. ) ;
#10064 = CARTESIAN_POINT ( 'NONE',  ( 26.79783616915502975, -7.489999999999998437, -4.586302262806838083E-16 ) ) ;
#10065 = FACE_OUTER_BOUND ( 'NONE', #143477, .T. ) ;
#10066 = DIRECTION ( 'NONE',  ( 0.3543493200069162685, -0.000000000000000000, -0.9351131265310288487 ) ) ;
#10067 = LINE ( 'NONE', #99949, #143281 ) ;
#10068 = LINE ( 'NONE', #53602, #134631 ) ;
#10069 = VERTEX_POINT ( 'NONE', #138722 ) ;
#10070 = DIRECTION ( 'NONE',  ( -1.000000000000000000, -0.000000000000000000, -0.000000000000000000 ) ) ;
#10071 = ORIENTED_EDGE ( 'NONE', *, *, #69687, .T. ) ;
#10072 = CARTESIAN_POINT ( 'NONE',  ( 19.28515664589288647, 1.196650378695337302, -30.59010235425025215 ) ) ;
#10073 = VERTEX_POINT ( 'NONE', #82915 ) ;
#10074 = DIRECTION ( 'NONE',  ( 0.7071067811865487940, 0.7071067811865463515, -0.000000000000000000 ) ) ;
#10076 = ORIENTED_EDGE ( 'NONE', *, *, #107350, .F. ) ;
#10075 = EDGE_CURVE ( 'NONE', #130332, #19651, #27079, .T. ) ;
#10077 = CARTESIAN_POINT ( 'NONE',  ( -9.183988606268997046, 28.73617430169793607, 5.000000000000000000 ) ) ;
#10078 = ORIENTED_EDGE ( 'NONE', *, *, #41116, .F. ) ;
#10079 = ORIENTED_EDGE ( 'NONE', *, *, #75503, .T. ) ;
#10080 = CIRCLE ( 'NONE', #28640, 2.500000000000000888 ) ;
#10081 = ORIENTED_EDGE ( 'NONE', *, *, #53, .T. ) ;
#10082 = ADVANCED_FACE ( 'NONE', ( #17613 ), #115479, .F. ) ;
#10083 = ADVANCED_FACE ( 'NONE', ( #81504 ), #5310, .T. ) ;
#10084 = CARTESIAN_POINT ( 'NONE',  ( -33.70710678118631165, -0.7407075233842788098, 5.000000000000000000 ) ) ;
#10085 = PLANE ( 'NONE',  #38286 ) ;
#10086 = MECHANICAL_DESIGN_GEOMETRIC_PRESENTATION_REPRESENTATION (  '', ( #858 ), #19400 ) ;
#10087 = DIRECTION ( 'NONE',  ( 0.6830127018922180770, -0.6830127018922204085, -0.2588190451025213501 ) ) ;
#10089 = EDGE_CURVE ( 'NONE', #73407, #20849, #10107, .T. ) ;
#10088 = CARTESIAN_POINT ( 'NONE',  ( 25.49999999999982947, -7.420205493532873398, -2.617629953481194871 ) ) ;
#10090 = CARTESIAN_POINT ( 'NONE',  ( 124.2504301918981184, 3.055000000000002824, -5.291415217122919401 ) ) ;
#10091 = FACE_OUTER_BOUND ( 'NONE', #107438, .T. ) ;
#10092 = EDGE_CURVE ( 'NONE', #71076, #135550, #93776, .T. ) ;
#10093 = PLANE ( 'NONE',  #108425 ) ;
#10094 = EDGE_CURVE ( 'NONE', #76593, #51414, #70639, .T. ) ;
#10096 = CARTESIAN_POINT ( 'NONE',  ( 0.3281693992235254487, -21.74070752338406365, 4.000000000000000000 ) ) ;
#10095 = AXIS2_PLACEMENT_3D ( 'NONE', #34212, #57405, #111018 ) ;
#10097 = PLANE ( 'NONE',  #15774 ) ;
#10098 = EDGE_CURVE ( 'NONE', #91612, #106603, #138001, .T. ) ;
#10099 = DIRECTION ( 'NONE',  ( 0.3543493200069162685, -0.000000000000000000, -0.9351131265310288487 ) ) ;
#10100 = AXIS2_PLACEMENT_3D ( 'NONE', #21185, #8825, #131388 ) ;
#10101 = LINE ( 'NONE', #54366, #95642 ) ;
#10102 = EDGE_LOOP ( 'NONE', ( #30870, #91775, #48933, #52954 ) ) ;
#10103 = ORIENTED_EDGE ( 'NONE', *, *, #56682, .F. ) ;
#10104 = ORIENTED_EDGE ( 'NONE', *, *, #84010, .F. ) ;
#10105 = DIRECTION ( 'NONE',  ( -0.000000000000000000, -0.3543493200069152693, 0.9351131265310292928 ) ) ;
#10106 = ORIENTED_EDGE ( 'NONE', *, *, #66644, .T. ) ;
#10107 = CIRCLE ( 'NONE', #128209, 2.500000000000000444 ) ;
#10108 = ORIENTED_EDGE ( 'NONE', *, *, #101234, .T. ) ;
#10109 = DIRECTION ( 'NONE',  ( -0.3543493200069163240, 0.000000000000000000, -0.9351131265310288487 ) ) ;
#10110 = PLANE ( 'NONE',  #114937 ) ;
#10111 = EDGE_CURVE ( 'NONE', #113508, #16702, #65744, .T. ) ;
#10112 = EDGE_CURVE ( 'NONE', #79734, #75031, #73462, .T. ) ;
#10113 = CARTESIAN_POINT ( 'NONE',  ( 10.49999999999992184, 1.087461875839246250, 4.000000000000000000 ) ) ;
#10114 = ORIENTED_EDGE ( 'NONE', *, *, #105560, .T. ) ;
#10115 = DIRECTION ( 'NONE',  ( 0.6830127018922180770, -0.6830127018922204085, -0.2588190451025213501 ) ) ;
#10116 = ORIENTED_EDGE ( 'NONE', *, *, #54417, .T. ) ;
#10117 = ADVANCED_FACE ( 'NONE', ( #93061 ), #16930, .F. ) ;
#10119 = AXIS2_PLACEMENT_3D ( 'NONE', #73930, #85493, #129723 ) ;
#10118 = CARTESIAN_POINT ( 'NONE',  ( -57.18398860626899705, 28.73617430169827358, 5.000000000000000000 ) ) ;
#10120 = DIRECTION ( 'NONE',  ( 0.7071067811865487940, 0.7071067811865463515, 0.000000000000000000 ) ) ;
#10121 = VECTOR ( 'NONE', #35480, 1000.000000000000000 ) ;
#10122 = CARTESIAN_POINT ( 'NONE',  ( 22.23373647476855197, 5.808823158059036373, 5.808823158059032821 ) ) ;
#10123 = EDGE_LOOP ( 'NONE', ( #81479, #59874, #123826, #128827 ) ) ;
#10124 = CARTESIAN_POINT ( 'NONE',  ( 93.53709685856479439, -3.054999999999999272, -5.291415217122919401 ) ) ;
#10125 = CARTESIAN_POINT ( 'NONE',  ( 6.540342856384453896, -9.242792321178736614, -2.199412111314436036 ) ) ;
#10126 = CARTESIAN_POINT ( 'NONE',  ( -48.48921356237309510, -27.52281430457089328, 5.000000000000000000 ) ) ;
#10127 = CARTESIAN_POINT ( 'NONE',  ( 17.85999999999999943, 9.521314400968980422E-16, 0.000000000000000000 ) ) ;
#10128 = VERTEX_POINT ( 'NONE', #61202 ) ;
#10129 = CYLINDRICAL_SURFACE ( 'NONE', #56749, 7.950000000000000178 ) ;
#10130 = VERTEX_POINT ( 'NONE', #6006 ) ;
#10131 = ORIENTED_EDGE ( 'NONE', *, *, #63865, .T. ) ;
#10133 = VECTOR ( 'NONE', #19968, 1000.000000000000000 ) ;
#10132 = CARTESIAN_POINT ( 'NONE',  ( 31.49999999999977973, 13.08746187583911436, 4.000000000000000000 ) ) ;
#10134 = CARTESIAN_POINT ( 'NONE',  ( -20.56319896779158185, -12.74070752338415069, 9.898150129686422716 ) ) ;
#10135 = DIRECTION ( 'NONE',  ( -0.6830127018922180770, -0.6830127018922204085, -0.2588190451025213501 ) ) ;
#10136 = FACE_OUTER_BOUND ( 'NONE', #127618, .T. ) ;
#10137 = ORIENTED_EDGE ( 'NONE', *, *, #93045, .F. ) ;
#10138 = CARTESIAN_POINT ( 'NONE',  ( 14.42840764549667476, 2.500000000000003553, 3.061616997868386099E-16 ) ) ;
#10139 = CARTESIAN_POINT ( 'NONE',  ( 56.99451991528749062, 28.92564299267978001, 4.000000000000000000 ) ) ;
#10140 = ADVANCED_FACE ( 'NONE', ( #50282 ), #94472, .F. ) ;
#10141 = ORIENTED_EDGE ( 'NONE', *, *, #137673, .T. ) ;
#10142 = DIRECTION ( 'NONE',  ( 0.000000000000000000, 0.000000000000000000, -1.000000000000000000 ) ) ;
#10143 = AXIS2_PLACEMENT_3D ( 'NONE', #27066, #4534, #81489 ) ;
#10144 = CARTESIAN_POINT ( 'NONE',  ( 18.18398860626898994, 28.73617430169800002, 5.000000000000000000 ) ) ;
#10145 = ORIENTED_EDGE ( 'NONE', *, *, #49440, .F. ) ;
#10147 = ORIENTED_EDGE ( 'NONE', *, *, #88004, .F. ) ;
#10146 = CARTESIAN_POINT ( 'NONE',  ( -36.18398860626899705, 28.73617430169812437, 5.000000000000000000 ) ) ;
#10148 = ORIENTED_EDGE ( 'NONE', *, *, #127231, .T. ) ;
#10149 = PLANE ( 'NONE',  #123488 ) ;
#10150 = DIRECTION ( 'NONE',  ( 0.000000000000000000, 0.000000000000000000, 1.000000000000000000 ) ) ;
#10151 = ORIENTED_EDGE ( 'NONE', *, *, #8457, .F. ) ;
#10152 = FACE_OUTER_BOUND ( 'NONE', #48320, .T. ) ;
#10153 = EDGE_CURVE ( 'NONE', #63922, #42670, #30678, .T. ) ;
#10154 = CARTESIAN_POINT ( 'NONE',  ( 1.499999999999984013, 14.14708470758591474, -0.5283514160166593587 ) ) ;
#10156 = VECTOR ( 'NONE', #102501, 1000.000000000000000 ) ;
#10155 = CARTESIAN_POINT ( 'NONE',  ( -33.18398860626899705, 28.73617430169810305, 5.000000000000000000 ) ) ;
#10157 = DIRECTION ( 'NONE',  ( 0.6830127018922180770, -0.6830127018922204085, -0.2588190451025213501 ) ) ;
#10158 = DIRECTION ( 'NONE',  ( 0.7071067811865487940, 0.7071067811865463515, -0.000000000000000000 ) ) ;
#10159 = EDGE_CURVE ( 'NONE', #118849, #100584, #131405, .T. ) ;
#10160 = CARTESIAN_POINT ( 'NONE',  ( -26.99999999999981526, 10.93112307739207267, 4.000000000000000000 ) ) ;
#10161 = CARTESIAN_POINT ( 'NONE',  ( 21.18398860626899349, 28.73617430169802134, 5.000000000000000000 ) ) ;
#10162 = CARTESIAN_POINT ( 'NONE',  ( 18.12391743882421480, 22.22500000000000142, -15.10221789024010874 ) ) ;
#10163 = CARTESIAN_POINT ( 'NONE',  ( -35.39513766812457618, 21.75929247661549226, 21.32995629748194588 ) ) ;
#10164 = CARTESIAN_POINT ( 'NONE',  ( 32.99999999999977973, -8.731860332648809120, -2.120594902707463536 ) ) ;
#10165 = CARTESIAN_POINT ( 'NONE',  ( 21.51665438641029482, 22.22500000000000142, 4.500000000000000888 ) ) ;
#10166 = CARTESIAN_POINT ( 'NONE',  ( -33.81246187583924012, -22.22500000000000142, 4.000000000000000000 ) ) ;
#10167 = ORIENTED_EDGE ( 'NONE', *, *, #42849, .T. ) ;
#10168 = VECTOR ( 'NONE', #54170, 999.9999999999998863 ) ;
#10169 = ORIENTED_EDGE ( 'NONE', *, *, #1232, .F. ) ;
#10170 = CARTESIAN_POINT ( 'NONE',  ( 97.54166666666667140, -3.975000000000002753, 6.884901960086286188 ) ) ;
#10171 = ORIENTED_EDGE ( 'NONE', *, *, #49256, .T. ) ;
#10172 = EDGE_LOOP ( 'NONE', ( #127159, #89750, #35819, #50662 ) ) ;
#10173 = EDGE_CURVE ( 'NONE', #32103, #116900, #41517, .T. ) ;
#10174 = EDGE_LOOP ( 'NONE', ( #106549, #143417, #64177, #79334, #44915 ) ) ;
#10175 = CARTESIAN_POINT ( 'NONE',  ( 42.48921356237308800, -27.52281430457085065, 5.000000000000000000 ) ) ;
#10176 = CARTESIAN_POINT ( 'NONE',  ( 32.99999999999977263, 19.93112307739198030, 4.000000000000000000 ) ) ;
#10177 = ORIENTED_EDGE ( 'NONE', *, *, #123231, .T. ) ;
#10178 = CARTESIAN_POINT ( 'NONE',  ( 6.328169399223481761, -3.740707523384245281, 4.000000000000000000 ) ) ;
#10179 = CARTESIAN_POINT ( 'NONE',  ( 12.19999999999999574, -39.93000000000000682, -40.00000000000000000 ) ) ;
#10180 = PLANE ( 'NONE',  #124 ) ;
#10181 = CARTESIAN_POINT ( 'NONE',  ( -72.18398860626899705, 28.73617430169837661, 5.000000000000000000 ) ) ;
#10182 = EDGE_CURVE ( 'NONE', #38066, #82163, #21203, .T. ) ;
#10183 = EDGE_LOOP ( 'NONE', ( #1692, #16563, #61399, #95948, #113499 ) ) ;
#10184 = CARTESIAN_POINT ( 'NONE',  ( 13.41054942568818298, 6.345126847568487882, -31.22086726222595132 ) ) ;
#10185 = PLANE ( 'NONE',  #105186 ) ;
#10186 = VECTOR ( 'NONE', #87313, 1000.000000000000000 ) ;
#10187 = DIRECTION ( 'NONE',  ( -1.000000000000000000, -1.224606353822377258E-16, -0.000000000000000000 ) ) ;
#10188 = CARTESIAN_POINT ( 'NONE',  ( 22.75000000000000355, -7.464222240803106570E-16, -6.094999999999989981 ) ) ;
#10189 = LINE ( 'NONE', #55877, #91675 ) ;
#10190 = CARTESIAN_POINT ( 'NONE',  ( 27.93336038379622011, 2.130196079827431532, -7.949999999999997513 ) ) ;
#10191 = DIRECTION ( 'NONE',  ( 0.7071067811865487940, 0.7071067811865463515, 0.000000000000000000 ) ) ;
#10192 = EDGE_CURVE ( 'NONE', #133341, #75052, #95907, .T. ) ;
#10193 = EDGE_LOOP ( 'NONE', ( #97808, #134758, #31535, #117418 ) ) ;
#10194 = ORIENTED_EDGE ( 'NONE', *, *, #99181, .F. ) ;
#10195 = CARTESIAN_POINT ( 'NONE',  ( 117.1045968585647898, 1.637169565754164946, -6.109999999999999432 ) ) ;
#10196 = ORIENTED_EDGE ( 'NONE', *, *, #1616, .T. ) ;
#10197 = CARTESIAN_POINT ( 'NONE',  ( -12.20000000000000284, -34.64999999999999147, -39.50000000000000000 ) ) ;
#10198 = CARTESIAN_POINT ( 'NONE',  ( -36.48921356237310221, -27.52281430457080802, 5.000000000000000000 ) ) ;
#10199 = DIRECTION ( 'NONE',  ( -0.7071067811865487940, 0.7071067811865463515, -0.000000000000000000 ) ) ;
#10200 = CARTESIAN_POINT ( 'NONE',  ( 17.29320749275915148, 20.25929247661551358, 20.83292124670811063 ) ) ;
#10201 = DIRECTION ( 'NONE',  ( -0.5735764363510503783, -0.8191520442889886899, 0.000000000000000000 ) ) ;
#10202 = DIRECTION ( 'NONE',  ( -1.000000000000000000, -0.000000000000000000, 0.000000000000000000 ) ) ;
#10203 = CARTESIAN_POINT ( 'NONE',  ( 123.5787635252314516, -7.482591942790325086E-16, 6.109999999999998543 ) ) ;
#10204 = EDGE_CURVE ( 'NONE', #71183, #43110, #56533, .T. ) ;
#10205 = VECTOR ( 'NONE', #95537, 1000.000000000000000 ) ;
#10206 = EDGE_LOOP ( 'NONE', ( #16319, #14721, #22641, #97990 ) ) ;
#10207 = CIRCLE ( 'NONE', #130598, 2.500000000000000444 ) ;
#10208 = ORIENTED_EDGE ( 'NONE', *, *, #10062, .T. ) ;
#10209 = CARTESIAN_POINT ( 'NONE',  ( -6.771599798802371950, -34.64999999999999147, 17.99210858042621908 ) ) ;
#10210 = DIRECTION ( 'NONE',  ( -1.000000000000000000, -1.224606353822377258E-16, -0.000000000000000000 ) ) ;
#10211 =( BOUNDED_CURVE ( )  B_SPLINE_CURVE ( 3, ( #132166, #30715, #54601, #77777 ),
 .UNSPECIFIED., .F., .T. ) 
 B_SPLINE_CURVE_WITH_KNOTS ( ( 4, 4 ),
 ( 5.920967161967926273, 7.341195215986634715 ),
 .UNSPECIFIED. ) 
 CURVE ( )  GEOMETRIC_REPRESENTATION_ITEM ( )  RATIONAL_B_SPLINE_CURVE ( ( 1.000000000000000000, 0.8388583629366618277, 0.8388583629366618277, 1.000000000000000000 ) ) 
 REPRESENTATION_ITEM ( '' )  );
#10212 = AXIS2_PLACEMENT_3D ( 'NONE', #20470, #108897, #64007 ) ;
#10213 = ORIENTED_EDGE ( 'NONE', *, *, #109440, .T. ) ;
#10214 = CARTESIAN_POINT ( 'NONE',  ( 37.04209685856476852, 5.291415217122923842, -3.054999999999996163 ) ) ;
#10215 = VECTOR ( 'NONE', #132834, 1000.000000000000000 ) ;
#10216 = EDGE_LOOP ( 'NONE', ( #31767, #97991, #13463, #85973, #35798 ) ) ;
#10217 = FACE_OUTER_BOUND ( 'NONE', #130782, .T. ) ;
#10218 = EDGE_CURVE ( 'NONE', #1803, #74547, #53864, .T. ) ;
#10219 = DIRECTION ( 'NONE',  ( 0.7071067811865487940, 0.7071067811865463515, -0.000000000000000000 ) ) ;
#10220 = DIRECTION ( 'NONE',  ( -0.6830127018922181881, 0.6830127018922202975, -0.2588190451025214056 ) ) ;
#10221 = AXIS2_PLACEMENT_3D ( 'NONE', #115788, #18630, #5617 ) ;
#10222 = CONICAL_SURFACE ( 'NONE', #26484, 2.055000000000001048, 0.9599310885968758145 ) ;
#10223 = CARTESIAN_POINT ( 'NONE',  ( 36.51626352523145158, -4.472830434245839371, 4.472830434245839371 ) ) ;
#10224 = VERTEX_POINT ( 'NONE', #120475 ) ;
#10225 = DIRECTION ( 'NONE',  ( 0.3543493200069162685, -0.000000000000000000, -0.9351131265310288487 ) ) ;
#10226 = VERTEX_POINT ( 'NONE', #10312 ) ;
#10227 = ORIENTED_EDGE ( 'NONE', *, *, #139070, .F. ) ;
#10228 = ORIENTED_EDGE ( 'NONE', *, *, #135474, .T. ) ;
#10229 = MECHANICAL_DESIGN_GEOMETRIC_PRESENTATION_REPRESENTATION (  '', ( #7941 ), #17187 ) ;
#10230 = DIRECTION ( 'NONE',  ( -0.6830127018922180770, -0.6830127018922204085, -0.2588190451025213501 ) ) ;
#10231 = CARTESIAN_POINT ( 'NONE',  ( 17.99451991528748351, 28.92564299267950645, 4.000000000000000000 ) ) ;
#10232 = VERTEX_POINT ( 'NONE', #32087 ) ;
#10233 = DIRECTION ( 'NONE',  ( 8.673617379884034239E-17, -1.000000000000000000, 0.000000000000000000 ) ) ;
#10234 = CARTESIAN_POINT ( 'NONE',  ( 24.85005128541009611, -8.240707523384189770, 17.25253755692244795 ) ) ;
#10235 = CIRCLE ( 'NONE', #79747, 1.320799999999990870 ) ;
#10236 = DIRECTION ( 'NONE',  ( 0.7071067811865486830, -0.7071067811865464625, -0.000000000000000000 ) ) ;
#10237 = FACE_OUTER_BOUND ( 'NONE', #3209, .T. ) ;
#10238 = FACE_BOUND ( 'NONE', #31698, .T. ) ;
#10239 = ORIENTED_EDGE ( 'NONE', *, *, #102832, .T. ) ;
#10240 = CARTESIAN_POINT ( 'NONE',  ( 13.17183060077638679, -2.240707523384255939, 4.000000000000000000 ) ) ;
#10241 = CARTESIAN_POINT ( 'NONE',  ( 3.225639847634929946, -48.88932940808381744, 39.16623080367947551 ) ) ;
#10242 = DIRECTION ( 'NONE',  ( 0.000000000000000000, -1.000000000000000000, 0.000000000000000000 ) ) ;
#10243 = ORIENTED_EDGE ( 'NONE', *, *, #19404, .T. ) ;
#10244 = PLANE ( 'NONE',  #31849 ) ;
#10245 = VERTEX_POINT ( 'NONE', #53100 ) ;
#10246 = ORIENTED_EDGE ( 'NONE', *, *, #120706, .T. ) ;
#10247 = DIRECTION ( 'NONE',  ( -0.7071067811865487940, 0.7071067811865463515, -0.000000000000000000 ) ) ;
#10248 = ORIENTED_EDGE ( 'NONE', *, *, #46903, .T. ) ;
#10249 = ADVANCED_FACE ( 'NONE', ( #142294 ), #98749, .F. ) ;
#10250 = CARTESIAN_POINT ( 'NONE',  ( 51.68293019189810877, -1.637169565754158951, -6.109999999999998543 ) ) ;
#10251 = ORIENTED_EDGE ( 'NONE', *, *, #78707, .T. ) ;
#10252 = DIRECTION ( 'NONE',  ( -0.7071067811865487940, 0.7071067811865463515, 0.000000000000000000 ) ) ;
#10253 = ADVANCED_FACE ( 'NONE', ( #129975 ), #97301, .F. ) ;
#10254 = FILL_AREA_STYLE_COLOUR ( '', #19489 ) ;
#10255 = DIRECTION ( 'NONE',  ( -0.000000000000000000, 0.3543493200069153248, 0.9351131265310292928 ) ) ;
#10256 = ORIENTED_EDGE ( 'NONE', *, *, #95497, .T. ) ;
#10257 = EDGE_CURVE ( 'NONE', #133408, #13443, #119773, .T. ) ;
#10258 = FACE_OUTER_BOUND ( 'NONE', #122651, .T. ) ;
#10259 = EDGE_CURVE ( 'NONE', #98954, #101163, #123673, .T. ) ;
#10260 = VECTOR ( 'NONE', #89953, 1000.000000000000000 ) ;
#10261 = CARTESIAN_POINT ( 'NONE',  ( -39.48921356237310221, -27.52281430457082934, 5.000000000000000000 ) ) ;
#10262 = CARTESIAN_POINT ( 'NONE',  ( -45.18398860626900415, 28.73617430169818832, 5.000000000000000000 ) ) ;
#10263 = CYLINDRICAL_SURFACE ( 'NONE', #122369, 6.349999999999997868 ) ;
#10264 = FACE_OUTER_BOUND ( 'NONE', #128408, .T. ) ;
#10265 = LINE ( 'NONE', #107443, #16266 ) ;
#10266 = VERTEX_POINT ( 'NONE', #119080 ) ;
#10267 = ORIENTED_EDGE ( 'NONE', *, *, #15900, .T. ) ;
#10268 = ORIENTED_EDGE ( 'NONE', *, *, #14239, .F. ) ;
#10269 = CARTESIAN_POINT ( 'NONE',  ( 3.469446951953614189E-15, -7.447814304570758104, 5.000000000000000000 ) ) ;
#10270 = CARTESIAN_POINT ( 'NONE',  ( -9.792893218813388145, 12.75929247661558996, 5.000000000000000000 ) ) ;
#10271 = ORIENTED_EDGE ( 'NONE', *, *, #54787, .T. ) ;
#10272 = ORIENTED_EDGE ( 'NONE', *, *, #71794, .F. ) ;
#10273 = LINE ( 'NONE', #63289, #9575 ) ;
#10275 = ADVANCED_FACE ( 'NONE', ( #31377 ), #109638, .F. ) ;
#10274 = CARTESIAN_POINT ( 'NONE',  ( 14.67183060077637613, 11.25929247661561128, 4.000000000000000000 ) ) ;
#10276 = EDGE_CURVE ( 'NONE', #16863, #7658, #19770, .T. ) ;
#10277 = LINE ( 'NONE', #54536, #111061 ) ;
#10278 = ORIENTED_EDGE ( 'NONE', *, *, #97038, .F. ) ;
#10279 = LINE ( 'NONE', #132826, #134255 ) ;
#10280 = COLOUR_RGB ( '', 0.40784314, 0.44705882, 0.49803922) ;
#10281 = EDGE_CURVE ( 'NONE', #61260, #107902, #29925, .T. ) ;
#10282 = CARTESIAN_POINT ( 'NONE',  ( -75.48921356237309510, -27.52281430457107803, 5.000000000000000000 ) ) ;
#10283 = VECTOR ( 'NONE', #25345, 1000.000000000000000 ) ;
#10284 = CARTESIAN_POINT ( 'NONE',  ( 19.75456980810189123, -6.871911579029512218, 3.967499999999996252 ) ) ;
#10285 = DIRECTION ( 'NONE',  ( -1.000000000000000000, -1.224606353822377258E-16, -0.000000000000000000 ) ) ;
#10286 = ORIENTED_EDGE ( 'NONE', *, *, #34526, .F. ) ;
#10287 = CARTESIAN_POINT ( 'NONE',  ( 122.9954301918981230, 5.291415217122917625, 3.055000000000002380 ) ) ;
#10288 = AXIS2_PLACEMENT_3D ( 'NONE', #14089, #82248, #135889 ) ;
#10289 = CARTESIAN_POINT ( 'NONE',  ( 6.183988606268994381, 28.73617430169791476, 5.000000000000000000 ) ) ;
#10290 = LINE ( 'NONE', #40118, #135264 ) ;
#10291 = ADVANCED_FACE ( 'NONE', ( #8158 ), #42270, .T. ) ;
#10293 = EDGE_LOOP ( 'NONE', ( #47735, #44106, #135895 ) ) ;
#10292 = CARTESIAN_POINT ( 'NONE',  ( -19.05000000000000071, 3.174999999999997158, 5.000000000000000000 ) ) ;
#10294 = CARTESIAN_POINT ( 'NONE',  ( -21.32816939922336985, -18.74070752338409207, 4.000000000000000000 ) ) ;
#10295 = ORIENTED_EDGE ( 'NONE', *, *, #73754, .T. ) ;
#10296 = DIRECTION ( 'NONE',  ( -0.6830127018922181881, 0.6830127018922202975, -0.2588190451025214056 ) ) ;
#10297 = CARTESIAN_POINT ( 'NONE',  ( -24.70612307739178348, 22.22500000000000142, 4.000000000000000000 ) ) ;
#10298 = DIRECTION ( 'NONE',  ( 1.000000000000000000, 0.000000000000000000, 0.000000000000000000 ) ) ;
#10299 = ORIENTED_EDGE ( 'NONE', *, *, #22679, .F. ) ;
#10300 = VECTOR ( 'NONE', #103376, 1000.000000000000000 ) ;
#10301 = LINE ( 'NONE', #63314, #125163 ) ;
#10302 = PLANE ( 'NONE',  #83770 ) ;
#10303 = ADVANCED_FACE ( 'NONE', ( #52396 ), #96581, .F. ) ;
#10304 = EDGE_LOOP ( 'NONE', ( #45505, #86295, #117562, #20927 ) ) ;
#10305 = DIRECTION ( 'NONE',  ( 0.7071067811865487940, 0.7071067811865463515, -0.000000000000000000 ) ) ;
#10306 = CARTESIAN_POINT ( 'NONE',  ( 27.53159235450332076, 3.061616997868375253E-16, -2.500000000000001332 ) ) ;
#10307 = EDGE_LOOP ( 'NONE', ( #56637, #18371 ) ) ;
#10308 = DIRECTION ( 'NONE',  ( -0.7071067811865486830, 0.7071067811865464625, 0.000000000000000000 ) ) ;
#10310 = ORIENTED_EDGE ( 'NONE', *, *, #25926, .F. ) ;
#10309 = CARTESIAN_POINT ( 'NONE',  ( 21.56169048593611137, 22.22500000000000142, -16.40491860849569861 ) ) ;
#10311 = EDGE_LOOP ( 'NONE', ( #78106, #133887, #11946, #39924 ) ) ;
#10312 = CARTESIAN_POINT ( 'NONE',  ( -19.49999999999986144, 9.431123077392085108, 4.000000000000000000 ) ) ;
#10313 = CARTESIAN_POINT ( 'NONE',  ( 37.40832548098978094, -0.7407075233842770334, 14.76736230305389341 ) ) ;
#10314 = VERTEX_POINT ( 'NONE', #58168 ) ;
#10315 = VECTOR ( 'NONE', #7022, 1000.000000000000000 ) ;
#10316 = ADVANCED_FACE ( 'NONE', ( #36375 ), #135688, .T. ) ;
#10317 = DIRECTION ( 'NONE',  ( 0.7071067811865486830, -0.7071067811865464625, -0.000000000000000000 ) ) ;
#10318 = AXIS2_PLACEMENT_3D ( 'NONE', #81860, #91301, #102873 ) ;
#10319 = CARTESIAN_POINT ( 'NONE',  ( 21.44840764549667611, 9.139736423841732040E-16, 0.000000000000000000 ) ) ;
#10320 = LINE ( 'NONE', #142990, #56169 ) ;
#10321 = ORIENTED_EDGE ( 'NONE', *, *, #65043, .F. ) ;
#10322 = STYLED_ITEM ( 'NONE', ( #138283 ), #7388 ) ;
#10323 = SURFACE_SIDE_STYLE ('',( #119783 ) ) ;
#10324 = DIRECTION ( 'NONE',  ( -0.6830127018922181881, 0.6830127018922202975, -0.2588190451025214056 ) ) ;
#10325 = DIRECTION ( 'NONE',  ( 0.7071067811865487940, 0.7071067811865463515, -0.000000000000000000 ) ) ;
#10326 =( NAMED_UNIT ( * ) PLANE_ANGLE_UNIT ( ) SI_UNIT ( $, .RADIAN. ) );
#10327 = CARTESIAN_POINT ( 'NONE',  ( 36.80793019189810167, -6.109999999999999432, 1.637169565754158507 ) ) ;
#10328 = CARTESIAN_POINT ( 'NONE',  ( -31.49999999999977973, 12.43112307739205669, 4.000000000000000000 ) ) ;
#10329 = CIRCLE ( 'NONE', #107512, 2.500000000000000444 ) ;
#10330 = EDGE_LOOP ( 'NONE', ( #55101, #40055, #129610, #23402, #124751 ) ) ;
#10331 = VERTEX_POINT ( 'NONE', #46587 ) ;
#10332 = CARTESIAN_POINT ( 'NONE',  ( -8.292893218813393474, -12.74070752338415247, 5.000000000000000000 ) ) ;
#10333 = ORIENTED_EDGE ( 'NONE', *, *, #51376, .F. ) ;
#10334 = EDGE_CURVE ( 'NONE', #113756, #98208, #114503, .T. ) ;
#10335 = ORIENTED_EDGE ( 'NONE', *, *, #24904, .F. ) ;
#10336 = CARTESIAN_POINT ( 'NONE',  ( 0.000000000000000000, 0.000000000000000000, 5.000000000000000000 ) ) ;
#10337 = DIRECTION ( 'NONE',  ( 0.7071067811865486830, -0.7071067811865464625, -0.000000000000000000 ) ) ;
#10338 = ORIENTED_EDGE ( 'NONE', *, *, #14548, .F. ) ;
#10339 = SURFACE_SIDE_STYLE ('',( #111065 ) ) ;
#10340 = DIRECTION ( 'NONE',  ( 0.000000000000000000, -1.000000000000000000, 0.000000000000000000 ) ) ;
#10341 = DIRECTION ( 'NONE',  ( 0.7071067811865486830, -0.7071067811865464625, -0.000000000000000000 ) ) ;
#10342 = LINE ( 'NONE', #132162, #55725 ) ;
#10343 = CARTESIAN_POINT ( 'NONE',  ( 117.9795968585647898, 6.109999999999999432, 1.637169565754164280 ) ) ;
#10344 = EDGE_CURVE ( 'NONE', #69819, #40894, #54240, .T. ) ;
#10345 = ORIENTED_EDGE ( 'NONE', *, *, #3389, .F. ) ;
#10346 = DIRECTION ( 'NONE',  ( -0.6830127018922181881, 0.6830127018922202975, -0.2588190451025214056 ) ) ;
#10347 = CARTESIAN_POINT ( 'NONE',  ( 0.000000000000000000, 8.616843969807042924, 0.000000000000000000 ) ) ;
#10348 = CARTESIAN_POINT ( 'NONE',  ( -72.18398860626899705, 28.73617430169837661, 5.000000000000000000 ) ) ;
#10349 = DIRECTION ( 'NONE',  ( 0.7071067811865487940, 0.7071067811865463515, 0.000000000000000000 ) ) ;
#10350 = DIRECTION ( 'NONE',  ( 0.6830127018922181881, 0.6830127018922202975, -0.2588190451025214056 ) ) ;
#10351 = PLANE ( 'NONE',  #2805 ) ;
#10352 = DIRECTION ( 'NONE',  ( -0.5735764363510501562, 0.8191520442889890230, 1.003171929053521419E-16 ) ) ;
#10353 = CARTESIAN_POINT ( 'NONE',  ( 53.45419371712956291, 6.884901960086283523, 3.975000000000002753 ) ) ;
#10354 = DIRECTION ( 'NONE',  ( -1.000000000000000000, -0.000000000000000000, -0.000000000000000000 ) ) ;
#10355 = DIRECTION ( 'NONE',  ( 0.6830127018922180770, -0.6830127018922204085, -0.2588190451025213501 ) ) ;
#10356 = ORIENTED_EDGE ( 'NONE', *, *, #35545, .F. ) ;
#10357 = EDGE_LOOP ( 'NONE', ( #86504, #143092, #33034, #35321 ) ) ;
#10358 = CARTESIAN_POINT ( 'NONE',  ( 41.97916666666665719, -7.950000000000001066, 2.130196079827424427 ) ) ;
#10359 = PLANE ( 'NONE',  #18387 ) ;
#10360 = CARTESIAN_POINT ( 'NONE',  ( -21.71230993966013045, -21.73547319004781642, 4.999917730833664642 ) ) ;
#10361 = EDGE_LOOP ( 'NONE', ( #120112, #35094, #135684, #973 ) ) ;
#10362 = CARTESIAN_POINT ( 'NONE',  ( -57.48921356237308800, -27.52281430457095368, 5.000000000000000000 ) ) ;
#10363 = AXIS2_PLACEMENT_3D ( 'NONE', #136323, #80547, #1501 ) ;
#10364 = PLANE ( 'NONE',  #134922 ) ;
#10365 = CARTESIAN_POINT ( 'NONE',  ( 43.45876352523143993, 0.000000000000000000, -6.110000000000001208 ) ) ;
#10366 = EDGE_CURVE ( 'NONE', #100225, #25077, #79201, .T. ) ;
#10367 = EDGE_LOOP ( 'NONE', ( #43209, #24044, #88520, #29531 ) ) ;
#10368 = CARTESIAN_POINT ( 'NONE',  ( 0.000000000000000000, -40.42999999999999261, 19.06900128115122328 ) ) ;
#10369 = ORIENTED_EDGE ( 'NONE', *, *, #99875, .F. ) ;
#10370 = EDGE_LOOP ( 'NONE', ( #49945, #2289, #140449, #43550 ) ) ;
#10371 = PLANE ( 'NONE',  #49274 ) ;
#10372 = DIRECTION ( 'NONE',  ( -0.000000000000000000, 0.3543493200069153248, 0.9351131265310292928 ) ) ;
#10373 = CARTESIAN_POINT ( 'NONE',  ( 38.99451991528749062, 28.92564299267965211, 4.000000000000000000 ) ) ;
#10374 = FACE_OUTER_BOUND ( 'NONE', #42228, .T. ) ;
#10376 = EDGE_CURVE ( 'NONE', #72906, #90062, #1553, .T. ) ;
#10375 = EDGE_LOOP ( 'NONE', ( #24516, #40006, #62879, #59263 ) ) ;
#10377 = FACE_OUTER_BOUND ( 'NONE', #140458, .T. ) ;
#10378 = DIRECTION ( 'NONE',  ( 0.3543493200069162685, -0.000000000000000000, -0.9351131265310288487 ) ) ;
#10380 = ORIENTED_EDGE ( 'NONE', *, *, #55966, .T. ) ;
#10379 = CARTESIAN_POINT ( 'NONE',  ( 9.816639616203772789, -1.633150327867681995, -6.094999999999993534 ) ) ;
#10381 = CARTESIAN_POINT ( 'NONE',  ( 81.95876352523143282, 0.000000000000000000, -6.110000000000001208 ) ) ;
#10382 = EDGE_CURVE ( 'NONE', #77649, #65242, #90017, .T. ) ;
#10383 = CARTESIAN_POINT ( 'NONE',  ( -23.99999999999983302, -21.03360074219752462, 5.000000000000000000 ) ) ;
#10384 = FILL_AREA_STYLE ('',( #90093 ) ) ;
#10385 =( NAMED_UNIT ( * ) PLANE_ANGLE_UNIT ( ) SI_UNIT ( $, .RADIAN. ) );
#10386 = CARTESIAN_POINT ( 'NONE',  ( -11.27718569542934191, -21.72500000000000853, 5.000000000000000000 ) ) ;
#10387 = AXIS2_PLACEMENT_3D ( 'NONE', #118030, #52788, #74589 ) ;
#10388 = EDGE_LOOP ( 'NONE', ( #118476, #139274, #136707, #31168 ) ) ;
#10389 = LINE ( 'NONE', #936, #54614 ) ;
#10390 = CARTESIAN_POINT ( 'NONE',  ( 67.87043019189812298, -3.055000000000001492, 5.291415217122917625 ) ) ;
#10391 = AXIS2_PLACEMENT_3D ( 'NONE', #90434, #134683, #100612 ) ;
#10392 = CARTESIAN_POINT ( 'NONE',  ( -27.48921356237309155, -27.52281430457074762, 5.000000000000000000 ) ) ;
#10393 = DIRECTION ( 'NONE',  ( 0.7071067811865486830, -0.7071067811865464625, -0.000000000000000000 ) ) ;
#10394 = DIRECTION ( 'NONE',  ( -0.000000000000000000, 0.000000000000000000, 1.000000000000000000 ) ) ;
#10395 = VERTEX_POINT ( 'NONE', #12457 ) ;
#10396 = ORIENTED_EDGE ( 'NONE', *, *, #135348, .F. ) ;
#10397 = LINE ( 'NONE', #42359, #53835 ) ;
#10398 = EDGE_LOOP ( 'NONE', ( #50520, #116823, #110041, #107520 ) ) ;
#10399 = EDGE_CURVE ( 'NONE', #51683, #25180, #56011, .T. ) ;
#10400 = VERTEX_POINT ( 'NONE', #100901 ) ;
#10401 = VECTOR ( 'NONE', #75274, 999.9999999999998863 ) ;
#10402 = FACE_OUTER_BOUND ( 'NONE', #1182, .T. ) ;
#10403 = VERTEX_POINT ( 'NONE', #132856 ) ;
#10404 = CARTESIAN_POINT ( 'NONE',  ( -13.49999999999991118, -5.568876922607754132, 4.000000000000000000 ) ) ;
#10405 = DIRECTION ( 'NONE',  ( -0.000000000000000000, -0.3543493200069152693, 0.9351131265310292928 ) ) ;
#10406 = DIRECTION ( 'NONE',  ( -0.3543493200069162685, -0.000000000000000000, -0.9351131265310288487 ) ) ;
#10407 = FACE_BOUND ( 'NONE', #76784, .T. ) ;
#10408 = CARTESIAN_POINT ( 'NONE',  ( 0.000000000000000000, 0.000000000000000000, 5.000000000000000000 ) ) ;
#10409 = CARTESIAN_POINT ( 'NONE',  ( 41.35002705046289151, -5.819803920172573086, -5.819803920172573086 ) ) ;
#10410 = CARTESIAN_POINT ( 'NONE',  ( -28.49999999999980460, 8.319652575858361487, -8.582050562765893176 ) ) ;
#10412 = ORIENTED_EDGE ( 'NONE', *, *, #94496, .F. ) ;
#10411 = DIRECTION ( 'NONE',  ( 0.7071067811865486830, -0.7071067811865464625, -0.000000000000000000 ) ) ;
#10413 = CARTESIAN_POINT ( 'NONE',  ( 23.20710678118638626, -8.240707523384200428, 5.000000000000000000 ) ) ;
#10414 = AXIS2_PLACEMENT_3D ( 'NONE', #79433, #33064, #109863 ) ;
#10415 = ORIENTED_EDGE ( 'NONE', *, *, #68268, .T. ) ;
#10416 = VECTOR ( 'NONE', #56168, 999.9999999999998863 ) ;
#10419 = ORIENTED_EDGE ( 'NONE', *, *, #128655, .F. ) ;
#10418 = EDGE_CURVE ( 'NONE', #101520, #136399, #80603, .T. ) ;
#10417 = AXIS2_PLACEMENT_3D ( 'NONE', #114412, #59356, #138316 ) ;
#10420 = CARTESIAN_POINT ( 'NONE',  ( 70.78709685856478018, 3.054999999999997495, 5.291415217122919401 ) ) ;
#10421 = ORIENTED_EDGE ( 'NONE', *, *, #27291, .F. ) ;
#10422 = CARTESIAN_POINT ( 'NONE',  ( -10.49999999999991829, -7.912538124160678699, 4.000000000000000000 ) ) ;
#10423 = VECTOR ( 'NONE', #113112, 1000.000000000000000 ) ;
#10424 = FACE_OUTER_BOUND ( 'NONE', #65480, .T. ) ;
#10425 = EDGE_CURVE ( 'NONE', #6529, #7602, #33544, .T. ) ;
#10426 = VERTEX_POINT ( 'NONE', #69017 ) ;
#10427 = CARTESIAN_POINT ( 'NONE',  ( 0.000000000000000000, -43.14999999999999147, -31.92499999999998295 ) ) ;
#10428 = ADVANCED_FACE ( 'NONE', ( #22596 ), #121920, .F. ) ;
#10429 = EDGE_CURVE ( 'NONE', #79752, #25013, #40149, .T. ) ;
#10430 = DIRECTION ( 'NONE',  ( -0.000000000000000000, 0.3543493200069152138, -0.9351131265310292928 ) ) ;
#10431 = CARTESIAN_POINT ( 'NONE',  ( 24.15612307739224818, -22.22500000000000142, 4.000000000000000000 ) ) ;
#10432 = CARTESIAN_POINT ( 'NONE',  ( 72.18398860626899705, 28.73617430169837661, 5.000000000000000000 ) ) ;
#10433 = DIRECTION ( 'NONE',  ( -0.000000000000000000, -0.3543493200069152693, 0.9351131265310292928 ) ) ;
#10434 = CARTESIAN_POINT ( 'NONE',  ( 9.328169399223474656, 11.25929247661560595, 4.000000000000000000 ) ) ;
#10435 = CARTESIAN_POINT ( 'NONE',  ( 17.53839644629417904, -9.740707523384184441, 17.74957260769615175 ) ) ;
#10436 = DIRECTION ( 'NONE',  ( 0.7071067811865487940, 0.7071067811865463515, 0.000000000000000000 ) ) ;
#10437 = ORIENTED_EDGE ( 'NONE', *, *, #68622, .F. ) ;
#10438 = VERTEX_POINT ( 'NONE', #58894 ) ;
#10439 = PLANE ( 'NONE',  #21790 ) ;
#10440 = CARTESIAN_POINT ( 'NONE',  ( 25.39999999999999858, -43.14999999999999147, -40.92499999999998295 ) ) ;
#10441 = EDGE_LOOP ( 'NONE', ( #17108, #137049, #40856, #114312 ) ) ;
#10442 = ORIENTED_EDGE ( 'NONE', *, *, #71252, .F. ) ;
#10443 = EDGE_CURVE ( 'NONE', #75102, #60630, #48676, .T. ) ;
#10444 = EDGE_CURVE ( 'NONE', #32455, #36309, #114620, .T. ) ;
#10445 = CARTESIAN_POINT ( 'NONE',  ( 35.72959685856474721, -6.110000000000000320, -1.637169565754161393 ) ) ;
#10446 = VERTEX_POINT ( 'NONE', #71878 ) ;
#10447 = CARTESIAN_POINT ( 'NONE',  ( -21.70710678118638981, 17.25929247661554911, 5.000000000000000000 ) ) ;
#10448 = DIRECTION ( 'NONE',  ( -0.7071067811865487940, 0.7071067811865463515, -0.000000000000000000 ) ) ;
#10449 = CARTESIAN_POINT ( 'NONE',  ( 26.87913961620377634, -5.278424836066145431, -3.047499999999993658 ) ) ;
#10450 = CARTESIAN_POINT ( 'NONE',  ( 9.461405300130673268, 9.830979504677589631, -29.00227189367402048 ) ) ;
#10451 = ADVANCED_FACE ( 'NONE', ( #15998 ), #26213, .F. ) ;
#10452 = VERTEX_POINT ( 'NONE', #94303 ) ;
#10453 = DIRECTION ( 'NONE',  ( -0.7071067811865486830, -0.7071067811865464625, 0.000000000000000000 ) ) ;
#10454 = ORIENTED_EDGE ( 'NONE', *, *, #5562, .F. ) ;
#10455 = LINE ( 'NONE', #33682, #4758 ) ;
#10456 = CARTESIAN_POINT ( 'NONE',  ( 30.18398860626900060, 28.73617430169808173, 5.000000000000000000 ) ) ;
#10457 = EDGE_CURVE ( 'NONE', #140051, #124154, #83450, .T. ) ;
#10459 = ORIENTED_EDGE ( 'NONE', *, *, #41042, .T. ) ;
#10458 = CARTESIAN_POINT ( 'NONE',  ( 22.49999999999984013, 1.030536316426532872, -5.498701923753849918 ) ) ;
#10460 = ORIENTED_EDGE ( 'NONE', *, *, #128798, .T. ) ;
#10461 = DIRECTION ( 'NONE',  ( -1.000000000000000000, -1.224606353822377258E-16, -0.000000000000000000 ) ) ;
#10462 = DIRECTION ( 'NONE',  ( -1.000000000000000000, -0.000000000000000000, -0.000000000000000000 ) ) ;
#10463 = LINE ( 'NONE', #85173, #47120 ) ;
#10464 = VERTEX_POINT ( 'NONE', #61712 ) ;
#10465 = FACE_OUTER_BOUND ( 'NONE', #52489, .T. ) ;
#10466 = ORIENTED_EDGE ( 'NONE', *, *, #24952, .F. ) ;
#10467 = ORIENTED_EDGE ( 'NONE', *, *, #10741, .T. ) ;
#10468 = LINE ( 'NONE', #64170, #95729 ) ;
#10469 = LINE ( 'NONE', #17256, #41768 ) ;
#10470 = EDGE_CURVE ( 'NONE', #70129, #786, #14579, .T. ) ;
#10471 = DIRECTION ( 'NONE',  ( 0.000000000000000000, -1.000000000000000000, 0.000000000000000000 ) ) ;
#10472 = CARTESIAN_POINT ( 'NONE',  ( -51.48921356237309510, -27.52281430457091460, 5.000000000000000000 ) ) ;
#10473 = DIRECTION ( 'NONE',  ( 0.000000000000000000, 0.000000000000000000, -1.000000000000000000 ) ) ;
#10474 = CARTESIAN_POINT ( 'NONE',  ( 0.4892135623730947680, -27.52281430457055578, 5.000000000000000000 ) ) ;
#10475 = DIRECTION ( 'NONE',  ( 0.000000000000000000, 0.000000000000000000, -1.000000000000000000 ) ) ;
#10476 = VERTEX_POINT ( 'NONE', #28356 ) ;
#10477 = CARTESIAN_POINT ( 'NONE',  ( 12.40000000000000213, -2.055000000000000160, 2.789133085058098087E-16 ) ) ;
#10478 = EDGE_CURVE ( 'NONE', #31980, #69883, #31123, .T. ) ;
#10479 = ORIENTED_EDGE ( 'NONE', *, *, #109268, .F. ) ;
#10480 = CARTESIAN_POINT ( 'NONE',  ( -0.1804868739969447966, -22.22500000000000142, 18.16599484154716393 ) ) ;
#10481 = EDGE_CURVE ( 'NONE', #109128, #124649, #3691, .T. ) ;
#10482 = CARTESIAN_POINT ( 'NONE',  ( 24.24169458425172508, 0.7592924766157138627, 14.37146558664977114 ) ) ;
#10483 = AXIS2_PLACEMENT_3D ( 'NONE', #5375, #138790, #107559 ) ;
#10484 = CARTESIAN_POINT ( 'NONE',  ( 50.99451991528749062, 28.92564299267973738, 4.000000000000000000 ) ) ;
#10485 = ORIENTED_EDGE ( 'NONE', *, *, #132062, .F. ) ;
#10486 = PLANE ( 'NONE',  #25198 ) ;
#10487 = DIRECTION ( 'NONE',  ( -0.000000000000000000, 0.3543493200069153248, 0.9351131265310292928 ) ) ;
#10488 = LINE ( 'NONE', #88078, #2817 ) ;
#10489 = EDGE_LOOP ( 'NONE', ( #142556, #33169, #22017, #66303 ) ) ;
#10490 = VECTOR ( 'NONE', #110578, 1000.000000000000000 ) ;
#10491 = ORIENTED_EDGE ( 'NONE', *, *, #49754, .F. ) ;
#10492 = CARTESIAN_POINT ( 'NONE',  ( 55.28643332384051945, -49.19207878844169812, 41.22112633374686652 ) ) ;
#10493 = CARTESIAN_POINT ( 'NONE',  ( -29.99999999999977973, 5.587461875839189851, 4.000000000000000000 ) ) ;
#10494 = CARTESIAN_POINT ( 'NONE',  ( 15.96626304157554266, -2.055000000000000160, 2.789133085058097101E-16 ) ) ;
#10495 = CARTESIAN_POINT ( 'NONE',  ( 51.74999999999999289, -9.735942053221458872E-16, 7.950000000000000178 ) ) ;
#10496 = EDGE_CURVE ( 'NONE', #76190, #2459, #38513, .T. ) ;
#10497 = CARTESIAN_POINT ( 'NONE',  ( 22.89835756248665888, 7.738675393078206177, 4.667276354320995857 ) ) ;
#10498 = CARTESIAN_POINT ( 'NONE',  ( 66.99543019189812298, 5.291415217122917625, 3.055000000000002380 ) ) ;
#10499 = FACE_OUTER_BOUND ( 'NONE', #66353, .T. ) ;
#10500 = AXIS2_PLACEMENT_3D ( 'NONE', #4946, #28184, #6366 ) ;
#10501 = CARTESIAN_POINT ( 'NONE',  ( 36.48921356237310221, -27.52281430457080802, 5.000000000000000000 ) ) ;
#10502 = CARTESIAN_POINT ( 'NONE',  ( 84.12500000000000000, -7.950000000000000178, -4.867971026610729436E-16 ) ) ;
#10503 = ORIENTED_EDGE ( 'NONE', *, *, #49153, .T. ) ;
#10504 = CARTESIAN_POINT ( 'NONE',  ( 1.199999999999999956, -0.5999999999999993117, -4.750000000000000000 ) ) ;
#10505 = ORIENTED_EDGE ( 'NONE', *, *, #52305, .T. ) ;
#10506 = DIRECTION ( 'NONE',  ( 0.7071067811865487940, -0.7071067811865463515, 0.000000000000000000 ) ) ;
#10507 = DIRECTION ( 'NONE',  ( 0.7071067811865487940, -0.7071067811865463515, 0.000000000000000000 ) ) ;
#10508 = CARTESIAN_POINT ( 'NONE',  ( 34.92499999999998295, -10.29806943317891310, 4.500000000000000888 ) ) ;
#10509 = CARTESIAN_POINT ( 'NONE',  ( 7.499999999999945821, -15.29013452822854013, 0.3645803511610531400 ) ) ;
#10510 = DIRECTION ( 'NONE',  ( 0.7071067811865486830, -0.7071067811865464625, -0.000000000000000000 ) ) ;
#10511 = LINE ( 'NONE', #43890, #60286 ) ;
#10512 = DIRECTION ( 'NONE',  ( -0.5735764363510499342, -0.8191520442889891340, 0.000000000000000000 ) ) ;
#10513 = ORIENTED_EDGE ( 'NONE', *, *, #40898, .F. ) ;
#10514 = ORIENTED_EDGE ( 'NONE', *, *, #7805, .T. ) ;
#10515 = CARTESIAN_POINT ( 'NONE',  ( -12.20000000000000462, -21.76999999999999247, -40.00000000000000000 ) ) ;
#10516 = FILL_AREA_STYLE_COLOUR ( '', #118530 ) ;
#10517 = CARTESIAN_POINT ( 'NONE',  ( 26.99999999999981171, -16.06887692260765377, 4.000000000000000000 ) ) ;
#10518 = STYLED_ITEM ( 'NONE', ( #99147 ), #120916 ) ;
#10519 = FACE_OUTER_BOUND ( 'NONE', #56120, .T. ) ;
#10520 = CARTESIAN_POINT ( 'NONE',  ( 88.16252705046289861, 7.949999999999998401, 1.460391307983218338E-15 ) ) ;
#10521 = VECTOR ( 'NONE', #55150, 1000.000000000000000 ) ;
#10522 = CARTESIAN_POINT ( 'NONE',  ( -25.39999999999996305, 3.061616997868383141E-16, -2.500000000000000000 ) ) ;
#10523 = ORIENTED_EDGE ( 'NONE', *, *, #49564, .F. ) ;
#10524 = CARTESIAN_POINT ( 'NONE',  ( 86.02083333333330017, 7.949999999999999289, 2.130196079827431532 ) ) ;
#10525 = AXIS2_PLACEMENT_3D ( 'NONE', #106353, #38290, #140441 ) ;
#10526 = FACE_OUTER_BOUND ( 'NONE', #100809, .T. ) ;
#10527 = EDGE_CURVE ( 'NONE', #126051, #90340, #92151, .T. ) ;
#10528 = CARTESIAN_POINT ( 'NONE',  ( -0.7586007421979610310, 21.72500000000000853, 5.000000000000000000 ) ) ;
#10529 = FACE_OUTER_BOUND ( 'NONE', #62223, .T. ) ;
#10530 = AXIS2_PLACEMENT_3D ( 'NONE', #88097, #130907, #96093 ) ;
#10531 = ORIENTED_EDGE ( 'NONE', *, *, #138838, .F. ) ;
#10532 = DIRECTION ( 'NONE',  ( 0.000000000000000000, -1.000000000000000000, 0.000000000000000000 ) ) ;
#10533 = VERTEX_POINT ( 'NONE', #137111 ) ;
#10534 = CARTESIAN_POINT ( 'NONE',  ( 74.52126352523141861, -4.472830434245839371, -4.472830434245840259 ) ) ;
#10535 = DIRECTION ( 'NONE',  ( -0.5735764363510507113, 0.8191520442889885789, 1.003171929053520926E-16 ) ) ;
#10536 = ORIENTED_EDGE ( 'NONE', *, *, #26376, .F. ) ;
#10537 = DIRECTION ( 'NONE',  ( -0.7071067811865487940, 0.7071067811865463515, 0.000000000000000000 ) ) ;
#10538 = LINE ( 'NONE', #76562, #45251 ) ;
#10539 = LINE ( 'NONE', #64238, #51204 ) ;
#10540 = CARTESIAN_POINT ( 'NONE',  ( -42.48921356237308800, -27.52281430457085065, 5.000000000000000000 ) ) ;
#10541 = EDGE_CURVE ( 'NONE', #100628, #10464, #125531, .T. ) ;
#10542 = CARTESIAN_POINT ( 'NONE',  ( 16.17183060077635659, -8.240707523384191546, 4.000000000000000000 ) ) ;
#10544 = ORIENTED_EDGE ( 'NONE', *, *, #3551, .T. ) ;
#10543 = DIRECTION ( 'NONE',  ( -1.000000000000000000, -1.224606353822377258E-16, -0.000000000000000000 ) ) ;
#10545 =( REPRESENTATION_RELATIONSHIP ('NONE','NONE', #69070, #58954 ) REPRESENTATION_RELATIONSHIP_WITH_TRANSFORMATION ( #95296 )SHAPE_REPRESENTATION_RELATIONSHIP( ) );
#10546 = EDGE_CURVE ( 'NONE', #119594, #104026, #129789, .T. ) ;
#10547 = DIRECTION ( 'NONE',  ( -0.7071067811865486830, -0.7071067811865464625, 0.000000000000000000 ) ) ;
#10548 = CARTESIAN_POINT ( 'NONE',  ( 2.206660635421510808, 21.75929247661549937, 4.998822639870701856 ) ) ;
#10549 = LINE ( 'NONE', #30175, #79550 ) ;
#10550 = CARTESIAN_POINT ( 'NONE',  ( 23.99451991528749062, 28.92564299267954908, 4.000000000000000000 ) ) ;
#10551 = VERTEX_POINT ( 'NONE', #108007 ) ;
#10552 = ORIENTED_EDGE ( 'NONE', *, *, #37843, .T. ) ;
#10553 = CARTESIAN_POINT ( 'NONE',  ( 61.83376352523143993, 6.110000000000001208, 1.122388791418549305E-15 ) ) ;
#10554 = ORIENTED_EDGE ( 'NONE', *, *, #86393, .F. ) ;
#10555 = EDGE_CURVE ( 'NONE', #22333, #126257, #117464, .T. ) ;
#10556 = DIRECTION ( 'NONE',  ( -0.7071067811865487940, 0.7071067811865463515, 0.000000000000000000 ) ) ;
#10557 = DIRECTION ( 'NONE',  ( 1.000000000000000000, 1.224606353822377258E-16, 0.000000000000000000 ) ) ;
#10558 = DIRECTION ( 'NONE',  ( 1.000000000000000000, 0.000000000000000000, 0.000000000000000000 ) ) ;
#10559 = CARTESIAN_POINT ( 'NONE',  ( -54.29974487139159578, -27.71228299555243879, 4.000000000000000000 ) ) ;
#10560 = EDGE_LOOP ( 'NONE', ( #80056, #63729, #50043 ) ) ;
#10561 = ORIENTED_EDGE ( 'NONE', *, *, #99922, .T. ) ;
#10562 = DIRECTION ( 'NONE',  ( 0.7071067811865487940, 0.7071067811865463515, 0.000000000000000000 ) ) ;
#10563 = FACE_OUTER_BOUND ( 'NONE', #68307, .T. ) ;
#10564 = EDGE_CURVE ( 'NONE', #92065, #115116, #7992, .T. ) ;
#10565 = EDGE_LOOP ( 'NONE', ( #4504, #12413, #117626, #2283 ) ) ;
#10566 = PLANE ( 'NONE',  #125301 ) ;
#10567 = LINE ( 'NONE', #30195, #68717 ) ;
#10568 = PLANE ( 'NONE',  #60914 ) ;
#10569 = EDGE_CURVE ( 'NONE', #19998, #51146, #142127, .T. ) ;
#10570 = EDGE_LOOP ( 'NONE', ( #114052, #35978, #38792, #54289, #40878 ) ) ;
#10571 = PLANE ( 'NONE',  #133350 ) ;
#10572 = CARTESIAN_POINT ( 'NONE',  ( -30.81246187583926144, -22.22500000000000142, 4.000000000000000000 ) ) ;
#10573 = LINE ( 'NONE', #99018, #25806 ) ;
#10574 = CARTESIAN_POINT ( 'NONE',  ( 18.79996877983152004, 8.259292476615627265, 16.85664084051836653 ) ) ;
#10575 = ADVANCED_FACE ( 'NONE', ( #63148 ), #10149, .F. ) ;
#10576 = CARTESIAN_POINT ( 'NONE',  ( -2.004924772211924555, -5.240707523384228850, 12.38332538355496659 ) ) ;
#10577 = LINE ( 'NONE', #122200, #14165 ) ;
#10579 = ORIENTED_EDGE ( 'NONE', *, *, #31781, .T. ) ;
#10578 = VECTOR ( 'NONE', #139878, 1000.000000000000000 ) ;
#10580 = EDGE_LOOP ( 'NONE', ( #64730, #52049, #42568, #121371 ) ) ;
#10581 = CARTESIAN_POINT ( 'NONE',  ( 114.0995968585647518, -6.109999999999997655, -1.637169565754160283 ) ) ;
#10582 = EDGE_LOOP ( 'NONE', ( #101397, #38925, #88341, #19055, #102491, #97567, #29044, #141985, #116303, #17522, #16778, #44898, #44800, #123154, #34916, #94424, #27459, #87782, #127810, #43765, #25069, #120980, #75999, #72239, #43384, #5614, #93405, #82117, #142793, #74385, #99692, #19701, #103530, #113281, #11066, #111155, #129531, #46274, #5459, #92133, #13474, #85217, #58092, #124606, #25024, #75160, #47981, #72176, #58743, #41887, #67165, #47928, #116733, #55917, #68212, #129910, #119038, #39495, #51690, #76774, #7472, #11734, #68497, #137032, #9127, #129493, #107767, #105785, #30850, #52116, #64340, #117701, #11095, #26862, #101731, #34594, #46324, #141723, #22457, #44051, #34386, #34712, #20469, #15879, #49036, #54406 ) ) ;
#10583 = VECTOR ( 'NONE', #94198, 1000.000000000000000 ) ;
#10584 = EDGE_LOOP ( 'NONE', ( #110614, #17892, #101559, #141735, #99028 ) ) ;
#10585 = EDGE_CURVE ( 'NONE', #57697, #134155, #29751, .T. ) ;
#10586 = CARTESIAN_POINT ( 'NONE',  ( 183.6687791239614569, -49.11951764990740088, 40.13200514437710353 ) ) ;
#10587 =( BOUNDED_CURVE ( )  B_SPLINE_CURVE ( 3, ( #38517, #28363, #82741, #117470 ),
 .UNSPECIFIED., .F., .F. ) 
 B_SPLINE_CURVE_WITH_KNOTS ( ( 4, 4 ),
 ( 4.350170835173026163, 4.500739107949217832 ),
 .UNSPECIFIED. ) 
 CURVE ( )  GEOMETRIC_REPRESENTATION_ITEM ( )  RATIONAL_B_SPLINE_CURVE ( ( 1.000000000000000000, 0.9981116584018955296, 0.9981116584018955296, 1.000000000000000000 ) ) 
 REPRESENTATION_ITEM ( '' )  );
#10588 = DIRECTION ( 'NONE',  ( -0.7071067811865487940, 0.7071067811865463515, -0.000000000000000000 ) ) ;
#10589 = EDGE_CURVE ( 'NONE', #19670, #391, #8675, .T. ) ;
#10590 = EDGE_CURVE ( 'NONE', #100722, #20115, #42813, .T. ) ;
#10591 = DIRECTION ( 'NONE',  ( 0.7071067811865487940, 0.7071067811865463515, 0.000000000000000000 ) ) ;
#10592 = ORIENTED_EDGE ( 'NONE', *, *, #62319, .T. ) ;
#10593 = CYLINDRICAL_SURFACE ( 'NONE', #73734, 2.500000000000000000 ) ;
#10594 = DIRECTION ( 'NONE',  ( 0.7071067811865486830, 0.7071067811865464625, 0.000000000000000000 ) ) ;
#10595 = CARTESIAN_POINT ( 'NONE',  ( 36.72916666666665719, 7.950000000000001954, -2.130196079827421762 ) ) ;
#10596 = AXIS2_PLACEMENT_3D ( 'NONE', #137744, #115212, #26115 ) ;
#10598 = CARTESIAN_POINT ( 'NONE',  ( -12.20000000000000284, -27.68200100598810209, 15.59110741220538188 ) ) ;
#10597 = DIRECTION ( 'NONE',  ( -0.7071067811865486830, -0.7071067811865464625, 0.000000000000000000 ) ) ;
#10599 = FACE_OUTER_BOUND ( 'NONE', #16902, .T. ) ;
#10600 = CARTESIAN_POINT ( 'NONE',  ( 25.97159235450331849, 9.902892378096218942E-16, 0.000000000000000000 ) ) ;
#10601 = ORIENTED_EDGE ( 'NONE', *, *, #49128, .F. ) ;
#10602 = ADVANCED_FACE ( 'NONE', ( #19600 ), #30852, .T. ) ;
#10603 = CARTESIAN_POINT ( 'NONE',  ( 29.99999999999979750, 14.87792677143811737, -11.06722581663433225 ) ) ;
#10604 = DIRECTION ( 'NONE',  ( 1.000000000000000000, 0.000000000000000000, 0.000000000000000000 ) ) ;
#10605 = ORIENTED_EDGE ( 'NONE', *, *, #39758, .T. ) ;
#10606 = ORIENTED_EDGE ( 'NONE', *, *, #125426, .T. ) ;
#10607 = EDGE_CURVE ( 'NONE', #42048, #49753, #31212, .T. ) ;
#10609 = ORIENTED_EDGE ( 'NONE', *, *, #91714, .T. ) ;
#10608 = EDGE_CURVE ( 'NONE', #108642, #13817, #119603, .T. ) ;
#10610 = CARTESIAN_POINT ( 'NONE',  ( 65.77126352523143282, 4.472830434245838482, 4.472830434245842035 ) ) ;
#10611 = ORIENTED_EDGE ( 'NONE', *, *, #132692, .F. ) ;
#10612 = VECTOR ( 'NONE', #46264, 999.9999999999998863 ) ;
#10613 = DIRECTION ( 'NONE',  ( 0.7071067811865487940, 0.7071067811865463515, -0.000000000000000000 ) ) ;
#10614 = AXIS2_PLACEMENT_3D ( 'NONE', #55342, #110393, #131468 ) ;
#10615 = CARTESIAN_POINT ( 'NONE',  ( 1.212472949537106048, 0.000000000000000000, 6.094999999999989981 ) ) ;
#10616 = CARTESIAN_POINT ( 'NONE',  ( 103.8337635252314328, 6.110000000000001208, 1.122388791418549305E-15 ) ) ;
#10617 = LINE ( 'NONE', #54884, #3119 ) ;
#10618 = CIRCLE ( 'NONE', #91673, 6.499999999999999112 ) ;
#10619 = EDGE_CURVE ( 'NONE', #86643, #114851, #87005, .T. ) ;
#10620 = AXIS2_PLACEMENT_3D ( 'NONE', #103607, #36251, #58764 ) ;
#10621 = ORIENTED_EDGE ( 'NONE', *, *, #136431, .T. ) ;
#10622 = LINE ( 'NONE', #132472, #111178 ) ;
#10623 = AXIS2_PLACEMENT_3D ( 'NONE', #1412, #53704, #100759 ) ;
#10624 = ADVANCED_FACE ( 'NONE', ( #62420 ), #42100, .T. ) ;
#10625 = DIRECTION ( 'NONE',  ( -0.7071067811865487940, 0.7071067811865463515, 0.000000000000000000 ) ) ;
#10626 = DIRECTION ( 'NONE',  ( 1.000000000000000000, 1.224606353822377258E-16, 0.000000000000000000 ) ) ;
#10627 = CARTESIAN_POINT ( 'NONE',  ( 12.29974487139158512, -27.71228299555214747, 4.000000000000000000 ) ) ;
#10628 = ORIENTED_EDGE ( 'NONE', *, *, #19186, .T. ) ;
#10629 = CARTESIAN_POINT ( 'NONE',  ( 34.92499999999998295, 1.800094516027155755, 4.759050581649325373 ) ) ;
#10630 = ORIENTED_EDGE ( 'NONE', *, *, #39621, .T. ) ;
#10631 = ORIENTED_EDGE ( 'NONE', *, *, #105264, .F. ) ;
#10632 = ORIENTED_EDGE ( 'NONE', *, *, #136286, .T. ) ;
#10633 = CARTESIAN_POINT ( 'NONE',  ( 125.4745968585647944, 1.637169565754164280, -6.109999999999996767 ) ) ;
#10634 = ORIENTED_EDGE ( 'NONE', *, *, #4816, .F. ) ;
#10635 = DIRECTION ( 'NONE',  ( 0.7071067811865486830, -0.7071067811865464625, -0.000000000000000000 ) ) ;
#10636 = PLANE ( 'NONE',  #108777 ) ;
#10637 = ORIENTED_EDGE ( 'NONE', *, *, #56706, .F. ) ;
#10638 = PLANE ( 'NONE',  #132192 ) ;
#10639 = ORIENTED_EDGE ( 'NONE', *, *, #124402, .F. ) ;
#10640 = EDGE_CURVE ( 'NONE', #57341, #46950, #109472, .T. ) ;
#10641 = ADVANCED_FACE ( 'NONE', ( #74732 ), #130533, .F. ) ;
#10642 = CARTESIAN_POINT ( 'NONE',  ( 9.895403141435220817, 2.126176841940962348, 7.934999999999989839 ) ) ;
#10643 = CARTESIAN_POINT ( 'NONE',  ( 33.18398860626899705, 28.73617430169810305, 5.000000000000000000 ) ) ;
#10644 = PLANE ( 'NONE',  #43732 ) ;
#10645 = DIRECTION ( 'NONE',  ( 0.5735764363510451602, 0.8191520442889924647, 0.000000000000000000 ) ) ;
#10646 = VERTEX_POINT ( 'NONE', #53688 ) ;
#10647 = EDGE_LOOP ( 'NONE', ( #83159, #44774 ) ) ;
#10648 = ORIENTED_EDGE ( 'NONE', *, *, #116500, .T. ) ;
#10649 =( NAMED_UNIT ( * ) SI_UNIT ( $, .STERADIAN. ) SOLID_ANGLE_UNIT ( ) );
#10650 = DIRECTION ( 'NONE',  ( 1.000000000000000000, 0.000000000000000000, 0.000000000000000000 ) ) ;
#10651 = AXIS2_PLACEMENT_3D ( 'NONE', #49092, #38907, #82420 ) ;
#10652 = PLANE ( 'NONE',  #70588 ) ;
#10653 = DIRECTION ( 'NONE',  ( -0.7071067811865486830, 0.7071067811865464625, 0.000000000000000000 ) ) ;
#10654 = DIRECTION ( 'NONE',  ( -1.000000000000000000, -1.224606353822377258E-16, -0.000000000000000000 ) ) ;
#10655 = CARTESIAN_POINT ( 'NONE',  ( 31.93793019189809712, -6.110000000000001208, 1.637169565754158951 ) ) ;
#10656 = DIRECTION ( 'NONE',  ( 0.7071067811865486830, -0.7071067811865464625, -0.000000000000000000 ) ) ;
#10657 = LINE ( 'NONE', #99093, #115984 ) ;
#10658 = ORIENTED_EDGE ( 'NONE', *, *, #8135, .T. ) ;
#10659 = CARTESIAN_POINT ( 'NONE',  ( 42.48921356237308800, -27.52281430457085065, 5.000000000000000000 ) ) ;
#10660 = ORIENTED_EDGE ( 'NONE', *, *, #130402, .F. ) ;
#10661 = DIRECTION ( 'NONE',  ( -0.000000000000000000, -0.000000000000000000, -1.000000000000000000 ) ) ;
#10662 = VERTEX_POINT ( 'NONE', #118911 ) ;
#10663 = LINE ( 'NONE', #44808, #131641 ) ;
#10665 = ORIENTED_EDGE ( 'NONE', *, *, #133532, .T. ) ;
#10664 = DIRECTION ( 'NONE',  ( -0.000000000000000000, 0.3543493200069153248, 0.9351131265310292928 ) ) ;
#10666 = LINE ( 'NONE', #19431, #79355 ) ;
#10667 = ORIENTED_EDGE ( 'NONE', *, *, #77054, .F. ) ;
#10668 = LINE ( 'NONE', #133223, #92463 ) ;
#10669 = VERTEX_POINT ( 'NONE', #63846 ) ;
#10670 = DIRECTION ( 'NONE',  ( 0.7071067811865486830, -0.7071067811865464625, -0.000000000000000000 ) ) ;
#10671 = EDGE_LOOP ( 'NONE', ( #41784, #69042, #52389, #71759 ) ) ;
#10672 = DIRECTION ( 'NONE',  ( -0.7071067811865486830, -0.7071067811865464625, -0.000000000000000000 ) ) ;
#10673 = AXIS2_PLACEMENT_3D ( 'NONE', #20594, #121341, #22027 ) ;
#10674 = CARTESIAN_POINT ( 'NONE',  ( 109.8916937171295416, 2.130196079827421762, 7.950000000000001066 ) ) ;
#10675 = CARTESIAN_POINT ( 'NONE',  ( 50.39169371712954870, 2.130196079827421762, 7.950000000000000178 ) ) ;
#10676 = DIRECTION ( 'NONE',  ( -0.000000000000000000, 0.000000000000000000, 1.000000000000000000 ) ) ;
#10677 = VECTOR ( 'NONE', #37540, 1000.000000000000000 ) ;
#10678 = DIRECTION ( 'NONE',  ( 0.7071067811865487940, 0.7071067811865463515, 0.000000000000000000 ) ) ;
#10679 = CARTESIAN_POINT ( 'NONE',  ( 7.940000000000001279, -33.26999999999999602, -10.00000000000000178 ) ) ;
#10680 = EDGE_CURVE ( 'NONE', #17012, #88778, #75428, .T. ) ;
#10681 = CARTESIAN_POINT ( 'NONE',  ( -31.17183060077625001, 3.759292476615681888, 4.000000000000000000 ) ) ;
#10682 = CARTESIAN_POINT ( 'NONE',  ( 11.08333333333333393, -5.278424836066144543, 3.047499999999995879 ) ) ;
#10683 = CARTESIAN_POINT ( 'NONE',  ( 14.85373647476855297, -5.808823158059035485, -5.808823158059033709 ) ) ;
#10684 = CARTESIAN_POINT ( 'NONE',  ( 18.18398860626898994, 28.73617430169800002, 5.000000000000000000 ) ) ;
#10685 = CARTESIAN_POINT ( 'NONE',  ( 17.84878961325748037, 4.584330080086930965E-16, 0.000000000000000000 ) ) ;
#10686 = VERTEX_POINT ( 'NONE', #73996 ) ;
#10687 = ORIENTED_EDGE ( 'NONE', *, *, #87402, .T. ) ;
#10689 = EDGE_CURVE ( 'NONE', #62934, #99425, #51542, .T. ) ;
#10688 = PLANE ( 'NONE',  #86048 ) ;
#10690 = ORIENTED_EDGE ( 'NONE', *, *, #121366, .T. ) ;
#10691 = DIRECTION ( 'NONE',  ( 0.6830127018922181881, 0.6830127018922202975, -0.2588190451025214056 ) ) ;
#10692 = CARTESIAN_POINT ( 'NONE',  ( 7.499999999999951150, -7.533600742197665845, 5.000000000000000000 ) ) ;
#10693 = CARTESIAN_POINT ( 'NONE',  ( 1.629999999999999893, -0.3999999999999997446, -2.303088455023527104 ) ) ;
#10694 = ORIENTED_EDGE ( 'NONE', *, *, #86751, .T. ) ;
#10695 = DIRECTION ( 'NONE',  ( -0.7071067811865487940, 0.7071067811865463515, -0.000000000000000000 ) ) ;
#10696 = DIRECTION ( 'NONE',  ( -1.000000000000000000, -0.000000000000000000, -0.000000000000000000 ) ) ;
#10697 = EDGE_CURVE ( 'NONE', #126057, #2927, #84864, .T. ) ;
#10698 = DIRECTION ( 'NONE',  ( 0.000000000000000000, 0.000000000000000000, -1.000000000000000000 ) ) ;
#10699 = VECTOR ( 'NONE', #83897, 1000.000000000000227 ) ;
#10700 = LINE ( 'NONE', #23001, #108704 ) ;
#10701 = ADVANCED_FACE ( 'NONE', ( #44238 ), #22431, .F. ) ;
#10702 = EDGE_CURVE ( 'NONE', #131451, #98806, #43502, .T. ) ;
#10703 = DIRECTION ( 'NONE',  ( 1.000000000000000000, 0.000000000000000000, 0.000000000000000000 ) ) ;
#10705 = ORIENTED_EDGE ( 'NONE', *, *, #60724, .F. ) ;
#10704 = CARTESIAN_POINT ( 'NONE',  ( 19.49999999999985789, 10.94296225409028089, -9.576120664313208408 ) ) ;
#10706 = SURFACE_SIDE_STYLE ('',( #15515 ) ) ;
#10707 = FILL_AREA_STYLE_COLOUR ( '', #121557 ) ;
#10708 = CARTESIAN_POINT ( 'NONE',  ( 23.32000000000000028, -2.055000000000000160, 2.789133085058098087E-16 ) ) ;
#10709 = CARTESIAN_POINT ( 'NONE',  ( 6.628407645496676714, -2.500000000000000888, 0.000000000000000000 ) ) ;
#10710 = MECHANICAL_DESIGN_GEOMETRIC_PRESENTATION_REPRESENTATION (  '', ( #100976 ), #131102 ) ;
#10711 = CARTESIAN_POINT ( 'NONE',  ( -27.29974487139158512, -27.71228299555225405, 4.000000000000000000 ) ) ;
#10713 = EDGE_CURVE ( 'NONE', #98608, #30859, #57987, .T. ) ;
#10712 = AXIS2_PLACEMENT_3D ( 'NONE', #73543, #98146, #95272 ) ;
#10715 = ADVANCED_FACE ( 'NONE', ( #68163 ), #111620, .T. ) ;
#10714 = ORIENTED_EDGE ( 'NONE', *, *, #112411, .F. ) ;
#10716 = EDGE_LOOP ( 'NONE', ( #18905, #2605, #127381, #47740 ) ) ;
#10717 = ORIENTED_EDGE ( 'NONE', *, *, #49147, .T. ) ;
#10718 = VECTOR ( 'NONE', #28245, 1000.000000000000000 ) ;
#10719 = CARTESIAN_POINT ( 'NONE',  ( 90.41709685856477563, 3.054999999999998828, 5.291415217122922066 ) ) ;
#10720 = ORIENTED_EDGE ( 'NONE', *, *, #130693, .F. ) ;
#10721 = EDGE_CURVE ( 'NONE', #19260, #103619, #57264, .T. ) ;
#10722 = CARTESIAN_POINT ( 'NONE',  ( 131.4501442085630742, -48.99436351328139239, 39.52330221397870247 ) ) ;
#10723 = VECTOR ( 'NONE', #13546, 999.9999999999998863 ) ;
#10724 = CARTESIAN_POINT ( 'NONE',  ( -18.18398860626898994, 28.73617430169800002, 5.000000000000000000 ) ) ;
#10725 = EDGE_LOOP ( 'NONE', ( #124183, #48643, #59309, #124345 ) ) ;
#10726 = DIRECTION ( 'NONE',  ( 0.3543493200069163240, 0.000000000000000000, -0.9351131265310288487 ) ) ;
#10727 = CARTESIAN_POINT ( 'NONE',  ( 48.97916666666665009, -7.950000000000000178, 2.130196079827424427 ) ) ;
#10728 = EDGE_CURVE ( 'NONE', #25602, #56797, #87722, .T. ) ;
#10729 = CARTESIAN_POINT ( 'NONE',  ( 83.76626352523145158, 4.472830434245839371, -4.472830434245838482 ) ) ;
#10730 = ORIENTED_EDGE ( 'NONE', *, *, #10721, .F. ) ;
#10731 = DIRECTION ( 'NONE',  ( -0.000000000000000000, 0.3543493200069153248, 0.9351131265310292928 ) ) ;
#10732 = CARTESIAN_POINT ( 'NONE',  ( 116.0625000000000000, -5.819803920172573086, -5.819803920172573974 ) ) ;
#10733 = EDGE_CURVE ( 'NONE', #128903, #76170, #33384, .T. ) ;
#10734 = EDGE_LOOP ( 'NONE', ( #50005, #68158, #136901 ) ) ;
#10735 = ORIENTED_EDGE ( 'NONE', *, *, #32945, .F. ) ;
#10736 = ORIENTED_EDGE ( 'NONE', *, *, #136700, .F. ) ;
#10737 = DIRECTION ( 'NONE',  ( 0.7071067811865487940, 0.7071067811865463515, 0.000000000000000000 ) ) ;
#10738 = DIRECTION ( 'NONE',  ( -1.000000000000000000, -0.000000000000000000, -0.000000000000000000 ) ) ;
#10739 = CARTESIAN_POINT ( 'NONE',  ( 18.87956980810189123, 3.967499999999998916, 6.871911579029510442 ) ) ;
#10740 = LINE ( 'NONE', #131850, #34947 ) ;
#10741 = EDGE_CURVE ( 'NONE', #126742, #29164, #56576, .T. ) ;
#10742 = CARTESIAN_POINT ( 'NONE',  ( 18.27825451568562443, 8.259292476615637923, 11.78515199841154448 ) ) ;
#10743 = CARTESIAN_POINT ( 'NONE',  ( 18.29974487139159223, -27.71228299555219010, 4.000000000000000000 ) ) ;
#10744 = SHAPE_REPRESENTATION_RELATIONSHIP ( 'NONE' , 'NONE' ,  #103311, #34315 ) ;
#10745 = ORIENTED_EDGE ( 'NONE', *, *, #113692, .F. ) ;
#10746 =( BOUNDED_CURVE ( )  B_SPLINE_CURVE ( 3, ( #99192, #76050, #10061, #86932 ),
 .UNSPECIFIED., .F., .T. ) 
 B_SPLINE_CURVE_WITH_KNOTS ( ( 4, 4 ),
 ( 1.610468072580458099, 1.654543780452488067 ),
 .UNSPECIFIED. ) 
 CURVE ( )  GEOMETRIC_REPRESENTATION_ITEM ( )  RATIONAL_B_SPLINE_CURVE ( ( 1.000000000000000000, 0.9998381175498709528, 0.9998381175498709528, 1.000000000000000000 ) ) 
 REPRESENTATION_ITEM ( '' )  );
#10747 = ORIENTED_EDGE ( 'NONE', *, *, #134375, .F. ) ;
#10748 = PLANE ( 'NONE',  #29458 ) ;
#10749 = ORIENTED_EDGE ( 'NONE', *, *, #100523, .F. ) ;
#10750 = ORIENTED_EDGE ( 'NONE', *, *, #77954, .T. ) ;
#10751 = EDGE_CURVE ( 'NONE', #5194, #59910, #110863, .T. ) ;
#10752 = CIRCLE ( 'NONE', #50228, 0.5000000000000000000 ) ;
#10753 = ADVANCED_FACE ( 'NONE', ( #79021 ), #35522, .T. ) ;
#10754 = CARTESIAN_POINT ( 'NONE',  ( 21.29159235450332233, 9.902892378096218942E-16, 0.000000000000000000 ) ) ;
#10755 = VERTEX_POINT ( 'NONE', #89157 ) ;
#10756 = LINE ( 'NONE', #120966, #18129 ) ;
#10757 = FILL_AREA_STYLE_COLOUR ( '', #50726 ) ;
#10758 = EDGE_CURVE ( 'NONE', #1674, #84583, #76882, .T. ) ;
#10759 = CARTESIAN_POINT ( 'NONE',  ( 18.18398860626898994, 28.73617430169800002, 5.000000000000000000 ) ) ;
#10760 = VECTOR ( 'NONE', #2472, 1000.000000000000000 ) ;
#10761 = FACE_OUTER_BOUND ( 'NONE', #117110, .T. ) ;
#10762 = CARTESIAN_POINT ( 'NONE',  ( 119.8541666666666572, -2.130196079827463507, -7.949999999999979750 ) ) ;
#10763 = EDGE_LOOP ( 'NONE', ( #9854, #5512, #58166, #127087, #132725, #106930, #115007, #23359, #46568 ) ) ;
#10764 = ADVANCED_FACE ( 'NONE', ( #55105 ), #13695, .F. ) ;
#10765 = DIRECTION ( 'NONE',  ( -0.7071067811865486830, -0.7071067811865464625, 0.000000000000000000 ) ) ;
#10767 = ORIENTED_EDGE ( 'NONE', *, *, #51040, .T. ) ;
#10766 = VECTOR ( 'NONE', #121837, 1000.000000000000000 ) ;
#10768 = CARTESIAN_POINT ( 'NONE',  ( 19.75393710176154016, -1.810825152012566219, -32.45514583868006753 ) ) ;
#10769 = EDGE_LOOP ( 'NONE', ( #67088, #124146, #100815, #127063, #5462 ) ) ;
#10770 = CARTESIAN_POINT ( 'NONE',  ( 116.4541937171295558, 6.884901960086283523, 3.975000000000002753 ) ) ;
#10771 = ORIENTED_EDGE ( 'NONE', *, *, #72463, .F. ) ;
#10772 = DIRECTION ( 'NONE',  ( -0.6830127018922181881, 0.6830127018922202975, -0.2588190451025214056 ) ) ;
#10773 = ORIENTED_EDGE ( 'NONE', *, *, #18277, .F. ) ;
#10774 = ORIENTED_EDGE ( 'NONE', *, *, #35599, .F. ) ;
#10775 = EDGE_LOOP ( 'NONE', ( #6562, #105474 ) ) ;
#10776 = VECTOR ( 'NONE', #129918, 1000.000000000000000 ) ;
#10777 = PLANE ( 'NONE',  #83629 ) ;
#10778 = CARTESIAN_POINT ( 'NONE',  ( 20.29298673570680123, -21.74070752338406720, 4.999753212805221558 ) ) ;
#10779 = FACE_OUTER_BOUND ( 'NONE', #122890, .T. ) ;
#10780 = STYLED_ITEM ( 'NONE', ( #105440 ), #92115 ) ;
#10781 = DIRECTION ( 'NONE',  ( -0.7071067811865486830, -0.7071067811865464625, -0.000000000000000000 ) ) ;
#10782 = EDGE_CURVE ( 'NONE', #47934, #46563, #132697, .T. ) ;
#10783 = PRODUCT_DEFINITION_SHAPE ( 'NONE', 'NONE',  #128095 ) ;
#10785 = AXIS2_PLACEMENT_3D ( 'NONE', #127889, #106804, #7493 ) ;
#10784 = DIRECTION ( 'NONE',  ( -0.7071067811865487940, 0.7071067811865463515, 0.000000000000000000 ) ) ;
#10786 = DIRECTION ( 'NONE',  ( -0.6830127018922180770, -0.6830127018922204085, -0.2588190451025213501 ) ) ;
#10787 = CARTESIAN_POINT ( 'NONE',  ( -28.49999999999980105, 8.900465351122127444, -2.516491619111447253 ) ) ;
#10788 = DIRECTION ( 'NONE',  ( 1.000000000000000000, 0.000000000000000000, 0.000000000000000000 ) ) ;
#10789 = DIRECTION ( 'NONE',  ( -0.7071067811865486830, -0.7071067811865464625, 0.000000000000000000 ) ) ;
#10790 = CARTESIAN_POINT ( 'NONE',  ( 11.99451991528749417, 28.92564299267946382, 4.000000000000000000 ) ) ;
#10791 = PRESENTATION_LAYER_ASSIGNMENT (  '', '', ( #1477 ) ) ;
#10792 = ORIENTED_EDGE ( 'NONE', *, *, #72823, .T. ) ;
#10793 = ORIENTED_EDGE ( 'NONE', *, *, #86774, .T. ) ;
#10794 = ORIENTED_EDGE ( 'NONE', *, *, #124173, .F. ) ;
#10795 = LINE ( 'NONE', #131177, #35628 ) ;
#10796 = VERTEX_POINT ( 'NONE', #1389 ) ;
#10797 = EDGE_LOOP ( 'NONE', ( #36828, #40489, #4231, #40619 ) ) ;
#10798 = FACE_OUTER_BOUND ( 'NONE', #24250, .T. ) ;
#10799 = LINE ( 'NONE', #102143, #20066 ) ;
#10800 = ADVANCED_FACE ( 'NONE', ( #90588 ), #65545, .T. ) ;
#10801 = CONICAL_SURFACE ( 'NONE', #114900, 2.055000000000001048, 0.9599310885968758145 ) ;
#10802 = PLANE ( 'NONE',  #40310 ) ;
#10803 = DIRECTION ( 'NONE',  ( -0.000000000000000000, 0.3543493200069153248, 0.9351131265310292928 ) ) ;
#10804 = EDGE_CURVE ( 'NONE', #89814, #130555, #45678, .T. ) ;
#10805 = ORIENTED_EDGE ( 'NONE', *, *, #123402, .T. ) ;
#10806 = LINE ( 'NONE', #133347, #78908 ) ;
#10807 = ORIENTED_EDGE ( 'NONE', *, *, #18970, .T. ) ;
#10808 = VECTOR ( 'NONE', #94018, 1000.000000000000000 ) ;
#10810 = DIRECTION ( 'NONE',  ( 1.000000000000000000, 0.000000000000000000, 0.000000000000000000 ) ) ;
#10809 = VECTOR ( 'NONE', #2915, 1000.000000000000227 ) ;
#10811 = EDGE_CURVE ( 'NONE', #33166, #41654, #10839, .T. ) ;
#10812 = AXIS2_PLACEMENT_3D ( 'NONE', #137697, #49972, #62271 ) ;
#10813 = CARTESIAN_POINT ( 'NONE',  ( 17.71290314143521982, 3.967499999999992699, -6.871911579029513994 ) ) ;
#10814 = VERTEX_POINT ( 'NONE', #99279 ) ;
#10815 = CARTESIAN_POINT ( 'NONE',  ( 86.53709685856478018, -3.054999999999999272, -5.291415217122919401 ) ) ;
#10816 = CARTESIAN_POINT ( 'NONE',  ( 6.176602844086411359, -9.397266779063615516, -1.419141200614698395 ) ) ;
#10817 = LINE ( 'NONE', #54387, #90729 ) ;
#10818 = DIRECTION ( 'NONE',  ( -2.969899378462214681E-16, 0.9667936545734399090, 0.2555582702174445942 ) ) ;
#10819 = ORIENTED_EDGE ( 'NONE', *, *, #63338, .F. ) ;
#10820 = ORIENTED_EDGE ( 'NONE', *, *, #94769, .F. ) ;
#10821 = EDGE_LOOP ( 'NONE', ( #21799, #47488, #52267 ) ) ;
#10822 = CARTESIAN_POINT ( 'NONE',  ( 9.591592354503321260, 9.902892378096218942E-16, 0.000000000000000000 ) ) ;
#10823 = CARTESIAN_POINT ( 'NONE',  ( 18.29177708983036155, -15.74070752338412049, 19.73771281079102025 ) ) ;
#10824 = DIRECTION ( 'NONE',  ( 1.000000000000000000, 0.000000000000000000, 0.000000000000000000 ) ) ;
#10825 = DIRECTION ( 'NONE',  ( 0.7071067811865487940, 0.7071067811865463515, 0.000000000000000000 ) ) ;
#10826 = CARTESIAN_POINT ( 'NONE',  ( 13.96000000000000085, -2.055000000000000160, 0.000000000000000000 ) ) ;
#10827 = EDGE_LOOP ( 'NONE', ( #122460, #64236, #22015, #132483 ) ) ;
#10828 = LINE ( 'NONE', #84851, #64625 ) ;
#10829 = ADVANCED_FACE ( 'NONE', ( #143525 ), #100038, .F. ) ;
#10830 = FACE_OUTER_BOUND ( 'NONE', #70848, .T. ) ;
#10831 = VERTEX_POINT ( 'NONE', #41015 ) ;
#10832 = FACE_OUTER_BOUND ( 'NONE', #58942, .T. ) ;
#10833 = DIRECTION ( 'NONE',  ( -0.6830127018922181881, 0.6830127018922202975, -0.2588190451025214056 ) ) ;
#10834 = ORIENTED_EDGE ( 'NONE', *, *, #52564, .T. ) ;
#10836 = VERTEX_POINT ( 'NONE', #62792 ) ;
#10835 = DIRECTION ( 'NONE',  ( 0.3543493200069162685, -0.000000000000000000, -0.9351131265310288487 ) ) ;
#10837 = ORIENTED_EDGE ( 'NONE', *, *, #21276, .F. ) ;
#10838 = EDGE_CURVE ( 'NONE', #70323, #67112, #135524, .T. ) ;
#10839 = LINE ( 'NONE', #23141, #72484 ) ;
#10841 = AXIS2_PLACEMENT_3D ( 'NONE', #21166, #87853, #42232 ) ;
#10840 = CARTESIAN_POINT ( 'NONE',  ( 34.42499999999998295, -21.02281430457037814, 5.000000000000000000 ) ) ;
#10842 = ORIENTED_EDGE ( 'NONE', *, *, #143170, .F. ) ;
#10843 = CARTESIAN_POINT ( 'NONE',  ( -26.99999999999981526, 14.96639925780211122, 5.000000000000000000 ) ) ;
#10844 = DIRECTION ( 'NONE',  ( -0.7071067811865486830, 0.7071067811865464625, 0.000000000000000000 ) ) ;
#10845 = VECTOR ( 'NONE', #45938, 1000.000000000000000 ) ;
#10846 = LINE ( 'NONE', #88461, #78527 ) ;
#10847 = DIRECTION ( 'NONE',  ( 0.6830127018922181881, 0.6830127018922202975, -0.2588190451025214056 ) ) ;
#10848 = CARTESIAN_POINT ( 'NONE',  ( 31.47916666666665364, -7.950000000000000178, 2.130196079827424427 ) ) ;
#10849 = DIRECTION ( 'NONE',  ( -0.000000000000000000, 0.3543493200069152138, -0.9351131265310292928 ) ) ;
#10850 = CARTESIAN_POINT ( 'NONE',  ( 31.49999999999979039, 9.052185695429082912, 5.000000000000000000 ) ) ;
#10851 = DIRECTION ( 'NONE',  ( -0.7071067811865486830, -0.7071067811865464625, 0.000000000000000000 ) ) ;
#10852 = CARTESIAN_POINT ( 'NONE',  ( -3.121473163371450532, -20.24070752338407431, 7.412974875817798903 ) ) ;
#10853 = CARTESIAN_POINT ( 'NONE',  ( -11.51078643762690490, -27.52281430457047406, 5.000000000000000000 ) ) ;
#10854 = CARTESIAN_POINT ( 'NONE',  ( 12.18398860626900060, 28.73617430169795739, 5.000000000000000000 ) ) ;
#10855 = CARTESIAN_POINT ( 'NONE',  ( -8.510786437626906675, -27.52281430457049183, 5.000000000000000000 ) ) ;
#10856 = DIRECTION ( 'NONE',  ( -0.000000000000000000, -1.000000000000000000, -0.000000000000000000 ) ) ;
#10857 = ORIENTED_EDGE ( 'NONE', *, *, #89335, .F. ) ;
#10858 = ORIENTED_EDGE ( 'NONE', *, *, #13481, .T. ) ;
#10859 = CARTESIAN_POINT ( 'NONE',  ( 101.9166666666666714, -6.884901960086287076, -3.975000000000000977 ) ) ;
#10860 = ORIENTED_EDGE ( 'NONE', *, *, #113036, .T. ) ;
#10861 = EDGE_LOOP ( 'NONE', ( #104495, #39016, #17230, #63991 ) ) ;
#10862 = VERTEX_POINT ( 'NONE', #2839 ) ;
#10863 = VECTOR ( 'NONE', #1580, 1000.000000000000227 ) ;
#10864 = DIRECTION ( 'NONE',  ( -1.000000000000000000, -1.224606353822377258E-16, -0.000000000000000000 ) ) ;
#10865 = CARTESIAN_POINT ( 'NONE',  ( 20.99065804761471199, 2.500000000000000888, 0.000000000000000000 ) ) ;
#10866 = ORIENTED_EDGE ( 'NONE', *, *, #43496, .T. ) ;
#10867 = DIRECTION ( 'NONE',  ( 0.000000000000000000, -1.000000000000000000, 0.000000000000000000 ) ) ;
#10868 = CARTESIAN_POINT ( 'NONE',  ( 6.540657738503846907, 2.055000000000001048, 0.000000000000000000 ) ) ;
#10870 = AXIS2_PLACEMENT_3D ( 'NONE', #135607, #59491, #80523 ) ;
#10869 = LINE ( 'NONE', #55138, #122797 ) ;
#10871 = CARTESIAN_POINT ( 'NONE',  ( -15.75860074219783513, 21.72499999999999432, 5.000000000000000000 ) ) ;
#10872 = ORIENTED_EDGE ( 'NONE', *, *, #82734, .T. ) ;
#10873 = EDGE_CURVE ( 'NONE', #91527, #75052, #81881, .T. ) ;
#10874 = PLANE ( 'NONE',  #37240 ) ;
#10875 = FACE_OUTER_BOUND ( 'NONE', #96640, .T. ) ;
#10876 = CARTESIAN_POINT ( 'NONE',  ( -33.70710678118631165, 5.259292476615663681, 5.000000000000000000 ) ) ;
#10877 = DIRECTION ( 'NONE',  ( -0.7071067811865487940, 0.7071067811865463515, 0.000000000000000000 ) ) ;
#10878 = CARTESIAN_POINT ( 'NONE',  ( -47.99451991528749062, 28.92564299267971251, 4.000000000000000000 ) ) ;
#10879 = CARTESIAN_POINT ( 'NONE',  ( 33.29974487139158867, -27.71228299555229313, 4.000000000000000000 ) ) ;
#10880 = CARTESIAN_POINT ( 'NONE',  ( -20.58838509405153872, 22.22500000000000142, 4.777194822843816802 ) ) ;
#10881 = EDGE_CURVE ( 'NONE', #46464, #33991, #129439, .T. ) ;
#10882 = ADVANCED_FACE ( 'NONE', ( #58722 ), #126074, .F. ) ;
#10883 = ORIENTED_EDGE ( 'NONE', *, *, #106107, .F. ) ;
#10884 = ORIENTED_EDGE ( 'NONE', *, *, #95378, .F. ) ;
#10885 = CARTESIAN_POINT ( 'NONE',  ( 118.2712635252314470, 4.472830434245839371, 4.472830434245842035 ) ) ;
#10886 = ADVANCED_FACE ( 'NONE', ( #125351 ), #70210, .T. ) ;
#10887 = AXIS2_PLACEMENT_3D ( 'NONE', #41446, #129894, #87108 ) ;
#10888 = VERTEX_POINT ( 'NONE', #80435 ) ;
#10889 = DIRECTION ( 'NONE',  ( -0.6830127018922180770, -0.6830127018922204085, -0.2588190451025213501 ) ) ;
#10890 = EDGE_CURVE ( 'NONE', #58827, #9095, #36207, .T. ) ;
#10891 = LINE ( 'NONE', #109524, #138180 ) ;
#10892 = EDGE_CURVE ( 'NONE', #35612, #40957, #125746, .T. ) ;
#10893 = FACE_OUTER_BOUND ( 'NONE', #96011, .T. ) ;
#10894 = DIRECTION ( 'NONE',  ( 0.3543493200069162685, -0.000000000000000000, -0.9351131265310288487 ) ) ;
#10895 = DIRECTION ( 'NONE',  ( 0.3543493200069162685, -0.000000000000000000, -0.9351131265310288487 ) ) ;
#10896 = ADVANCED_FACE ( 'NONE', ( #114454 ), #3525, .F. ) ;
#10897 = CARTESIAN_POINT ( 'NONE',  ( 115.8495968585647802, 6.109999999999996767, 1.637169565754163836 ) ) ;
#10899 = ORIENTED_EDGE ( 'NONE', *, *, #106226, .T. ) ;
#10898 = VECTOR ( 'NONE', #48973, 1000.000000000000000 ) ;
#10900 = ORIENTED_EDGE ( 'NONE', *, *, #57447, .T. ) ;
#10901 = DIRECTION ( 'NONE',  ( -0.6830127018922180770, -0.6830127018922204085, -0.2588190451025213501 ) ) ;
#10902 =( NAMED_UNIT ( * ) SI_UNIT ( $, .STERADIAN. ) SOLID_ANGLE_UNIT ( ) );
#10903 = EDGE_CURVE ( 'NONE', #104204, #60317, #19264, .T. ) ;
#10904 = ORIENTED_EDGE ( 'NONE', *, *, #112761, .T. ) ;
#10905 = ORIENTED_EDGE ( 'NONE', *, *, #84266, .F. ) ;
#10906 = VECTOR ( 'NONE', #122739, 1000.000000000000000 ) ;
#10907 = CARTESIAN_POINT ( 'NONE',  ( 40.83376352523143993, 6.110000000000001208, 1.122388791418549305E-15 ) ) ;
#10908 = VERTEX_POINT ( 'NONE', #15813 ) ;
#10909 = CARTESIAN_POINT ( 'NONE',  ( -17.01299345042646749, -0.9444868035190713274, -36.39086428169088094 ) ) ;
#10910 = LINE ( 'NONE', #45053, #31652 ) ;
#10911 = CARTESIAN_POINT ( 'NONE',  ( -20.99999999999984723, 8.966399257802164513, 5.000000000000000000 ) ) ;
#10912 = ADVANCED_FACE ( 'NONE', ( #27433 ), #106973, .T. ) ;
#10913 = AXIS2_PLACEMENT_3D ( 'NONE', #36618, #72159, #117037 ) ;
#10914 = VECTOR ( 'NONE', #32934, 1000.000000000000000 ) ;
#10915 = AXIS2_PLACEMENT_3D ( 'NONE', #47361, #36428, #5184 ) ;
#10916 = CARTESIAN_POINT ( 'NONE',  ( 30.09959685856478018, -6.109999999999997655, -1.637169565754160283 ) ) ;
#10917 = ORIENTED_EDGE ( 'NONE', *, *, #3403, .F. ) ;
#10918 = LINE ( 'NONE', #55184, #66432 ) ;
#10919 = EDGE_LOOP ( 'NONE', ( #17575, #84950, #109361 ) ) ;
#10920 = ORIENTED_EDGE ( 'NONE', *, *, #62506, .F. ) ;
#10921 = AXIS2_PLACEMENT_3D ( 'NONE', #133798, #100459, #45390 ) ;
#10922 = EDGE_LOOP ( 'NONE', ( #79873, #71519, #18855, #56172 ) ) ;
#10923 = CARTESIAN_POINT ( 'NONE',  ( -1.171830600776462061, -20.24070752338407786, 4.000000000000000000 ) ) ;
#10924 = ORIENTED_EDGE ( 'NONE', *, *, #129152, .F. ) ;
#10925 = CARTESIAN_POINT ( 'NONE',  ( -25.01899999999999835, 3.174999999999998046, 1.444000000000000394 ) ) ;
#10926 = EDGE_CURVE ( 'NONE', #120446, #90697, #136211, .T. ) ;
#10927 = DIRECTION ( 'NONE',  ( 0.7071067811865487940, -0.7071067811865463515, 0.000000000000000000 ) ) ;
#10928 = ADVANCED_FACE ( 'NONE', ( #81144 ), #96332, .T. ) ;
#10929 = CARTESIAN_POINT ( 'NONE',  ( -72.18398860626899705, 28.73617430169837661, 5.000000000000000000 ) ) ;
#10930 = FACE_BOUND ( 'NONE', #17757, .T. ) ;
#10931 = EDGE_LOOP ( 'NONE', ( #11713, #85734, #85442, #73324, #103170, #102916 ) ) ;
#10932 = DIRECTION ( 'NONE',  ( 0.7071067811865487940, -0.7071067811865463515, 0.000000000000000000 ) ) ;
#10933 = LINE ( 'NONE', #44342, #53882 ) ;
#10934 = FACE_OUTER_BOUND ( 'NONE', #14311, .T. ) ;
#10935 = VERTEX_POINT ( 'NONE', #82557 ) ;
#10936 = DIRECTION ( 'NONE',  ( -0.7071067811865486830, -0.7071067811865464625, -0.000000000000000000 ) ) ;
#10937 = ORIENTED_EDGE ( 'NONE', *, *, #95403, .T. ) ;
#10938 = VECTOR ( 'NONE', #40282, 1000.000000000000000 ) ;
#10939 = EDGE_LOOP ( 'NONE', ( #14303, #113302, #22318, #99897 ) ) ;
#10940 = FILL_AREA_STYLE_COLOUR ( '', #114298 ) ;
#10941 = EDGE_CURVE ( 'NONE', #140728, #85524, #7652, .T. ) ;
#10942 = EDGE_LOOP ( 'NONE', ( #83129, #135686, #85684, #128238 ) ) ;
#10943 = CARTESIAN_POINT ( 'NONE',  ( 43.95376352523145158, -6.109999999999998543, -3.741295971395162543E-16 ) ) ;
#10944 = AXIS2_PLACEMENT_3D ( 'NONE', #23122, #33373, #67409 ) ;
#10945 = ORIENTED_EDGE ( 'NONE', *, *, #118311, .T. ) ;
#10946 = LINE ( 'NONE', #130650, #111203 ) ;
#10947 = EDGE_CURVE ( 'NONE', #94548, #32452, #136932, .T. ) ;
#10948 = LINE ( 'NONE', #55943, #132111 ) ;
#10949 = ORIENTED_EDGE ( 'NONE', *, *, #30753, .F. ) ;
#10950 = CARTESIAN_POINT ( 'NONE',  ( -11.99999999999991296, 19.93112307739198386, 4.000000000000000000 ) ) ;
#10951 = DIRECTION ( 'NONE',  ( 0.7071067811865486830, -0.7071067811865464625, -0.000000000000000000 ) ) ;
#10952 = AXIS2_PLACEMENT_3D ( 'NONE', #120759, #52649, #131660 ) ;
#10953 = LINE ( 'NONE', #13108, #22364 ) ;
#10954 = CARTESIAN_POINT ( 'NONE',  ( 27.32816939922333432, 17.25929247661553489, 4.000000000000000000 ) ) ;
#10955 = DIRECTION ( 'NONE',  ( 0.7071067811865486830, -0.7071067811865464625, -0.000000000000000000 ) ) ;
#10956 = DIRECTION ( 'NONE',  ( 0.000000000000000000, -1.000000000000000000, 0.000000000000000000 ) ) ;
#10957 = CARTESIAN_POINT ( 'NONE',  ( -39.29974487139159578, -27.71228299555233576, 4.000000000000000000 ) ) ;
#10958 = ORIENTED_EDGE ( 'NONE', *, *, #16461, .T. ) ;
#10959 = VECTOR ( 'NONE', #131083, 1000.000000000000000 ) ;
#10960 = ORIENTED_EDGE ( 'NONE', *, *, #96802, .T. ) ;
#10961 = ORIENTED_EDGE ( 'NONE', *, *, #101657, .T. ) ;
#10962 = DIRECTION ( 'NONE',  ( -0.7071067811865487940, 0.7071067811865463515, 0.000000000000000000 ) ) ;
#10963 = CARTESIAN_POINT ( 'NONE',  ( 31.82816939922331656, 18.75929247661552779, 4.000000000000000000 ) ) ;
#10964 = EDGE_LOOP ( 'NONE', ( #31577, #91235, #21833, #49192 ) ) ;
#10965 = VERTEX_POINT ( 'NONE', #117823 ) ;
#10966 = DIRECTION ( 'NONE',  ( -0.000000000000000000, -1.000000000000000000, -0.000000000000000000 ) ) ;
#10967 = CARTESIAN_POINT ( 'NONE',  ( -21.18398860626899349, 28.73617430169802134, 5.000000000000000000 ) ) ;
#10968 = EDGE_CURVE ( 'NONE', #25822, #93317, #18513, .T. ) ;
#10969 = EDGE_CURVE ( 'NONE', #23067, #123360, #140329, .T. ) ;
#10970 = CARTESIAN_POINT ( 'NONE',  ( 20.99065804761471199, 2.500000000000000444, 0.000000000000000000 ) ) ;
#10971 = ORIENTED_EDGE ( 'NONE', *, *, #86600, .T. ) ;
#10972 = DIRECTION ( 'NONE',  ( 0.000000000000000000, -1.000000000000000000, 0.000000000000000000 ) ) ;
#10973 = LINE ( 'NONE', #55242, #5066 ) ;
#10974 = ADVANCED_FACE ( 'NONE', ( #107685 ), #30874, .T. ) ;
#10975 = CARTESIAN_POINT ( 'NONE',  ( 30.10873647476854842, -5.808823158059033709, 5.808823158059035485 ) ) ;
#10976 = CARTESIAN_POINT ( 'NONE',  ( -28.49999999999980460, 6.431123077392117082, 4.000000000000000000 ) ) ;
#10977 = VERTEX_POINT ( 'NONE', #33736 ) ;
#10978 = CARTESIAN_POINT ( 'NONE',  ( 123.2870968585647944, 3.054999999999997939, 5.291415217122920289 ) ) ;
#10979 = CIRCLE ( 'NONE', #92038, 2.500000000000000888 ) ;
#10980 = ADVANCED_FACE ( 'NONE', ( #54073 ), #9041, .F. ) ;
#10981 = DIRECTION ( 'NONE',  ( -1.000000000000000000, -1.224606353822377258E-16, -0.000000000000000000 ) ) ;
#10982 = LINE ( 'NONE', #111016, #3271 ) ;
#10984 = ORIENTED_EDGE ( 'NONE', *, *, #61384, .F. ) ;
#10983 = CARTESIAN_POINT ( 'NONE',  ( 9.411614905948244569, 22.22499999999999787, 4.777194822843815913 ) ) ;
#10985 = CARTESIAN_POINT ( 'NONE',  ( 25.39999999999999858, 7.464222240803104598E-16, -6.094999999999989093 ) ) ;
#10986 = ORIENTED_EDGE ( 'NONE', *, *, #136603, .T. ) ;
#10987 = DIRECTION ( 'NONE',  ( 0.6830127018922181881, 0.6830127018922202975, -0.2588190451025214056 ) ) ;
#10988 = DIRECTION ( 'NONE',  ( 0.3543493200069163240, -0.000000000000000000, -0.9351131265310288487 ) ) ;
#10989 = LINE ( 'NONE', #12443, #112060 ) ;
#10991 = EDGE_CURVE ( 'NONE', #128295, #115416, #77940, .T. ) ;
#10990 = ORIENTED_EDGE ( 'NONE', *, *, #47309, .T. ) ;
#10992 = AXIS2_PLACEMENT_3D ( 'NONE', #48171, #126424, #36568 ) ;
#10993 = EDGE_CURVE ( 'NONE', #91708, #63130, #75103, .T. ) ;
#10994 = CARTESIAN_POINT ( 'NONE',  ( 6.462472949537106715, -7.464222240803106570E-16, -6.094999999999989981 ) ) ;
#10995 = CARTESIAN_POINT ( 'NONE',  ( 48.48921356237309510, -27.52281430457089328, 5.000000000000000000 ) ) ;
#10996 = ORIENTED_EDGE ( 'NONE', *, *, #17068, .F. ) ;
#10997 = DIRECTION ( 'NONE',  ( 0.000000000000000000, 0.000000000000000000, 1.000000000000000000 ) ) ;
#10998 = VECTOR ( 'NONE', #92644, 1000.000000000000000 ) ;
#10999 = DIRECTION ( 'NONE',  ( 0.6830127018922181881, 0.6830127018922202975, -0.2588190451025214056 ) ) ;
#11000 = ORIENTED_EDGE ( 'NONE', *, *, #47976, .F. ) ;
#11001 = AXIS2_PLACEMENT_3D ( 'NONE', #55554, #21490, #141857 ) ;
#11002 = LINE ( 'NONE', #79917, #103986 ) ;
#11004 = ORIENTED_EDGE ( 'NONE', *, *, #80247, .T. ) ;
#11003 = PLANE ( 'NONE',  #30164 ) ;
#11005 = EDGE_CURVE ( 'NONE', #124489, #32019, #52596, .T. ) ;
#11006 = ORIENTED_EDGE ( 'NONE', *, *, #68435, .F. ) ;
#11007 = CARTESIAN_POINT ( 'NONE',  ( 17.42079396106911560, 4.797059468579773167, -29.42940194308667401 ) ) ;
#11008 = CARTESIAN_POINT ( 'NONE',  ( -25.39999999999996305, 3.061616997868383141E-16, -2.500000000000000000 ) ) ;
#11009 = VECTOR ( 'NONE', #65210, 1000.000000000000000 ) ;
#11010 = ORIENTED_EDGE ( 'NONE', *, *, #89778, .T. ) ;
#11011 = COLOUR_RGB ( '', 0.09019608, 0.27058824, 0.51372549) ;
#11012 = CARTESIAN_POINT ( 'NONE',  ( 32.67183060077623935, 17.25929247661554200, 4.000000000000000000 ) ) ;
#11013 = CARTESIAN_POINT ( 'NONE',  ( -14.67183060077636370, -3.740707523384238176, 4.000000000000000000 ) ) ;
#11014 = CARTESIAN_POINT ( 'NONE',  ( -17.99999999999986855, -12.41253812416062985, 4.000000000000000000 ) ) ;
#11015 = ORIENTED_EDGE ( 'NONE', *, *, #25652, .T. ) ;
#11016 = LINE ( 'NONE', #53871, #20983 ) ;
#11017 = DIRECTION ( 'NONE',  ( -0.000000000000000000, 0.000000000000000000, 1.000000000000000000 ) ) ;
#11018 = CARTESIAN_POINT ( 'NONE',  ( 2.148183550381434603, 17.25929247661554200, 8.802941693769207987 ) ) ;
#11019 = DIRECTION ( 'NONE',  ( -0.000000000000000000, 0.3543493200069153248, 0.9351131265310292928 ) ) ;
#11020 = CARTESIAN_POINT ( 'NONE',  ( 27.62043019189810877, 3.055000000000002380, -5.291415217122917625 ) ) ;
#11021 = DIRECTION ( 'NONE',  ( -1.000000000000000000, -0.000000000000000000, -0.000000000000000000 ) ) ;
#11022 = ORIENTED_EDGE ( 'NONE', *, *, #121000, .F. ) ;
#11023 = ORIENTED_EDGE ( 'NONE', *, *, #43055, .T. ) ;
#11024 = CARTESIAN_POINT ( 'NONE',  ( 125.3958333333333428, -2.130196079827427091, 7.949999999999999289 ) ) ;
#11025 = VERTEX_POINT ( 'NONE', #41732 ) ;
#11026 = ORIENTED_EDGE ( 'NONE', *, *, #33932, .F. ) ;
#11027 = CARTESIAN_POINT ( 'NONE',  ( -14.99999999999989164, -16.06887692260766087, 4.000000000000000000 ) ) ;
#11028 = CARTESIAN_POINT ( 'NONE',  ( -33.48921356237309510, -27.52281430457078670, 5.000000000000000000 ) ) ;
#11029 = ORIENTED_EDGE ( 'NONE', *, *, #43165, .F. ) ;
#11030 =( BOUNDED_CURVE ( )  B_SPLINE_CURVE ( 2, ( #131040, #89662, #142627, #99085, #120854, #9953, #43320, #133890, #45484, #54225, #32442, #55625, #100557 ),
 .UNSPECIFIED., .F., .T. ) 
 B_SPLINE_CURVE_WITH_KNOTS ( ( 3, 2, 2, 2, 2, 2, 3 ),
 ( 0.5500000000000001554, 0.5583333333333334592, 0.5666666666666667629, 0.5750000000000000666, 0.5833333333333334814, 0.5916666666666667851, 0.6000000000000000888 ),
 .UNSPECIFIED. ) 
 CURVE ( )  GEOMETRIC_REPRESENTATION_ITEM ( )  RATIONAL_B_SPLINE_CURVE ( ( 0.9999999999999995559, 0.9659258262890687563, 1.000000000000000000, 0.9659258262890683122, 1.000000000000000000, 0.9659258262890683122, 1.000000000000000000, 0.9659258262890683122, 1.000000000000000000, 0.9659258262890683122, 1.000000000000000000, 0.9659258262890678681, 1.000000000000000444 ) ) 
 REPRESENTATION_ITEM ( '' )  );
#11031 = CARTESIAN_POINT ( 'NONE',  ( -74.99451991528749772, 28.92564299267990435, 4.000000000000000000 ) ) ;
#11032 = DIRECTION ( 'NONE',  ( 0.7071067811865487940, 0.7071067811865463515, 0.000000000000000000 ) ) ;
#11033 = DIRECTION ( 'NONE',  ( -1.000000000000000000, 0.000000000000000000, 0.000000000000000000 ) ) ;
#11034 = CARTESIAN_POINT ( 'NONE',  ( -4.362461875838996583, 22.22500000000000142, 4.000000000000000000 ) ) ;
#11035 = CARTESIAN_POINT ( 'NONE',  ( 122.7920968585647756, -5.291415217122921177, 3.054999999999999272 ) ) ;
#11036 = ORIENTED_EDGE ( 'NONE', *, *, #120554, .F. ) ;
#11037 = CARTESIAN_POINT ( 'NONE',  ( 14.99999999999990052, -6.033600742197674727, 5.000000000000000000 ) ) ;
#11038 = DIRECTION ( 'NONE',  ( 0.000000000000000000, -1.000000000000000000, 0.000000000000000000 ) ) ;
#11039 = VECTOR ( 'NONE', #86428, 1000.000000000000000 ) ;
#11040 = DIRECTION ( 'NONE',  ( -1.000000000000000000, -0.000000000000000000, -0.000000000000000000 ) ) ;
#11041 = DIRECTION ( 'NONE',  ( -1.000000000000000000, -0.000000000000000000, -0.000000000000000000 ) ) ;
#11042 = FACE_OUTER_BOUND ( 'NONE', #128508, .T. ) ;
#11043 = CARTESIAN_POINT ( 'NONE',  ( 56.99451991528749062, 28.92564299267978001, 4.000000000000000000 ) ) ;
#11044 = CARTESIAN_POINT ( 'NONE',  ( 29.99999999999979039, -16.60178936734445898, 0.8616154019348201132 ) ) ;
#11045 = CARTESIAN_POINT ( 'NONE',  ( 56.95419371712956291, 6.884901960086283523, 3.975000000000002753 ) ) ;
#11046 = DIRECTION ( 'NONE',  ( -1.000000000000000000, 0.000000000000000000, -0.000000000000000000 ) ) ;
#11047 = EDGE_CURVE ( 'NONE', #98610, #115536, #132345, .T. ) ;
#11048 = CARTESIAN_POINT ( 'NONE',  ( -12.69999999999998153, 0.000000000000000000, 0.000000000000000000 ) ) ;
#11049 = EDGE_LOOP ( 'NONE', ( #8259, #137665, #101322, #77516, #98232, #79687 ) ) ;
#11050 = ORIENTED_EDGE ( 'NONE', *, *, #111323, .T. ) ;
#11051 = CARTESIAN_POINT ( 'NONE',  ( 41.83333333333333570, -6.884901960086287964, 3.974999999999998312 ) ) ;
#11052 = EDGE_CURVE ( 'NONE', #115757, #81768, #108364, .T. ) ;
#11053 = EDGE_CURVE ( 'NONE', #113523, #127303, #66268, .T. ) ;
#11054 = DIRECTION ( 'NONE',  ( 1.000000000000000000, 0.000000000000000000, 0.000000000000000000 ) ) ;
#11055 = EDGE_CURVE ( 'NONE', #94607, #51968, #11195, .T. ) ;
#11056 = CARTESIAN_POINT ( 'NONE',  ( 5.994519915287488843, 28.92564299267942118, 4.000000000000000000 ) ) ;
#11057 = VERTEX_POINT ( 'NONE', #32291 ) ;
#11058 = EDGE_CURVE ( 'NONE', #99644, #99824, #96772, .T. ) ;
#11059 = DIRECTION ( 'NONE',  ( -0.7071067811865486830, -0.7071067811865464625, -0.000000000000000000 ) ) ;
#11060 = DIRECTION ( 'NONE',  ( -0.000000000000000000, 0.000000000000000000, 1.000000000000000000 ) ) ;
#11061 = CARTESIAN_POINT ( 'NONE',  ( 40.83376352523143993, 6.110000000000001208, 1.122388791418549305E-15 ) ) ;
#11063 = EDGE_CURVE ( 'NONE', #125846, #113106, #141026, .T. ) ;
#11062 = ORIENTED_EDGE ( 'NONE', *, *, #138528, .T. ) ;
#11064 = CYLINDRICAL_SURFACE ( 'NONE', #133604, 5.999999999999998224 ) ;
#11065 = VERTEX_POINT ( 'NONE', #9803 ) ;
#11066 = ORIENTED_EDGE ( 'NONE', *, *, #14501, .F. ) ;
#11067 = LINE ( 'NONE', #87243, #128016 ) ;
#11068 = CARTESIAN_POINT ( 'NONE',  ( 33.79289321881321939, 3.759292476615678336, 5.000000000000000000 ) ) ;
#11069 = CARTESIAN_POINT ( 'NONE',  ( -34.92500000000001137, 15.58119340046981449, 2.482413320905447307 ) ) ;
#11070 = EDGE_CURVE ( 'NONE', #125811, #98878, #99662, .T. ) ;
#11071 = CARTESIAN_POINT ( 'NONE',  ( -81.48921356237309510, -27.52281430457112066, 5.000000000000000000 ) ) ;
#11072 = ORIENTED_EDGE ( 'NONE', *, *, #24523, .T. ) ;
#11073 = ADVANCED_FACE ( 'NONE', ( #55475 ), #21412, .F. ) ;
#11074 = CARTESIAN_POINT ( 'NONE',  ( 0.000000000000000000, 0.000000000000000000, 5.000000000000000000 ) ) ;
#11076 = ORIENTED_EDGE ( 'NONE', *, *, #22679, .T. ) ;
#11075 = LINE ( 'NONE', #31445, #33712 ) ;
#11077 = CARTESIAN_POINT ( 'NONE',  ( 79.18793019189810423, 6.110000000000002984, -1.637169565754156730 ) ) ;
#11078 = FACE_OUTER_BOUND ( 'NONE', #4361, .T. ) ;
#11079 = FACE_OUTER_BOUND ( 'NONE', #105405, .T. ) ;
#11080 = DIRECTION ( 'NONE',  ( -1.000000000000000000, 0.000000000000000000, -0.000000000000000000 ) ) ;
#11081 =( NAMED_UNIT ( * ) SI_UNIT ( $, .STERADIAN. ) SOLID_ANGLE_UNIT ( ) );
#11082 = ADVANCED_FACE ( 'NONE', ( #109838 ), #53306, .F. ) ;
#11083 = ORIENTED_EDGE ( 'NONE', *, *, #89920, .F. ) ;
#11084 = MECHANICAL_DESIGN_GEOMETRIC_PRESENTATION_REPRESENTATION (  '', ( #57508 ), #76009 ) ;
#11085 = CARTESIAN_POINT ( 'NONE',  ( -25.49999999999982236, 0.4311230773921901349, 4.000000000000000000 ) ) ;
#11086 = CARTESIAN_POINT ( 'NONE',  ( 67.43293019189812298, 1.637169565754156508, 6.110000000000000320 ) ) ;
#11087 = DIRECTION ( 'NONE',  ( -0.5735764363510501562, 0.8191520442889890230, 1.003171929053521419E-16 ) ) ;
#11088 = CARTESIAN_POINT ( 'NONE',  ( -32.27718569542918203, -21.72500000000000142, 5.000000000000000000 ) ) ;
#11089 = CARTESIAN_POINT ( 'NONE',  ( 19.05000000000000071, 3.174999999999997158, 5.000000000000000000 ) ) ;
#11090 = ORIENTED_EDGE ( 'NONE', *, *, #122748, .T. ) ;
#11091 = VERTEX_POINT ( 'NONE', #44634 ) ;
#11092 = PLANE ( 'NONE',  #35320 ) ;
#11093 = ORIENTED_EDGE ( 'NONE', *, *, #70212, .T. ) ;
#11094 = CARTESIAN_POINT ( 'NONE',  ( -5.671830600776431197, 2.259292476615694323, 4.000000000000000000 ) ) ;
#11095 = ORIENTED_EDGE ( 'NONE', *, *, #124617, .T. ) ;
#11096 = CARTESIAN_POINT ( 'NONE',  ( 0.9387690737794647244, -0.3999999999999998002, -2.166563419957292957 ) ) ;
#11097 = FACE_OUTER_BOUND ( 'NONE', #127249, .T. ) ;
#11098 = EDGE_CURVE ( 'NONE', #47328, #29533, #75800, .T. ) ;
#11099 = AXIS2_PLACEMENT_3D ( 'NONE', #101049, #56180, #55430 ) ;
#11100 = LINE ( 'NONE', #109735, #129961 ) ;
#11101 = VECTOR ( 'NONE', #13261, 1000.000000000000000 ) ;
#11102 = FACE_BOUND ( 'NONE', #45927, .T. ) ;
#11103 = FACE_OUTER_BOUND ( 'NONE', #13864, .T. ) ;
#11104 = LINE ( 'NONE', #1654, #109106 ) ;
#11105 = PLANE ( 'NONE',  #71203 ) ;
#11107 = EDGE_LOOP ( 'NONE', ( #28870, #25540, #82963, #128463 ) ) ;
#11106 = DIRECTION ( 'NONE',  ( 0.3543493200069162685, -0.000000000000000000, -0.9351131265310288487 ) ) ;
#11108 = VECTOR ( 'NONE', #6659, 1000.000000000000000 ) ;
#11109 = VECTOR ( 'NONE', #131879, 1000.000000000000000 ) ;
#11110 = LINE ( 'NONE', #112607, #136592 ) ;
#11111 = ADVANCED_FACE ( 'NONE', ( #64924 ), #98740, .T. ) ;
#11112 = VERTEX_POINT ( 'NONE', #48160 ) ;
#11113 = VERTEX_POINT ( 'NONE', #36556 ) ;
#11114 = CARTESIAN_POINT ( 'NONE',  ( 71.95376352523145158, -6.109999999999998543, -3.741295971395162543E-16 ) ) ;
#11115 = ORIENTED_EDGE ( 'NONE', *, *, #90142, .F. ) ;
#11116 = LINE ( 'NONE', #98860, #77718 ) ;
#11117 = LINE ( 'NONE', #142406, #21176 ) ;
#11118 = ADVANCED_FACE ( 'NONE', ( #35166 ), #105659, .T. ) ;
#11119 = ORIENTED_EDGE ( 'NONE', *, *, #91714, .F. ) ;
#11120 = CARTESIAN_POINT ( 'NONE',  ( 54.29974487139159578, -27.71228299555243879, 4.000000000000000000 ) ) ;
#11121 = FACE_OUTER_BOUND ( 'NONE', #104882, .T. ) ;
#11122 = LINE ( 'NONE', #99571, #124754 ) ;
#11123 = FACE_OUTER_BOUND ( 'NONE', #68974, .T. ) ;
#11124 = ADVANCED_FACE ( 'NONE', ( #67060 ), #24948, .T. ) ;
#11125 = PLANE ( 'NONE',  #139571 ) ;
#11126 = DIRECTION ( 'NONE',  ( -0.7071067811865486830, -0.7071067811865464625, -0.000000000000000000 ) ) ;
#11127 = VERTEX_POINT ( 'NONE', #136571 ) ;
#11128 = ORIENTED_EDGE ( 'NONE', *, *, #79071, .F. ) ;
#11129 = FACE_OUTER_BOUND ( 'NONE', #1417, .T. ) ;
#11130 = FILL_AREA_STYLE_COLOUR ( '', #55949 ) ;
#11131 = VECTOR ( 'NONE', #98065, 1000.000000000000000 ) ;
#11132 = VERTEX_POINT ( 'NONE', #69204 ) ;
#11133 = VERTEX_POINT ( 'NONE', #78646 ) ;
#11134 = EDGE_CURVE ( 'NONE', #51507, #7626, #1049, .T. ) ;
#11135 = CARTESIAN_POINT ( 'NONE',  ( 26.97959685856476497, 6.109999999999999432, 1.637169565754164280 ) ) ;
#11136 = VECTOR ( 'NONE', #66639, 1000.000000000000000 ) ;
#11137 = ORIENTED_EDGE ( 'NONE', *, *, #785, .F. ) ;
#11138 = CARTESIAN_POINT ( 'NONE',  ( 127.2418942207595194, -46.18886352141515772, -34.92499999999998295 ) ) ;
#11139 = FACE_OUTER_BOUND ( 'NONE', #122062, .T. ) ;
#11140 = CARTESIAN_POINT ( 'NONE',  ( 21.19163961620376924, 6.094999999999988205, -1.633150327867694651 ) ) ;
#11141 = CARTESIAN_POINT ( 'NONE',  ( 16.93425912790457843, 5.488690751113135313, -29.15508941616193539 ) ) ;
#11142 = ORIENTED_EDGE ( 'NONE', *, *, #129727, .F. ) ;
#11143 = ORIENTED_EDGE ( 'NONE', *, *, #57313, .T. ) ;
#11144 = DIRECTION ( 'NONE',  ( -1.000000000000000000, -0.000000000000000000, -0.000000000000000000 ) ) ;
#11145 = CARTESIAN_POINT ( 'NONE',  ( -26.99999999999980460, 5.966399257802205369, 5.000000000000000000 ) ) ;
#11146 = VECTOR ( 'NONE', #34721, 1000.000000000000000 ) ;
#11148 = ORIENTED_EDGE ( 'NONE', *, *, #1454, .T. ) ;
#11147 = CARTESIAN_POINT ( 'NONE',  ( 32.99999999999975842, -4.447814304570784749, 5.000000000000000000 ) ) ;
#11149 = VERTEX_POINT ( 'NONE', #111245 ) ;
#11150 = CARTESIAN_POINT ( 'NONE',  ( -26.29289321881327623, -18.74070752338408852, 5.000000000000000000 ) ) ;
#11151 = CARTESIAN_POINT ( 'NONE',  ( 25.11017322888192993, -22.22499999999999787, 4.785647885939354751 ) ) ;
#11152 = VECTOR ( 'NONE', #46773, 1000.000000000000000 ) ;
#11153 = DIRECTION ( 'NONE',  ( 0.7071067811865487940, -0.7071067811865463515, 0.000000000000000000 ) ) ;
#11154 = VERTEX_POINT ( 'NONE', #103233 ) ;
#11155 = FACE_OUTER_BOUND ( 'NONE', #117967, .T. ) ;
#11157 = ORIENTED_EDGE ( 'NONE', *, *, #83427, .T. ) ;
#11156 = EDGE_CURVE ( 'NONE', #126185, #16532, #45337, .T. ) ;
#11158 = DIRECTION ( 'NONE',  ( 0.7071067811865487940, 0.7071067811865463515, 0.000000000000000000 ) ) ;
#11159 = CARTESIAN_POINT ( 'NONE',  ( 27.24999999999999645, -9.735942053221458872E-16, 7.950000000000000178 ) ) ;
#11160 = DIRECTION ( 'NONE',  ( 0.7071067811865487940, 0.7071067811865463515, 0.000000000000000000 ) ) ;
#11161 = CARTESIAN_POINT ( 'NONE',  ( -34.92499999999997584, 0.000000000000000000, -0.5000000000000004441 ) ) ;
#11162 = CARTESIAN_POINT ( 'NONE',  ( -31.92499999999997584, -21.76999999999999247, -39.50000000000000000 ) ) ;
#11163 = FACE_OUTER_BOUND ( 'NONE', #140533, .T. ) ;
#11165 = EDGE_CURVE ( 'NONE', #10977, #95984, #89513, .T. ) ;
#11164 = DIRECTION ( 'NONE',  ( 0.3543493200069162685, -0.000000000000000000, -0.9351131265310288487 ) ) ;
#11166 = LINE ( 'NONE', #131570, #13544 ) ;
#11167 = VERTEX_POINT ( 'NONE', #81529 ) ;
#11168 = ADVANCED_FACE ( 'NONE', ( #3203 ), #17705, .T. ) ;
#11169 = DIRECTION ( 'NONE',  ( 0.7071067811865487940, 0.7071067811865463515, 0.000000000000000000 ) ) ;
#11170 = VERTEX_POINT ( 'NONE', #100406 ) ;
#11171 = LINE ( 'NONE', #55448, #42456 ) ;
#11172 = CARTESIAN_POINT ( 'NONE',  ( 35.16170612452598476, -6.740707523384216415, 16.75550250614875836 ) ) ;
#11173 = LINE ( 'NONE', #45316, #66757 ) ;
#11174 = ORIENTED_EDGE ( 'NONE', *, *, #25728, .F. ) ;
#11175 = LINE ( 'NONE', #2457, #80893 ) ;
#11176 = FACE_OUTER_BOUND ( 'NONE', #89911, .T. ) ;
#11177 = CARTESIAN_POINT ( 'NONE',  ( 29.99999999999979394, -16.06887692260766087, 4.000000000000000000 ) ) ;
#11178 = ORIENTED_EDGE ( 'NONE', *, *, #60358, .T. ) ;
#11179 = FACE_OUTER_BOUND ( 'NONE', #19784, .T. ) ;
#11180 = LINE ( 'NONE', #34410, #78937 ) ;
#11181 = UNCERTAINTY_MEASURE_WITH_UNIT (LENGTH_MEASURE( 1.000000000000000082E-05 ), #23420, 'distance_accuracy_value', 'NONE');
#11182 = CARTESIAN_POINT ( 'NONE',  ( 131.5423521607622490, -52.00875322212550600, 39.33676470588235929 ) ) ;
#11183 = SURFACE_SIDE_STYLE ('',( #91477 ) ) ;
#11184 = LINE ( 'NONE', #130894, #129253 ) ;
#11185 = CARTESIAN_POINT ( 'NONE',  ( 69.47459685856475176, 1.637169565754164280, -6.109999999999997655 ) ) ;
#11186 = EDGE_CURVE ( 'NONE', #72863, #133600, #37282, .T. ) ;
#11187 = LINE ( 'NONE', #23531, #37143 ) ;
#11188 = LINE ( 'NONE', #33730, #55479 ) ;
#11189 = CARTESIAN_POINT ( 'NONE',  ( 32.89169371712954870, 2.130196079827421762, 7.950000000000000178 ) ) ;
#11190 = AXIS2_PLACEMENT_3D ( 'NONE', #2998, #123394, #13144 ) ;
#11191 = CARTESIAN_POINT ( 'NONE',  ( 4.828169399223496860, 15.75929247661555976, 4.000000000000000000 ) ) ;
#11192 = EDGE_LOOP ( 'NONE', ( #6135, #103139, #11813, #30520 ) ) ;
#11193 = LINE ( 'NONE', #34419, #106640 ) ;
#11194 = EDGE_LOOP ( 'NONE', ( #597, #101217, #21221, #118504 ) ) ;
#11195 = LINE ( 'NONE', #43173, #68667 ) ;
#11196 = DIRECTION ( 'NONE',  ( -0.000000000000000000, 0.3543493200069153248, 0.9351131265310292928 ) ) ;
#11197 = AXIS2_PLACEMENT_3D ( 'NONE', #2757, #22344, #78205 ) ;
#11198 = VECTOR ( 'NONE', #85526, 1000.000000000000000 ) ;
#11199 = VECTOR ( 'NONE', #87100, 1000.000000000000227 ) ;
#11200 = DIRECTION ( 'NONE',  ( -0.7071067811865487940, 0.7071067811865463515, -0.000000000000000000 ) ) ;
#11201 = CARTESIAN_POINT ( 'NONE',  ( 104.7875270504628986, 0.000000000000000000, -7.949999999999998401 ) ) ;
#11202 = LINE ( 'NONE', #55484, #97264 ) ;
#11203 = AXIS2_PLACEMENT_3D ( 'NONE', #25108, #125151, #112842 ) ;
#11204 = CARTESIAN_POINT ( 'NONE',  ( -8.994519915287490619, 28.92564299267944250, 4.000000000000000000 ) ) ;
#11205 = ORIENTED_EDGE ( 'NONE', *, *, #75456, .F. ) ;
#11206 = VERTEX_POINT ( 'NONE', #23541 ) ;
#11207 = DIRECTION ( 'NONE',  ( 0.000000000000000000, 0.000000000000000000, 1.000000000000000000 ) ) ;
#11208 = FACE_OUTER_BOUND ( 'NONE', #888, .T. ) ;
#11209 = UNCERTAINTY_MEASURE_WITH_UNIT (LENGTH_MEASURE( 1.000000000000000082E-05 ), #69662, 'distance_accuracy_value', 'NONE');
#11210 = MECHANICAL_DESIGN_GEOMETRIC_PRESENTATION_REPRESENTATION (  '', ( #29753 ), #129311 ) ;
#11211 = AXIS2_PLACEMENT_3D ( 'NONE', #126441, #16226, #5366 ) ;
#11212 = DIRECTION ( 'NONE',  ( -0.000000000000000000, 0.000000000000000000, 1.000000000000000000 ) ) ;
#11213 = PLANE ( 'NONE',  #108163 ) ;
#11214 = CARTESIAN_POINT ( 'NONE',  ( 81.74586038379622721, 3.974999999999996980, 6.884901960086287964 ) ) ;
#11215 = DIRECTION ( 'NONE',  ( 0.3543493200069162685, -0.000000000000000000, -0.9351131265310288487 ) ) ;
#11216 = EDGE_CURVE ( 'NONE', #78997, #12173, #3716, .T. ) ;
#11217 = DIRECTION ( 'NONE',  ( 0.9707728879609256456, 0.000000000000000000, -0.2400000000000085398 ) ) ;
#11218 = ORIENTED_EDGE ( 'NONE', *, *, #136515, .F. ) ;
#11219 = CARTESIAN_POINT ( 'NONE',  ( 69.54166666666667140, -3.975000000000002753, 6.884901960086286188 ) ) ;
#11220 = CARTESIAN_POINT ( 'NONE',  ( 15.29974487139158867, -27.71228299555216879, 4.000000000000000000 ) ) ;
#11221 = EDGE_CURVE ( 'NONE', #12102, #12477, #84785, .T. ) ;
#11222 = LINE ( 'NONE', #111268, #13831 ) ;
#11223 = CARTESIAN_POINT ( 'NONE',  ( -12.69999999999998153, 0.000000000000000000, 0.000000000000000000 ) ) ;
#11224 = VECTOR ( 'NONE', #53101, 1000.000000000000000 ) ;
#11225 = ORIENTED_EDGE ( 'NONE', *, *, #69089, .F. ) ;
#11226 = EDGE_CURVE ( 'NONE', #77764, #60323, #12653, .T. ) ;
#11227 = EDGE_CURVE ( 'NONE', #68726, #20176, #113388, .T. ) ;
#11228 = LINE ( 'NONE', #20704, #79271 ) ;
#11229 = ORIENTED_EDGE ( 'NONE', *, *, #92485, .F. ) ;
#11230 = AXIS2_PLACEMENT_3D ( 'NONE', #3219, #90238, #134482 ) ;
#11231 = FACE_OUTER_BOUND ( 'NONE', #77424, .T. ) ;
#11232 = CARTESIAN_POINT ( 'NONE',  ( 77.58376352523144703, -6.110000000000001208, -3.741295971395164515E-16 ) ) ;
#11233 = DIRECTION ( 'NONE',  ( 0.000000000000000000, 0.000000000000000000, 1.000000000000000000 ) ) ;
#11235 = VERTEX_POINT ( 'NONE', #112690 ) ;
#11234 = VECTOR ( 'NONE', #46421, 1000.000000000000000 ) ;
#11236 = DIRECTION ( 'NONE',  ( -0.7071067811865487940, 0.7071067811865463515, 0.000000000000000000 ) ) ;
#11237 = VECTOR ( 'NONE', #6356, 999.9999999999998863 ) ;
#11238 = DIRECTION ( 'NONE',  ( -0.7071067811865486830, 0.7071067811865464625, 0.000000000000000000 ) ) ;
#11239 = LINE ( 'NONE', #90254, #74392 ) ;
#11240 = AXIS2_PLACEMENT_3D ( 'NONE', #36324, #31165, #63795 ) ;
#11241 = EDGE_CURVE ( 'NONE', #71647, #24426, #47492, .T. ) ;
#11242 = PLANE ( 'NONE',  #39431 ) ;
#11243 = EDGE_CURVE ( 'NONE', #86591, #22993, #13356, .T. ) ;
#11244 = CARTESIAN_POINT ( 'NONE',  ( -14.51078643762690490, -27.52281430457045275, 5.000000000000000000 ) ) ;
#11246 = EDGE_LOOP ( 'NONE', ( #94858, #78679, #40210, #8156 ) ) ;
#11245 = CARTESIAN_POINT ( 'NONE',  ( 8.510786437626906675, -27.52281430457049183, 5.000000000000000000 ) ) ;
#11247 = CARTESIAN_POINT ( 'NONE',  ( 128.9683591370938416, -52.14999999999999147, -41.64500000000001023 ) ) ;
#11249 = B_SPLINE_CURVE_WITH_KNOTS ( 'NONE', 3,
 ( #96614, #51024, #139494, #140854, #82244, #38716, #82939, #11765 ),
 .UNSPECIFIED., .F., .F.,
 ( 4, 2, 2, 4 ),
 ( 2.778266744796018861E-17, 0.001415444524343407963, 0.002123166786515097524, 0.002830889048686786869 ),
 .UNSPECIFIED. ) ;
#11248 = DIRECTION ( 'NONE',  ( 0.7071067811865487940, 0.7071067811865463515, -0.000000000000000000 ) ) ;
#11250 = CARTESIAN_POINT ( 'NONE',  ( 23.48860328114998453, 7.166961737892989959, 4.667035327419719160 ) ) ;
#11251 = PLANE ( 'NONE',  #46143 ) ;
#11252 = VECTOR ( 'NONE', #629, 1000.000000000000000 ) ;
#11253 = ORIENTED_EDGE ( 'NONE', *, *, #116546, .F. ) ;
#11254 = EDGE_CURVE ( 'NONE', #80031, #32625, #124284, .T. ) ;
#11255 = ORIENTED_EDGE ( 'NONE', *, *, #42576, .F. ) ;
#11256 = CARTESIAN_POINT ( 'NONE',  ( 60.08376352523143993, -6.110000000000001208, -3.741295971395164515E-16 ) ) ;
#11257 = EDGE_LOOP ( 'NONE', ( #35928, #125200, #105636, #70712 ) ) ;
#11258 = DIRECTION ( 'NONE',  ( -1.000000000000000000, -0.000000000000000000, -0.000000000000000000 ) ) ;
#11259 = CARTESIAN_POINT ( 'NONE',  ( -5.292893218813420120, 5.259292476615661016, 5.000000000000000000 ) ) ;
#11260 = CARTESIAN_POINT ( 'NONE',  ( 9.208651418775088970, -2.500000000000000000, 3.061616997868383634E-16 ) ) ;
#11261 = CARTESIAN_POINT ( 'NONE',  ( 124.4750270504628844, -5.819803920172573086, 5.819803920172573086 ) ) ;
#11262 = CARTESIAN_POINT ( 'NONE',  ( 9.682526172861077640, -2.055000000000000160, 2.789133085058097101E-16 ) ) ;
#11263 = EDGE_LOOP ( 'NONE', ( #100659, #86757, #106197, #120648 ) ) ;
#11265 = EDGE_CURVE ( 'NONE', #41140, #48586, #25675, .T. ) ;
#11264 = ORIENTED_EDGE ( 'NONE', *, *, #110314, .F. ) ;
#11266 = VECTOR ( 'NONE', #133023, 1000.000000000000000 ) ;
#11267 = DIRECTION ( 'NONE',  ( -0.6830127018922181881, 0.6830127018922202975, -0.2588190451025214056 ) ) ;
#11268 = VERTEX_POINT ( 'NONE', #114120 ) ;
#11269 = CARTESIAN_POINT ( 'NONE',  ( 69.18398860626899705, 28.73617430169835529, 5.000000000000000000 ) ) ;
#11270 = CARTESIAN_POINT ( 'NONE',  ( 112.3708603837962272, 6.884901960086289741, -3.974999999999993427 ) ) ;
#11271 = EDGE_CURVE ( 'NONE', #65560, #18319, #31609, .T. ) ;
#11272 = DIRECTION ( 'NONE',  ( -0.000000000000000000, -0.3543493200069152693, 0.9351131265310292928 ) ) ;
#11273 = ORIENTED_EDGE ( 'NONE', *, *, #12891, .T. ) ;
#11274 = FACE_BOUND ( 'NONE', #139112, .T. ) ;
#11275 = CARTESIAN_POINT ( 'NONE',  ( 14.81601139373099585, 28.73617430169776910, 5.000000000000000000 ) ) ;
#11276 = EDGE_CURVE ( 'NONE', #120628, #116635, #85054, .T. ) ;
#11277 = CARTESIAN_POINT ( 'NONE',  ( 128.8886022459138019, 0.000000000000000000, -6.349999999999997868 ) ) ;
#11278 = CARTESIAN_POINT ( 'NONE',  ( 61.81249999999998579, 5.819803920172571310, 5.819803920172576639 ) ) ;
#11279 = EDGE_CURVE ( 'NONE', #37795, #139420, #16953, .T. ) ;
#11280 = DIRECTION ( 'NONE',  ( 0.3543493200069162685, -0.000000000000000000, -0.9351131265310288487 ) ) ;
#11281 = FACE_OUTER_BOUND ( 'NONE', #141308, .T. ) ;
#11283 = ADVANCED_FACE ( 'NONE', ( #82237 ), #50305, .F. ) ;
#11282 = SURFACE_STYLE_FILL_AREA ( #120782 ) ;
#11284 = ORIENTED_EDGE ( 'NONE', *, *, #129750, .F. ) ;
#11285 = ORIENTED_EDGE ( 'NONE', *, *, #61707, .T. ) ;
#11286 = CARTESIAN_POINT ( 'NONE',  ( 106.9537635252314516, -6.109999999999998543, -3.741295971395162543E-16 ) ) ;
#11287 = ORIENTED_EDGE ( 'NONE', *, *, #25478, .T. ) ;
#11288 = VERTEX_POINT ( 'NONE', #137316 ) ;
#11289 = DIRECTION ( 'NONE',  ( -0.000000000000000000, -0.3543493200069152693, 0.9351131265310292928 ) ) ;
#11290 = CARTESIAN_POINT ( 'NONE',  ( 30.18398860626900060, 28.73617430169808173, 5.000000000000000000 ) ) ;
#11291 = VERTEX_POINT ( 'NONE', #94492 ) ;
#11292 = CARTESIAN_POINT ( 'NONE',  ( 34.45011844616453089, -17.99769585840587638, 5.000000000000001776 ) ) ;
#11293 = DIRECTION ( 'NONE',  ( -0.6830127018922180770, -0.6830127018922204085, -0.2588190451025214056 ) ) ;
#11294 = FACE_OUTER_BOUND ( 'NONE', #15248, .T. ) ;
#11295 = DIRECTION ( 'NONE',  ( -0.000000000000000000, -0.3543493200069152693, 0.9351131265310292928 ) ) ;
#11296 = DIRECTION ( 'NONE',  ( -0.7071067811865487940, 0.7071067811865463515, 0.000000000000000000 ) ) ;
#11297 = VECTOR ( 'NONE', #38101, 1000.000000000000000 ) ;
#11298 = VECTOR ( 'NONE', #30856, 1000.000000000000000 ) ;
#11299 = CARTESIAN_POINT ( 'NONE',  ( -5.816011393731002066, 28.73617430169783304, 5.000000000000000000 ) ) ;
#11300 = VECTOR ( 'NONE', #108244, 1000.000000000000000 ) ;
#11301 = ORIENTED_EDGE ( 'NONE', *, *, #75926, .T. ) ;
#11302 = DIRECTION ( 'NONE',  ( 0.7071067811865486830, -0.7071067811865464625, -0.000000000000000000 ) ) ;
#11303 = CARTESIAN_POINT ( 'NONE',  ( -15.48921356237309510, -27.52281430457066236, 5.000000000000000000 ) ) ;
#11304 = VECTOR ( 'NONE', #123147, 1000.000000000000000 ) ;
#11305 = ORIENTED_EDGE ( 'NONE', *, *, #25557, .F. ) ;
#11306 = ORIENTED_EDGE ( 'NONE', *, *, #106985, .T. ) ;
#11307 = ORIENTED_EDGE ( 'NONE', *, *, #18303, .T. ) ;
#11308 = CARTESIAN_POINT ( 'NONE',  ( 54.68793019189810423, 6.110000000000002984, -1.637169565754156730 ) ) ;
#11309 = ORIENTED_EDGE ( 'NONE', *, *, #116652, .T. ) ;
#11310 = AXIS2_PLACEMENT_3D ( 'NONE', #123413, #58173, #89325 ) ;
#11311 = CARTESIAN_POINT ( 'NONE',  ( 11.72733514412567857, 3.061616997868383634E-16, -2.500000000000000444 ) ) ;
#11312 = CARTESIAN_POINT ( 'NONE',  ( -0.8291937171295610254, -3.047499999999997211, -5.278424836066143655 ) ) ;
#11313 = CARTESIAN_POINT ( 'NONE',  ( 91.14626352523144703, -4.472830434245840259, 4.472830434245838482 ) ) ;
#11314 = DIRECTION ( 'NONE',  ( -0.3543493200069162685, -0.000000000000000000, -0.9351131265310288487 ) ) ;
#11315 = ORIENTED_EDGE ( 'NONE', *, *, #39848, .T. ) ;
#11316 = PLANE ( 'NONE',  #18655 ) ;
#11317 = EDGE_CURVE ( 'NONE', #109641, #116177, #40845, .T. ) ;
#11318 = VECTOR ( 'NONE', #52231, 1000.000000000000000 ) ;
#11319 = VECTOR ( 'NONE', #85082, 999.9999999999998863 ) ;
#11320 = DIRECTION ( 'NONE',  ( -0.6830127018922181881, 0.6830127018922202975, -0.2588190451025214056 ) ) ;
#11321 = PLANE ( 'NONE',  #40568 ) ;
#11322 = VERTEX_POINT ( 'NONE', #38707 ) ;
#11323 = VECTOR ( 'NONE', #24116, 1000.000000000000227 ) ;
#11324 = CARTESIAN_POINT ( 'NONE',  ( -8.999999999999941380, 7.931123077392104648, 4.000000000000000000 ) ) ;
#11325 = FACE_OUTER_BOUND ( 'NONE', #6881, .T. ) ;
#11326 = ORIENTED_EDGE ( 'NONE', *, *, #15356, .T. ) ;
#11327 = VERTEX_POINT ( 'NONE', #106793 ) ;
#11328 = VERTEX_POINT ( 'NONE', #82933 ) ;
#11329 = CARTESIAN_POINT ( 'NONE',  ( 124.5995968585647802, -6.109999999999997655, -1.637169565754160283 ) ) ;
#11330 = VECTOR ( 'NONE', #127920, 1000.000000000000000 ) ;
#11331 = VECTOR ( 'NONE', #141031, 1000.000000000000000 ) ;
#11332 = DIRECTION ( 'NONE',  ( -0.000000000000000000, 0.000000000000000000, 1.000000000000000000 ) ) ;
#11333 = AXIS2_PLACEMENT_3D ( 'NONE', #49048, #114953, #81690 ) ;
#11334 = EDGE_CURVE ( 'NONE', #14833, #58719, #62610, .T. ) ;
#11335 = DIRECTION ( 'NONE',  ( 0.6830127018922180770, -0.6830127018922204085, -0.2588190451025213501 ) ) ;
#11336 = ORIENTED_EDGE ( 'NONE', *, *, #123718, .T. ) ;
#11337 = EDGE_CURVE ( 'NONE', #129172, #59038, #105371, .T. ) ;
#11338 = CARTESIAN_POINT ( 'NONE',  ( 20.58838509405154582, 22.22500000000000853, 4.777194822843815913 ) ) ;
#11339 = ORIENTED_EDGE ( 'NONE', *, *, #128639, .F. ) ;
#11340 = VECTOR ( 'NONE', #98439, 1000.000000000000000 ) ;
#11341 = AXIS2_PLACEMENT_3D ( 'NONE', #60624, #21173, #97267 ) ;
#11342 = CARTESIAN_POINT ( 'NONE',  ( 15.58290314143522082, 3.967499999999992699, -6.871911579029513994 ) ) ;
#11343 = DIRECTION ( 'NONE',  ( -1.000000000000000000, -3.115803279706882722E-16, 0.000000000000000000 ) ) ;
#11344 = EDGE_CURVE ( 'NONE', #110391, #63778, #51015, .T. ) ;
#11345 = DIRECTION ( 'NONE',  ( -0.7071067811865486830, -0.7071067811865464625, -0.000000000000000000 ) ) ;
#11346 = ORIENTED_EDGE ( 'NONE', *, *, #140544, .T. ) ;
#11347 = ORIENTED_EDGE ( 'NONE', *, *, #47910, .F. ) ;
#11348 = ORIENTED_EDGE ( 'NONE', *, *, #130896, .F. ) ;
#11349 = CARTESIAN_POINT ( 'NONE',  ( -27.18398860626900060, 28.73617430169806042, 5.000000000000000000 ) ) ;
#11350 = FACE_BOUND ( 'NONE', #38408, .T. ) ;
#11351 = VECTOR ( 'NONE', #96578, 1000.000000000000227 ) ;
#11352 = PLANE ( 'NONE',  #82075 ) ;
#11353 = DIRECTION ( 'NONE',  ( -0.7071067811865486830, -0.7071067811865464625, 0.000000000000000000 ) ) ;
#11354 = EDGE_CURVE ( 'NONE', #60934, #113076, #48880, .T. ) ;
#11355 = PLANE ( 'NONE',  #43775 ) ;
#11356 = CARTESIAN_POINT ( 'NONE',  ( 34.47516574401890921, 16.49051761211545752, 4.998110765256835286 ) ) ;
#11357 = LINE ( 'NONE', #99836, #4638 ) ;
#11358 = DIRECTION ( 'NONE',  ( -0.7071067811865487940, 0.7071067811865463515, 0.000000000000000000 ) ) ;
#11359 = ORIENTED_EDGE ( 'NONE', *, *, #36713, .F. ) ;
#11360 = CARTESIAN_POINT ( 'NONE',  ( -17.99999999999986855, -4.068876922607775448, 4.000000000000000000 ) ) ;
#11361 = ORIENTED_EDGE ( 'NONE', *, *, #5244, .F. ) ;
#11362 = ADVANCED_FACE ( 'NONE', ( #29242 ), #139486, .F. ) ;
#11363 = EDGE_CURVE ( 'NONE', #87598, #36751, #72815, .T. ) ;
#11364 = CARTESIAN_POINT ( 'NONE',  ( -2.816011393730999401, 28.73617430169785436, 5.000000000000000000 ) ) ;
#11365 = ORIENTED_EDGE ( 'NONE', *, *, #59800, .F. ) ;
#11366 = CARTESIAN_POINT ( 'NONE',  ( -33.48921356237309510, -27.52281430457078670, 5.000000000000000000 ) ) ;
#11368 = ORIENTED_EDGE ( 'NONE', *, *, #131184, .F. ) ;
#11367 = CARTESIAN_POINT ( 'NONE',  ( -0.4892135623730947680, -27.52281430457055578, 5.000000000000000000 ) ) ;
#11369 = PLANE ( 'NONE',  #106477 ) ;
#11370 = DIRECTION ( 'NONE',  ( 0.7071067811865487940, -0.7071067811865463515, 0.000000000000000000 ) ) ;
#11371 = ORIENTED_EDGE ( 'NONE', *, *, #46718, .T. ) ;
#11372 = CARTESIAN_POINT ( 'NONE',  ( 34.92499999999998295, 9.759292476615621936, 4.255531930566176513 ) ) ;
#11373 = ORIENTED_EDGE ( 'NONE', *, *, #18742, .T. ) ;
#11374 = CARTESIAN_POINT ( 'NONE',  ( 36.18398860626899705, 28.73617430169812437, 5.000000000000000000 ) ) ;
#11375 = ORIENTED_EDGE ( 'NONE', *, *, #115461, .T. ) ;
#11376 = CARTESIAN_POINT ( 'NONE',  ( -34.82816939922328459, -11.24070752338416135, 4.000000000000000000 ) ) ;
#11377 = CARTESIAN_POINT ( 'NONE',  ( 114.1208603837962414, -6.884901960086286188, 3.974999999999997424 ) ) ;
#11378 = DIRECTION ( 'NONE',  ( 1.000000000000000000, 0.000000000000000000, 0.000000000000000000 ) ) ;
#11379 = DIRECTION ( 'NONE',  ( -0.7071067811865486830, -0.7071067811865464625, 0.000000000000000000 ) ) ;
#11380 = CARTESIAN_POINT ( 'NONE',  ( -2.843876922607561752, -22.22500000000000142, 4.000000000000000000 ) ) ;
#11382 = EDGE_CURVE ( 'NONE', #141849, #118741, #27102, .T. ) ;
#11381 = CARTESIAN_POINT ( 'NONE',  ( 2.501836514860421801, -17.24070752338410273, 8.407044977365218941 ) ) ;
#11383 = CARTESIAN_POINT ( 'NONE',  ( 22.49999999999984723, -6.839392718269110105, -8.480912228396139341 ) ) ;
#11384 = CARTESIAN_POINT ( 'NONE',  ( 13.70833333333333393, 3.047499999999997655, 5.278424836066143655 ) ) ;
#11385 = DIRECTION ( 'NONE',  ( 0.000000000000000000, -1.000000000000000000, 0.000000000000000000 ) ) ;
#11386 = CARTESIAN_POINT ( 'NONE',  ( -24.49816348513941833, -17.24070752338410628, 8.407044977365281113 ) ) ;
#11387 = DIRECTION ( 'NONE',  ( -0.000000000000000000, -0.3543493200069152693, 0.9351131265310292928 ) ) ;
#11388 = ORIENTED_EDGE ( 'NONE', *, *, #120883, .T. ) ;
#11390 = VERTEX_POINT ( 'NONE', #71345 ) ;
#11389 = ADVANCED_FACE ( 'NONE', ( #18332 ), #15482, .F. ) ;
#11391 = EDGE_CURVE ( 'NONE', #65367, #36132, #15315, .T. ) ;
#11392 = DIRECTION ( 'NONE',  ( -0.000000000000000000, -0.3543493200069152693, 0.9351131265310292928 ) ) ;
#11393 = VERTEX_POINT ( 'NONE', #126411 ) ;
#11394 = AXIS2_PLACEMENT_3D ( 'NONE', #18867, #107308, #23887 ) ;
#11395 = CARTESIAN_POINT ( 'NONE',  ( 106.6045968585647472, 1.637169565754164946, -6.109999999999999432 ) ) ;
#11396 = CARTESIAN_POINT ( 'NONE',  ( -30.18398860626900060, 28.73617430169808173, 5.000000000000000000 ) ) ;
#11397 = LINE ( 'NONE', #12845, #71818 ) ;
#11398 = DIRECTION ( 'NONE',  ( -0.000000000000000000, 0.3543493200069153248, 0.9351131265310292928 ) ) ;
#11399 =( NAMED_UNIT ( * ) SI_UNIT ( $, .STERADIAN. ) SOLID_ANGLE_UNIT ( ) );
#11400 = ORIENTED_EDGE ( 'NONE', *, *, #102313, .F. ) ;
#11401 = VECTOR ( 'NONE', #77530, 1000.000000000000227 ) ;
#11402 = CIRCLE ( 'NONE', #13686, 3.000000000000000444 ) ;
#11403 = EDGE_CURVE ( 'NONE', #106511, #50767, #116264, .T. ) ;
#11404 = DIRECTION ( 'NONE',  ( -0.3543493200069162685, -0.000000000000000000, -0.9351131265310288487 ) ) ;
#11405 = AXIS2_PLACEMENT_3D ( 'NONE', #121512, #21510, #99768 ) ;
#11406 = CARTESIAN_POINT ( 'NONE',  ( -22.17183060077631751, -14.24070752338413293, 4.000000000000000000 ) ) ;
#11407 = EDGE_CURVE ( 'NONE', #21343, #16391, #5335, .T. ) ;
#11408 = PLANE ( 'NONE',  #20768 ) ;
#11409 = EDGE_CURVE ( 'NONE', #17718, #122293, #26935, .T. ) ;
#11410 = FILL_AREA_STYLE ('',( #110726 ) ) ;
#11412 = ORIENTED_EDGE ( 'NONE', *, *, #20737, .F. ) ;
#11411 = PLANE ( 'NONE',  #89163 ) ;
#11413 = CARTESIAN_POINT ( 'NONE',  ( 15.18398860626900237, 28.73617430169797871, 5.000000000000000000 ) ) ;
#11414 = CARTESIAN_POINT ( 'NONE',  ( 19.60343192894631414, -14.24070752338413293, 19.24067776001730223 ) ) ;
#11415 = LINE ( 'NONE', #53541, #93260 ) ;
#11416 = FACE_OUTER_BOUND ( 'NONE', #22922, .T. ) ;
#11417 = VECTOR ( 'NONE', #123237, 1000.000000000000000 ) ;
#11418 = PLANE ( 'NONE',  #9900 ) ;
#11419 = ORIENTED_EDGE ( 'NONE', *, *, #2742, .F. ) ;
#11420 = VERTEX_POINT ( 'NONE', #17636 ) ;
#11421 = ORIENTED_EDGE ( 'NONE', *, *, #45142, .F. ) ;
#11423 = EDGE_CURVE ( 'NONE', #56879, #16801, #97325, .T. ) ;
#11422 = CARTESIAN_POINT ( 'NONE',  ( 94.20876352523144703, -7.482591942790329030E-16, 6.110000000000001208 ) ) ;
#11424 = ORIENTED_EDGE ( 'NONE', *, *, #66726, .F. ) ;
#11425 = EDGE_CURVE ( 'NONE', #108094, #51277, #71051, .T. ) ;
#11426 = LINE ( 'NONE', #45563, #125002 ) ;
#11427 = DIRECTION ( 'NONE',  ( 0.3543493200069162685, -0.000000000000000000, -0.9351131265310288487 ) ) ;
#11428 = VECTOR ( 'NONE', #52071, 1000.000000000000114 ) ;
#11429 = VECTOR ( 'NONE', #26378, 1000.000000000000227 ) ;
#11430 = FACE_OUTER_BOUND ( 'NONE', #82029, .T. ) ;
#11431 = FACE_OUTER_BOUND ( 'NONE', #5771, .T. ) ;
#11432 = VERTEX_POINT ( 'NONE', #29946 ) ;
#11433 = EDGE_CURVE ( 'NONE', #98689, #2221, #138190, .T. ) ;
#11434 = DIRECTION ( 'NONE',  ( -0.000000000000000000, 0.3543493200069153248, 0.9351131265310292928 ) ) ;
#11436 =( BOUNDED_CURVE ( )  B_SPLINE_CURVE ( 3, ( #52247, #63163, #129804, #19616 ),
 .UNSPECIFIED., .F., .F. ) 
 B_SPLINE_CURVE_WITH_KNOTS ( ( 4, 4 ),
 ( 5.043186909253406291, 5.074607125596347856 ),
 .UNSPECIFIED. ) 
 CURVE ( )  GEOMETRIC_REPRESENTATION_ITEM ( )  RATIONAL_B_SPLINE_CURVE ( ( 1.000000000000000000, 0.9999177325257868620, 0.9999177325257868620, 1.000000000000000000 ) ) 
 REPRESENTATION_ITEM ( '' )  );
#11435 = LINE ( 'NONE', #75321, #136851 ) ;
#11437 = VECTOR ( 'NONE', #130944, 1000.000000000000227 ) ;
#11438 = CARTESIAN_POINT ( 'NONE',  ( 86.82876352523145158, 0.000000000000000000, -6.109999999999998543 ) ) ;
#11439 = EDGE_LOOP ( 'NONE', ( #65281, #74381, #72542, #22901 ) ) ;
#11440 = DIRECTION ( 'NONE',  ( 0.7071067811865487940, -0.7071067811865463515, 0.000000000000000000 ) ) ;
#11441 = CARTESIAN_POINT ( 'NONE',  ( -33.31657961132769685, -6.740707523384209310, 11.88629033278132496 ) ) ;
#11442 = AXIS2_PLACEMENT_3D ( 'NONE', #8064, #96487, #108795 ) ;
#11443 = AXIS2_PLACEMENT_3D ( 'NONE', #87914, #11757, #19794 ) ;
#11444 = CIRCLE ( 'NONE', #64678, 2.055000000000000604 ) ;
#11445 = VERTEX_POINT ( 'NONE', #8857 ) ;
#11446 = ORIENTED_EDGE ( 'NONE', *, *, #92415, .F. ) ;
#11447 = ORIENTED_EDGE ( 'NONE', *, *, #128759, .T. ) ;
#11448 = CARTESIAN_POINT ( 'NONE',  ( -57.48921356237308800, -27.52281430457095368, 5.000000000000000000 ) ) ;
#11449 = VECTOR ( 'NONE', #127138, 1000.000000000000227 ) ;
#11450 = DIRECTION ( 'NONE',  ( -0.3543493200069163795, -9.265275131829747941E-33, -0.9351131265310288487 ) ) ;
#11451 = CARTESIAN_POINT ( 'NONE',  ( 15.23373647476855375, 5.808823158059035485, 5.808823158059032821 ) ) ;
#11452 = FACE_OUTER_BOUND ( 'NONE', #99432, .T. ) ;
#11453 = AXIS2_PLACEMENT_3D ( 'NONE', #118588, #51932, #109142 ) ;
#11454 = CARTESIAN_POINT ( 'NONE',  ( -10.49999999999992539, 13.46639925780212366, 5.000000000000000000 ) ) ;
#11455 = DIRECTION ( 'NONE',  ( 0.000000000000000000, 1.000000000000000000, 0.000000000000000000 ) ) ;
#11456 = EDGE_CURVE ( 'NONE', #99319, #127035, #119796, .T. ) ;
#11457 = LINE ( 'NONE', #57889, #130716 ) ;
#11458 = EDGE_CURVE ( 'NONE', #46893, #59884, #131429, .T. ) ;
#11459 = VERTEX_POINT ( 'NONE', #120498 ) ;
#11460 = EDGE_LOOP ( 'NONE', ( #66438, #10459, #115132, #124448 ) ) ;
#11461 = CARTESIAN_POINT ( 'NONE',  ( 12.69999999999999574, -22.26999999999999247, -0.2071067811865477670 ) ) ;
#11462 = VERTEX_POINT ( 'NONE', #75623 ) ;
#11463 = ORIENTED_EDGE ( 'NONE', *, *, #111778, .F. ) ;
#11464 = AXIS2_PLACEMENT_3D ( 'NONE', #138369, #108371, #1746 ) ;
#11465 = EDGE_CURVE ( 'NONE', #58699, #71262, #43697, .T. ) ;
#11466 = DIRECTION ( 'NONE',  ( -0.7071067811865486830, -0.7071067811865464625, 0.000000000000000000 ) ) ;
#11467 = EDGE_LOOP ( 'NONE', ( #129244, #91493, #71513, #39499 ) ) ;
#11468 = FACE_OUTER_BOUND ( 'NONE', #31486, .T. ) ;
#11469 = LINE ( 'NONE', #78206, #3125 ) ;
#11470 = CARTESIAN_POINT ( 'NONE',  ( 34.42499999999998295, -19.45860074219776692, 5.000000000000000000 ) ) ;
#11471 = CARTESIAN_POINT ( 'NONE',  ( 67.50000000000000000, 0.000000000000000000, -7.950000000000000178 ) ) ;
#11472 = DIRECTION ( 'NONE',  ( 0.000000000000000000, 0.000000000000000000, 1.000000000000000000 ) ) ;
#11473 = ORIENTED_EDGE ( 'NONE', *, *, #53467, .T. ) ;
#11474 = FACE_OUTER_BOUND ( 'NONE', #49991, .T. ) ;
#11475 = ORIENTED_EDGE ( 'NONE', *, *, #137002, .F. ) ;
#11476 = FACE_OUTER_BOUND ( 'NONE', #73966, .T. ) ;
#11477 = ORIENTED_EDGE ( 'NONE', *, *, #57378, .T. ) ;
#11478 = CARTESIAN_POINT ( 'NONE',  ( 26.75159235450331963, 9.902892378096218942E-16, 0.000000000000000000 ) ) ;
#11479 = VERTEX_POINT ( 'NONE', #107518 ) ;
#11480 = DIRECTION ( 'NONE',  ( 0.3543493200069162685, -0.000000000000000000, -0.9351131265310288487 ) ) ;
#11481 = ORIENTED_EDGE ( 'NONE', *, *, #29731, .T. ) ;
#11482 = ORIENTED_EDGE ( 'NONE', *, *, #116056, .F. ) ;
#11483 = ORIENTED_EDGE ( 'NONE', *, *, #19732, .F. ) ;
#11484 = DIRECTION ( 'NONE',  ( 0.6830127018922181881, 0.6830127018922202975, -0.2588190451025214056 ) ) ;
#11485 = DIRECTION ( 'NONE',  ( -0.7071067811865486830, -0.7071067811865464625, -0.000000000000000000 ) ) ;
#11486 = DIRECTION ( 'NONE',  ( -1.000000000000000000, -1.224606353822377258E-16, -0.000000000000000000 ) ) ;
#11487 = FACE_OUTER_BOUND ( 'NONE', #14834, .T. ) ;
#11488 = DIRECTION ( 'NONE',  ( 0.7071067811865487940, 0.7071067811865463515, 0.000000000000000000 ) ) ;
#11489 = CARTESIAN_POINT ( 'NONE',  ( 24.18398860626899705, 28.73617430169804265, 5.000000000000000000 ) ) ;
#11490 = DIRECTION ( 'NONE',  ( 0.7071067811865486830, -0.7071067811865464625, -0.000000000000000000 ) ) ;
#11491 = CARTESIAN_POINT ( 'NONE',  ( -29.99999999999979039, 1.761378380278656675, -6.096875308897323542 ) ) ;
#11492 = EDGE_LOOP ( 'NONE', ( #101238, #139912, #32168, #122033 ) ) ;
#11493 = DIRECTION ( 'NONE',  ( -0.7071067811865486830, -0.7071067811865464625, 0.000000000000000000 ) ) ;
#11494 = PLANE ( 'NONE',  #7772 ) ;
#11495 = ORIENTED_EDGE ( 'NONE', *, *, #4997, .T. ) ;
#11496 = ORIENTED_EDGE ( 'NONE', *, *, #32543, .F. ) ;
#11497 = VERTEX_POINT ( 'NONE', #98084 ) ;
#11498 = LINE ( 'NONE', #111566, #91202 ) ;
#11499 = AXIS2_PLACEMENT_3D ( 'NONE', #119047, #129202, #95152 ) ;
#11500 = VECTOR ( 'NONE', #99078, 1000.000000000000000 ) ;
#11501 = ORIENTED_EDGE ( 'NONE', *, *, #129106, .F. ) ;
#11502 = VECTOR ( 'NONE', #106469, 1000.000000000000227 ) ;
#11505 = ORIENTED_EDGE ( 'NONE', *, *, #112209, .T. ) ;
#11504 = EDGE_CURVE ( 'NONE', #92319, #65131, #132155, .T. ) ;
#11503 = AXIS2_PLACEMENT_3D ( 'NONE', #17570, #71279, #129188 ) ;
#11506 = LINE ( 'NONE', #134054, #58402 ) ;
#11507 = PLANE ( 'NONE',  #75677 ) ;
#11508 = FACE_OUTER_BOUND ( 'NONE', #21459, .T. ) ;
#11509 = ADVANCED_FACE ( 'NONE', ( #98770 ), #21227, .F. ) ;
#11510 = LINE ( 'NONE', #55792, #75082 ) ;
#11511 = LINE ( 'NONE', #55793, #92651 ) ;
#11512 = ORIENTED_EDGE ( 'NONE', *, *, #48108, .F. ) ;
#11513 = CARTESIAN_POINT ( 'NONE',  ( -13.82816939922343025, -8.240707523384196875, 4.000000000000000000 ) ) ;
#11515 = ORIENTED_EDGE ( 'NONE', *, *, #20664, .T. ) ;
#11514 = AXIS2_PLACEMENT_3D ( 'NONE', #55496, #112016, #111263 ) ;
#11517 = EDGE_CURVE ( 'NONE', #112409, #41303, #141592, .T. ) ;
#11516 = DIRECTION ( 'NONE',  ( -1.000000000000000000, 0.000000000000000000, -0.000000000000000000 ) ) ;
#11518 = EDGE_CURVE ( 'NONE', #94849, #138021, #44447, .T. ) ;
#11519 = CARTESIAN_POINT ( 'NONE',  ( 14.79623647476855375, 7.934999999999990727, -1.457635852685135314E-15 ) ) ;
#11520 = ORIENTED_EDGE ( 'NONE', *, *, #68335, .T. ) ;
#11521 = CARTESIAN_POINT ( 'NONE',  ( 79.97459685856479439, 1.637169565754164280, -6.109999999999997655 ) ) ;
#11522 = DIRECTION ( 'NONE',  ( -0.6830127018922181881, 0.6830127018922202975, -0.2588190451025214056 ) ) ;
#11523 = EDGE_CURVE ( 'NONE', #95983, #14590, #32848, .T. ) ;
#11524 = DIRECTION ( 'NONE',  ( -0.000000000000000000, -0.3543493200069152693, 0.9351131265310292928 ) ) ;
#11525 = VERTEX_POINT ( 'NONE', #109663 ) ;
#11526 = ORIENTED_EDGE ( 'NONE', *, *, #95553, .T. ) ;
#11527 = ORIENTED_EDGE ( 'NONE', *, *, #132226, .F. ) ;
#11529 = AXIS2_PLACEMENT_3D ( 'NONE', #135030, #135713, #134287 ) ;
#11528 = DIRECTION ( 'NONE',  ( -0.7071067811865486830, 0.7071067811865464625, 0.000000000000000000 ) ) ;
#11530 = PLANE ( 'NONE',  #125061 ) ;
#11532 = PLANE ( 'NONE',  #76638 ) ;
#11531 = AXIS2_PLACEMENT_3D ( 'NONE', #106687, #84288, #128483 ) ;
#11533 = CARTESIAN_POINT ( 'NONE',  ( 16.93289034258302550, -0.6086847910684115570, -34.86941310074139011 ) ) ;
#11534 = CARTESIAN_POINT ( 'NONE',  ( -1.499999999999990896, 3.431123077392149501, 4.000000000000000000 ) ) ;
#11535 = VERTEX_POINT ( 'NONE', #77071 ) ;
#11536 = CARTESIAN_POINT ( 'NONE',  ( 36.48921356237310221, -27.52281430457080802, 5.000000000000000000 ) ) ;
#11537 = EDGE_CURVE ( 'NONE', #88432, #12339, #110352, .T. ) ;
#11538 = PLANE ( 'NONE',  #67455 ) ;
#11539 = DIRECTION ( 'NONE',  ( -0.7071067811865486830, -0.7071067811865464625, -0.000000000000000000 ) ) ;
#11540 = ORIENTED_EDGE ( 'NONE', *, *, #52236, .T. ) ;
#11541 = CARTESIAN_POINT ( 'NONE',  ( -12.29974487139158512, -27.71228299555214747, 4.000000000000000000 ) ) ;
#11542 = ADVANCED_FACE ( 'NONE', ( #130733 ), #31400, .T. ) ;
#11544 = VECTOR ( 'NONE', #68884, 1000.000000000000000 ) ;
#11543 = CARTESIAN_POINT ( 'NONE',  ( -34.92500000000001137, -22.22500000000000142, 4.000000000000000000 ) ) ;
#11545 = ORIENTED_EDGE ( 'NONE', *, *, #8084, .T. ) ;
#11547 = ORIENTED_EDGE ( 'NONE', *, *, #55115, .T. ) ;
#11546 = PLANE ( 'NONE',  #69518 ) ;
#11548 = VERTEX_POINT ( 'NONE', #11027 ) ;
#11549 = CARTESIAN_POINT ( 'NONE',  ( 31.98012225071433789, -17.24070752338409562, 20.23474786156476313 ) ) ;
#11550 = AXIS2_PLACEMENT_3D ( 'NONE', #6950, #115718, #84579 ) ;
#11551 = CARTESIAN_POINT ( 'NONE',  ( 26.99999999999981526, -18.41253812416056590, 4.000000000000000000 ) ) ;
#11552 = EDGE_CURVE ( 'NONE', #949, #112797, #52417, .T. ) ;
#11553 = ORIENTED_EDGE ( 'NONE', *, *, #30145, .T. ) ;
#11554 = UNCERTAINTY_MEASURE_WITH_UNIT (LENGTH_MEASURE( 1.000000000000000082E-05 ), #123803, 'distance_accuracy_value', 'NONE');
#11555 = LINE ( 'NONE', #100042, #15052 ) ;
#11556 = CARTESIAN_POINT ( 'NONE',  ( -25.49999999999982592, -12.66682484999669178, -0.6294897503864504973 ) ) ;
#11557 = VECTOR ( 'NONE', #20580, 1000.000000000000000 ) ;
#11558 = FACE_OUTER_BOUND ( 'NONE', #91823, .T. ) ;
#11559 = FACE_OUTER_BOUND ( 'NONE', #51733, .T. ) ;
#11560 = DIRECTION ( 'NONE',  ( 0.6830127018922181881, 0.6830127018922202975, -0.2588190451025214056 ) ) ;
#11562 = EDGE_CURVE ( 'NONE', #11751, #35892, #143008, .T. ) ;
#11561 = FACE_OUTER_BOUND ( 'NONE', #133698, .T. ) ;
#11563 = CARTESIAN_POINT ( 'NONE',  ( 19.49999999999987210, -11.94781430457070215, 5.000000000000000000 ) ) ;
#11565 = VECTOR ( 'NONE', #24100, 1000.000000000000000 ) ;
#11564 = CARTESIAN_POINT ( 'NONE',  ( 18.35373647476854941, -5.808823158059035485, -5.808823158059033709 ) ) ;
#11566 = LINE ( 'NONE', #53701, #127750 ) ;
#11567 = DIRECTION ( 'NONE',  ( -0.000000000000000000, 0.000000000000000000, 1.000000000000000000 ) ) ;
#11568 = CARTESIAN_POINT ( 'NONE',  ( -2.292986735706930457, -21.74070752338405299, 4.999753212805217117 ) ) ;
#11569 = LINE ( 'NONE', #55850, #29171 ) ;
#11570 = ORIENTED_EDGE ( 'NONE', *, *, #119608, .T. ) ;
#11571 = EDGE_LOOP ( 'NONE', ( #91312, #74018, #129542, #51838 ) ) ;
#11572 = EDGE_CURVE ( 'NONE', #138595, #68933, #30703, .T. ) ;
#11573 = CARTESIAN_POINT ( 'NONE',  ( 103.9583333333333286, 3.974999999999997424, 6.884901960086288852 ) ) ;
#11574 = VERTEX_POINT ( 'NONE', #87203 ) ;
#11575 = ORIENTED_EDGE ( 'NONE', *, *, #31558, .F. ) ;
#11576 = EDGE_CURVE ( 'NONE', #51437, #139749, #64029, .T. ) ;
#11577 = ORIENTED_EDGE ( 'NONE', *, *, #3520, .F. ) ;
#11578 = DIRECTION ( 'NONE',  ( -0.000000000000000000, 0.3543493200069153248, 0.9351131265310292928 ) ) ;
#11579 = PLANE ( 'NONE',  #143499 ) ;
#11580 = AXIS2_PLACEMENT_3D ( 'NONE', #77709, #110294, #98717 ) ;
#11581 = ORIENTED_EDGE ( 'NONE', *, *, #126480, .T. ) ;
#11582 = CARTESIAN_POINT ( 'NONE',  ( 2.301729841053981485, -4.814824860968089633E-32, 2.500000000000000444 ) ) ;
#11583 = EDGE_CURVE ( 'NONE', #10965, #11574, #77767, .T. ) ;
#11584 =( NAMED_UNIT ( * ) PLANE_ANGLE_UNIT ( ) SI_UNIT ( $, .RADIAN. ) );
#11585 = CARTESIAN_POINT ( 'NONE',  ( 0.000000000000000000, 0.000000000000000000, 5.000000000000000000 ) ) ;
#11586 = DIRECTION ( 'NONE',  ( -0.7071067811865486830, -0.7071067811865464625, 0.000000000000000000 ) ) ;
#11587 = ORIENTED_EDGE ( 'NONE', *, *, #27688, .T. ) ;
#11588 = CARTESIAN_POINT ( 'NONE',  ( 1.499999999999992673, -1.912538124160737318, 4.000000000000000000 ) ) ;
#11589 = FACE_OUTER_BOUND ( 'NONE', #38532, .T. ) ;
#11590 = LINE ( 'NONE', #727, #15069 ) ;
#11591 = CIRCLE ( 'NONE', #92629, 2.500000000000000888 ) ;
#11592 = DIRECTION ( 'NONE',  ( -0.000000000000000000, 0.000000000000000000, 1.000000000000000000 ) ) ;
#11593 = DIRECTION ( 'NONE',  ( 1.000000000000000000, 1.224606353822377258E-16, 0.000000000000000000 ) ) ;
#11594 = CARTESIAN_POINT ( 'NONE',  ( 86.26669371712955581, -7.949999999999998401, 2.130196079827423983 ) ) ;
#11595 = DIRECTION ( 'NONE',  ( -0.3543493200069162685, -0.000000000000000000, -0.9351131265310288487 ) ) ;
#11596 = ORIENTED_EDGE ( 'NONE', *, *, #47022, .F. ) ;
#11597 = ORIENTED_EDGE ( 'NONE', *, *, #137614, .T. ) ;
#11598 = CARTESIAN_POINT ( 'NONE',  ( 124.8337635252314470, 6.110000000000001208, 1.122388791418549305E-15 ) ) ;
#11599 = VERTEX_POINT ( 'NONE', #22617 ) ;
#11600 = EDGE_CURVE ( 'NONE', #34867, #5353, #67628, .T. ) ;
#11601 = FACE_OUTER_BOUND ( 'NONE', #45914, .T. ) ;
#11602 = CARTESIAN_POINT ( 'NONE',  ( 18.63425672184678916, 4.584330080086930965E-16, 0.000000000000000000 ) ) ;
#11603 = ADVANCED_FACE ( 'NONE', ( #112521 ), #133574, .F. ) ;
#11604 = CARTESIAN_POINT ( 'NONE',  ( 26.43999999999999773, -2.055000000000000160, 0.000000000000000000 ) ) ;
#11605 = AXIS2_PLACEMENT_3D ( 'NONE', #20813, #132489, #121552 ) ;
#11606 = CARTESIAN_POINT ( 'NONE',  ( 118.3287635252314658, 0.000000000000000000, -6.109999999999998543 ) ) ;
#11607 = EDGE_LOOP ( 'NONE', ( #45508, #79874, #94444, #78458 ) ) ;
#11609 = ORIENTED_EDGE ( 'NONE', *, *, #32765, .F. ) ;
#11608 = AXIS2_PLACEMENT_3D ( 'NONE', #58249, #124878, #101690 ) ;
#11610 = LINE ( 'NONE', #34131, #131847 ) ;
#11611 = VECTOR ( 'NONE', #55070, 1000.000000000000000 ) ;
#11612 = VECTOR ( 'NONE', #43499, 999.9999999999998863 ) ;
#11613 = VECTOR ( 'NONE', #675, 1000.000000000000000 ) ;
#11614 = DIRECTION ( 'NONE',  ( -0.7071067811865486830, -0.7071067811865464625, 0.000000000000000000 ) ) ;
#11615 = VECTOR ( 'NONE', #36843, 1000.000000000000227 ) ;
#11616 = VERTEX_POINT ( 'NONE', #34255 ) ;
#11617 = ORIENTED_EDGE ( 'NONE', *, *, #40425, .T. ) ;
#11618 = CARTESIAN_POINT ( 'NONE',  ( 37.62543019189811133, 5.291415217122919401, 3.055000000000002824 ) ) ;
#11619 = ORIENTED_EDGE ( 'NONE', *, *, #119887, .F. ) ;
#11620 = FACE_OUTER_BOUND ( 'NONE', #6820, .T. ) ;
#11621 = CARTESIAN_POINT ( 'NONE',  ( -34.45011844616455221, -8.997695858405947433, 5.000000000000000888 ) ) ;
#11622 = LINE ( 'NONE', #120376, #36882 ) ;
#11623 = VECTOR ( 'NONE', #84220, 999.9999999999998863 ) ;
#11624 =( BOUNDED_CURVE ( )  B_SPLINE_CURVE ( 2, ( #65493, #128572, #75630, #8184, #73490, #117654, #63357, #41547, #51020, #18340, #40852, #97334, #130001 ),
 .UNSPECIFIED., .F., .F. ) 
 B_SPLINE_CURVE_WITH_KNOTS ( ( 3, 2, 2, 2, 2, 2, 3 ),
 ( 0.4166666666666667962, 0.4194444444444445641, 0.4222222222222223320, 0.4250000000000000999, 0.4277777777777778678, 0.4305555555555556912, 0.4333333333333334592 ),
 .UNSPECIFIED. ) 
 CURVE ( )  GEOMETRIC_REPRESENTATION_ITEM ( )  RATIONAL_B_SPLINE_CURVE ( ( 0.9999999999999986677, 0.9659258262890696445, 1.000000000000000000, 0.9659258262890683122, 1.000000000000000000, 0.9659258262890683122, 1.000000000000000000, 0.9659258262890683122, 1.000000000000000000, 0.9659258262890683122, 1.000000000000000000, 0.9659258262890669799, 1.000000000000001332 ) ) 
 REPRESENTATION_ITEM ( '' )  );
#11625 = EDGE_CURVE ( 'NONE', #67882, #25495, #24094, .T. ) ;
#11626 = CARTESIAN_POINT ( 'NONE',  ( 33.74543019189811588, -5.291415217122918513, -3.055000000000000160 ) ) ;
#11627 = EDGE_LOOP ( 'NONE', ( #4065, #121174, #94175, #121391 ) ) ;
#11628 = CARTESIAN_POINT ( 'NONE',  ( -24.18398860626899705, 28.73617430169804265, 5.000000000000000000 ) ) ;
#11629 = EDGE_LOOP ( 'NONE', ( #119563, #90667, #121590, #1960 ) ) ;
#11630 = ORIENTED_EDGE ( 'NONE', *, *, #140323, .F. ) ;
#11631 = VECTOR ( 'NONE', #115887, 1000.000000000000227 ) ;
#11632 = ORIENTED_EDGE ( 'NONE', *, *, #90330, .T. ) ;
#11633 = AXIS2_PLACEMENT_3D ( 'NONE', #17675, #95255, #37326 ) ;
#11635 = CARTESIAN_POINT ( 'NONE',  ( -29.99999999999979039, -18.41253812416056235, 4.000000000000000000 ) ) ;
#11634 = VECTOR ( 'NONE', #134203, 1000.000000000000000 ) ;
#11636 = CARTESIAN_POINT ( 'NONE',  ( 29.29289321881325137, 11.25929247661560773, 5.000000000000000000 ) ) ;
#11637 = ORIENTED_EDGE ( 'NONE', *, *, #128832, .T. ) ;
#11638 = PLANE ( 'NONE',  #71476 ) ;
#11639 = AXIS2_PLACEMENT_3D ( 'NONE', #136583, #46049, #101828 ) ;
#11640 = CARTESIAN_POINT ( 'NONE',  ( 32.20710678118632586, 12.75929247661558641, 5.000000000000000000 ) ) ;
#11641 = CARTESIAN_POINT ( 'NONE',  ( -5.999999999999970690, 20.58746187583905041, 4.000000000000000000 ) ) ;
#11642 = VECTOR ( 'NONE', #98254, 1000.000000000000000 ) ;
#11643 = LINE ( 'NONE', #87806, #18904 ) ;
#11644 = FACE_BOUND ( 'NONE', #78172, .T. ) ;
#11645 = ORIENTED_EDGE ( 'NONE', *, *, #2203, .T. ) ;
#11646 = DIRECTION ( 'NONE',  ( -1.000000000000000000, -0.000000000000000000, -0.000000000000000000 ) ) ;
#11647 = PRESENTATION_LAYER_ASSIGNMENT (  '', '', ( #55688 ) ) ;
#11648 = CARTESIAN_POINT ( 'NONE',  ( 34.49999999999975131, -16.91253812416058366, 4.000000000000000000 ) ) ;
#11649 = CARTESIAN_POINT ( 'NONE',  ( 48.48921356237309510, -27.52281430457089328, 5.000000000000000000 ) ) ;
#11650 = ORIENTED_EDGE ( 'NONE', *, *, #42681, .T. ) ;
#11651 = PLANE ( 'NONE',  #48110 ) ;
#11652 = EDGE_LOOP ( 'NONE', ( #140346, #104251, #70753, #43258 ) ) ;
#11653 = ORIENTED_EDGE ( 'NONE', *, *, #88314, .T. ) ;
#11654 = ORIENTED_EDGE ( 'NONE', *, *, #26515, .F. ) ;
#11655 = CARTESIAN_POINT ( 'NONE',  ( 43.80793019189810877, -6.109999999999998543, 1.637169565754158507 ) ) ;
#11656 = ORIENTED_EDGE ( 'NONE', *, *, #118139, .T. ) ;
#11657 = VECTOR ( 'NONE', #137312, 1000.000000000000114 ) ;
#11658 = DIRECTION ( 'NONE',  ( 1.000000000000000000, 0.000000000000000000, 0.000000000000000000 ) ) ;
#11659 = CARTESIAN_POINT ( 'NONE',  ( 42.29974487139158157, -27.71228299555235708, 4.000000000000000000 ) ) ;
#11660 = DIRECTION ( 'NONE',  ( -0.7071067811865486830, 0.7071067811865464625, 0.000000000000000000 ) ) ;
#11661 = ORIENTED_EDGE ( 'NONE', *, *, #14904, .F. ) ;
#11662 = LINE ( 'NONE', #800, #100076 ) ;
#11664 = FACE_OUTER_BOUND ( 'NONE', #125779, .T. ) ;
#11663 = VECTOR ( 'NONE', #45710, 1000.000000000000227 ) ;
#11665 = CARTESIAN_POINT ( 'NONE',  ( 30.18398860626900060, 28.73617430169808173, 5.000000000000000000 ) ) ;
#11666 = DIRECTION ( 'NONE',  ( 0.3543493200069162685, -0.000000000000000000, -0.9351131265310288487 ) ) ;
#11667 = CARTESIAN_POINT ( 'NONE',  ( 8.423184310185783730, 0.000000000000000000, 2.500000000000000444 ) ) ;
#11668 = CARTESIAN_POINT ( 'NONE',  ( 19.49999999999987210, -8.947814304570730570, 5.000000000000000000 ) ) ;
#11669 = FILL_AREA_STYLE ('',( #110992 ) ) ;
#11670 = VERTEX_POINT ( 'NONE', #34989 ) ;
#11671 = EDGE_CURVE ( 'NONE', #53073, #90399, #90794, .T. ) ;
#11672 = ORIENTED_EDGE ( 'NONE', *, *, #40867, .F. ) ;
#11673 = AXIS2_PLACEMENT_3D ( 'NONE', #15956, #71123, #137802 ) ;
#11674 = VERTEX_POINT ( 'NONE', #78477 ) ;
#11675 = CARTESIAN_POINT ( 'NONE',  ( 9.489213562373095101, -27.52281430457062328, 5.000000000000000000 ) ) ;
#11676 = CARTESIAN_POINT ( 'NONE',  ( -38.95341186370431785, 14.25929247661557042, 18.84478104361336648 ) ) ;
#11677 = ORIENTED_EDGE ( 'NONE', *, *, #79285, .F. ) ;
#11678 = ORIENTED_EDGE ( 'NONE', *, *, #70497, .F. ) ;
#11679 = FACE_OUTER_BOUND ( 'NONE', #36786, .T. ) ;
#11680 = LINE ( 'NONE', #9548, #36340 ) ;
#11681 = ADVANCED_FACE ( 'NONE', ( #103082 ), #25496, .F. ) ;
#11682 = EDGE_CURVE ( 'NONE', #86567, #3709, #68350, .T. ) ;
#11683 = DIRECTION ( 'NONE',  ( 0.7071067811865487940, 0.7071067811865463515, 0.000000000000000000 ) ) ;
#11684 = ORIENTED_EDGE ( 'NONE', *, *, #19721, .T. ) ;
#11685 = LINE ( 'NONE', #99418, #4606 ) ;
#11686 = VECTOR ( 'NONE', #31194, 1000.000000000000114 ) ;
#11688 = EDGE_CURVE ( 'NONE', #48357, #73550, #132880, .T. ) ;
#11687 = CARTESIAN_POINT ( 'NONE',  ( -7.122370700763609008, -39.92999999999999261, 19.06900128115122328 ) ) ;
#11689 = EDGE_CURVE ( 'NONE', #19565, #14349, #2062, .T. ) ;
#11690 = CARTESIAN_POINT ( 'NONE',  ( 24.85873647476855908, 5.808823158059031044, -5.808823158059038150 ) ) ;
#11691 = CARTESIAN_POINT ( 'NONE',  ( 2.139447441471317379, -9.629649721936179265E-32, 2.500000000000000444 ) ) ;
#11692 = ADVANCED_FACE ( 'NONE', ( #80626 ), #124826, .F. ) ;
#11693 = ORIENTED_EDGE ( 'NONE', *, *, #84416, .T. ) ;
#11694 = CARTESIAN_POINT ( 'NONE',  ( 106.9537635252314516, -6.109999999999999432, -3.741295971395163529E-16 ) ) ;
#11695 = EDGE_CURVE ( 'NONE', #37816, #29497, #95032, .T. ) ;
#11696 = LINE ( 'NONE', #66836, #44275 ) ;
#11697 = CARTESIAN_POINT ( 'NONE',  ( 4.371765549556129393, -8.240707523384200428, 11.38925528200751458 ) ) ;
#11699 = VERTEX_POINT ( 'NONE', #5151 ) ;
#11698 = PLANE ( 'NONE',  #67793 ) ;
#11700 = DIRECTION ( 'NONE',  ( 0.7071067811865487940, 0.7071067811865463515, 0.000000000000000000 ) ) ;
#11701 = ORIENTED_EDGE ( 'NONE', *, *, #134051, .F. ) ;
#11702 = ADVANCED_FACE ( 'NONE', ( #48008 ), #26238, .T. ) ;
#11703 = DIRECTION ( 'NONE',  ( 0.7071067811865487940, 0.7071067811865463515, 0.000000000000000000 ) ) ;
#11704 = CARTESIAN_POINT ( 'NONE',  ( -34.92500000000001137, -8.143876922607470092, 4.000000000000000000 ) ) ;
#11705 = DIRECTION ( 'NONE',  ( -0.7071067811865486830, -0.7071067811865464625, -0.000000000000000000 ) ) ;
#11706 = ORIENTED_EDGE ( 'NONE', *, *, #135782, .T. ) ;
#11707 = AXIS2_PLACEMENT_3D ( 'NONE', #14368, #4129, #61482 ) ;
#11708 = DIRECTION ( 'NONE',  ( 0.7071067811865486830, -0.7071067811865464625, -0.000000000000000000 ) ) ;
#11709 = EDGE_CURVE ( 'NONE', #14462, #143141, #71907, .T. ) ;
#11710 = AXIS2_PLACEMENT_3D ( 'NONE', #13953, #100982, #133631 ) ;
#11711 = DIRECTION ( 'NONE',  ( -1.000000000000000000, -4.708078457166071843E-14, 0.000000000000000000 ) ) ;
#11712 = PLANE ( 'NONE',  #90793 ) ;
#11713 = ORIENTED_EDGE ( 'NONE', *, *, #15487, .F. ) ;
#11714 = AXIS2_PLACEMENT_3D ( 'NONE', #56000, #89311, #66850 ) ;
#11715 = CIRCLE ( 'NONE', #78936, 2.552699999999990865 ) ;
#11716 = AXIS2_PLACEMENT_3D ( 'NONE', #3510, #15107, #14422 ) ;
#11717 = VECTOR ( 'NONE', #10895, 1000.000000000000227 ) ;
#11718 = DIRECTION ( 'NONE',  ( 0.000000000000000000, -1.000000000000000000, 0.000000000000000000 ) ) ;
#11720 = ORIENTED_EDGE ( 'NONE', *, *, #68771, .F. ) ;
#11719 = VECTOR ( 'NONE', #13466, 1000.000000000000227 ) ;
#11721 = ADVANCED_FACE ( 'NONE', ( #116080 ), #15316, .F. ) ;
#11722 = FACE_OUTER_BOUND ( 'NONE', #52523, .T. ) ;
#11724 = ORIENTED_EDGE ( 'NONE', *, *, #23886, .T. ) ;
#11723 = DIRECTION ( 'NONE',  ( 0.3543493200069163240, 0.000000000000000000, 0.9351131265310288487 ) ) ;
#11725 = ORIENTED_EDGE ( 'NONE', *, *, #56208, .F. ) ;
#11726 = CARTESIAN_POINT ( 'NONE',  ( -30.29974487139158867, -27.71228299555227537, 4.000000000000000000 ) ) ;
#11727 = VECTOR ( 'NONE', #98299, 1000.000000000000000 ) ;
#11728 = LINE ( 'NONE', #3014, #126936 ) ;
#11729 = EDGE_CURVE ( 'NONE', #64057, #106060, #70503, .T. ) ;
#11730 = ORIENTED_EDGE ( 'NONE', *, *, #118281, .T. ) ;
#11731 = LINE ( 'NONE', #56015, #48323 ) ;
#11732 = CARTESIAN_POINT ( 'NONE',  ( -28.49999999999979750, 10.94296225409023826, -9.576120664313320319 ) ) ;
#11733 = CARTESIAN_POINT ( 'NONE',  ( 18.48921356237309510, -27.52281430457068367, 5.000000000000000000 ) ) ;
#11734 = ORIENTED_EDGE ( 'NONE', *, *, #61538, .F. ) ;
#11735 = AXIS2_PLACEMENT_3D ( 'NONE', #33, #45762, #25383 ) ;
#11736 = DIRECTION ( 'NONE',  ( -0.6830127018922180770, -0.6830127018922204085, -0.2588190451025213501 ) ) ;
#11737 = LINE ( 'NONE', #55289, #67615 ) ;
#11739 = ADVANCED_FACE ( 'NONE', ( #59598 ), #104492, .T. ) ;
#11738 = CARTESIAN_POINT ( 'NONE',  ( -2.999999999999975131, 15.45873954670185135, -0.03131636524293310297 ) ) ;
#11740 = LINE ( 'NONE', #109652, #80760 ) ;
#11741 = CARTESIAN_POINT ( 'NONE',  ( 129.2875270504628986, 0.000000000000000000, -7.949999999999998401 ) ) ;
#11742 = CARTESIAN_POINT ( 'NONE',  ( 4.998069433178977228, -22.22500000000000142, 4.500000000000000888 ) ) ;
#11743 = AXIS2_PLACEMENT_3D ( 'NONE', #122372, #25943, #103471 ) ;
#11744 = ORIENTED_EDGE ( 'NONE', *, *, #54990, .F. ) ;
#11745 = EDGE_LOOP ( 'NONE', ( #142019, #9102, #29773, #311 ) ) ;
#11746 = ADVANCED_FACE ( 'NONE', ( #126260 ), #39263, .F. ) ;
#11747 = AXIS2_PLACEMENT_3D ( 'NONE', #143050, #141639, #96647 ) ;
#11748 = ORIENTED_EDGE ( 'NONE', *, *, #88926, .T. ) ;
#11749 = EDGE_CURVE ( 'NONE', #137381, #76116, #137141, .T. ) ;
#11750 = VECTOR ( 'NONE', #123448, 1000.000000000000000 ) ;
#11751 = VERTEX_POINT ( 'NONE', #115331 ) ;
#11752 = DIRECTION ( 'NONE',  ( 0.7071067811865487940, 0.7071067811865463515, -0.000000000000000000 ) ) ;
#11753 = LINE ( 'NONE', #12483, #78735 ) ;
#11754 = VECTOR ( 'NONE', #20314, 1000.000000000000000 ) ;
#11755 = ORIENTED_EDGE ( 'NONE', *, *, #133037, .T. ) ;
#11756 = EDGE_CURVE ( 'NONE', #74522, #42386, #137866, .T. ) ;
#11757 = DIRECTION ( 'NONE',  ( -0.000000000000000000, 0.000000000000000000, 1.000000000000000000 ) ) ;
#11759 = EDGE_CURVE ( 'NONE', #135854, #84525, #84214, .T. ) ;
#11758 = PLANE ( 'NONE',  #14222 ) ;
#11760 = FACE_OUTER_BOUND ( 'NONE', #101406, .T. ) ;
#11761 = DIRECTION ( 'NONE',  ( -0.7071067811865486830, -0.7071067811865464625, 0.000000000000000000 ) ) ;
#11762 = CARTESIAN_POINT ( 'NONE',  ( 126.1462635252314328, -4.472830434245840259, 4.472830434245839371 ) ) ;
#11763 = VECTOR ( 'NONE', #14064, 1000.000000000000000 ) ;
#11764 = EDGE_LOOP ( 'NONE', ( #43205, #138969, #133033, #24722 ) ) ;
#11765 = CARTESIAN_POINT ( 'NONE',  ( 1.666965064704732269, -1.287028696899377367E-11, -6.428034935295263708 ) ) ;
#11766 = DIRECTION ( 'NONE',  ( 0.000000000000000000, 0.000000000000000000, -1.000000000000000000 ) ) ;
#11767 = DIRECTION ( 'NONE',  ( 0.7071067811865487940, 0.7071067811865463515, 0.000000000000000000 ) ) ;
#11768 = CARTESIAN_POINT ( 'NONE',  ( 0.3485740145173168991, 5.832717272428934230, -5.114375124908068670 ) ) ;
#11769 = CARTESIAN_POINT ( 'NONE',  ( 7.499999999999960032, 1.087461875839230707, 4.000000000000000000 ) ) ;
#11770 = DIRECTION ( 'NONE',  ( -0.7071067811865486830, -0.7071067811865464625, 0.000000000000000000 ) ) ;
#11771 = CARTESIAN_POINT ( 'NONE',  ( -34.92500000000001137, -22.22500000000000142, 4.000000000000000000 ) ) ;
#11772 = CARTESIAN_POINT ( 'NONE',  ( 47.32919371712955581, -3.975000000000001865, 6.884901960086284411 ) ) ;
#11773 = CARTESIAN_POINT ( 'NONE',  ( -34.92500000000001137, 16.51246187583933533, 4.000000000000000000 ) ) ;
#11774 = PLANE ( 'NONE',  #55468 ) ;
#11775 = AXIS2_PLACEMENT_3D ( 'NONE', #85051, #19081, #130730 ) ;
#11776 = VERTEX_POINT ( 'NONE', #73322 ) ;
#11777 = ORIENTED_EDGE ( 'NONE', *, *, #34197, .T. ) ;
#11778 = CARTESIAN_POINT ( 'NONE',  ( 46.50000000000000000, 0.000000000000000000, -7.950000000000000178 ) ) ;
#11779 = EDGE_CURVE ( 'NONE', #142313, #3243, #61056, .T. ) ;
#11780 = DIRECTION ( 'NONE',  ( 1.000000000000000000, 0.000000000000000000, 0.000000000000000000 ) ) ;
#11781 = AXIS2_PLACEMENT_3D ( 'NONE', #22285, #10696, #122321 ) ;
#11782 = CARTESIAN_POINT ( 'NONE',  ( -30.18398860626900060, 28.73617430169808173, 5.000000000000000000 ) ) ;
#11783 = EDGE_LOOP ( 'NONE', ( #142176, #89925, #96218, #918, #58583 ) ) ;
#11784 = VECTOR ( 'NONE', #47292, 1000.000000000000000 ) ;
#11785 = CARTESIAN_POINT ( 'NONE',  ( -1.320800000000306618, -4.493284886149243553E-13, 3.775643966265820328 ) ) ;
#11786 = DIRECTION ( 'NONE',  ( 0.7071067811865486830, -0.7071067811865464625, -0.000000000000000000 ) ) ;
#11787 = CARTESIAN_POINT ( 'NONE',  ( 37.47959685856476852, 6.109999999999999432, 1.637169565754164280 ) ) ;
#11788 = EDGE_CURVE ( 'NONE', #100098, #116562, #9430, .T. ) ;
#11789 = EDGE_LOOP ( 'NONE', ( #41158, #73228, #56972, #89183 ) ) ;
#11790 = FACE_OUTER_BOUND ( 'NONE', #97705, .T. ) ;
#11791 = VERTEX_POINT ( 'NONE', #31942 ) ;
#11792 = ORIENTED_EDGE ( 'NONE', *, *, #79705, .T. ) ;
#11793 = PLANE ( 'NONE',  #56223 ) ;
#11794 = CARTESIAN_POINT ( 'NONE',  ( -34.92500000000001137, -22.22500000000000142, 4.000000000000000000 ) ) ;
#11795 = CARTESIAN_POINT ( 'NONE',  ( 19.05000000000000071, 3.174999999999997158, 4.000000000000000000 ) ) ;
#11796 = DIRECTION ( 'NONE',  ( -0.7071067811865486830, -0.7071067811865463515, 0.000000000000000000 ) ) ;
#11797 = EDGE_LOOP ( 'NONE', ( #127209, #90395, #56898, #39550 ) ) ;
#11798 = ADVANCED_FACE ( 'NONE', ( #64567 ), #7304, .F. ) ;
#11799 = DIRECTION ( 'NONE',  ( -0.3543493200069163240, -0.000000000000000000, 0.9351131265310288487 ) ) ;
#11800 = ORIENTED_EDGE ( 'NONE', *, *, #69575, .F. ) ;
#11801 = CARTESIAN_POINT ( 'NONE',  ( 86.18793019189810423, 6.110000000000002984, -1.637169565754156730 ) ) ;
#11802 = DIRECTION ( 'NONE',  ( -0.7071067811865487940, 0.7071067811865463515, -0.000000000000000000 ) ) ;
#11803 = DIRECTION ( 'NONE',  ( 0.6830127018922181881, 0.6830127018922202975, -0.2588190451025214056 ) ) ;
#11804 = DIRECTION ( 'NONE',  ( 1.000000000000000000, 0.000000000000000000, 0.000000000000000000 ) ) ;
#11805 = LINE ( 'NONE', #121999, #76445 ) ;
#11806 = VECTOR ( 'NONE', #129108, 1000.000000000000227 ) ;
#11807 = VERTEX_POINT ( 'NONE', #63179 ) ;
#11808 = CARTESIAN_POINT ( 'NONE',  ( -51.48921356237309510, -27.52281430457091460, 5.000000000000000000 ) ) ;
#11809 = CARTESIAN_POINT ( 'NONE',  ( 60.72459685856477307, -1.637169565754160949, 6.109999999999997655 ) ) ;
#11810 = LINE ( 'NONE', #24147, #53337 ) ;
#11811 = CARTESIAN_POINT ( 'NONE',  ( 0.000000000000000000, 0.000000000000000000, 5.000000000000000000 ) ) ;
#11812 = FACE_OUTER_BOUND ( 'NONE', #135836, .T. ) ;
#11813 = ORIENTED_EDGE ( 'NONE', *, *, #112682, .T. ) ;
#11814 = FACE_OUTER_BOUND ( 'NONE', #52365, .T. ) ;
#11815 = VECTOR ( 'NONE', #64515, 1000.000000000000000 ) ;
#11816 = ORIENTED_EDGE ( 'NONE', *, *, #43594, .T. ) ;
#11817 = ADVANCED_FACE ( 'NONE', ( #84891 ), #135907, .T. ) ;
#11818 = AXIS2_PLACEMENT_3D ( 'NONE', #25056, #35977, #124389 ) ;
#11819 = VECTOR ( 'NONE', #115041, 1000.000000000000000 ) ;
#11820 = EDGE_CURVE ( 'NONE', #40982, #28348, #52951, .T. ) ;
#11821 = CARTESIAN_POINT ( 'NONE',  ( 33.51679449616821671, 22.27000000000000668, -13.80793696990846620 ) ) ;
#11822 = EDGE_LOOP ( 'NONE', ( #61125, #2281, #119925, #96590 ) ) ;
#11823 = LINE ( 'NONE', #34318, #74673 ) ;
#11824 = DIRECTION ( 'NONE',  ( 0.7071067811865487940, -0.7071067811865463515, 0.000000000000000000 ) ) ;
#11825 = VECTOR ( 'NONE', #109459, 1000.000000000000000 ) ;
#11826 = VECTOR ( 'NONE', #41737, 1000.000000000000000 ) ;
#11827 = VECTOR ( 'NONE', #140660, 1000.000000000000000 ) ;
#11828 = VECTOR ( 'NONE', #8562, 1000.000000000000000 ) ;
#11829 = AXIS2_PLACEMENT_3D ( 'NONE', #134413, #24910, #93031 ) ;
#11830 = CARTESIAN_POINT ( 'NONE',  ( -47.99451991528749062, 28.92564299267971251, 4.000000000000000000 ) ) ;
#11831 = FACE_BOUND ( 'NONE', #36851, .T. ) ;
#11832 = EDGE_CURVE ( 'NONE', #71992, #39593, #43530, .T. ) ;
#11833 = LINE ( 'NONE', #13970, #22480 ) ;
#11834 = FACE_OUTER_BOUND ( 'NONE', #58370, .T. ) ;
#11835 = FACE_OUTER_BOUND ( 'NONE', #106827, .T. ) ;
#11837 = ORIENTED_EDGE ( 'NONE', *, *, #16759, .F. ) ;
#11836 = DIRECTION ( 'NONE',  ( 1.000000000000000000, 0.000000000000000000, 0.000000000000000000 ) ) ;
#11838 = CARTESIAN_POINT ( 'NONE',  ( -32.99451991528749062, 28.92564299267960948, 4.000000000000000000 ) ) ;
#11839 = VERTEX_POINT ( 'NONE', #41376 ) ;
#11840 = ORIENTED_EDGE ( 'NONE', *, *, #19624, .T. ) ;
#11841 = CARTESIAN_POINT ( 'NONE',  ( 73.99543019189810877, 5.291415217122916737, 3.055000000000001936 ) ) ;
#11842 = ORIENTED_EDGE ( 'NONE', *, *, #82349, .T. ) ;
#11843 = DIRECTION ( 'NONE',  ( -1.000000000000000000, 0.000000000000000000, 0.000000000000000000 ) ) ;
#11844 = AXIS2_PLACEMENT_3D ( 'NONE', #133135, #44723, #108632 ) ;
#11845 = DIRECTION ( 'NONE',  ( -0.000000000000000000, -0.3543493200069152693, 0.9351131265310292928 ) ) ;
#11846 = ORIENTED_EDGE ( 'NONE', *, *, #27965, .T. ) ;
#11847 = DIRECTION ( 'NONE',  ( 0.000000000000000000, -1.000000000000000000, 0.000000000000000000 ) ) ;
#11848 = VECTOR ( 'NONE', #955, 999.9999999999998863 ) ;
#11849 = CARTESIAN_POINT ( 'NONE',  ( 19.51058707530271974, 22.22500000000000142, 25.62767885193487771 ) ) ;
#11850 = DIRECTION ( 'NONE',  ( -0.7071067811865487940, 0.7071067811865463515, 0.000000000000000000 ) ) ;
#11851 = VECTOR ( 'NONE', #70881, 1000.000000000000227 ) ;
#11852 = CARTESIAN_POINT ( 'NONE',  ( -24.64327148205084583, 5.259292476615665457, 4.831541298974430632 ) ) ;
#11853 = PLANE ( 'NONE',  #133851 ) ;
#11854 = FACE_OUTER_BOUND ( 'NONE', #114008, .T. ) ;
#11855 = AXIS2_PLACEMENT_3D ( 'NONE', #87493, #53428, #119373 ) ;
#11856 = DIRECTION ( 'NONE',  ( -0.3543493200069162685, -0.000000000000000000, -0.9351131265310288487 ) ) ;
#11857 = DIRECTION ( 'NONE',  ( 0.7071067811865487940, 0.7071067811865463515, 0.000000000000000000 ) ) ;
#11858 = VERTEX_POINT ( 'NONE', #97152 ) ;
#11859 = VERTEX_POINT ( 'NONE', #42839 ) ;
#11860 =( GEOMETRIC_REPRESENTATION_CONTEXT ( 3 ) GLOBAL_UNCERTAINTY_ASSIGNED_CONTEXT ( ( #111437 ) ) GLOBAL_UNIT_ASSIGNED_CONTEXT ( ( #91839, #68693, #48348 ) ) REPRESENTATION_CONTEXT ( 'NONE', 'WORKASPACE' ) );
#11861 = DIRECTION ( 'NONE',  ( 0.7071067811865487940, 0.7071067811865463515, 0.000000000000000000 ) ) ;
#11862 = DIRECTION ( 'NONE',  ( -0.6830127018922181881, 0.6830127018922202975, -0.2588190451025214056 ) ) ;
#11863 = ORIENTED_EDGE ( 'NONE', *, *, #74609, .T. ) ;
#11864 = ORIENTED_EDGE ( 'NONE', *, *, #96256, .F. ) ;
#11865 = EDGE_LOOP ( 'NONE', ( #62040, #24294, #115358, #63078 ) ) ;
#11866 = AXIS2_PLACEMENT_3D ( 'NONE', #44249, #24607, #47147 ) ;
#11867 = ADVANCED_FACE ( 'NONE', ( #76167 ), #131984, .F. ) ;
#11868 = CARTESIAN_POINT ( 'NONE',  ( 27.41709685856476142, 3.054999999999998828, 5.291415217122922066 ) ) ;
#11869 = VERTEX_POINT ( 'NONE', #108747 ) ;
#11870 = CARTESIAN_POINT ( 'NONE',  ( 13.82816939922344091, -5.240707523384225297, 4.000000000000000000 ) ) ;
#11871 = DIRECTION ( 'NONE',  ( -0.7071067811865487940, 0.7071067811865463515, 0.000000000000000000 ) ) ;
#11872 = EDGE_CURVE ( 'NONE', #83353, #16402, #20324, .T. ) ;
#11873 = STYLED_ITEM ( 'NONE', ( #91727 ), #41693 ) ;
#11874 = CARTESIAN_POINT ( 'NONE',  ( 29.79580628287044419, -5.278424836066144543, 3.047499999999995879 ) ) ;
#11875 = CARTESIAN_POINT ( 'NONE',  ( 14.45122993026753377, 4.938655920609167360, -31.93222277579656776 ) ) ;
#11876 = EDGE_CURVE ( 'NONE', #42560, #60723, #141413, .T. ) ;
#11877 = EDGE_LOOP ( 'NONE', ( #139918, #132953, #90025, #117985 ) ) ;
#11878 = LINE ( 'NONE', #43822, #36446 ) ;
#11879 = EDGE_CURVE ( 'NONE', #129514, #46484, #118940, .T. ) ;
#11880 = CARTESIAN_POINT ( 'NONE',  ( -20.99999999999985079, -13.44781430457069149, 5.000000000000000000 ) ) ;
#11881 = VECTOR ( 'NONE', #63900, 1000.000000000000000 ) ;
#11882 = CARTESIAN_POINT ( 'NONE',  ( -2.510786437626908008, -27.52281430457053446, 5.000000000000000000 ) ) ;
#11884 = ORIENTED_EDGE ( 'NONE', *, *, #25740, .F. ) ;
#11883 = LINE ( 'NONE', #1697, #5421 ) ;
#11885 = VECTOR ( 'NONE', #6017, 1000.000000000000000 ) ;
#11886 = EDGE_LOOP ( 'NONE', ( #79045, #95484, #55603, #46154 ) ) ;
#11887 = ADVANCED_FACE ( 'NONE', ( #32670 ), #86338, .F. ) ;
#11888 = DIRECTION ( 'NONE',  ( 0.000000000000000000, -9.130123557772670799E-17, 1.000000000000000000 ) ) ;
#11889 = DIRECTION ( 'NONE',  ( -0.000000000000000000, -0.3543493200069152693, 0.9351131265310292928 ) ) ;
#11890 = DIRECTION ( 'NONE',  ( -0.000000000000000000, 0.000000000000000000, 1.000000000000000000 ) ) ;
#11891 = EDGE_LOOP ( 'NONE', ( #117432, #27505, #93429, #4531 ) ) ;
#11892 = PLANE ( 'NONE',  #131231 ) ;
#11893 = ORIENTED_EDGE ( 'NONE', *, *, #91461, .T. ) ;
#11894 = ADVANCED_FACE ( 'NONE', ( #75458 ), #54439, .T. ) ;
#11895 = VECTOR ( 'NONE', #109339, 1000.000000000000000 ) ;
#11896 = CARTESIAN_POINT ( 'NONE',  ( 5.994519915287488843, 28.92564299267942118, 4.000000000000000000 ) ) ;
#11897 = FACE_OUTER_BOUND ( 'NONE', #28070, .T. ) ;
#11898 = CIRCLE ( 'NONE', #60598, 1.898649999999994842 ) ;
#11899 = DIRECTION ( 'NONE',  ( 0.000000000000000000, 0.000000000000000000, 1.000000000000000000 ) ) ;
#11900 = DIRECTION ( 'NONE',  ( -1.000000000000000000, -1.224606353822377258E-16, -0.000000000000000000 ) ) ;
#11901 =( BOUNDED_CURVE ( )  B_SPLINE_CURVE ( 2, ( #67805, #54068, #143175, #11931, #64918, #56217, #10502, #53302, #98257, #329, #109834, #132338, #66352 ),
 .UNSPECIFIED., .F., .F. ) 
 B_SPLINE_CURVE_WITH_KNOTS ( ( 3, 2, 2, 2, 2, 2, 3 ),
 ( 0.4000000000000000777, 0.4027777777777778456, 0.4055555555555556135, 0.4083333333333334370, 0.4111111111111112049, 0.4138888888888889728, 0.4166666666666667962 ),
 .UNSPECIFIED. ) 
 CURVE ( )  GEOMETRIC_REPRESENTATION_ITEM ( )  RATIONAL_B_SPLINE_CURVE ( ( 0.9999999999999993339, 0.9659258262890689783, 1.000000000000000000, 0.9659258262890683122, 1.000000000000000000, 0.9659258262890683122, 1.000000000000000000, 0.9659258262890683122, 1.000000000000000000, 0.9659258262890683122, 1.000000000000000000, 0.9659258262890669799, 1.000000000000001332 ) ) 
 REPRESENTATION_ITEM ( '' )  );
#11902 = CARTESIAN_POINT ( 'NONE',  ( -30.18398860626900060, 28.73617430169808173, 5.000000000000000000 ) ) ;
#11903 = EDGE_CURVE ( 'NONE', #135734, #106183, #76908, .T. ) ;
#11904 = LINE ( 'NONE', #14046, #35518 ) ;
#11905 = CARTESIAN_POINT ( 'NONE',  ( 152.4000000000000057, 0.000000000000000000, -33.92499999999998295 ) ) ;
#11906 = ADVANCED_FACE ( 'NONE', ( #29777 ), #53715, .T. ) ;
#11907 = ORIENTED_EDGE ( 'NONE', *, *, #112687, .F. ) ;
#11908 = DIRECTION ( 'NONE',  ( -0.7071067811865486830, -0.7071067811865464625, 0.000000000000000000 ) ) ;
#11909 = ORIENTED_EDGE ( 'NONE', *, *, #97449, .F. ) ;
#11910 = AXIS2_PLACEMENT_3D ( 'NONE', #23570, #2500, #370 ) ;
#11911 = DIRECTION ( 'NONE',  ( 0.6830127018922181881, 0.6830127018922202975, -0.2588190451025214056 ) ) ;
#11912 = DIRECTION ( 'NONE',  ( 0.7071067811865486830, -0.7071067811865464625, -0.000000000000000000 ) ) ;
#11913 = EDGE_CURVE ( 'NONE', #84298, #15918, #98613, .T. ) ;
#11914 = CYLINDRICAL_SURFACE ( 'NONE', #93662, 0.5000000000000004441 ) ;
#11915 = PLANE ( 'NONE',  #57561 ) ;
#11916 = VERTEX_POINT ( 'NONE', #52259 ) ;
#11917 = CARTESIAN_POINT ( 'NONE',  ( 23.52487387214939574, 14.25929247661557042, 9.797011795316691973 ) ) ;
#11918 = LINE ( 'NONE', #133035, #120583 ) ;
#11919 = DIRECTION ( 'NONE',  ( 0.7071067811865487940, -0.7071067811865463515, 0.000000000000000000 ) ) ;
#11920 = VERTEX_POINT ( 'NONE', #107352 ) ;
#11921 = CARTESIAN_POINT ( 'NONE',  ( -4.499999999999968914, 16.08746187583908949, 4.000000000000000000 ) ) ;
#11922 = CARTESIAN_POINT ( 'NONE',  ( -48.48921356237309510, -27.52281430457089328, 5.000000000000000000 ) ) ;
#11923 = AXIS2_PLACEMENT_3D ( 'NONE', #81675, #6179, #138899 ) ;
#11924 = CARTESIAN_POINT ( 'NONE',  ( 23.99999999999983302, -5.527737879153171718, -7.983877177622427546 ) ) ;
#11925 = CARTESIAN_POINT ( 'NONE',  ( 55.32876352523144448, 0.000000000000000000, -6.109999999999999432 ) ) ;
#11926 = CARTESIAN_POINT ( 'NONE',  ( 6.489213562373093325, -27.52281430457059841, 5.000000000000000000 ) ) ;
#11927 = VECTOR ( 'NONE', #103173, 999.9999999999998863 ) ;
#11928 = AXIS2_PLACEMENT_3D ( 'NONE', #125802, #138821, #116336 ) ;
#11929 = CARTESIAN_POINT ( 'NONE',  ( 2.999999999999999112, 1.194621026894847171, -17.40906030209848510 ) ) ;
#11930 = FILL_AREA_STYLE_COLOUR ( '', #74211 ) ;
#11931 = CARTESIAN_POINT ( 'NONE',  ( 84.56250000000000000, -5.819803920172573086, -5.819803920172573974 ) ) ;
#11932 = ORIENTED_EDGE ( 'NONE', *, *, #9508, .T. ) ;
#11933 = EDGE_CURVE ( 'NONE', #6993, #136433, #96441, .T. ) ;
#11934 = EDGE_LOOP ( 'NONE', ( #104819, #125726, #19535, #74727 ) ) ;
#11935 = VECTOR ( 'NONE', #100567, 1000.000000000000000 ) ;
#11936 = PRESENTATION_LAYER_ASSIGNMENT (  '', '', ( #21155 ) ) ;
#11937 = VECTOR ( 'NONE', #24597, 1000.000000000000000 ) ;
#11938 = DIRECTION ( 'NONE',  ( -1.000000000000000000, -0.000000000000000000, -0.000000000000000000 ) ) ;
#11939 = VECTOR ( 'NONE', #14322, 1000.000000000000000 ) ;
#11940 = TOROIDAL_SURFACE ( 'NONE', #92986, 4.000000000000000000, 1.000000000000000000 ) ;
#11941 = CARTESIAN_POINT ( 'NONE',  ( -38.99451991528749062, 28.92564299267965211, 4.000000000000000000 ) ) ;
#11942 = CARTESIAN_POINT ( 'NONE',  ( -5.510786437626906675, -27.52281430457051314, 5.000000000000000000 ) ) ;
#11943 = DIRECTION ( 'NONE',  ( 1.000000000000000000, 0.000000000000000000, 0.000000000000000000 ) ) ;
#11944 = CARTESIAN_POINT ( 'NONE',  ( 10.52840764549667618, -2.499999999999998224, 0.000000000000000000 ) ) ;
#11945 = CARTESIAN_POINT ( 'NONE',  ( 34.92499999999998295, -21.72500000000000142, 5.000000000000000000 ) ) ;
#11946 = ORIENTED_EDGE ( 'NONE', *, *, #118742, .T. ) ;
#11947 = ORIENTED_EDGE ( 'NONE', *, *, #72348, .T. ) ;
#11948 = DIRECTION ( 'NONE',  ( 0.7071067811865487940, -0.7071067811865463515, 0.000000000000000000 ) ) ;
#11949 = DIRECTION ( 'NONE',  ( -0.6830127018922181881, 0.6830127018922202975, -0.2588190451025214056 ) ) ;
#11950 = AXIS2_PLACEMENT_3D ( 'NONE', #52293, #41419, #52996 ) ;
#11951 = LINE ( 'NONE', #1063, #35805 ) ;
#11952 = EDGE_CURVE ( 'NONE', #20334, #24733, #100768, .T. ) ;
#11953 = CARTESIAN_POINT ( 'NONE',  ( 20.99999999999985079, -15.41253812416059787, 4.000000000000000000 ) ) ;
#11954 = CARTESIAN_POINT ( 'NONE',  ( 72.12086038379622721, -6.884901960086286188, 3.974999999999997424 ) ) ;
#11955 = LINE ( 'NONE', #33752, #90294 ) ;
#11956 = FACE_OUTER_BOUND ( 'NONE', #10769, .T. ) ;
#11957 = ORIENTED_EDGE ( 'NONE', *, *, #86200, .T. ) ;
#11958 = CARTESIAN_POINT ( 'NONE',  ( 75.81250000000000000, 5.819803920172571310, 5.819803920172575751 ) ) ;
#11959 = DIRECTION ( 'NONE',  ( -0.7071067811865487940, 0.7071067811865463515, -0.000000000000000000 ) ) ;
#11960 = EDGE_CURVE ( 'NONE', #44265, #109300, #134858, .T. ) ;
#11961 = PLANE ( 'NONE',  #87966 ) ;
#11962 = CARTESIAN_POINT ( 'NONE',  ( 5.292893218813427225, -0.7407075233842735917, 5.000000000000000000 ) ) ;
#11963 = ORIENTED_EDGE ( 'NONE', *, *, #14981, .F. ) ;
#11964 = AXIS2_PLACEMENT_3D ( 'NONE', #81970, #4293, #101530 ) ;
#11965 = CARTESIAN_POINT ( 'NONE',  ( 39.48921356237310221, -27.52281430457082934, 5.000000000000000000 ) ) ;
#11966 = ORIENTED_EDGE ( 'NONE', *, *, #107722, .T. ) ;
#11967 = VECTOR ( 'NONE', #110420, 1000.000000000000227 ) ;
#11968 = ADVANCED_BREP_SHAPE_REPRESENTATION ( '', ( #142469, #127880 ), #35272 ) ;
#11969 = EDGE_CURVE ( 'NONE', #95196, #78216, #110193, .T. ) ;
#11970 = DIRECTION ( 'NONE',  ( -0.7071067811865486830, 0.7071067811865464625, 0.000000000000000000 ) ) ;
#11971 = CARTESIAN_POINT ( 'NONE',  ( 66.35459685856476142, -1.637169565754161615, 6.110000000000000320 ) ) ;
#11972 = AXIS2_PLACEMENT_3D ( 'NONE', #110290, #10966, #55233 ) ;
#11973 = ORIENTED_EDGE ( 'NONE', *, *, #4533, .T. ) ;
#11974 = VECTOR ( 'NONE', #18535, 1000.000000000000000 ) ;
#11975 = CARTESIAN_POINT ( 'NONE',  ( 17.53719725875415847, 4.202752102959690472E-16, 0.000000000000000000 ) ) ;
#11976 = CARTESIAN_POINT ( 'NONE',  ( -34.75611968250420603, -0.1870657452926316466, 4.955485411084897152 ) ) ;
#11977 = DIRECTION ( 'NONE',  ( -0.000000000000000000, 0.3543493200069153248, 0.9351131265310292928 ) ) ;
#11978 = ADVANCED_FACE ( 'NONE', ( #22461 ), #45705, .F. ) ;
#11979 = LINE ( 'NONE', #67851, #120296 ) ;
#11980 = ORIENTED_EDGE ( 'NONE', *, *, #125128, .F. ) ;
#11981 = DIRECTION ( 'NONE',  ( -0.000000000000000000, 0.3543493200069153248, 0.9351131265310292928 ) ) ;
#11982 = CARTESIAN_POINT ( 'NONE',  ( 16.96247294953710849, -7.464222240803106570E-16, -6.094999999999989981 ) ) ;
#11983 = CARTESIAN_POINT ( 'NONE',  ( 0.000000000000000000, -4.870000000000014317, -10.00000000000000178 ) ) ;
#11984 = VECTOR ( 'NONE', #37933, 999.9999999999998863 ) ;
#11985 = PLANE ( 'NONE',  #22894 ) ;
#11986 = EDGE_LOOP ( 'NONE', ( #75286, #91244, #23647 ) ) ;
#11987 = ORIENTED_EDGE ( 'NONE', *, *, #120889, .T. ) ;
#11988 = CARTESIAN_POINT ( 'NONE',  ( 68.25043019189810423, 3.055000000000002824, -5.291415217122919401 ) ) ;
#11989 = VERTEX_POINT ( 'NONE', #100064 ) ;
#11990 = DIRECTION ( 'NONE',  ( 0.6830127018922181881, 0.6830127018922202975, -0.2588190451025214056 ) ) ;
#11991 = CARTESIAN_POINT ( 'NONE',  ( 27.79333936457828358, 21.75929247661549226, 4.998822639870708073 ) ) ;
#11992 = VECTOR ( 'NONE', #95617, 1000.000000000000227 ) ;
#11993 = CYLINDRICAL_SURFACE ( 'NONE', #29466, 2.500000000000000000 ) ;
#11994 = CARTESIAN_POINT ( 'NONE',  ( -12.48921356237309155, -27.52281430457064104, 5.000000000000000000 ) ) ;
#11995 = ORIENTED_EDGE ( 'NONE', *, *, #102741, .T. ) ;
#11996 = ORIENTED_EDGE ( 'NONE', *, *, #19289, .F. ) ;
#11997 = VECTOR ( 'NONE', #86320, 1000.000000000000000 ) ;
#11998 = LINE ( 'NONE', #112753, #116317 ) ;
#11999 = EDGE_CURVE ( 'NONE', #103339, #84629, #22460, .T. ) ;
#12000 = ORIENTED_EDGE ( 'NONE', *, *, #76231, .F. ) ;
#12001 = EDGE_CURVE ( 'NONE', #62749, #93258, #66715, .T. ) ;
#12002 = DIRECTION ( 'NONE',  ( -0.7071067811865487940, 0.7071067811865463515, 0.000000000000000000 ) ) ;
#12003 = CARTESIAN_POINT ( 'NONE',  ( 3.005480084712505828, 28.92564299267936079, 4.000000000000000000 ) ) ;
#12004 = FACE_OUTER_BOUND ( 'NONE', #87774, .T. ) ;
#12005 = VECTOR ( 'NONE', #6701, 1000.000000000000000 ) ;
#12006 = ORIENTED_EDGE ( 'NONE', *, *, #37144, .F. ) ;
#12007 = FACE_BOUND ( 'NONE', #105330, .T. ) ;
#12008 = EDGE_CURVE ( 'NONE', #103350, #21017, #91344, .T. ) ;
#12009 = LINE ( 'NONE', #411, #91833 ) ;
#12010 = DIRECTION ( 'NONE',  ( 0.6830127018922180770, -0.6830127018922204085, -0.2588190451025213501 ) ) ;
#12011 = PLANE ( 'NONE',  #6527 ) ;
#12012 = AXIS2_PLACEMENT_3D ( 'NONE', #2853, #103585, #48512 ) ;
#12013 = PLANE ( 'NONE',  #31837 ) ;
#12014 = PRODUCT_DEFINITION ( 'UNKNOWN', '', #132846, #61802 ) ;
#12015 = DIRECTION ( 'NONE',  ( -0.7071067811865486830, -0.7071067811865464625, -0.000000000000000000 ) ) ;
#12016 = DIRECTION ( 'NONE',  ( -0.4153784070974642084, -0.7373070763208201539, -0.5327654776019346006 ) ) ;
#12017 = ORIENTED_EDGE ( 'NONE', *, *, #71649, .T. ) ;
#12018 = ORIENTED_EDGE ( 'NONE', *, *, #64508, .F. ) ;
#12019 = CARTESIAN_POINT ( 'NONE',  ( 101.7037635252314374, 6.109999999999998543, 1.122388791418548911E-15 ) ) ;
#12020 = ORIENTED_EDGE ( 'NONE', *, *, #24534, .T. ) ;
#12021 = DIRECTION ( 'NONE',  ( 2.496005001405478586E-15, 1.000000000000000000, -0.000000000000000000 ) ) ;
#12022 = VERTEX_POINT ( 'NONE', #35553 ) ;
#12023 = FACE_OUTER_BOUND ( 'NONE', #83363, .T. ) ;
#12024 = AXIS2_PLACEMENT_3D ( 'NONE', #40831, #117634, #51000 ) ;
#12025 = CIRCLE ( 'NONE', #49120, 2.055000000000000604 ) ;
#12026 = AXIS2_PLACEMENT_3D ( 'NONE', #13060, #57334, #80503 ) ;
#12027 = EDGE_CURVE ( 'NONE', #57842, #52361, #78310, .T. ) ;
#12028 = CARTESIAN_POINT ( 'NONE',  ( -12.70000000000000995, 12.19802518668052471, 4.711086268963014412 ) ) ;
#12029 = VECTOR ( 'NONE', #77008, 1000.000000000000000 ) ;
#12030 = AXIS2_PLACEMENT_3D ( 'NONE', #105282, #50922, #14713 ) ;
#12031 = PLANE ( 'NONE',  #54048 ) ;
#12032 = EDGE_LOOP ( 'NONE', ( #140684, #102826, #36079, #103101 ) ) ;
#12033 = DIRECTION ( 'NONE',  ( 0.000000000000000000, -1.000000000000000000, 0.000000000000000000 ) ) ;
#12034 = CARTESIAN_POINT ( 'NONE',  ( 27.29974487139158512, -27.71228299555225405, 4.000000000000000000 ) ) ;
#12035 = DIRECTION ( 'NONE',  ( 0.000000000000000000, -1.000000000000000000, 0.000000000000000000 ) ) ;
#12036 = PLANE ( 'NONE',  #59680 ) ;
#12037 = LINE ( 'NONE', #68598, #49701 ) ;
#12038 = FACE_OUTER_BOUND ( 'NONE', #99960, .T. ) ;
#12039 = AXIS2_PLACEMENT_3D ( 'NONE', #99690, #75132, #32321 ) ;
#12040 = AXIS2_PLACEMENT_3D ( 'NONE', #54086, #85228, #139664 ) ;
#12041 =( GEOMETRIC_REPRESENTATION_CONTEXT ( 3 ) GLOBAL_UNCERTAINTY_ASSIGNED_CONTEXT ( ( #57787 ) ) GLOBAL_UNIT_ASSIGNED_CONTEXT ( ( #133637, #66245, #48573 ) ) REPRESENTATION_CONTEXT ( 'NONE', 'WORKASPACE' ) );
#12042 = FACE_OUTER_BOUND ( 'NONE', #120090, .T. ) ;
#12043 = ORIENTED_EDGE ( 'NONE', *, *, #110056, .T. ) ;
#12044 = CARTESIAN_POINT ( 'NONE',  ( 0.7071067811865450192, -3.740707523384246613, 5.000000000000000000 ) ) ;
#12045 = DIRECTION ( 'NONE',  ( -0.6830127018922181881, 0.6830127018922202975, -0.2588190451025214056 ) ) ;
#12046 = ORIENTED_EDGE ( 'NONE', *, *, #42551, .F. ) ;
#12047 = ORIENTED_EDGE ( 'NONE', *, *, #100318, .T. ) ;
#12048 = ORIENTED_EDGE ( 'NONE', *, *, #62326, .F. ) ;
#12049 = CARTESIAN_POINT ( 'NONE',  ( 54.97959685856476852, 6.109999999999999432, 1.637169565754164280 ) ) ;
#12050 = EDGE_LOOP ( 'NONE', ( #16997, #95294, #9301, #128433 ) ) ;
#12051 = DIRECTION ( 'NONE',  ( 0.7071067811865486830, -0.7071067811865464625, -0.000000000000000000 ) ) ;
#12052 = ADVANCED_FACE ( 'NONE', ( #55859 ), #82727, .T. ) ;
#12053 = CARTESIAN_POINT ( 'NONE',  ( 10.83747294953710671, 6.094999999999989981, -1.119633336120465690E-15 ) ) ;
#12054 = CARTESIAN_POINT ( 'NONE',  ( 87.20876352523143282, -7.482591942790329030E-16, 6.110000000000001208 ) ) ;
#12055 = FACE_OUTER_BOUND ( 'NONE', #113673, .T. ) ;
#12056 = EDGE_CURVE ( 'NONE', #7217, #51414, #68190, .T. ) ;
#12058 = EDGE_LOOP ( 'NONE', ( #15203, #61854, #91197, #21249 ) ) ;
#12057 = EDGE_CURVE ( 'NONE', #58140, #108385, #41013, .T. ) ;
#12059 = LINE ( 'NONE', #56347, #11719 ) ;
#12060 = PLANE ( 'NONE',  #107166 ) ;
#12061 = ORIENTED_EDGE ( 'NONE', *, *, #39190, .F. ) ;
#12062 = EDGE_CURVE ( 'NONE', #31236, #135328, #25331, .T. ) ;
#12063 = CARTESIAN_POINT ( 'NONE',  ( 24.70710678118637205, 20.25929247661550647, 5.000000000000000000 ) ) ;
#12064 = CONICAL_SURFACE ( 'NONE', #93112, 9.524999999999991473, 1.029744258676653645 ) ;
#12065 = LINE ( 'NONE', #1177, #103059 ) ;
#12066 = ORIENTED_EDGE ( 'NONE', *, *, #23611, .T. ) ;
#12067 = VECTOR ( 'NONE', #16657, 1000.000000000000114 ) ;
#12068 = CARTESIAN_POINT ( 'NONE',  ( 22.22674160717820513, -11.24070752338415780, 18.24660765846987331 ) ) ;
#12069 = ORIENTED_EDGE ( 'NONE', *, *, #20418, .F. ) ;
#12070 = VECTOR ( 'NONE', #131181, 1000.000000000000000 ) ;
#12071 = ORIENTED_EDGE ( 'NONE', *, *, #60422, .F. ) ;
#12072 = EDGE_LOOP ( 'NONE', ( #142374, #122576, #118254, #56799 ) ) ;
#12073 = FACE_OUTER_BOUND ( 'NONE', #15808, .T. ) ;
#12074 = DIRECTION ( 'NONE',  ( 1.000000000000000000, 0.000000000000000000, 0.000000000000000000 ) ) ;
#12075 = EDGE_CURVE ( 'NONE', #37853, #142351, #34102, .T. ) ;
#12076 = LINE ( 'NONE', #111389, #97182 ) ;
#12077 = EDGE_CURVE ( 'NONE', #132053, #42748, #68880, .T. ) ;
#12078 = DIRECTION ( 'NONE',  ( 0.7071067811865486830, -0.7071067811865464625, -0.000000000000000000 ) ) ;
#12079 = ORIENTED_EDGE ( 'NONE', *, *, #108955, .F. ) ;
#12080 = VECTOR ( 'NONE', #99390, 1000.000000000000000 ) ;
#12081 = CARTESIAN_POINT ( 'NONE',  ( -72.18398860626899705, 28.73617430169837661, 5.000000000000000000 ) ) ;
#12082 = EDGE_CURVE ( 'NONE', #15337, #28681, #14585, .T. ) ;
#12083 = CARTESIAN_POINT ( 'NONE',  ( 10.77040314143521904, -7.934999999999989839, 2.126176841940957907 ) ) ;
#12084 = LINE ( 'NONE', #1882, #16059 ) ;
#12085 = LINE ( 'NONE', #25827, #99271 ) ;
#12086 = DIRECTION ( 'NONE',  ( -0.3543493200069162685, -0.000000000000000000, -0.9351131265310288487 ) ) ;
#12087 = ORIENTED_EDGE ( 'NONE', *, *, #75077, .F. ) ;
#12088 = ORIENTED_EDGE ( 'NONE', *, *, #56137, .T. ) ;
#12089 = VECTOR ( 'NONE', #99728, 1000.000000000000000 ) ;
#12090 = ORIENTED_EDGE ( 'NONE', *, *, #32051, .T. ) ;
#12091 = FACE_OUTER_BOUND ( 'NONE', #107319, .T. ) ;
#12092 = DIRECTION ( 'NONE',  ( -0.6830127018922180770, -0.6830127018922204085, -0.2588190451025213501 ) ) ;
#12093 = EDGE_CURVE ( 'NONE', #108226, #130681, #90616, .T. ) ;
#12094 = AXIS2_PLACEMENT_3D ( 'NONE', #33225, #99862, #525 ) ;
#12095 = LINE ( 'NONE', #142630, #142282 ) ;
#12096 = CARTESIAN_POINT ( 'NONE',  ( 38.99451991528749062, 28.92564299267965211, 4.000000000000000000 ) ) ;
#12097 = DIRECTION ( 'NONE',  ( 1.000000000000000000, 0.000000000000000000, 0.000000000000000000 ) ) ;
#12098 = LINE ( 'NONE', #1209, #39124 ) ;
#12099 = DIRECTION ( 'NONE',  ( 0.000000000000000000, -0.000000000000000000, -1.000000000000000000 ) ) ;
#12100 = LINE ( 'NONE', #109991, #97278 ) ;
#12101 = FACE_OUTER_BOUND ( 'NONE', #51698, .T. ) ;
#12102 = VERTEX_POINT ( 'NONE', #13723 ) ;
#12103 = CARTESIAN_POINT ( 'NONE',  ( 0.000000000000000000, 0.000000000000000000, 5.000000000000000000 ) ) ;
#12104 = EDGE_CURVE ( 'NONE', #12281, #6181, #132722, .T. ) ;
#12105 = AXIS2_PLACEMENT_3D ( 'NONE', #138354, #14436, #102880 ) ;
#12106 = VERTEX_POINT ( 'NONE', #77612 ) ;
#12107 = CARTESIAN_POINT ( 'NONE',  ( 17.52071992270299106, -3.088060075592792497, -34.88610987998131208 ) ) ;
#12108 = ORIENTED_EDGE ( 'NONE', *, *, #88850, .F. ) ;
#12109 = DIRECTION ( 'NONE',  ( -0.7071067811865487940, -0.7071067811865463515, -0.000000000000000000 ) ) ;
#12111 = ORIENTED_EDGE ( 'NONE', *, *, #116484, .F. ) ;
#12110 = CARTESIAN_POINT ( 'NONE',  ( 18.71230993966015532, -21.73547319004781286, 4.999917730833664642 ) ) ;
#12112 = PLANE ( 'NONE',  #87996 ) ;
#12113 = FACE_OUTER_BOUND ( 'NONE', #21352, .T. ) ;
#12114 = ORIENTED_EDGE ( 'NONE', *, *, #53889, .T. ) ;
#12115 = LINE ( 'NONE', #87553, #78635 ) ;
#12117 = ORIENTED_EDGE ( 'NONE', *, *, #125536, .T. ) ;
#12116 = VECTOR ( 'NONE', #119641, 1000.000000000000000 ) ;
#12118 = LINE ( 'NONE', #56402, #130148 ) ;
#12119 = VERTEX_POINT ( 'NONE', #36237 ) ;
#12120 = DIRECTION ( 'NONE',  ( -0.000000000000000000, -1.000000000000000000, -0.000000000000000000 ) ) ;
#12121 = EDGE_CURVE ( 'NONE', #102027, #123748, #110893, .T. ) ;
#12122 = CARTESIAN_POINT ( 'NONE',  ( 112.9541937171295558, 6.884901960086283523, 3.975000000000002753 ) ) ;
#12123 = LINE ( 'NONE', #59255, #1896 ) ;
#12124 = ORIENTED_EDGE ( 'NONE', *, *, #141170, .T. ) ;
#12125 = CARTESIAN_POINT ( 'NONE',  ( -12.48921356237309155, -27.52281430457064104, 5.000000000000000000 ) ) ;
#12126 = FACE_OUTER_BOUND ( 'NONE', #40416, .T. ) ;
#12127 = DIRECTION ( 'NONE',  ( -0.000000000000000000, -0.3543493200069152693, 0.9351131265310292928 ) ) ;
#12128 = CARTESIAN_POINT ( 'NONE',  ( 13.12500000000000178, 6.094999999999989981, -1.119633336120465690E-15 ) ) ;
#12129 = CARTESIAN_POINT ( 'NONE',  ( 24.62456980810188867, -6.871911579029512218, 3.967499999999996252 ) ) ;
#12130 = VECTOR ( 'NONE', #49943, 1000.000000000000000 ) ;
#12131 = VECTOR ( 'NONE', #81117, 1000.000000000000000 ) ;
#12133 = LINE ( 'NONE', #131074, #134640 ) ;
#12132 = AXIS2_PLACEMENT_3D ( 'NONE', #92980, #69840, #3781 ) ;
#12134 = CARTESIAN_POINT ( 'NONE',  ( 25.49999999999982236, 0.4311230773921849169, 4.000000000000000000 ) ) ;
#12135 = ORIENTED_EDGE ( 'NONE', *, *, #127473, .T. ) ;
#12136 = ORIENTED_EDGE ( 'NONE', *, *, #12296, .F. ) ;
#12137 = VECTOR ( 'NONE', #14919, 1000.000000000000000 ) ;
#12138 =( GEOMETRIC_REPRESENTATION_CONTEXT ( 3 ) GLOBAL_UNCERTAINTY_ASSIGNED_CONTEXT ( ( #139282 ) ) GLOBAL_UNIT_ASSIGNED_CONTEXT ( ( #60207, #4299, #14543 ) ) REPRESENTATION_CONTEXT ( 'NONE', 'WORKASPACE' ) );
#12139 = DIRECTION ( 'NONE',  ( 0.000000000000000000, -1.000000000000000000, 0.000000000000000000 ) ) ;
#12140 = ORIENTED_EDGE ( 'NONE', *, *, #36199, .T. ) ;
#12141 = ADVANCED_FACE ( 'NONE', ( #15839 ), #39822, .T. ) ;
#12142 = CARTESIAN_POINT ( 'NONE',  ( 89.68793019189810423, 6.110000000000002984, -1.637169565754156730 ) ) ;
#12143 = CARTESIAN_POINT ( 'NONE',  ( -9.707106781186475075, -0.7407075233842735917, 5.000000000000000000 ) ) ;
#12144 = CARTESIAN_POINT ( 'NONE',  ( 26.99999999999981171, 1.552185695429152856, 5.000000000000000000 ) ) ;
#12145 = VECTOR ( 'NONE', #127731, 1000.000000000000000 ) ;
#12147 = VECTOR ( 'NONE', #122683, 1000.000000000000000 ) ;
#12146 = DIRECTION ( 'NONE',  ( 0.000000000000000000, -1.000000000000000000, 0.000000000000000000 ) ) ;
#12148 = PLANE ( 'NONE',  #140496 ) ;
#12149 = ORIENTED_EDGE ( 'NONE', *, *, #36653, .F. ) ;
#12150 = DIRECTION ( 'NONE',  ( 0.7071067811865486830, -0.7071067811865464625, -0.000000000000000000 ) ) ;
#12151 = FILL_AREA_STYLE ('',( #34634 ) ) ;
#12152 = FACE_OUTER_BOUND ( 'NONE', #39125, .T. ) ;
#12153 = CARTESIAN_POINT ( 'NONE',  ( 23.35681257248248954, -20.24070752338406365, 21.22881796311218139 ) ) ;
#12154 = EDGE_CURVE ( 'NONE', #99775, #57637, #92725, .T. ) ;
#12155 = LINE ( 'NONE', #99143, #128131 ) ;
#12157 = ORIENTED_EDGE ( 'NONE', *, *, #17062, .T. ) ;
#12156 = CARTESIAN_POINT ( 'NONE',  ( 21.48921356237309155, -27.52281430457070499, 5.000000000000000000 ) ) ;
#12158 = CARTESIAN_POINT ( 'NONE',  ( -33.48921356237309510, -27.52281430457078670, 5.000000000000000000 ) ) ;
#12159 = CARTESIAN_POINT ( 'NONE',  ( 102.6000270504628844, 5.819803920172570422, 5.819803920172575751 ) ) ;
#12160 = DIRECTION ( 'NONE',  ( -0.7071067811865487940, 0.7071067811865463515, 0.000000000000000000 ) ) ;
#12161 = CARTESIAN_POINT ( 'NONE',  ( -7.940000000000001279, -33.26999999999999602, -8.101350000000008933 ) ) ;
#12162 = CARTESIAN_POINT ( 'NONE',  ( 156.1500000000000057, -49.14999999999999147, -45.92499999999969162 ) ) ;
#12163 = VERTEX_POINT ( 'NONE', #128240 ) ;
#12164 = VERTEX_POINT ( 'NONE', #105726 ) ;
#12165 = VERTEX_POINT ( 'NONE', #136962 ) ;
#12166 = CARTESIAN_POINT ( 'NONE',  ( 88.22959685856474721, -6.110000000000000320, -1.637169565754161393 ) ) ;
#12167 = VECTOR ( 'NONE', #6018, 1000.000000000000000 ) ;
#12168 = VERTEX_POINT ( 'NONE', #104303 ) ;
#12169 = CARTESIAN_POINT ( 'NONE',  ( 4.495848767239241539, 2.500000000000000888, 0.000000000000000000 ) ) ;
#12170 = LINE ( 'NONE', #69440, #36354 ) ;
#12171 = LINE ( 'NONE', #111489, #22511 ) ;
#12172 = LINE ( 'NONE', #57158, #84826 ) ;
#12173 = VERTEX_POINT ( 'NONE', #5704 ) ;
#12174 = CARTESIAN_POINT ( 'NONE',  ( 184.0791405606631201, -51.15040958483977818, 36.98623100868706359 ) ) ;
#12175 = CARTESIAN_POINT ( 'NONE',  ( -38.99451991528749062, 28.92564299267965211, 4.000000000000000000 ) ) ;
#12176 = VECTOR ( 'NONE', #105462, 999.9999999999998863 ) ;
#12177 = DIRECTION ( 'NONE',  ( 0.7071067811865486830, -0.7071067811865464625, -0.000000000000000000 ) ) ;
#12178 = CARTESIAN_POINT ( 'NONE',  ( 86.24543019189812298, -5.291415217122918513, -3.055000000000000160 ) ) ;
#12179 = ORIENTED_EDGE ( 'NONE', *, *, #61205, .T. ) ;
#12180 = EDGE_CURVE ( 'NONE', #22506, #129819, #48065, .T. ) ;
#12181 = CIRCLE ( 'NONE', #90864, 1.000000000000000888 ) ;
#12182 = DIRECTION ( 'NONE',  ( -0.000000000000000000, -0.3543493200069152693, 0.9351131265310292928 ) ) ;
#12183 = CARTESIAN_POINT ( 'NONE',  ( -34.92500000000001137, 11.81665438641030441, 4.500000000000000888 ) ) ;
#12184 = ORIENTED_EDGE ( 'NONE', *, *, #137673, .F. ) ;
#12185 = EDGE_LOOP ( 'NONE', ( #73994, #101275, #41388, #111253 ) ) ;
#12186 = EDGE_CURVE ( 'NONE', #70620, #132165, #14471, .T. ) ;
#12187 = LINE ( 'NONE', #11448, #46977 ) ;
#12188 = EDGE_CURVE ( 'NONE', #136794, #2587, #69597, .T. ) ;
#12189 =( LENGTH_UNIT ( ) NAMED_UNIT ( * ) SI_UNIT ( .MILLI., .METRE. ) );
#12190 = CARTESIAN_POINT ( 'NONE',  ( 20.92123647476855197, -9.717572351234235426E-16, -7.934999999999990727 ) ) ;
#12191 = DIRECTION ( 'NONE',  ( 0.7071067811865486830, -0.7071067811865464625, -0.000000000000000000 ) ) ;
#12192 = CARTESIAN_POINT ( 'NONE',  ( 164.2063197296438943, 26.96999999999993847, 34.37654022073930804 ) ) ;
#12193 = LINE ( 'NONE', #35426, #108914 ) ;
#12194 = DIRECTION ( 'NONE',  ( -0.7071067811865486830, 0.7071067811865464625, 0.000000000000000000 ) ) ;
#12195 = EDGE_LOOP ( 'NONE', ( #108792, #21968, #101512, #140783 ) ) ;
#12197 = ORIENTED_EDGE ( 'NONE', *, *, #104535, .F. ) ;
#12196 = ADVANCED_FACE ( 'NONE', ( #71723, #49272, #113780 ), #94855, .F. ) ;
#12198 = DIRECTION ( 'NONE',  ( 0.000000000000000000, -1.000000000000000000, 0.000000000000000000 ) ) ;
#12199 = ORIENTED_EDGE ( 'NONE', *, *, #22503, .T. ) ;
#12200 = ORIENTED_EDGE ( 'NONE', *, *, #112289, .T. ) ;
#12201 = VECTOR ( 'NONE', #138935, 1000.000000000000000 ) ;
#12202 = EDGE_CURVE ( 'NONE', #48357, #89870, #94153, .T. ) ;
#12203 = CARTESIAN_POINT ( 'NONE',  ( -24.18398860626899705, 28.73617430169804265, 5.000000000000000000 ) ) ;
#12204 = ORIENTED_EDGE ( 'NONE', *, *, #33086, .T. ) ;
#12205 = CARTESIAN_POINT ( 'NONE',  ( -4.171830600776436526, -5.240707523384232402, 4.000000000000000000 ) ) ;
#12206 = DIRECTION ( 'NONE',  ( -0.6830127018922181881, 0.6830127018922202975, -0.2588190451025214056 ) ) ;
#12207 = LINE ( 'NONE', #76055, #55344 ) ;
#12208 = CARTESIAN_POINT ( 'NONE',  ( -26.99999999999981171, -10.44781430457072702, 5.000000000000000000 ) ) ;
#12209 = VERTEX_POINT ( 'NONE', #116632 ) ;
#12210 = PRESENTATION_STYLE_ASSIGNMENT (( #55751 ) ) ;
#12211 = VERTEX_POINT ( 'NONE', #81172 ) ;
#12212 = CARTESIAN_POINT ( 'NONE',  ( 8.188407645496676324, 9.139736423841732040E-16, 0.000000000000000000 ) ) ;
#12213 = VERTEX_POINT ( 'NONE', #136236 ) ;
#12214 = FILL_AREA_STYLE_COLOUR ( '', #72423 ) ;
#12215 = VERTEX_POINT ( 'NONE', #125381 ) ;
#12216 = DIRECTION ( 'NONE',  ( -0.7071067811865486830, -0.7071067811865464625, 0.000000000000000000 ) ) ;
#12217 = ORIENTED_EDGE ( 'NONE', *, *, #93750, .T. ) ;
#12218 = VERTEX_POINT ( 'NONE', #114478 ) ;
#12219 = VECTOR ( 'NONE', #81188, 1000.000000000000227 ) ;
#12220 = EDGE_LOOP ( 'NONE', ( #92663, #5804, #77285, #86962 ) ) ;
#12221 = FACE_OUTER_BOUND ( 'NONE', #33807, .T. ) ;
#12222 = EDGE_CURVE ( 'NONE', #49377, #114574, #126101, .T. ) ;
#12223 = DIRECTION ( 'NONE',  ( 0.7071067811865487940, 0.7071067811865463515, 0.000000000000000000 ) ) ;
#12224 = CARTESIAN_POINT ( 'NONE',  ( 22.37177410554622980, -1.784312229707115893, 4.000000000000000000 ) ) ;
#12225 = CARTESIAN_POINT ( 'NONE',  ( 119.4379301918980900, -6.110000000000001208, 1.637169565754158951 ) ) ;
#12226 = DIRECTION ( 'NONE',  ( -1.000000000000000000, -0.000000000000000000, -0.000000000000000000 ) ) ;
#12227 = EDGE_CURVE ( 'NONE', #77399, #32218, #54418, .T. ) ;
#12228 = CARTESIAN_POINT ( 'NONE',  ( -23.20710678118638626, -14.24070752338412937, 5.000000000000000000 ) ) ;
#12229 = DIRECTION ( 'NONE',  ( -0.000000000000000000, -0.3543493200069152693, 0.9351131265310292928 ) ) ;
#12230 = VECTOR ( 'NONE', #18307, 1000.000000000000000 ) ;
#12231 = CARTESIAN_POINT ( 'NONE',  ( 8.999999999999937828, -8.151047557385062703, -8.977947279169821826 ) ) ;
#12232 = ADVANCED_FACE ( 'NONE', ( #17315 ), #31074, .F. ) ;
#12234 = EDGE_CURVE ( 'NONE', #45041, #118319, #96975, .T. ) ;
#12233 = AXIS2_PLACEMENT_3D ( 'NONE', #28516, #53843, #8824 ) ;
#12235 = VECTOR ( 'NONE', #11856, 1000.000000000000227 ) ;
#12236 = DIRECTION ( 'NONE',  ( -0.000000000000000000, -0.000000000000000000, 1.000000000000000000 ) ) ;
#12237 = ORIENTED_EDGE ( 'NONE', *, *, #71081, .T. ) ;
#12238 = DIRECTION ( 'NONE',  ( -1.000000000000000000, -0.000000000000000000, -0.000000000000000000 ) ) ;
#12239 = DIRECTION ( 'NONE',  ( 1.000000000000000000, 0.000000000000000000, 0.000000000000000000 ) ) ;
#12240 = CARTESIAN_POINT ( 'NONE',  ( -10.49999999999991829, 0.4497235411627317769, -5.599840258123564674 ) ) ;
#12241 = ORIENTED_EDGE ( 'NONE', *, *, #70849, .T. ) ;
#12242 = ORIENTED_EDGE ( 'NONE', *, *, #131938, .T. ) ;
#12243 = ORIENTED_EDGE ( 'NONE', *, *, #54482, .F. ) ;
#12244 = VECTOR ( 'NONE', #70161, 999.9999999999998863 ) ;
#12245 = CARTESIAN_POINT ( 'NONE',  ( 60.18398860626900415, 28.73617430169829490, 5.000000000000000000 ) ) ;
#12246 = ORIENTED_EDGE ( 'NONE', *, *, #52715, .T. ) ;
#12247 = EDGE_LOOP ( 'NONE', ( #93015, #66710, #102469, #60919 ) ) ;
#12248 = LINE ( 'NONE', #100708, #60672 ) ;
#12249 = CARTESIAN_POINT ( 'NONE',  ( -42.18398860626899705, 28.73617430169816700, 5.000000000000000000 ) ) ;
#12250 = CARTESIAN_POINT ( 'NONE',  ( -34.92500000000001137, -7.285322628117655519, -6.182564397582745563 ) ) ;
#12251 = EDGE_CURVE ( 'NONE', #53667, #76579, #10008, .T. ) ;
#12252 = LINE ( 'NONE', #102856, #141183 ) ;
#12253 = ADVANCED_FACE ( 'NONE', ( #84721 ), #107866, .F. ) ;
#12254 = LINE ( 'NONE', #34036, #37099 ) ;
#12255 = ORIENTED_EDGE ( 'NONE', *, *, #87596, .F. ) ;
#12256 = CARTESIAN_POINT ( 'NONE',  ( -25.41009064519816718, 9.759292476615621936, 11.28811694763772877 ) ) ;
#12257 = EDGE_LOOP ( 'NONE', ( #87094, #140643, #107802, #111179 ) ) ;
#12258 = CARTESIAN_POINT ( 'NONE',  ( 14.11732500641695509, -0.1862019290248694003, 4.000000000000000000 ) ) ;
#12259 = AXIS2_PLACEMENT_3D ( 'NONE', #71892, #104476, #35707 ) ;
#12260 = CARTESIAN_POINT ( 'NONE',  ( 19.60873647476855197, -5.808823158059033709, 5.808823158059035485 ) ) ;
#12261 = ORIENTED_EDGE ( 'NONE', *, *, #6917, .F. ) ;
#12262 = CARTESIAN_POINT ( 'NONE',  ( 83.62043019189812298, 3.055000000000002380, -5.291415217122917625 ) ) ;
#12263 = EDGE_CURVE ( 'NONE', #139982, #58396, #119457, .T. ) ;
#12264 = LINE ( 'NONE', #68138, #22784 ) ;
#12265 = CARTESIAN_POINT ( 'NONE',  ( -34.42500000000001137, -6.022814304570508703, 5.000000000000000000 ) ) ;
#12266 = ORIENTED_EDGE ( 'NONE', *, *, #124001, .F. ) ;
#12267 = DIRECTION ( 'NONE',  ( 0.7071067811865487940, 0.7071067811865463515, 0.000000000000000000 ) ) ;
#12268 = ORIENTED_EDGE ( 'NONE', *, *, #112550, .T. ) ;
#12269 = ORIENTED_EDGE ( 'NONE', *, *, #90707, .T. ) ;
#12270 = CARTESIAN_POINT ( 'NONE',  ( 11.25346039003969523, 4.202752102959690472E-16, 0.000000000000000000 ) ) ;
#12271 = LINE ( 'NONE', #10823, #71791 ) ;
#12272 = ADVANCED_FACE ( 'NONE', ( #128932 ), #108564, .F. ) ;
#12273 = CARTESIAN_POINT ( 'NONE',  ( -32.99451991528749062, 28.92564299267960948, 4.000000000000000000 ) ) ;
#12274 = CARTESIAN_POINT ( 'NONE',  ( 2.816011393730999401, 28.73617430169785436, 5.000000000000000000 ) ) ;
#12275 = VERTEX_POINT ( 'NONE', #98448 ) ;
#12276 = AXIS2_PLACEMENT_3D ( 'NONE', #65052, #110641, #75222 ) ;
#12277 =( LENGTH_UNIT ( ) NAMED_UNIT ( * ) SI_UNIT ( .MILLI., .METRE. ) );
#12278 = VECTOR ( 'NONE', #101782, 1000.000000000000000 ) ;
#12279 = CARTESIAN_POINT ( 'NONE',  ( -24.18398860626899705, 28.73617430169804265, 5.000000000000000000 ) ) ;
#12280 = PLANE ( 'NONE',  #23709 ) ;
#12281 = VERTEX_POINT ( 'NONE', #87576 ) ;
#12282 = CARTESIAN_POINT ( 'NONE',  ( 8.488313940715631389, 6.759292476615645917, 16.35960578974467694 ) ) ;
#12283 = EDGE_CURVE ( 'NONE', #93111, #71989, #52594, .T. ) ;
#12284 = DIRECTION ( 'NONE',  ( 0.6830127018922180770, -0.6830127018922204085, -0.2588190451025213501 ) ) ;
#12285 = VERTEX_POINT ( 'NONE', #75292 ) ;
#12287 = ORIENTED_EDGE ( 'NONE', *, *, #13794, .F. ) ;
#12286 = LINE ( 'NONE', #75425, #23210 ) ;
#12288 = ORIENTED_EDGE ( 'NONE', *, *, #118638, .T. ) ;
#12289 = DIRECTION ( 'NONE',  ( -0.7071067811865487940, 0.7071067811865463515, 0.000000000000000000 ) ) ;
#12290 = DIRECTION ( 'NONE',  ( 0.000000000000000000, -1.000000000000000000, 0.000000000000000000 ) ) ;
#12291 = ORIENTED_EDGE ( 'NONE', *, *, #73548, .T. ) ;
#12292 = CARTESIAN_POINT ( 'NONE',  ( -34.92500000000001137, 8.816654386410331057, 4.500000000000000888 ) ) ;
#12293 = AXIS2_PLACEMENT_3D ( 'NONE', #107322, #108721, #118173 ) ;
#12294 = CARTESIAN_POINT ( 'NONE',  ( 0.000000000000000000, 8.966399257802175171, 5.000000000000000000 ) ) ;
#12295 = LINE ( 'NONE', #25307, #108734 ) ;
#12296 = EDGE_CURVE ( 'NONE', #8442, #89327, #63705, .T. ) ;
#12298 = AXIS2_PLACEMENT_3D ( 'NONE', #101791, #36539, #114100 ) ;
#12297 = DIRECTION ( 'NONE',  ( -0.7071067811865486830, -0.7071067811865464625, 0.000000000000000000 ) ) ;
#12299 = LINE ( 'NONE', #134838, #80726 ) ;
#12300 = CARTESIAN_POINT ( 'NONE',  ( 41.35681257248237586, -20.24070752338406720, 21.22881796311222047 ) ) ;
#12301 = DIRECTION ( 'NONE',  ( -0.7071067811865486830, 0.7071067811865464625, 0.000000000000000000 ) ) ;
#12302 = LINE ( 'NONE', #68177, #79597 ) ;
#12303 = LINE ( 'NONE', #100754, #25134 ) ;
#12304 = CARTESIAN_POINT ( 'NONE',  ( 22.43706980810188867, 2.126176841940952134, -7.934999999999993392 ) ) ;
#12305 = CARTESIAN_POINT ( 'NONE',  ( -34.28351269101152354, -22.22500000000000142, 5.243083521430598637 ) ) ;
#12306 = AXIS2_PLACEMENT_3D ( 'NONE', #94867, #16604, #3568 ) ;
#12307 = LINE ( 'NONE', #136227, #41266 ) ;
#12308 = CARTESIAN_POINT ( 'NONE',  ( 110.0833333333333428, 6.884901960086290629, -3.974999999999994316 ) ) ;
#12309 = CARTESIAN_POINT ( 'NONE',  ( -34.49999999999975131, -7.912538124160673370, 4.000000000000000000 ) ) ;
#12310 = ORIENTED_EDGE ( 'NONE', *, *, #105507, .T. ) ;
#12311 =( BOUNDED_CURVE ( )  B_SPLINE_CURVE ( 3, ( #106286, #6961, #43231, #85270 ),
 .UNSPECIFIED., .F., .F. ) 
 B_SPLINE_CURVE_WITH_KNOTS ( ( 4, 4 ),
 ( 1.142100667999822905, 1.182775789206201633 ),
 .UNSPECIFIED. ) 
 CURVE ( )  GEOMETRIC_REPRESENTATION_ITEM ( )  RATIONAL_B_SPLINE_CURVE ( ( 1.000000000000000000, 0.9998621326283523292, 0.9998621326283523292, 1.000000000000000000 ) ) 
 REPRESENTATION_ITEM ( '' )  );
#12312 = ORIENTED_EDGE ( 'NONE', *, *, #79764, .T. ) ;
#12313 = CARTESIAN_POINT ( 'NONE',  ( 99.72916666666665719, 7.950000000000001954, -2.130196079827421762 ) ) ;
#12314 = ORIENTED_EDGE ( 'NONE', *, *, #32548, .T. ) ;
#12315 = ORIENTED_EDGE ( 'NONE', *, *, #106180, .T. ) ;
#12316 = ORIENTED_EDGE ( 'NONE', *, *, #36552, .T. ) ;
#12317 = DIRECTION ( 'NONE',  ( 0.000000000000000000, -1.000000000000000000, 0.000000000000000000 ) ) ;
#12318 = DIRECTION ( 'NONE',  ( -1.000000000000000000, -0.000000000000000000, -0.000000000000000000 ) ) ;
#12319 = AXIS2_PLACEMENT_3D ( 'NONE', #115570, #83742, #104736 ) ;
#12320 = CARTESIAN_POINT ( 'NONE',  ( 12.27820156798389561, 8.651982939446476450, -3.925326872160782798 ) ) ;
#12321 = ORIENTED_EDGE ( 'NONE', *, *, #139992, .F. ) ;
#12322 = DIRECTION ( 'NONE',  ( -1.000000000000000000, -0.000000000000000000, -0.000000000000000000 ) ) ;
#12323 = CARTESIAN_POINT ( 'NONE',  ( 32.99999999999977973, -16.44781430457066662, 5.000000000000000000 ) ) ;
#12324 = DIRECTION ( 'NONE',  ( -0.7071067811865486830, 0.7071067811865464625, 0.000000000000000000 ) ) ;
#12325 = DIRECTION ( 'NONE',  ( -0.7071067811865486830, -0.7071067811865464625, 0.000000000000000000 ) ) ;
#12326 = ORIENTED_EDGE ( 'NONE', *, *, #34263, .F. ) ;
#12327 = CARTESIAN_POINT ( 'NONE',  ( 20.24139925780189841, 21.72500000000000853, 5.000000000000000000 ) ) ;
#12328 = CARTESIAN_POINT ( 'NONE',  ( 12.79289321881337038, -17.24070752338410273, 5.000000000000000000 ) ) ;
#12330 = VECTOR ( 'NONE', #80146, 1000.000000000000227 ) ;
#12329 = DIRECTION ( 'NONE',  ( -0.000000000000000000, 0.000000000000000000, 1.000000000000000000 ) ) ;
#12331 = CARTESIAN_POINT ( 'NONE',  ( -57.48921356237308800, -27.52281430457095368, 5.000000000000000000 ) ) ;
#12332 = CARTESIAN_POINT ( 'NONE',  ( 23.33333333333333570, 5.278424836066143655, -3.047499999999997655 ) ) ;
#12333 = CARTESIAN_POINT ( 'NONE',  ( 35.99451991528749772, 28.92564299267963079, 4.000000000000000000 ) ) ;
#12334 = LINE ( 'NONE', #34115, #100789 ) ;
#12335 = DIRECTION ( 'NONE',  ( -1.000000000000000000, -1.224606353822377258E-16, -0.000000000000000000 ) ) ;
#12336 = ORIENTED_EDGE ( 'NONE', *, *, #53115, .T. ) ;
#12337 = ORIENTED_EDGE ( 'NONE', *, *, #11363, .F. ) ;
#12338 = CARTESIAN_POINT ( 'NONE',  ( 115.9379301918980900, -6.110000000000001208, 1.637169565754158951 ) ) ;
#12339 = VERTEX_POINT ( 'NONE', #43366 ) ;
#12340 = EDGE_CURVE ( 'NONE', #26730, #83228, #9021, .T. ) ;
#12341 = LINE ( 'NONE', #110918, #8458 ) ;
#12342 = VECTOR ( 'NONE', #21748, 1000.000000000000000 ) ;
#12343 = DIRECTION ( 'NONE',  ( -0.7071067811865486830, -0.7071067811865464625, 0.000000000000000000 ) ) ;
#12344 = CARTESIAN_POINT ( 'NONE',  ( -16.49999999999988631, -14.56887692260766087, 4.000000000000000000 ) ) ;
#12346 = VECTOR ( 'NONE', #65235, 1000.000000000000000 ) ;
#12345 = DIRECTION ( 'NONE',  ( 0.7071067811865486830, -0.7071067811865464625, -0.000000000000000000 ) ) ;
#12347 = CARTESIAN_POINT ( 'NONE',  ( 114.3912635252314232, -4.472830434245839371, -4.472830434245839371 ) ) ;
#12348 = VERTEX_POINT ( 'NONE', #73843 ) ;
#12349 = EDGE_CURVE ( 'NONE', #136794, #39797, #118765, .T. ) ;
#12350 = EDGE_LOOP ( 'NONE', ( #84445, #48626, #98553, #110758 ) ) ;
#12351 = VECTOR ( 'NONE', #140132, 1000.000000000000227 ) ;
#12352 = PRODUCT_DEFINITION_FORMATION_WITH_SPECIFIED_SOURCE ( 'ANY', '', #110337, .NOT_KNOWN. ) ;
#12353 = FACE_OUTER_BOUND ( 'NONE', #59935, .T. ) ;
#12354 = ORIENTED_EDGE ( 'NONE', *, *, #83819, .F. ) ;
#12355 = EDGE_LOOP ( 'NONE', ( #90303, #142154, #35733, #18536 ) ) ;
#12356 = CARTESIAN_POINT ( 'NONE',  ( 38.50043019189809712, -3.055000000000002380, 5.291415217122920289 ) ) ;
#12357 = EDGE_CURVE ( 'NONE', #13638, #93212, #18721, .T. ) ;
#12358 = VERTEX_POINT ( 'NONE', #109325 ) ;
#12359 = LINE ( 'NONE', #134160, #107035 ) ;
#12360 = EDGE_CURVE ( 'NONE', #115620, #143546, #41203, .T. ) ;
#12361 = CARTESIAN_POINT ( 'NONE',  ( 1.525403141435219379, 2.126176841940962348, 7.934999999999988951 ) ) ;
#12362 = PRESENTATION_LAYER_ASSIGNMENT (  '', '', ( #116575 ) ) ;
#12363 = EDGE_CURVE ( 'NONE', #43296, #28403, #107173, .T. ) ;
#12364 = VECTOR ( 'NONE', #110876, 1000.000000000000000 ) ;
#12365 = CARTESIAN_POINT ( 'NONE',  ( 30.53709685856477307, -3.054999999999998828, -5.291415217122919401 ) ) ;
#12366 = ORIENTED_EDGE ( 'NONE', *, *, #97459, .T. ) ;
#12367 = EDGE_CURVE ( 'NONE', #143444, #11445, #52090, .T. ) ;
#12368 = PLANE ( 'NONE',  #20133 ) ;
#12369 = ORIENTED_EDGE ( 'NONE', *, *, #95993, .T. ) ;
#12370 = VERTEX_POINT ( 'NONE', #12143 ) ;
#12371 = VERTEX_POINT ( 'NONE', #89028 ) ;
#12372 = CONICAL_SURFACE ( 'NONE', #68011, 2.500000000000000444, 0.9599310885968830309 ) ;
#12373 = EDGE_CURVE ( 'NONE', #110737, #117346, #133246, .T. ) ;
#12374 = CARTESIAN_POINT ( 'NONE',  ( 0.000000000000000000, 9.735942053221458872E-16, -7.950000000000000178 ) ) ;
#12375 = EDGE_LOOP ( 'NONE', ( #31128, #32761, #14358, #98270 ) ) ;
#12376 = CIRCLE ( 'NONE', #142077, 5.968999999999998529 ) ;
#12377 = DIRECTION ( 'NONE',  ( -0.000000000000000000, -0.3543493200069152693, 0.9351131265310292928 ) ) ;
#12378 = LINE ( 'NONE', #53780, #98849 ) ;
#12379 = EDGE_CURVE ( 'NONE', #123460, #26065, #76729, .T. ) ;
#12380 = CARTESIAN_POINT ( 'NONE',  ( 29.99999999999979039, 8.587461875839165870, 4.000000000000000000 ) ) ;
#12381 = CIRCLE ( 'NONE', #123477, 2.500000000000000444 ) ;
#12382 = FACE_BOUND ( 'NONE', #55008, .T. ) ;
#12383 = EDGE_LOOP ( 'NONE', ( #99512, #139166, #85799 ) ) ;
#12384 = CARTESIAN_POINT ( 'NONE',  ( -9.328169399223463998, -21.74070752338406365, 4.000000000000000000 ) ) ;
#12385 = LINE ( 'NONE', #45774, #134083 ) ;
#12386 = CARTESIAN_POINT ( 'NONE',  ( -2.207106781186522149, -11.24070752338417023, 5.000000000000000000 ) ) ;
#12387 = CARTESIAN_POINT ( 'NONE',  ( -9.183988606268997046, 28.73617430169793607, 5.000000000000000000 ) ) ;
#12388 = VERTEX_POINT ( 'NONE', #21609 ) ;
#12389 = CARTESIAN_POINT ( 'NONE',  ( 24.98330628287044419, 6.094999999999991758, 1.633150327867686880 ) ) ;
#12390 = ORIENTED_EDGE ( 'NONE', *, *, #72116, .F. ) ;
#12392 = ORIENTED_EDGE ( 'NONE', *, *, #28436, .T. ) ;
#12391 = ADVANCED_FACE ( 'NONE', ( #79613 ), #22279, .T. ) ;
#12393 = EDGE_LOOP ( 'NONE', ( #95364, #74800, #10690, #12903 ) ) ;
#12394 = VECTOR ( 'NONE', #64123, 1000.000000000000000 ) ;
#12395 = CARTESIAN_POINT ( 'NONE',  ( 42.93293019189810877, 1.637169565754156508, 6.110000000000000320 ) ) ;
#12396 = EDGE_LOOP ( 'NONE', ( #61610, #31871, #40293, #12241 ) ) ;
#12397 = CARTESIAN_POINT ( 'NONE',  ( 4.911592354503321545, 9.902892378096218942E-16, 0.000000000000000000 ) ) ;
#12398 = FACE_OUTER_BOUND ( 'NONE', #104938, .T. ) ;
#12399 = ADVANCED_FACE ( 'NONE', ( #22989 ), #12844, .F. ) ;
#12400 = ORIENTED_EDGE ( 'NONE', *, *, #25145, .T. ) ;
#12401 = DIRECTION ( 'NONE',  ( 0.7071067811865487940, -0.7071067811865463515, 0.000000000000000000 ) ) ;
#12402 = CARTESIAN_POINT ( 'NONE',  ( 3.183988606268992161, 28.73617430169789699, 5.000000000000000000 ) ) ;
#12403 = AXIS2_PLACEMENT_3D ( 'NONE', #110033, #45546, #10703 ) ;
#12404 = ADVANCED_FACE ( 'NONE', ( #78865 ), #101303, .F. ) ;
#12405 = EDGE_CURVE ( 'NONE', #33213, #10686, #88304, .T. ) ;
#12406 = LINE ( 'NONE', #77694, #15720 ) ;
#12407 = CARTESIAN_POINT ( 'NONE',  ( 27.52400138585429445, 22.03583458319437582, 4.979811245910090278 ) ) ;
#12408 = LINE ( 'NONE', #135638, #111917 ) ;
#12409 = VERTEX_POINT ( 'NONE', #110024 ) ;
#12410 = ORIENTED_EDGE ( 'NONE', *, *, #45473, .T. ) ;
#12412 = ORIENTED_EDGE ( 'NONE', *, *, #50669, .F. ) ;
#12411 = VECTOR ( 'NONE', #7435, 1000.000000000000000 ) ;
#12413 = ORIENTED_EDGE ( 'NONE', *, *, #116729, .F. ) ;
#12414 = CARTESIAN_POINT ( 'NONE',  ( -17.99451991528748351, 28.92564299267950645, 4.000000000000000000 ) ) ;
#12415 = FACE_OUTER_BOUND ( 'NONE', #81168, .T. ) ;
#12416 = EDGE_LOOP ( 'NONE', ( #25831, #110158, #103284, #78631 ) ) ;
#12417 = ADVANCED_FACE ( 'NONE', ( #57830 ), #78142, .F. ) ;
#12418 = ORIENTED_EDGE ( 'NONE', *, *, #72587, .T. ) ;
#12419 = LINE ( 'NONE', #57388, #95285 ) ;
#12420 = DIRECTION ( 'NONE',  ( 0.6830127018922181881, 0.6830127018922202975, -0.2588190451025214056 ) ) ;
#12421 = EDGE_CURVE ( 'NONE', #42811, #86060, #57124, .T. ) ;
#12422 = DIRECTION ( 'NONE',  ( 1.734723475976806848E-16, -1.000000000000000000, 0.000000000000000000 ) ) ;
#12423 = MECHANICAL_DESIGN_GEOMETRIC_PRESENTATION_REPRESENTATION (  '', ( #9840 ), #142126 ) ;
#12424 = ORIENTED_EDGE ( 'NONE', *, *, #127901, .T. ) ;
#12425 = CARTESIAN_POINT ( 'NONE',  ( -4.998069433178984333, -22.22500000000000142, 4.500000000000000888 ) ) ;
#12426 = CARTESIAN_POINT ( 'NONE',  ( 23.55512991947088963, -0.7407075233842735917, 4.307968247157003994 ) ) ;
#12427 = CARTESIAN_POINT ( 'NONE',  ( 28.50456980810189123, 6.871911579029510442, -3.967499999999998916 ) ) ;
#12428 = FILL_AREA_STYLE_COLOUR ( '', #9059 ) ;
#12429 = VERTEX_POINT ( 'NONE', #90429 ) ;
#12431 = DIRECTION ( 'NONE',  ( 0.7071067811865486830, -0.7071067811865464625, -0.000000000000000000 ) ) ;
#12430 = CARTESIAN_POINT ( 'NONE',  ( 109.4329301918981088, 1.637169565754156730, 6.110000000000001208 ) ) ;
#12432 = EDGE_CURVE ( 'NONE', #68468, #105421, #102023, .T. ) ;
#12433 = CARTESIAN_POINT ( 'NONE',  ( -8.816011393731004731, 28.73617430169781173, 5.000000000000000000 ) ) ;
#12434 = FACE_OUTER_BOUND ( 'NONE', #43790, .T. ) ;
#12435 = DIRECTION ( 'NONE',  ( -0.3543493200069162685, -0.000000000000000000, -0.9351131265310288487 ) ) ;
#12437 = ORIENTED_EDGE ( 'NONE', *, *, #59279, .F. ) ;
#12436 = DIRECTION ( 'NONE',  ( 0.3543493200069162685, -0.000000000000000000, -0.9351131265310288487 ) ) ;
#12438 = CARTESIAN_POINT ( 'NONE',  ( 6.066782984417857350, 4.584330080086930965E-16, 0.000000000000000000 ) ) ;
#12439 = ORIENTED_EDGE ( 'NONE', *, *, #123410, .F. ) ;
#12440 = CARTESIAN_POINT ( 'NONE',  ( -29.99999999999978328, 2.966399257802232459, 5.000000000000000000 ) ) ;
#12441 = ADVANCED_FACE ( 'NONE', ( #32493 ), #34625, .F. ) ;
#12442 = CARTESIAN_POINT ( 'NONE',  ( 128.0531643868628464, -51.20434817233906699, -36.87500513592858198 ) ) ;
#12443 = CARTESIAN_POINT ( 'NONE',  ( 33.27825451568553206, 8.259292476615634371, 11.78515199841158356 ) ) ;
#12445 = EDGE_LOOP ( 'NONE', ( #9388, #113424, #15376, #95714 ) ) ;
#12444 = CONICAL_SURFACE ( 'NONE', #102704, 2.500000000000000444, 0.9599310885968830309 ) ;
#12446 = LINE ( 'NONE', #69729, #32030 ) ;
#12447 = DIRECTION ( 'NONE',  ( -0.7071067811865486830, -0.7071067811865464625, -0.000000000000000000 ) ) ;
#12448 = FACE_OUTER_BOUND ( 'NONE', #91426, .T. ) ;
#12449 = ORIENTED_EDGE ( 'NONE', *, *, #124592, .T. ) ;
#12450 = DIRECTION ( 'NONE',  ( -2.781805975412905890E-17, 0.3543493200069152693, 0.9351131265310292928 ) ) ;
#12451 = ORIENTED_EDGE ( 'NONE', *, *, #81111, .T. ) ;
#12452 = DIRECTION ( 'NONE',  ( -0.6830127018922180770, -0.6830127018922204085, -0.2588190451025213501 ) ) ;
#12454 = EDGE_LOOP ( 'NONE', ( #79200, #13284, #57601, #54642 ) ) ;
#12453 = DIRECTION ( 'NONE',  ( 0.3543493200069162685, -0.000000000000000000, -0.9351131265310288487 ) ) ;
#12455 =( REPRESENTATION_RELATIONSHIP ('NONE','NONE', #69070, #118114 ) REPRESENTATION_RELATIONSHIP_WITH_TRANSFORMATION ( #65576 )SHAPE_REPRESENTATION_RELATIONSHIP( ) );
#12456 = EDGE_LOOP ( 'NONE', ( #77496, #31661, #138133, #139546 ) ) ;
#12457 = CARTESIAN_POINT ( 'NONE',  ( -28.17183060077627843, 9.759292476615620160, 4.000000000000000000 ) ) ;
#12458 = CARTESIAN_POINT ( 'NONE',  ( 27.99999999999996803, -49.14999999999999147, 53.92499999999996874 ) ) ;
#12459 = AXIS2_PLACEMENT_3D ( 'NONE', #51839, #20602, #21341 ) ;
#12460 = ORIENTED_EDGE ( 'NONE', *, *, #126042, .F. ) ;
#12461 = CARTESIAN_POINT ( 'NONE',  ( -44.99451991528749772, 28.92564299267969474, 4.000000000000000000 ) ) ;
#12462 = EDGE_CURVE ( 'NONE', #27078, #8640, #134676, .T. ) ;
#12463 = AXIS2_PLACEMENT_3D ( 'NONE', #26053, #24610, #36908 ) ;
#12464 = DIRECTION ( 'NONE',  ( 0.6830127018922180770, -0.6830127018922204085, -0.2588190451025213501 ) ) ;
#12465 = CARTESIAN_POINT ( 'NONE',  ( -25.17183060077628909, 21.75929247661549581, 4.000000000000000000 ) ) ;
#12466 = ORIENTED_EDGE ( 'NONE', *, *, #100476, .T. ) ;
#12467 = CARTESIAN_POINT ( 'NONE',  ( -12.18398860626900060, 28.73617430169795739, 5.000000000000000000 ) ) ;
#12468 = DIRECTION ( 'NONE',  ( -0.000000000000000000, 0.3543493200069152138, -0.9351131265310292928 ) ) ;
#12469 = LINE ( 'NONE', #11018, #758 ) ;
#12470 = LINE ( 'NONE', #134273, #74862 ) ;
#12471 = CARTESIAN_POINT ( 'NONE',  ( 125.5000000000000000, -3.441786896390352624, 7.166352137582667758 ) ) ;
#12472 = CARTESIAN_POINT ( 'NONE',  ( 30.68293019189811943, -1.637169565754159173, -6.109999999999999432 ) ) ;
#12473 = DIRECTION ( 'NONE',  ( 0.7071067811865487940, 0.7071067811865463515, 0.000000000000000000 ) ) ;
#12474 = ORIENTED_EDGE ( 'NONE', *, *, #140104, .T. ) ;
#12475 = VERTEX_POINT ( 'NONE', #46987 ) ;
#12476 = EDGE_LOOP ( 'NONE', ( #137015, #35794, #61325, #41176 ) ) ;
#12477 = VERTEX_POINT ( 'NONE', #131800 ) ;
#12478 =( GEOMETRIC_REPRESENTATION_CONTEXT ( 3 ) GLOBAL_UNCERTAINTY_ASSIGNED_CONTEXT ( ( #89525 ) ) GLOBAL_UNIT_ASSIGNED_CONTEXT ( ( #61011, #103038, #136367 ) ) REPRESENTATION_CONTEXT ( 'NONE', 'WORKASPACE' ) );
#12479 = ORIENTED_EDGE ( 'NONE', *, *, #69450, .T. ) ;
#12480 = VECTOR ( 'NONE', #79978, 1000.000000000000000 ) ;
#12481 = ORIENTED_EDGE ( 'NONE', *, *, #15351, .T. ) ;
#12482 = CARTESIAN_POINT ( 'NONE',  ( 0.7519484157939031466, -6.935901868405398574, -2.430364388579535628 ) ) ;
#12483 = CARTESIAN_POINT ( 'NONE',  ( -34.92500000000001137, 12.31448516125890436, 8.755464546898137357 ) ) ;
#12484 = ORIENTED_EDGE ( 'NONE', *, *, #127392, .F. ) ;
#12485 = CARTESIAN_POINT ( 'NONE',  ( 0.000000000000000000, 0.000000000000000000, 5.000000000000000000 ) ) ;
#12487 = VECTOR ( 'NONE', #116690, 1000.000000000000000 ) ;
#12486 = FACE_OUTER_BOUND ( 'NONE', #71804, .T. ) ;
#12488 = DIRECTION ( 'NONE',  ( -0.6830127018922180770, -0.6830127018922204085, -0.2588190451025213501 ) ) ;
#12489 = VECTOR ( 'NONE', #103707, 999.9999999999998863 ) ;
#12490 = FACE_OUTER_BOUND ( 'NONE', #78385, .T. ) ;
#12491 = CARTESIAN_POINT ( 'NONE',  ( 119.1462635252314470, -4.472830434245840259, 4.472830434245839371 ) ) ;
#12492 = ORIENTED_EDGE ( 'NONE', *, *, #38227, .T. ) ;
#12493 = CARTESIAN_POINT ( 'NONE',  ( -0.005480084712502889671, 28.92564299267938210, 4.000000000000000000 ) ) ;
#12494 = CARTESIAN_POINT ( 'NONE',  ( 14.01088028653938089, -22.02621442084248571, 4.990779571109220214 ) ) ;
#12495 = PLANE ( 'NONE',  #121330 ) ;
#12496 = DIRECTION ( 'NONE',  ( -1.000000000000000000, -1.224606353822377258E-16, -0.000000000000000000 ) ) ;
#12497 = LINE ( 'NONE', #54604, #114505 ) ;
#12498 =( BOUNDED_CURVE ( )  B_SPLINE_CURVE ( 2, ( #37473, #5513, #81709, #71527, #15652, #26580, #126585, #36732, #94671, #17134, #70136, #38887, #70825 ),
 .UNSPECIFIED., .F., .T. ) 
 B_SPLINE_CURVE_WITH_KNOTS ( ( 3, 2, 2, 2, 2, 2, 3 ),
 ( 0.06666666666665739538, 0.06944444444443478859, 0.07222222222221218180, 0.07499999999998957501, 0.07777777777776696821, 0.08055555555554437530, 0.08333333333332175463 ),
 .UNSPECIFIED. ) 
 CURVE ( )  GEOMETRIC_REPRESENTATION_ITEM ( )  RATIONAL_B_SPLINE_CURVE ( ( 1.000000000000113687, 0.9659258262889546254, 1.000000000000000000, 0.9659258262890683122, 1.000000000000000000, 0.9659258262890683122, 1.000000000000000000, 0.9659258262890683122, 1.000000000000000000, 0.9659258262890683122, 1.000000000000000000, 0.9659258262892103097, 0.9999999999998580025 ) ) 
 REPRESENTATION_ITEM ( '' )  );
#12499 = LINE ( 'NONE', #56780, #76953 ) ;
#12500 = CARTESIAN_POINT ( 'NONE',  ( -6.328169399223485314, -0.7407075233842735917, 4.000000000000000000 ) ) ;
#12501 = VECTOR ( 'NONE', #33656, 1000.000000000000000 ) ;
#12502 = CARTESIAN_POINT ( 'NONE',  ( 50.10002705046289151, 5.819803920172570422, 5.819803920172574863 ) ) ;
#12503 = DIRECTION ( 'NONE',  ( -0.7071067811865486830, 0.7071067811865464625, 0.000000000000000000 ) ) ;
#12504 = VECTOR ( 'NONE', #43830, 999.9999999999998863 ) ;
#12505 = CARTESIAN_POINT ( 'NONE',  ( -24.15612307739226239, -22.22500000000000853, 4.000000000000000000 ) ) ;
#12506 = ORIENTED_EDGE ( 'NONE', *, *, #16087, .T. ) ;
#12507 = ORIENTED_EDGE ( 'NONE', *, *, #140064, .T. ) ;
#12508 = CARTESIAN_POINT ( 'NONE',  ( 49.56249999999999289, -5.819803920172572198, -5.819803920172573086 ) ) ;
#12509 = CARTESIAN_POINT ( 'NONE',  ( 0.000000000000000000, 0.000000000000000000, 5.000000000000000000 ) ) ;
#12510 = VECTOR ( 'NONE', #129450, 1000.000000000000000 ) ;
#12511 = ORIENTED_EDGE ( 'NONE', *, *, #62865, .F. ) ;
#12512 = DIRECTION ( 'NONE',  ( -0.6830127018922181881, 0.6830127018922202975, -0.2588190451025214056 ) ) ;
#12513 = DIRECTION ( 'NONE',  ( 0.000000000000000000, 1.000000000000000000, 0.000000000000000000 ) ) ;
#12514 = VECTOR ( 'NONE', #141323, 1000.000000000000000 ) ;
#12515 = EDGE_CURVE ( 'NONE', #89327, #103007, #543, .T. ) ;
#12516 = CARTESIAN_POINT ( 'NONE',  ( 40.25043019189809712, 3.055000000000002824, -5.291415217122919401 ) ) ;
#12517 = ORIENTED_EDGE ( 'NONE', *, *, #141699, .T. ) ;
#12518 = EDGE_CURVE ( 'NONE', #102268, #51675, #34081, .T. ) ;
#12519 = CARTESIAN_POINT ( 'NONE',  ( 15.44591897758377286, -1.592173378680614926, 4.204195949441833058 ) ) ;
#12520 = ORIENTED_EDGE ( 'NONE', *, *, #20065, .F. ) ;
#12521 = VECTOR ( 'NONE', #2815, 999.9999999999998863 ) ;
#12522 = CARTESIAN_POINT ( 'NONE',  ( -34.42500000000001137, 0.000000000000000000, 4.500000000000000888 ) ) ;
#12523 = CARTESIAN_POINT ( 'NONE',  ( -18.48921356237309510, -27.52281430457068367, 5.000000000000000000 ) ) ;
#12524 = EDGE_CURVE ( 'NONE', #89838, #115114, #23749, .T. ) ;
#12525 = ORIENTED_EDGE ( 'NONE', *, *, #30202, .F. ) ;
#12526 = CARTESIAN_POINT ( 'NONE',  ( 34.92499999999998295, 22.22500000000000142, 4.000000000000000000 ) ) ;
#12527 = ADVANCED_FACE ( 'NONE', ( #132550 ), #121611, .T. ) ;
#12528 = EDGE_CURVE ( 'NONE', #22434, #94617, #72301, .T. ) ;
#12529 = ORIENTED_EDGE ( 'NONE', *, *, #57276, .F. ) ;
#12530 = LINE ( 'NONE', #68391, #132754 ) ;
#12531 = CARTESIAN_POINT ( 'NONE',  ( -31.11017322888190151, -22.22500000000000497, 4.785647885939355639 ) ) ;
#12532 = PLANE ( 'NONE',  #70892 ) ;
#12533 = CARTESIAN_POINT ( 'NONE',  ( 8.423184310185783730, -2.500000000000000444, 3.061616997868384127E-16 ) ) ;
#12534 = LINE ( 'NONE', #77813, #44044 ) ;
#12535 = CARTESIAN_POINT ( 'NONE',  ( -14.28769006033961020, -21.73547319004781286, 4.999917730833664642 ) ) ;
#12536 = ADVANCED_FACE ( 'NONE', ( #70158 ), #83131, .T. ) ;
#12537 = EDGE_CURVE ( 'NONE', #25811, #77500, #26602, .T. ) ;
#12538 = EDGE_LOOP ( 'NONE', ( #72770, #101368, #84208, #65762 ) ) ;
#12539 = DIRECTION ( 'NONE',  ( 0.7071067811865487940, 0.7071067811865463515, 0.000000000000000000 ) ) ;
#12540 = CARTESIAN_POINT ( 'NONE',  ( 57.37043019189810877, -3.055000000000001492, 5.291415217122917625 ) ) ;
#12541 = DIRECTION ( 'NONE',  ( 0.7071067811865487940, 0.7071067811865463515, 0.000000000000000000 ) ) ;
#12542 = ADVANCED_FACE ( 'NONE', ( #59269 ), #114317, .F. ) ;
#12543 = DIRECTION ( 'NONE',  ( -0.6830127018922180770, -0.6830127018922204085, -0.2588190451025213501 ) ) ;
#12544 = FACE_OUTER_BOUND ( 'NONE', #137993, .T. ) ;
#12545 = ORIENTED_EDGE ( 'NONE', *, *, #22063, .F. ) ;
#12546 = CARTESIAN_POINT ( 'NONE',  ( 78.18398860626899705, 28.73617430169841924, 5.000000000000000000 ) ) ;
#12547 = VERTEX_POINT ( 'NONE', #17158 ) ;
#12548 = VECTOR ( 'NONE', #140766, 1000.000000000000000 ) ;
#12549 = ADVANCED_FACE ( 'NONE', ( #91846 ), #58578, .F. ) ;
#12550 = DIRECTION ( 'NONE',  ( -0.7071067811865486830, 0.7071067811865464625, 0.000000000000000000 ) ) ;
#12551 = EDGE_LOOP ( 'NONE', ( #39242, #141587, #84820, #142515 ) ) ;
#12552 = DIRECTION ( 'NONE',  ( 1.000000000000000000, 0.000000000000000000, 0.000000000000000000 ) ) ;
#12553 = DIRECTION ( 'NONE',  ( 0.3543493200069162685, -0.000000000000000000, -0.9351131265310288487 ) ) ;
#12554 = DIRECTION ( 'NONE',  ( -0.7071067811865487940, 0.7071067811865463515, 0.000000000000000000 ) ) ;
#12555 = DIRECTION ( 'NONE',  ( 0.7071067811865486830, -0.7071067811865464625, -0.000000000000000000 ) ) ;
#12556 = FACE_BOUND ( 'NONE', #79977, .T. ) ;
#12557 = LINE ( 'NONE', #22691, #135924 ) ;
#12558 = CARTESIAN_POINT ( 'NONE',  ( -45.18398860626900415, 28.73617430169818832, 5.000000000000000000 ) ) ;
#12559 = FACE_OUTER_BOUND ( 'NONE', #61235, .T. ) ;
#12561 = ORIENTED_EDGE ( 'NONE', *, *, #96012, .F. ) ;
#12560 = CARTESIAN_POINT ( 'NONE',  ( 48.48921356237309510, -27.52281430457089328, 5.000000000000000000 ) ) ;
#12563 = EDGE_CURVE ( 'NONE', #11170, #60604, #38208, .T. ) ;
#12562 = AXIS2_PLACEMENT_3D ( 'NONE', #105308, #115433, #5964 ) ;
#12564 = CARTESIAN_POINT ( 'NONE',  ( 12.40000000000000213, 9.521314400968980422E-16, 0.000000000000000000 ) ) ;
#12565 = ORIENTED_EDGE ( 'NONE', *, *, #113633, .F. ) ;
#12566 = AXIS2_PLACEMENT_3D ( 'NONE', #526, #97718, #131789 ) ;
#12567 = VERTEX_POINT ( 'NONE', #36753 ) ;
#12568 = CARTESIAN_POINT ( 'NONE',  ( 78.07876352523145158, -7.482591942790325086E-16, 6.109999999999998543 ) ) ;
#12569 = ORIENTED_EDGE ( 'NONE', *, *, #38528, .F. ) ;
#12570 = PLANE ( 'NONE',  #131010 ) ;
#12571 = DIRECTION ( 'NONE',  ( -0.7071067811865486830, -0.7071067811865464625, 0.000000000000000000 ) ) ;
#12572 = VECTOR ( 'NONE', #130198, 1000.000000000000000 ) ;
#12573 = EDGE_CURVE ( 'NONE', #23940, #60723, #14994, .T. ) ;
#12574 = VERTEX_POINT ( 'NONE', #124484 ) ;
#12575 = DIRECTION ( 'NONE',  ( -0.000000000000000000, 0.000000000000000000, 1.000000000000000000 ) ) ;
#12576 = DIRECTION ( 'NONE',  ( -0.000000000000000000, 0.3543493200069153248, 0.9351131265310292928 ) ) ;
#12577 = EDGE_CURVE ( 'NONE', #83408, #11149, #138221, .T. ) ;
#12578 = CARTESIAN_POINT ( 'NONE',  ( 59.99451991528749772, 28.92564299267980132, 4.000000000000000000 ) ) ;
#12579 = SURFACE_STYLE_FILL_AREA ( #99574 ) ;
#12580 = VECTOR ( 'NONE', #80667, 1000.000000000000000 ) ;
#12581 = DIRECTION ( 'NONE',  ( -0.7071067811865486830, -0.7071067811865464625, 0.000000000000000000 ) ) ;
#12582 = EDGE_CURVE ( 'NONE', #88566, #120007, #126604, .T. ) ;
#12583 = DIRECTION ( 'NONE',  ( -1.000000000000000000, -0.000000000000000000, -0.000000000000000000 ) ) ;
#12584 = CARTESIAN_POINT ( 'NONE',  ( -15.85181644961845748, 17.25929247661554200, 8.802941693769165354 ) ) ;
#12585 = EDGE_LOOP ( 'NONE', ( #64684, #79963, #89047, #33999 ) ) ;
#12586 = ORIENTED_EDGE ( 'NONE', *, *, #26386, .T. ) ;
#12587 = DIRECTION ( 'NONE',  ( 0.000000000000000000, 1.000000000000000000, 0.000000000000000000 ) ) ;
#12588 = DIRECTION ( 'NONE',  ( 0.7071067811865487940, 0.7071067811865463515, 0.000000000000000000 ) ) ;
#12589 = VERTEX_POINT ( 'NONE', #125205 ) ;
#12590 = ADVANCED_FACE ( 'NONE', ( #69409 ), #25158, .F. ) ;
#12591 = ORIENTED_EDGE ( 'NONE', *, *, #7259, .F. ) ;
#12592 = ORIENTED_EDGE ( 'NONE', *, *, #69124, .T. ) ;
#12593 = VECTOR ( 'NONE', #96398, 1000.000000000000000 ) ;
#12594 = CARTESIAN_POINT ( 'NONE',  ( 27.12543019189810067, 5.291415217122919401, 3.055000000000002824 ) ) ;
#12595 = VERTEX_POINT ( 'NONE', #125928 ) ;
#12596 = CARTESIAN_POINT ( 'NONE',  ( -6.183988606268994381, 28.73617430169791476, 5.000000000000000000 ) ) ;
#12597 = EDGE_CURVE ( 'NONE', #139414, #128406, #70845, .T. ) ;
#12598 = AXIS2_PLACEMENT_3D ( 'NONE', #83213, #126689, #71630 ) ;
#12599 = CARTESIAN_POINT ( 'NONE',  ( 89.76669371712954160, -7.949999999999998401, 2.130196079827423983 ) ) ;
#12600 = VECTOR ( 'NONE', #25212, 1000.000000000000000 ) ;
#12601 = CARTESIAN_POINT ( 'NONE',  ( 30.81663961620377279, -1.633150327867691987, -6.094999999999989093 ) ) ;
#12602 = VECTOR ( 'NONE', #94803, 999.9999999999998863 ) ;
#12603 = CARTESIAN_POINT ( 'NONE',  ( 15.53628966088338004, 3.145490004818007446, -30.03788422909113720 ) ) ;
#12604 = ORIENTED_EDGE ( 'NONE', *, *, #69220, .F. ) ;
#12605 = EDGE_CURVE ( 'NONE', #81561, #16866, #16407, .T. ) ;
#12606 = CARTESIAN_POINT ( 'NONE',  ( -36.48921356237310221, -27.52281430457080802, 5.000000000000000000 ) ) ;
#12607 = DIRECTION ( 'NONE',  ( 0.000000000000000000, -1.000000000000000000, 0.000000000000000000 ) ) ;
#12608 = CARTESIAN_POINT ( 'NONE',  ( -68.99451991528748351, 28.92564299267986172, 4.000000000000000000 ) ) ;
#12610 = ORIENTED_EDGE ( 'NONE', *, *, #12709, .T. ) ;
#12609 = DIRECTION ( 'NONE',  ( -0.7071067811865486830, 0.7071067811865464625, 0.000000000000000000 ) ) ;
#12611 = EDGE_LOOP ( 'NONE', ( #43002, #78438, #38669, #119267 ) ) ;
#12612 = SURFACE_SIDE_STYLE ('',( #111952 ) ) ;
#12613 = CARTESIAN_POINT ( 'NONE',  ( 12.48921356237309155, -27.52281430457064104, 5.000000000000000000 ) ) ;
#12614 = ORIENTED_EDGE ( 'NONE', *, *, #46183, .T. ) ;
#12615 = FACE_OUTER_BOUND ( 'NONE', #113746, .T. ) ;
#12616 = CYLINDRICAL_SURFACE ( 'NONE', #82705, 2.500000000000000000 ) ;
#12617 = ORIENTED_EDGE ( 'NONE', *, *, #54497, .F. ) ;
#12618 = ADVANCED_FACE ( 'NONE', ( #60705 ), #105564, .F. ) ;
#12619 = LINE ( 'NONE', #25638, #139849 ) ;
#12620 = SURFACE_SIDE_STYLE ('',( #89473 ) ) ;
#12621 = CARTESIAN_POINT ( 'NONE',  ( -21.18398860626899349, 28.73617430169802134, 5.000000000000000000 ) ) ;
#12622 = LINE ( 'NONE', #59050, #48515 ) ;
#12623 = LINE ( 'NONE', #101055, #88683 ) ;
#12624 = CARTESIAN_POINT ( 'NONE',  ( -18.48921356237309510, -27.52281430457068367, 5.000000000000000000 ) ) ;
#12625 = DIRECTION ( 'NONE',  ( 0.7071067811865487940, 0.7071067811865463515, 0.000000000000000000 ) ) ;
#12626 = ADVANCED_FACE ( 'NONE', ( #15673 ), #14292, .F. ) ;
#12627 = DIRECTION ( 'NONE',  ( 0.7071067811865487940, 0.7071067811865463515, 0.000000000000000000 ) ) ;
#12628 = EDGE_LOOP ( 'NONE', ( #75920, #3059, #132140, #82577 ) ) ;
#12629 = ORIENTED_EDGE ( 'NONE', *, *, #141179, .T. ) ;
#12630 = LINE ( 'NONE', #80774, #117344 ) ;
#12631 = DIRECTION ( 'NONE',  ( 0.3543493200069162685, -0.000000000000000000, -0.9351131265310288487 ) ) ;
#12632 = CARTESIAN_POINT ( 'NONE',  ( -0.3129301918981139408, -2.126176841940956130, 7.934999999999991616 ) ) ;
#12633 = LINE ( 'NONE', #80777, #85252 ) ;
#12634 = EDGE_CURVE ( 'NONE', #108829, #13986, #93284, .T. ) ;
#12635 = ORIENTED_EDGE ( 'NONE', *, *, #140543, .F. ) ;
#12636 = CARTESIAN_POINT ( 'NONE',  ( 0.000000000000000000, 0.000000000000000000, 5.000000000000000000 ) ) ;
#12637 = FACE_OUTER_BOUND ( 'NONE', #17083, .T. ) ;
#12638 =( NAMED_UNIT ( * ) SI_UNIT ( $, .STERADIAN. ) SOLID_ANGLE_UNIT ( ) );
#12639 = ORIENTED_EDGE ( 'NONE', *, *, #79343, .T. ) ;
#12640 = FACE_OUTER_BOUND ( 'NONE', #48627, .T. ) ;
#12641 = DIRECTION ( 'NONE',  ( -0.7071067811865486830, -0.7071067811865464625, -0.000000000000000000 ) ) ;
#12642 = UNCERTAINTY_MEASURE_WITH_UNIT (LENGTH_MEASURE( 1.000000000000000082E-05 ), #107224, 'distance_accuracy_value', 'NONE');
#12643 = DIRECTION ( 'NONE',  ( -0.7071067811865487940, 0.7071067811865463515, -0.000000000000000000 ) ) ;
#12644 = CARTESIAN_POINT ( 'NONE',  ( 52.99543019189811588, 5.291415217122917625, 3.055000000000002380 ) ) ;
#12645 = VECTOR ( 'NONE', #57372, 1000.000000000000227 ) ;
#12646 = PLANE ( 'NONE',  #58082 ) ;
#12647 = EDGE_CURVE ( 'NONE', #134939, #86178, #117158, .T. ) ;
#12648 = DIRECTION ( 'NONE',  ( -0.000000000000000000, 0.3543493200069153248, 0.9351131265310292928 ) ) ;
#12649 = CARTESIAN_POINT ( 'NONE',  ( -57.29974487139158157, -27.71228299555246011, 4.000000000000000000 ) ) ;
#12650 = ORIENTED_EDGE ( 'NONE', *, *, #54130, .F. ) ;
#12651 = CARTESIAN_POINT ( 'NONE',  ( -17.67183060077635304, -15.74070752338413115, 4.000000000000000000 ) ) ;
#12652 = ORIENTED_EDGE ( 'NONE', *, *, #37822, .T. ) ;
#12653 = LINE ( 'NONE', #1742, #82516 ) ;
#12654 = DIRECTION ( 'NONE',  ( -0.7071067811865487940, 0.7071067811865463515, 0.000000000000000000 ) ) ;
#12655 = FACE_OUTER_BOUND ( 'NONE', #45220, .T. ) ;
#12656 = DIRECTION ( 'NONE',  ( -0.7071067811865487940, 0.7071067811865463515, -0.000000000000000000 ) ) ;
#12657 = ADVANCED_FACE ( 'NONE', ( #41048 ), #85248, .F. ) ;
#12658 = FACE_OUTER_BOUND ( 'NONE', #130438, .T. ) ;
#12659 = DIRECTION ( 'NONE',  ( 0.000000000000000000, 0.000000000000000000, -1.000000000000000000 ) ) ;
#12660 = ORIENTED_EDGE ( 'NONE', *, *, #78037, .F. ) ;
#12661 = VERTEX_POINT ( 'NONE', #83875 ) ;
#12662 = LINE ( 'NONE', #14084, #37139 ) ;
#12663 = CARTESIAN_POINT ( 'NONE',  ( 26.51360224591381254, -6.350000000000003197, -3.888253587292850026E-16 ) ) ;
#12664 = UNCERTAINTY_MEASURE_WITH_UNIT (LENGTH_MEASURE( 1.000000000000000082E-05 ), #120019, 'distance_accuracy_value', 'NONE');
#12665 = CYLINDRICAL_SURFACE ( 'NONE', #77498, 2.500000000000000000 ) ;
#12666 = CARTESIAN_POINT ( 'NONE',  ( 15.64997294953710671, -4.461849672132299105, 4.461849672132299993 ) ) ;
#12667 = CARTESIAN_POINT ( 'NONE',  ( 70.95419371712955581, 6.884901960086283523, 3.975000000000002753 ) ) ;
#12668 = DIRECTION ( 'NONE',  ( -0.6830127018922180770, -0.6830127018922204085, -0.2588190451025213501 ) ) ;
#12669 = PRESENTATION_LAYER_ASSIGNMENT (  '', '', ( #107567 ) ) ;
#12670 = DIRECTION ( 'NONE',  ( -0.7071067811865487940, 0.7071067811865463515, 0.000000000000000000 ) ) ;
#12671 = ORIENTED_EDGE ( 'NONE', *, *, #60963, .F. ) ;
#12672 = CARTESIAN_POINT ( 'NONE',  ( 72.75000000000000000, -9.735942053221458872E-16, 7.950000000000000178 ) ) ;
#12673 = DIRECTION ( 'NONE',  ( 1.000000000000000000, 0.000000000000000000, 0.000000000000000000 ) ) ;
#12674 = VECTOR ( 'NONE', #143024, 999.9999999999998863 ) ;
#12675 = CARTESIAN_POINT ( 'NONE',  ( 25.17665910159957221, 5.259292476615669010, 15.86257073897091807 ) ) ;
#12676 = DIRECTION ( 'NONE',  ( -1.000000000000000000, -0.000000000000000000, -0.000000000000000000 ) ) ;
#12677 = ORIENTED_EDGE ( 'NONE', *, *, #23334, .F. ) ;
#12678 = DIRECTION ( 'NONE',  ( -0.7071067811865486830, -0.7071067811865464625, 0.000000000000000000 ) ) ;
#12679 = AXIS2_PLACEMENT_3D ( 'NONE', #82384, #60661, #104826 ) ;
#12680 = CARTESIAN_POINT ( 'NONE',  ( 4.499999999999983125, 4.087461875839196956, 4.000000000000000000 ) ) ;
#12681 = CARTESIAN_POINT ( 'NONE',  ( 66.93793019189809002, -6.110000000000001208, 1.637169565754158951 ) ) ;
#12682 = ORIENTED_EDGE ( 'NONE', *, *, #36771, .F. ) ;
#12683 = EDGE_CURVE ( 'NONE', #110962, #87033, #130214, .T. ) ;
#12684 = ORIENTED_EDGE ( 'NONE', *, *, #24389, .T. ) ;
#12685 = LINE ( 'NONE', #125030, #96195 ) ;
#12686 = PLANE ( 'NONE',  #129941 ) ;
#12687 = CARTESIAN_POINT ( 'NONE',  ( 27.18398860626900060, 28.73617430169806042, 5.000000000000000000 ) ) ;
#12688 = ADVANCED_FACE ( 'NONE', ( #7684 ), #75137, .F. ) ;
#12690 = ORIENTED_EDGE ( 'NONE', *, *, #39874, .T. ) ;
#12689 = FACE_OUTER_BOUND ( 'NONE', #107718, .T. ) ;
#12691 = FACE_OUTER_BOUND ( 'NONE', #89945, .T. ) ;
#12692 = CARTESIAN_POINT ( 'NONE',  ( -25.39999999999996305, 3.061616997868383141E-16, -2.500000000000000000 ) ) ;
#12693 = DIRECTION ( 'NONE',  ( 0.000000000000000000, 1.000000000000000000, 0.000000000000000000 ) ) ;
#12694 = LINE ( 'NONE', #137364, #32252 ) ;
#12695 = ORIENTED_EDGE ( 'NONE', *, *, #120626, .T. ) ;
#12696 = VECTOR ( 'NONE', #131630, 1000.000000000000000 ) ;
#12698 = VERTEX_POINT ( 'NONE', #96123 ) ;
#12697 = EDGE_CURVE ( 'NONE', #124724, #88761, #126466, .T. ) ;
#12699 = EDGE_CURVE ( 'NONE', #130956, #70680, #30905, .T. ) ;
#12700 = CARTESIAN_POINT ( 'NONE',  ( 56.72959685856476142, -6.110000000000000320, -1.637169565754161393 ) ) ;
#12701 = AXIS2_PLACEMENT_3D ( 'NONE', #66145, #10987, #99 ) ;
#12702 = AXIS2_PLACEMENT_3D ( 'NONE', #107369, #129121, #74039 ) ;
#12703 = VERTEX_POINT ( 'NONE', #30159 ) ;
#12704 = EDGE_CURVE ( 'NONE', #63837, #93434, #114860, .T. ) ;
#12705 = VECTOR ( 'NONE', #125990, 1000.000000000000000 ) ;
#12706 = CARTESIAN_POINT ( 'NONE',  ( 11.25346039003969523, -2.055000000000000160, 2.789133085058097101E-16 ) ) ;
#12707 = CARTESIAN_POINT ( 'NONE',  ( 34.92499999999998295, -20.14387692260739016, 4.000000000000000000 ) ) ;
#12709 = EDGE_CURVE ( 'NONE', #129026, #131707, #95419, .T. ) ;
#12708 = DIRECTION ( 'NONE',  ( 0.000000000000000000, -1.000000000000000000, 0.000000000000000000 ) ) ;
#12710 = CARTESIAN_POINT ( 'NONE',  ( -29.99999999999979750, -6.108550654416986525, -3.114665004255035452 ) ) ;
#12711 = DIRECTION ( 'NONE',  ( -1.000000000000000000, -1.224606353822377258E-16, -0.000000000000000000 ) ) ;
#12712 = ORIENTED_EDGE ( 'NONE', *, *, #86051, .T. ) ;
#12713 = ORIENTED_EDGE ( 'NONE', *, *, #92159, .T. ) ;
#12714 = EDGE_CURVE ( 'NONE', #136079, #127597, #64962, .T. ) ;
#12715 = DIRECTION ( 'NONE',  ( 0.7071067811865487940, 0.7071067811865463515, 0.000000000000000000 ) ) ;
#12716 = SURFACE_STYLE_USAGE ( .BOTH. , #25015 ) ;
#12717 = EDGE_CURVE ( 'NONE', #110945, #28039, #141060, .T. ) ;
#12718 = ORIENTED_EDGE ( 'NONE', *, *, #91564, .T. ) ;
#12719 = DIRECTION ( 'NONE',  ( 1.000000000000000000, 1.224606353822377258E-16, 0.000000000000000000 ) ) ;
#12720 = DIRECTION ( 'NONE',  ( -0.7071067811865486830, -0.7071067811865464625, 0.000000000000000000 ) ) ;
#12721 = CARTESIAN_POINT ( 'NONE',  ( 20.29289321881331531, -6.740707523384211086, 5.000000000000000000 ) ) ;
#12722 = VERTEX_POINT ( 'NONE', #107716 ) ;
#12723 = EDGE_CURVE ( 'NONE', #489, #35500, #8374, .T. ) ;
#12724 = FACE_BOUND ( 'NONE', #5015, .T. ) ;
#12725 = DIRECTION ( 'NONE',  ( 0.6830127018922180770, -0.6830127018922204085, -0.2588190451025213501 ) ) ;
#12726 = CARTESIAN_POINT ( 'NONE',  ( 7.939999999999994174, -39.93000000000000682, -12.24789999999999957 ) ) ;
#12727 = CARTESIAN_POINT ( 'NONE',  ( -12.69999999999998153, 0.000000000000000000, 0.000000000000000000 ) ) ;
#12728 = ADVANCED_FACE ( 'NONE', ( #41765 ), #106265, .F. ) ;
#12729 = CARTESIAN_POINT ( 'NONE',  ( 32.99451991528749062, 28.92564299267960948, 4.000000000000000000 ) ) ;
#12730 = CARTESIAN_POINT ( 'NONE',  ( 61.51850992298124510, -5.517728913817708470E-14, 1.431893130534310539E-16 ) ) ;
#12731 = ORIENTED_EDGE ( 'NONE', *, *, #123005, .T. ) ;
#12732 = ORIENTED_EDGE ( 'NONE', *, *, #99913, .T. ) ;
#12733 = CARTESIAN_POINT ( 'NONE',  ( 107.9745968585647660, 1.637169565754164280, -6.109999999999996767 ) ) ;
#12734 = ORIENTED_EDGE ( 'NONE', *, *, #64284, .T. ) ;
#12735 = CARTESIAN_POINT ( 'NONE',  ( -30.18398860626900060, 28.73617430169808173, 5.000000000000000000 ) ) ;
#12736 = ORIENTED_EDGE ( 'NONE', *, *, #86410, .F. ) ;
#12737 = DIRECTION ( 'NONE',  ( 0.5735764363510444941, 0.8191520442889929088, 0.000000000000000000 ) ) ;
#12738 = CARTESIAN_POINT ( 'NONE',  ( -27.48921356237309155, -27.52281430457074762, 5.000000000000000000 ) ) ;
#12739 = LINE ( 'NONE', #1826, #88801 ) ;
#12740 = EDGE_LOOP ( 'NONE', ( #67069, #104615, #85489, #58976 ) ) ;
#12741 = DIRECTION ( 'NONE',  ( -0.7071067811865486830, -0.7071067811865464625, 0.000000000000000000 ) ) ;
#12742 = CARTESIAN_POINT ( 'NONE',  ( 55.56056557994604361, -52.00875322212549179, -39.86617647058817937 ) ) ;
#12743 = CARTESIAN_POINT ( 'NONE',  ( -17.51078643762690845, -27.52281430457043143, 5.000000000000000000 ) ) ;
#12745 = FACE_OUTER_BOUND ( 'NONE', #15451, .T. ) ;
#12744 = CARTESIAN_POINT ( 'NONE',  ( 68.22916666666665719, 7.950000000000001954, -2.130196079827421762 ) ) ;
#12746 = EDGE_CURVE ( 'NONE', #56310, #52592, #75830, .T. ) ;
#12747 = PLANE ( 'NONE',  #60100 ) ;
#12748 = CARTESIAN_POINT ( 'NONE',  ( 33.18398860626899705, 28.73617430169810305, 5.000000000000000000 ) ) ;
#12749 = ORIENTED_EDGE ( 'NONE', *, *, #45996, .T. ) ;
#12750 = CARTESIAN_POINT ( 'NONE',  ( 87.18749999999998579, -5.819803920172573974, 5.819803920172573086 ) ) ;
#12751 = EDGE_CURVE ( 'NONE', #26635, #44135, #94688, .T. ) ;
#12752 = DIRECTION ( 'NONE',  ( 0.7071067811865487940, 0.7071067811865463515, 0.000000000000000000 ) ) ;
#12753 = ORIENTED_EDGE ( 'NONE', *, *, #3106, .T. ) ;
#12754 = ORIENTED_EDGE ( 'NONE', *, *, #129002, .F. ) ;
#12755 = VERTEX_POINT ( 'NONE', #117854 ) ;
#12756 = CARTESIAN_POINT ( 'NONE',  ( 52.06293019189810423, 1.637169565754157174, 6.110000000000002984 ) ) ;
#12757 = ORIENTED_EDGE ( 'NONE', *, *, #103142, .F. ) ;
#12758 = EDGE_CURVE ( 'NONE', #18442, #59390, #18541, .T. ) ;
#12759 = DIRECTION ( 'NONE',  ( -0.7071067811865486830, -0.7071067811865464625, 0.000000000000000000 ) ) ;
#12760 = VECTOR ( 'NONE', #119467, 999.9999999999998863 ) ;
#12761 = CARTESIAN_POINT ( 'NONE',  ( 10.39997294953710671, 4.461849672132297329, -4.461849672132302658 ) ) ;
#12762 = CARTESIAN_POINT ( 'NONE',  ( 90.85459685856478984, -1.637169565754161615, 6.110000000000000320 ) ) ;
#12763 = CARTESIAN_POINT ( 'NONE',  ( -31.03340032343004040, 6.759292476615653023, 12.28218704918514881 ) ) ;
#12764 = ORIENTED_EDGE ( 'NONE', *, *, #33628, .F. ) ;
#12765 = VECTOR ( 'NONE', #98451, 999.9999999999998863 ) ;
#12766 = ADVANCED_FACE ( 'NONE', ( #138947 ), #1447, .T. ) ;
#12767 = ORIENTED_EDGE ( 'NONE', *, *, #117103, .T. ) ;
#12768 = CARTESIAN_POINT ( 'NONE',  ( -15.18398860626900237, 28.73617430169797871, 5.000000000000000000 ) ) ;
#12769 = CARTESIAN_POINT ( 'NONE',  ( 4.828169399223493308, 12.75929247661559351, 4.000000000000000000 ) ) ;
#12770 = EDGE_LOOP ( 'NONE', ( #133551, #5253, #91523, #3136 ) ) ;
#12771 = SURFACE_STYLE_USAGE ( .BOTH. , #69330 ) ;
#12772 = CARTESIAN_POINT ( 'NONE',  ( -12.69999999999998153, 0.000000000000000000, 0.000000000000000000 ) ) ;
#12773 = LINE ( 'NONE', #57050, #24311 ) ;
#12774 = ORIENTED_EDGE ( 'NONE', *, *, #128213, .T. ) ;
#12775 = CARTESIAN_POINT ( 'NONE',  ( -41.39513766812454776, 21.75929247661549226, 21.32995629748196009 ) ) ;
#12776 = VECTOR ( 'NONE', #53693, 1000.000000000000000 ) ;
#12777 = ORIENTED_EDGE ( 'NONE', *, *, #89514, .T. ) ;
#12778 = ORIENTED_EDGE ( 'NONE', *, *, #109795, .T. ) ;
#12779 = VERTEX_POINT ( 'NONE', #39650 ) ;
#12780 =( LENGTH_UNIT ( ) NAMED_UNIT ( * ) SI_UNIT ( .MILLI., .METRE. ) );
#12781 = CYLINDRICAL_SURFACE ( 'NONE', #86299, 4.375000000000001776 ) ;
#12782 = LINE ( 'NONE', #4007, #102656 ) ;
#12783 = ADVANCED_FACE ( 'NONE', ( #37128 ), #33074, .F. ) ;
#12784 = CARTESIAN_POINT ( 'NONE',  ( 25.35824297541124750, 15.75929247661555799, 19.34181609438693528 ) ) ;
#12785 = EDGE_CURVE ( 'NONE', #40894, #64109, #81384, .T. ) ;
#12786 = CARTESIAN_POINT ( 'NONE',  ( -19.59167451900987089, -0.7407075233842665973, 14.76736230305375841 ) ) ;
#12787 = ORIENTED_EDGE ( 'NONE', *, *, #45365, .T. ) ;
#12788 = CARTESIAN_POINT ( 'NONE',  ( 13.29826936130429260, -2.500000000000001776, 0.000000000000000000 ) ) ;
#12789 = VECTOR ( 'NONE', #84732, 1000.000000000000000 ) ;
#12790 = VECTOR ( 'NONE', #90916, 1000.000000000000000 ) ;
#12791 = CARTESIAN_POINT ( 'NONE',  ( 20.68706980810189222, -2.126176841940956130, 7.934999999999991616 ) ) ;
#12792 = DIRECTION ( 'NONE',  ( -1.000000000000000000, -1.224606353822377258E-16, -0.000000000000000000 ) ) ;
#12793 = AXIS2_PLACEMENT_3D ( 'NONE', #90253, #37324, #134502 ) ;
#12794 = CARTESIAN_POINT ( 'NONE',  ( -27.70701326429286127, -21.74070752338406365, 4.999753212805221558 ) ) ;
#12795 = EDGE_CURVE ( 'NONE', #8995, #116753, #143214, .T. ) ;
#12796 = AXIS2_PLACEMENT_3D ( 'NONE', #63925, #87097, #40748 ) ;
#12797 = LINE ( 'NONE', #124429, #65264 ) ;
#12798 = ORIENTED_EDGE ( 'NONE', *, *, #28759, .T. ) ;
#12799 = ORIENTED_EDGE ( 'NONE', *, *, #1838, .F. ) ;
#12800 = ORIENTED_EDGE ( 'NONE', *, *, #95656, .F. ) ;
#12801 = DIRECTION ( 'NONE',  ( 1.000000000000000000, 0.000000000000000000, 0.000000000000000000 ) ) ;
#12802 = CARTESIAN_POINT ( 'NONE',  ( -34.92500000000001137, -18.18334561358938473, 4.500000000000000888 ) ) ;
#12803 = UNCERTAINTY_MEASURE_WITH_UNIT (LENGTH_MEASURE( 1.000000000000000082E-05 ), #9369, 'distance_accuracy_value', 'NONE');
#12804 = PLANE ( 'NONE',  #128302 ) ;
#12806 = EDGE_CURVE ( 'NONE', #32218, #22939, #65707, .T. ) ;
#12805 = FACE_OUTER_BOUND ( 'NONE', #12032, .T. ) ;
#12807 = CARTESIAN_POINT ( 'NONE',  ( 5.979278404433885363, 9.486416045811226994, -0.5818371488247532364 ) ) ;
#12808 = ADVANCED_FACE ( 'NONE', ( #110556 ), #142520, .F. ) ;
#12809 = LINE ( 'NONE', #79571, #50711 ) ;
#12810 = EDGE_CURVE ( 'NONE', #54347, #111783, #26266, .T. ) ;
#12811 = CARTESIAN_POINT ( 'NONE',  ( 32.99451991528749062, 28.92564299267960948, 4.000000000000000000 ) ) ;
#12812 = CARTESIAN_POINT ( 'NONE',  ( 41.99451991528749062, 28.92564299267967343, 4.000000000000000000 ) ) ;
#12813 = CARTESIAN_POINT ( 'NONE',  ( -54.48921356237310221, -27.52281430457093236, 5.000000000000000000 ) ) ;
#12814 = FACE_OUTER_BOUND ( 'NONE', #138041, .T. ) ;
#12815 = ORIENTED_EDGE ( 'NONE', *, *, #115188, .T. ) ;
#12816 = ORIENTED_EDGE ( 'NONE', *, *, #43085, .T. ) ;
#12817 = DIRECTION ( 'NONE',  ( -0.7071067811865486830, -0.7071067811865464625, 0.000000000000000000 ) ) ;
#12819 = ORIENTED_EDGE ( 'NONE', *, *, #66799, .T. ) ;
#12818 = CARTESIAN_POINT ( 'NONE',  ( -34.42500000000001137, 14.97718569542927014, 5.000000000000000000 ) ) ;
#12820 = EDGE_CURVE ( 'NONE', #39673, #116876, #109871, .T. ) ;
#12821 = FILL_AREA_STYLE ('',( #133220 ) ) ;
#12822 = CARTESIAN_POINT ( 'NONE',  ( -15.18398860626900237, 28.73617430169797871, 5.000000000000000000 ) ) ;
#12823 = ORIENTED_EDGE ( 'NONE', *, *, #36228, .T. ) ;
#12824 = EDGE_LOOP ( 'NONE', ( #52031, #20705, #9922, #6358, #36111 ) ) ;
#12825 = CARTESIAN_POINT ( 'NONE',  ( 34.92499999999998295, 22.22500000000000142, 0.4999999999999995559 ) ) ;
#12826 = ORIENTED_EDGE ( 'NONE', *, *, #61486, .F. ) ;
#12827 = CARTESIAN_POINT ( 'NONE',  ( -2.292893218813438772, 2.259292476615690770, 5.000000000000000000 ) ) ;
#12828 = CARTESIAN_POINT ( 'NONE',  ( 103.1833603837962130, -2.130196079827426203, 7.949999999999997513 ) ) ;
#12829 = LINE ( 'NONE', #101285, #127350 ) ;
#12830 = LINE ( 'NONE', #80280, #45959 ) ;
#12831 = ORIENTED_EDGE ( 'NONE', *, *, #105191, .F. ) ;
#12832 = DIRECTION ( 'NONE',  ( 0.000000000000000000, 0.000000000000000000, -1.000000000000000000 ) ) ;
#12833 = FACE_OUTER_BOUND ( 'NONE', #139729, .T. ) ;
#12834 = CARTESIAN_POINT ( 'NONE',  ( 15.48921356237309510, -27.52281430457066236, 5.000000000000000000 ) ) ;
#12835 = CARTESIAN_POINT ( 'NONE',  ( 12.68750000000000178, 4.461849672132297329, -4.461849672132302658 ) ) ;
#12836 = DIRECTION ( 'NONE',  ( -1.000000000000000000, -1.224606353822377258E-16, -0.000000000000000000 ) ) ;
#12837 = CARTESIAN_POINT ( 'NONE',  ( 14.70025512860841133, -27.71228299555195917, 4.000000000000000000 ) ) ;
#12838 = DIRECTION ( 'NONE',  ( -0.7071067811865487940, 0.7071067811865463515, -0.000000000000000000 ) ) ;
#12839 = ORIENTED_EDGE ( 'NONE', *, *, #42869, .F. ) ;
#12840 = ORIENTED_EDGE ( 'NONE', *, *, #13550, .F. ) ;
#12841 = LINE ( 'NONE', #46241, #16700 ) ;
#12842 = ORIENTED_EDGE ( 'NONE', *, *, #27836, .T. ) ;
#12843 = CARTESIAN_POINT ( 'NONE',  ( 92.75043019189810423, 3.055000000000002824, -5.291415217122919401 ) ) ;
#12844 = PLANE ( 'NONE',  #126671 ) ;
#12845 = CARTESIAN_POINT ( 'NONE',  ( 7.930039745135869289, -0.7407075233842770334, 13.87443053587609398 ) ) ;
#12846 = ADVANCED_FACE ( 'NONE', ( #32325 ), #44665, .F. ) ;
#12847 = CARTESIAN_POINT ( 'NONE',  ( 12.48921356237309155, -27.52281430457064104, 5.000000000000000000 ) ) ;
#12848 = CARTESIAN_POINT ( 'NONE',  ( 125.3761450143287846, -47.18881911353553704, -35.55177538329112963 ) ) ;
#12849 = ORIENTED_EDGE ( 'NONE', *, *, #98349, .F. ) ;
#12850 = PLANE ( 'NONE',  #17339 ) ;
#12851 = DIRECTION ( 'NONE',  ( 0.7071067811865487940, 0.7071067811865463515, 0.000000000000000000 ) ) ;
#12852 = DIRECTION ( 'NONE',  ( 0.7071067811865487940, 0.7071067811865463515, 0.000000000000000000 ) ) ;
#12853 = ORIENTED_EDGE ( 'NONE', *, *, #13618, .T. ) ;
#12854 = DIRECTION ( 'NONE',  ( -0.6830127018922181881, 0.6830127018922202975, -0.2588190451025214056 ) ) ;
#12855 =( NAMED_UNIT ( * ) PLANE_ANGLE_UNIT ( ) SI_UNIT ( $, .RADIAN. ) );
#12857 = EDGE_LOOP ( 'NONE', ( #60370, #5641, #119389 ) ) ;
#12856 = DIRECTION ( 'NONE',  ( -0.6830127018922180770, -0.6830127018922204085, -0.2588190451025213501 ) ) ;
#12858 = DIRECTION ( 'NONE',  ( 0.7071067811865487940, 0.7071067811865463515, -0.000000000000000000 ) ) ;
#12859 = DIRECTION ( 'NONE',  ( 1.000000000000000000, 0.000000000000000000, 0.000000000000000000 ) ) ;
#12860 = PLANE ( 'NONE',  #24824 ) ;
#12861 = CARTESIAN_POINT ( 'NONE',  ( 34.42499999999998295, -7.458600742197882383, 5.000000000000000000 ) ) ;
#12862 = ORIENTED_EDGE ( 'NONE', *, *, #122342, .T. ) ;
#12863 = AXIS2_PLACEMENT_3D ( 'NONE', #108239, #21279, #42339 ) ;
#12864 = VERTEX_POINT ( 'NONE', #54798 ) ;
#12865 = ORIENTED_EDGE ( 'NONE', *, *, #1610, .F. ) ;
#12866 = EDGE_CURVE ( 'NONE', #53228, #8502, #98977, .T. ) ;
#12867 = CARTESIAN_POINT ( 'NONE',  ( 86.04209685856477563, 5.291415217122923842, -3.054999999999996163 ) ) ;
#12868 =( BOUNDED_CURVE ( )  B_SPLINE_CURVE ( 2, ( #126933, #38522, #39247, #4386, #116065, #48687, #83460, #6545, #51551, #107333, #87733, #74007, #141393 ),
 .UNSPECIFIED., .F., .T. ) 
 B_SPLINE_CURVE_WITH_KNOTS ( ( 3, 2, 2, 2, 2, 2, 3 ),
 ( 0.05711758424084519004, 0.05833333333333333426, 0.06666666666666666574, 0.07500000000000001110, 0.08333333333333334259, 0.09166666666666667407, 0.1000000000000000333 ),
 .UNSPECIFIED. ) 
 CURVE ( )  GEOMETRIC_REPRESENTATION_ITEM ( )  RATIONAL_B_SPLINE_CURVE ( ( 0.9915083049239661328, 0.9950289225080382050, 1.000000000000000000, 0.9659258262890683122, 1.000000000000000000, 0.9659258262890683122, 1.000000000000000000, 0.9659258262890683122, 1.000000000000000000, 0.9659258262890683122, 1.000000000000000000, 0.9659258262890682012, 1.000000000000000222 ) ) 
 REPRESENTATION_ITEM ( '' )  );
#12869 = ORIENTED_EDGE ( 'NONE', *, *, #56631, .F. ) ;
#12870 = EDGE_CURVE ( 'NONE', #86631, #69033, #111279, .T. ) ;
#12871 = EDGE_CURVE ( 'NONE', #120303, #117585, #25528, .T. ) ;
#12872 = VECTOR ( 'NONE', #64986, 999.9999999999998863 ) ;
#12873 = CARTESIAN_POINT ( 'NONE',  ( 14.67183060077637968, -3.740707523384234623, 4.000000000000000000 ) ) ;
#12874 = CARTESIAN_POINT ( 'NONE',  ( -34.75611968250420603, 10.70565069852396434, 4.955485411084901592 ) ) ;
#12875 = EDGE_CURVE ( 'NONE', #84298, #41034, #77973, .T. ) ;
#12876 = PLANE ( 'NONE',  #117407 ) ;
#12877 = CARTESIAN_POINT ( 'NONE',  ( -12.20000000000000284, -25.47159979880235881, 14.98806839329795260 ) ) ;
#12878 = ORIENTED_EDGE ( 'NONE', *, *, #44624, .T. ) ;
#12879 = EDGE_CURVE ( 'NONE', #101519, #117394, #91526, .T. ) ;
#12880 = CARTESIAN_POINT ( 'NONE',  ( 33.29974487139158867, -27.71228299555229313, 4.000000000000000000 ) ) ;
#12881 = LINE ( 'NONE', #58609, #85947 ) ;
#12882 = LINE ( 'NONE', #112231, #83484 ) ;
#12883 = CARTESIAN_POINT ( 'NONE',  ( 83.32876352523143737, 0.000000000000000000, -6.109999999999998543 ) ) ;
#12884 = AXIS2_PLACEMENT_3D ( 'NONE', #42490, #97539, #86694 ) ;
#12885 = VERTEX_POINT ( 'NONE', #113977 ) ;
#12886 = EDGE_CURVE ( 'NONE', #71177, #23274, #58950, .T. ) ;
#12887 = DIRECTION ( 'NONE',  ( -0.7071067811865487940, 0.7071067811865463515, -0.000000000000000000 ) ) ;
#12888 = CARTESIAN_POINT ( 'NONE',  ( -32.20710678118632586, 3.759292476615683665, 5.000000000000000000 ) ) ;
#12889 = VERTEX_POINT ( 'NONE', #84918 ) ;
#12890 = ORIENTED_EDGE ( 'NONE', *, *, #22191, .T. ) ;
#12891 = EDGE_CURVE ( 'NONE', #96290, #138539, #18192, .T. ) ;
#12892 = CARTESIAN_POINT ( 'NONE',  ( 34.42499999999998295, 17.97718569542920619, 5.000000000000000000 ) ) ;
#12893 = EDGE_CURVE ( 'NONE', #28113, #15358, #37872, .T. ) ;
#12894 = CARTESIAN_POINT ( 'NONE',  ( 15.18398860626900237, 28.73617430169797871, 5.000000000000000000 ) ) ;
#12895 = DIRECTION ( 'NONE',  ( -0.000000000000000000, -0.3543493200069152693, 0.9351131265310292928 ) ) ;
#12896 = EDGE_CURVE ( 'NONE', #97018, #92519, #103785, .T. ) ;
#12897 = VECTOR ( 'NONE', #8386, 999.9999999999998863 ) ;
#12898 = FACE_OUTER_BOUND ( 'NONE', #117350, .T. ) ;
#12899 = PLANE ( 'NONE',  #68232 ) ;
#12900 = VECTOR ( 'NONE', #127163, 1000.000000000000000 ) ;
#12901 = EDGE_LOOP ( 'NONE', ( #92474, #12819, #46608, #129177, #95457, #52290 ) ) ;
#12903 = ORIENTED_EDGE ( 'NONE', *, *, #75289, .F. ) ;
#12902 = VECTOR ( 'NONE', #90135, 999.9999999999998863 ) ;
#12904 = PLANE ( 'NONE',  #122065 ) ;
#12905 = VERTEX_POINT ( 'NONE', #48735 ) ;
#12906 = EDGE_LOOP ( 'NONE', ( #139796, #39332, #78702, #45739, #74020, #104729 ) ) ;
#12907 = EDGE_CURVE ( 'NONE', #110525, #119001, #26963, .T. ) ;
#12908 = STYLED_ITEM ( 'NONE', ( #125167 ), #133441 ) ;
#12909 = DIRECTION ( 'NONE',  ( 0.000000000000000000, -1.000000000000000000, 0.000000000000000000 ) ) ;
#12910 = EDGE_LOOP ( 'NONE', ( #6892, #25467, #78587 ) ) ;
#12911 = DIRECTION ( 'NONE',  ( 0.7071067811865486830, -0.7071067811865464625, -0.000000000000000000 ) ) ;
#12912 = DIRECTION ( 'NONE',  ( -1.000000000000000000, -0.000000000000000000, -0.000000000000000000 ) ) ;
#12913 = CYLINDRICAL_SURFACE ( 'NONE', #13256, 0.5000000000000004441 ) ;
#12914 = ADVANCED_FACE ( 'NONE', ( #116831 ), #114674, .F. ) ;
#12915 = DIRECTION ( 'NONE',  ( -0.000000000000000000, 0.000000000000000000, 1.000000000000000000 ) ) ;
#12916 = DIRECTION ( 'NONE',  ( -0.3543493200069162685, -0.000000000000000000, -0.9351131265310288487 ) ) ;
#12917 = ORIENTED_EDGE ( 'NONE', *, *, #31591, .T. ) ;
#12918 = LINE ( 'NONE', #45603, #127425 ) ;
#12919 = EDGE_LOOP ( 'NONE', ( #90702, #37490, #129900, #95507 ) ) ;
#12920 = DIRECTION ( 'NONE',  ( 0.6830127018922181881, 0.6830127018922202975, -0.2588190451025214056 ) ) ;
#12921 = ORIENTED_EDGE ( 'NONE', *, *, #46847, .T. ) ;
#12922 = LINE ( 'NONE', #123869, #120902 ) ;
#12923 = ORIENTED_EDGE ( 'NONE', *, *, #14943, .T. ) ;
#12924 = DIRECTION ( 'NONE',  ( 0.7071067811865486830, -0.7071067811865464625, -0.000000000000000000 ) ) ;
#12925 = ORIENTED_EDGE ( 'NONE', *, *, #126330, .T. ) ;
#12926 = EDGE_CURVE ( 'NONE', #113088, #55705, #82796, .T. ) ;
#12927 = ORIENTED_EDGE ( 'NONE', *, *, #72659, .T. ) ;
#12928 = ORIENTED_EDGE ( 'NONE', *, *, #72173, .T. ) ;
#12929 = ADVANCED_FACE ( 'NONE', ( #94358 ), #138598, .T. ) ;
#12930 = PRESENTATION_STYLE_ASSIGNMENT (( #71629 ) ) ;
#12931 = DIRECTION ( 'NONE',  ( 0.000000000000000000, -1.000000000000000000, 0.000000000000000000 ) ) ;
#12932 = CARTESIAN_POINT ( 'NONE',  ( 25.17183060077629975, 0.7592924766157207461, 4.000000000000000000 ) ) ;
#12933 = CARTESIAN_POINT ( 'NONE',  ( 113.8962635252314186, 4.472830434245840259, -4.472830434245838482 ) ) ;
#12934 = DIRECTION ( 'NONE',  ( 0.6830127018922181881, 0.6830127018922202975, -0.2588190451025214056 ) ) ;
#12935 = EDGE_CURVE ( 'NONE', #18415, #100098, #73351, .T. ) ;
#12936 = CARTESIAN_POINT ( 'NONE',  ( -28.80981832425534606, -18.74070752338408852, 7.910009926591575535 ) ) ;
#12937 = PLANE ( 'NONE',  #65236 ) ;
#12938 = DIRECTION ( 'NONE',  ( 1.000000000000000000, 0.000000000000000000, 0.000000000000000000 ) ) ;
#12939 = LINE ( 'NONE', #33334, #13523 ) ;
#12940 = EDGE_LOOP ( 'NONE', ( #59977, #108801, #34420, #38257 ) ) ;
#12941 = DIRECTION ( 'NONE',  ( -0.6830127018922181881, 0.6830127018922202975, -0.2588190451025214056 ) ) ;
#12942 = CARTESIAN_POINT ( 'NONE',  ( -63.29974487139158867, -27.71228299555250274, 4.000000000000000000 ) ) ;
#12943 = PLANE ( 'NONE',  #65703 ) ;
#12944 = ADVANCED_FACE ( 'NONE', ( #137170 ), #28408, .F. ) ;
#12945 = EDGE_LOOP ( 'NONE', ( #33299, #64789, #106945, #134076, #99145, #7889 ) ) ;
#12946 = ORIENTED_EDGE ( 'NONE', *, *, #143524, .F. ) ;
#12947 = CARTESIAN_POINT ( 'NONE',  ( 23.32000000000000028, 2.055000000000001492, 0.000000000000000000 ) ) ;
#12948 = ORIENTED_EDGE ( 'NONE', *, *, #142978, .T. ) ;
#12949 = LINE ( 'NONE', #1353, #14361 ) ;
#12950 = CARTESIAN_POINT ( 'NONE',  ( 15.06663961620376924, 1.633150327867695095, 6.094999999999988205 ) ) ;
#12951 = CARTESIAN_POINT ( 'NONE',  ( -26.99451991528749417, 28.92564299267956685, 4.000000000000000000 ) ) ;
#12952 = EDGE_CURVE ( 'NONE', #138262, #6023, #104522, .T. ) ;
#12953 = CARTESIAN_POINT ( 'NONE',  ( -11.99999999999992006, -1.068876922607800761, 4.000000000000000000 ) ) ;
#12954 = CARTESIAN_POINT ( 'NONE',  ( -14.18753812416042770, -22.22500000000000142, 4.000000000000000000 ) ) ;
#12955 = EDGE_CURVE ( 'NONE', #121709, #68092, #60339, .T. ) ;
#12956 = ORIENTED_EDGE ( 'NONE', *, *, #84508, .F. ) ;
#12957 = PLANE ( 'NONE',  #51051 ) ;
#12958 = ORIENTED_EDGE ( 'NONE', *, *, #81534, .F. ) ;
#12959 = CARTESIAN_POINT ( 'NONE',  ( -14.99999999999989519, -21.84840872380826227, 2.849755605029573591 ) ) ;
#12960 = VECTOR ( 'NONE', #128311, 1000.000000000000000 ) ;
#12961 = CARTESIAN_POINT ( 'NONE',  ( 20.92123647476855197, -9.717572351234235426E-16, -7.934999999999990727 ) ) ;
#12962 = EDGE_LOOP ( 'NONE', ( #128129, #75582, #104105, #15694 ) ) ;
#12963 = CARTESIAN_POINT ( 'NONE',  ( 80.70376352523145158, 6.109999999999999432, 1.122388791418549108E-15 ) ) ;
#12964 = DIRECTION ( 'NONE',  ( 0.000000000000000000, 0.000000000000000000, -1.000000000000000000 ) ) ;
#12965 = VECTOR ( 'NONE', #94903, 1000.000000000000000 ) ;
#12966 = FACE_OUTER_BOUND ( 'NONE', #54057, .T. ) ;
#12967 = EDGE_CURVE ( 'NONE', #31893, #57582, #5179, .T. ) ;
#12968 = ORIENTED_EDGE ( 'NONE', *, *, #31406, .F. ) ;
#12969 = VERTEX_POINT ( 'NONE', #49476 ) ;
#12970 = ORIENTED_EDGE ( 'NONE', *, *, #112715, .T. ) ;
#12971 = CARTESIAN_POINT ( 'NONE',  ( -8.700255128608413102, -27.71228299555199825, 4.000000000000000000 ) ) ;
#12972 = CARTESIAN_POINT ( 'NONE',  ( -65.99451991528749772, 28.92564299267984396, 4.000000000000000000 ) ) ;
#12973 = DIRECTION ( 'NONE',  ( 0.7071067811865487940, -0.7071067811865463515, 0.000000000000000000 ) ) ;
#12974 = PLANE ( 'NONE',  #121342 ) ;
#12975 = ORIENTED_EDGE ( 'NONE', *, *, #74363, .T. ) ;
#12976 = EDGE_CURVE ( 'NONE', #68408, #93537, #93666, .T. ) ;
#12977 = AXIS2_PLACEMENT_3D ( 'NONE', #112007, #56925, #80108 ) ;
#12978 = FILL_AREA_STYLE ('',( #99264 ) ) ;
#12979 = FACE_OUTER_BOUND ( 'NONE', #2426, .T. ) ;
#12980 = ORIENTED_EDGE ( 'NONE', *, *, #11098, .F. ) ;
#12981 = LINE ( 'NONE', #47124, #53982 ) ;
#12982 = VERTEX_POINT ( 'NONE', #38564 ) ;
#12983 = EDGE_CURVE ( 'NONE', #21557, #8470, #7331, .T. ) ;
#12985 = ORIENTED_EDGE ( 'NONE', *, *, #10702, .F. ) ;
#12984 = CARTESIAN_POINT ( 'NONE',  ( 58.54058136200957563, -46.07581969935342414, -35.63601533997326243 ) ) ;
#12986 = VECTOR ( 'NONE', #96143, 1000.000000000000000 ) ;
#12987 = VERTEX_POINT ( 'NONE', #116107 ) ;
#12988 = EDGE_CURVE ( 'NONE', #98697, #20563, #119616, .T. ) ;
#12989 = CARTESIAN_POINT ( 'NONE',  ( 60.29974487139158867, -27.71228299555248142, 4.000000000000000000 ) ) ;
#12990 = CARTESIAN_POINT ( 'NONE',  ( 7.499999999999952927, 0.4311230773921831960, 4.000000000000000000 ) ) ;
#12991 = VERTEX_POINT ( 'NONE', #16804 ) ;
#12992 = DIRECTION ( 'NONE',  ( -0.7071067811865486830, -0.7071067811865464625, 0.000000000000000000 ) ) ;
#12993 = UNCERTAINTY_MEASURE_WITH_UNIT (LENGTH_MEASURE( 1.000000000000000082E-05 ), #36176, 'distance_accuracy_value', 'NONE');
#12994 = ORIENTED_EDGE ( 'NONE', *, *, #24543, .T. ) ;
#12995 = CIRCLE ( 'NONE', #94032, 2.500000000000000444 ) ;
#12996 = AXIS2_PLACEMENT_3D ( 'NONE', #140908, #72871, #85820 ) ;
#12997 = LINE ( 'NONE', #101447, #36003 ) ;
#12998 = CARTESIAN_POINT ( 'NONE',  ( 23.00840764549667483, 9.139736423841732040E-16, 0.000000000000000000 ) ) ;
#12999 = AXIS2_PLACEMENT_3D ( 'NONE', #28918, #4975, #28210 ) ;
#13000 = CARTESIAN_POINT ( 'NONE',  ( -20.99999999999985079, -15.41253812416059787, 4.000000000000000000 ) ) ;
#13001 = CARTESIAN_POINT ( 'NONE',  ( 47.32919371712955581, -3.975000000000001865, 6.884901960086284411 ) ) ;
#13003 = AXIS2_PLACEMENT_3D ( 'NONE', #138407, #15858, #49984 ) ;
#13002 = FACE_OUTER_BOUND ( 'NONE', #32844, .T. ) ;
#13004 = DIRECTION ( 'NONE',  ( 0.000000000000000000, -1.000000000000000000, 0.000000000000000000 ) ) ;
#13005 = LINE ( 'NONE', #36222, #72664 ) ;
#13006 = CARTESIAN_POINT ( 'NONE',  ( 57.48921356237308800, -27.52281430457095368, 5.000000000000000000 ) ) ;
#13007 = CARTESIAN_POINT ( 'NONE',  ( 23.02040314143522082, 7.934999999999989839, -2.126176841940961904 ) ) ;
#13008 = DIRECTION ( 'NONE',  ( 0.7071067811865487940, 0.7071067811865463515, -0.000000000000000000 ) ) ;
#13009 = CYLINDRICAL_SURFACE ( 'NONE', #119997, 7.950000000000000178 ) ;
#13010 = VECTOR ( 'NONE', #125371, 1000.000000000000227 ) ;
#13011 = CARTESIAN_POINT ( 'NONE',  ( -0.4892135623730947680, -27.52281430457055578, 5.000000000000000000 ) ) ;
#13012 = DIRECTION ( 'NONE',  ( 0.000000000000000000, 0.000000000000000000, 1.000000000000000000 ) ) ;
#13013 = ORIENTED_EDGE ( 'NONE', *, *, #109605, .T. ) ;
#13014 = EDGE_CURVE ( 'NONE', #57955, #99416, #61083, .T. ) ;
#13015 = VERTEX_POINT ( 'NONE', #83513 ) ;
#13016 = CARTESIAN_POINT ( 'NONE',  ( 89.52083333333332860, 7.949999999999999289, 2.130196079827431532 ) ) ;
#13017 = ORIENTED_EDGE ( 'NONE', *, *, #58467, .T. ) ;
#13018 = ORIENTED_EDGE ( 'NONE', *, *, #45142, .T. ) ;
#13019 = VERTEX_POINT ( 'NONE', #127728 ) ;
#13020 = DIRECTION ( 'NONE',  ( 0.7071067811865486830, -0.7071067811865464625, -0.000000000000000000 ) ) ;
#13021 = CARTESIAN_POINT ( 'NONE',  ( 42.18398860626899705, 28.73617430169816700, 5.000000000000000000 ) ) ;
#13022 = DIRECTION ( 'NONE',  ( 1.000000000000000000, 0.000000000000000000, 0.000000000000000000 ) ) ;
#13023 = EDGE_LOOP ( 'NONE', ( #4793, #26703, #60983, #43694 ) ) ;
#13024 = CARTESIAN_POINT ( 'NONE',  ( 27.00000000000000355, 0.000000000000000000, 0.000000000000000000 ) ) ;
#13025 = CARTESIAN_POINT ( 'NONE',  ( 7.499999999999948486, -16.91253812416058011, 4.000000000000000000 ) ) ;
#13026 = FACE_OUTER_BOUND ( 'NONE', #111403, .T. ) ;
#13027 = FACE_OUTER_BOUND ( 'NONE', #59108, .T. ) ;
#13028 = VERTEX_POINT ( 'NONE', #55158 ) ;
#13029 = CARTESIAN_POINT ( 'NONE',  ( -14.51078643762690490, -27.52281430457045275, 5.000000000000000000 ) ) ;
#13030 = CARTESIAN_POINT ( 'NONE',  ( -25.49999999999981881, 3.431123077392149501, 4.000000000000000000 ) ) ;
#13031 = ADVANCED_FACE ( 'NONE', ( #76194 ), #9461, .T. ) ;
#13032 = CARTESIAN_POINT ( 'NONE',  ( 27.00000000000004974, 3.781023723404877579, 6.868722978355127573 ) ) ;
#13033 = DIRECTION ( 'NONE',  ( 0.7071067811865487940, 0.7071067811865463515, 0.000000000000000000 ) ) ;
#13034 = LINE ( 'NONE', #90638, #96294 ) ;
#13035 = LINE ( 'NONE', #44287, #36020 ) ;
#13036 = CARTESIAN_POINT ( 'NONE',  ( 11.93159235450332112, 9.902892378096218942E-16, 0.000000000000000000 ) ) ;
#13037 = EDGE_CURVE ( 'NONE', #119486, #81792, #74047, .T. ) ;
#13038 = ORIENTED_EDGE ( 'NONE', *, *, #80551, .T. ) ;
#13039 = EDGE_LOOP ( 'NONE', ( #113514, #23393, #107616, #139517, #29659 ) ) ;
#13040 = EDGE_CURVE ( 'NONE', #56501, #66484, #105750, .T. ) ;
#13041 = CARTESIAN_POINT ( 'NONE',  ( 124.2504301918981184, 3.055000000000002824, -5.291415217122919401 ) ) ;
#13042 = VERTEX_POINT ( 'NONE', #132743 ) ;
#13043 = EDGE_CURVE ( 'NONE', #92202, #114427, #43555, .T. ) ;
#13044 = LINE ( 'NONE', #47188, #77965 ) ;
#13045 = AXIS2_PLACEMENT_3D ( 'NONE', #51941, #129472, #62827 ) ;
#13046 = LINE ( 'NONE', #14495, #124468 ) ;
#13047 = EDGE_CURVE ( 'NONE', #26531, #118332, #42153, .T. ) ;
#13048 = EDGE_CURVE ( 'NONE', #75885, #13822, #64596, .T. ) ;
#13049 = CARTESIAN_POINT ( 'NONE',  ( -11.81601139373100651, 28.73617430169779041, 5.000000000000000000 ) ) ;
#13050 = CYLINDRICAL_SURFACE ( 'NONE', #99807, 2.500000000000000000 ) ;
#13051 = CARTESIAN_POINT ( 'NONE',  ( 114.9745968585647660, 1.637169565754164058, -6.109999999999996767 ) ) ;
#13052 = EDGE_LOOP ( 'NONE', ( #26514, #60550, #59326, #131306 ) ) ;
#13053 = ORIENTED_EDGE ( 'NONE', *, *, #80612, .T. ) ;
#13054 = VECTOR ( 'NONE', #33036, 999.9999999999998863 ) ;
#13055 = CARTESIAN_POINT ( 'NONE',  ( -24.48921356237309510, -27.52281430457072631, 5.000000000000000000 ) ) ;
#13056 = VERTEX_POINT ( 'NONE', #118965 ) ;
#13057 = VERTEX_POINT ( 'NONE', #119653 ) ;
#13058 = EDGE_CURVE ( 'NONE', #143372, #99698, #97940, .T. ) ;
#13059 = ORIENTED_EDGE ( 'NONE', *, *, #44627, .T. ) ;
#13060 = CARTESIAN_POINT ( 'NONE',  ( 0.000000000000000000, 0.000000000000000000, 5.000000000000000000 ) ) ;
#13061 = EDGE_CURVE ( 'NONE', #72010, #58791, #52982, .T. ) ;
#13062 = CARTESIAN_POINT ( 'NONE',  ( 2.837903141435219379, -6.871911579029513106, -3.967499999999993587 ) ) ;
#13063 = EDGE_CURVE ( 'NONE', #140203, #78331, #97176, .T. ) ;
#13064 = VECTOR ( 'NONE', #142412, 1000.000000000000000 ) ;
#13065 = DIRECTION ( 'NONE',  ( 0.7071067811865486830, -0.7071067811865464625, -0.000000000000000000 ) ) ;
#13066 = ORIENTED_EDGE ( 'NONE', *, *, #28168, .T. ) ;
#13067 = AXIS2_PLACEMENT_3D ( 'NONE', #75870, #120032, #51978 ) ;
#13068 = ORIENTED_EDGE ( 'NONE', *, *, #54836, .T. ) ;
#13069 = LINE ( 'NONE', #114536, #131191 ) ;
#13070 = ORIENTED_EDGE ( 'NONE', *, *, #91129, .F. ) ;
#13071 = ORIENTED_EDGE ( 'NONE', *, *, #19603, .F. ) ;
#13072 = EDGE_CURVE ( 'NONE', #50807, #72701, #103375, .T. ) ;
#13073 = VERTEX_POINT ( 'NONE', #65343 ) ;
#13074 = DIRECTION ( 'NONE',  ( -1.000000000000000000, -0.000000000000000000, -0.000000000000000000 ) ) ;
#13075 = PRESENTATION_STYLE_ASSIGNMENT (( #32733 ) ) ;
#13076 = DIRECTION ( 'NONE',  ( -1.000000000000000000, -0.000000000000000000, -0.000000000000000000 ) ) ;
#13077 = ORIENTED_EDGE ( 'NONE', *, *, #123429, .T. ) ;
#13078 = DIRECTION ( 'NONE',  ( -0.000000000000000000, 0.000000000000000000, 1.000000000000000000 ) ) ;
#13079 = LINE ( 'NONE', #47907, #126577 ) ;
#13080 = ADVANCED_FACE ( 'NONE', ( #87064 ), #63897, .F. ) ;
#13081 = PRESENTATION_STYLE_ASSIGNMENT (( #100126 ) ) ;
#13082 = FACE_BOUND ( 'NONE', #36726, .T. ) ;
#13083 = ORIENTED_EDGE ( 'NONE', *, *, #863, .F. ) ;
#13084 = DIRECTION ( 'NONE',  ( 0.000000000000000000, 0.000000000000000000, -1.000000000000000000 ) ) ;
#13085 = CARTESIAN_POINT ( 'NONE',  ( 0.000000000000000000, 0.000000000000000000, 5.000000000000000000 ) ) ;
#13086 = FACE_OUTER_BOUND ( 'NONE', #140068, .T. ) ;
#13087 = DIRECTION ( 'NONE',  ( -0.6830127018922181881, 0.6830127018922202975, -0.2588190451025214056 ) ) ;
#13088 = ORIENTED_EDGE ( 'NONE', *, *, #96736, .F. ) ;
#13089 = EDGE_CURVE ( 'NONE', #19080, #112760, #31967, .T. ) ;
#13090 = CARTESIAN_POINT ( 'NONE',  ( -3.299744871391591339, -27.71228299555208352, 4.000000000000000000 ) ) ;
#13091 = ORIENTED_EDGE ( 'NONE', *, *, #120157, .T. ) ;
#13092 = EDGE_CURVE ( 'NONE', #74639, #46818, #10891, .T. ) ;
#13093 = ORIENTED_EDGE ( 'NONE', *, *, #34640, .T. ) ;
#13094 = CONICAL_SURFACE ( 'NONE', #75638, 8.094999999999991758, 0.7853981633974466137 ) ;
#13095 = VERTEX_POINT ( 'NONE', #99336 ) ;
#13096 = CIRCLE ( 'NONE', #43254, 2.500000000000000888 ) ;
#13097 = ADVANCED_FACE ( 'NONE', ( #8047 ), #107378, .T. ) ;
#13098 = AXIS2_PLACEMENT_3D ( 'NONE', #86873, #85410, #65139 ) ;
#13099 = CARTESIAN_POINT ( 'NONE',  ( 51.39126352523145158, -4.472830434245838482, -4.472830434245838482 ) ) ;
#13100 = VERTEX_POINT ( 'NONE', #132008 ) ;
#13101 = VECTOR ( 'NONE', #103383, 1000.000000000000227 ) ;
#13102 = FACE_OUTER_BOUND ( 'NONE', #16725, .T. ) ;
#13103 = DIRECTION ( 'NONE',  ( 0.3543493200069162685, -0.000000000000000000, -0.9351131265310288487 ) ) ;
#13104 = EDGE_LOOP ( 'NONE', ( #126659, #13650, #10805, #107861, #22527 ) ) ;
#13105 = CARTESIAN_POINT ( 'NONE',  ( 34.92499999999998295, -4.298069433178973497, 4.500000000000000888 ) ) ;
#13106 = LINE ( 'NONE', #13808, #57468 ) ;
#13107 = AXIS2_PLACEMENT_3D ( 'NONE', #29598, #73836, #118010 ) ;
#13108 = CARTESIAN_POINT ( 'NONE',  ( 57.48921356237308800, -27.52281430457095368, 5.000000000000000000 ) ) ;
#13109 = DIRECTION ( 'NONE',  ( -0.000000000000000000, 0.3543493200069153248, 0.9351131265310292928 ) ) ;
#13110 = SURFACE_STYLE_FILL_AREA ( #103004 ) ;
#13111 = FACE_OUTER_BOUND ( 'NONE', #70720, .T. ) ;
#13112 = ORIENTED_EDGE ( 'NONE', *, *, #9743, .T. ) ;
#13113 = ORIENTED_EDGE ( 'NONE', *, *, #104923, .T. ) ;
#13114 = ORIENTED_EDGE ( 'NONE', *, *, #90415, .F. ) ;
#13115 = ORIENTED_EDGE ( 'NONE', *, *, #134671, .F. ) ;
#13116 = CARTESIAN_POINT ( 'NONE',  ( -13.49999999999990408, -11.56887692260769995, 4.000000000000000000 ) ) ;
#13117 = VERTEX_POINT ( 'NONE', #44295 ) ;
#13118 = ORIENTED_EDGE ( 'NONE', *, *, #126761, .T. ) ;
#13119 = CARTESIAN_POINT ( 'NONE',  ( 160.4291323974385080, 26.96999999999993847, -34.92499999999998295 ) ) ;
#13120 = DIRECTION ( 'NONE',  ( 0.7071067811865486830, -0.7071067811865464625, -0.000000000000000000 ) ) ;
#13121 = ORIENTED_EDGE ( 'NONE', *, *, #126924, .T. ) ;
#13122 = DIRECTION ( 'NONE',  ( -1.000000000000000000, -1.224606353822377258E-16, -0.000000000000000000 ) ) ;
#13123 = LINE ( 'NONE', #90737, #56066 ) ;
#13124 = CARTESIAN_POINT ( 'NONE',  ( 26.02540314143521982, 2.126176841940962348, 7.934999999999989839 ) ) ;
#13125 = AXIS2_PLACEMENT_3D ( 'NONE', #46365, #123899, #24556 ) ;
#13126 = LINE ( 'NONE', #1527, #29891 ) ;
#13127 = ORIENTED_EDGE ( 'NONE', *, *, #48184, .T. ) ;
#13129 = DIRECTION ( 'NONE',  ( 0.7071067811865487940, 0.7071067811865463515, -0.000000000000000000 ) ) ;
#13128 = CARTESIAN_POINT ( 'NONE',  ( 114.5370968585647802, -3.054999999999999272, -5.291415217122919401 ) ) ;
#13130 = CARTESIAN_POINT ( 'NONE',  ( 26.99999999999981881, 14.96639925780211122, 5.000000000000000000 ) ) ;
#13131 = CARTESIAN_POINT ( 'NONE',  ( 12.51665438641036054, 22.22500000000000142, 4.500000000000000888 ) ) ;
#13132 = ORIENTED_EDGE ( 'NONE', *, *, #116955, .T. ) ;
#13133 = DIRECTION ( 'NONE',  ( -0.000000000000000000, -0.000000000000000000, 1.000000000000000000 ) ) ;
#13135 = ORIENTED_EDGE ( 'NONE', *, *, #23899, .F. ) ;
#13134 = LINE ( 'NONE', #834, #28650 ) ;
#13136 = VECTOR ( 'NONE', #5893, 1000.000000000000000 ) ;
#13137 = CARTESIAN_POINT ( 'NONE',  ( 2.843876922607555091, -22.22500000000000497, 4.000000000000000000 ) ) ;
#13138 = VERTEX_POINT ( 'NONE', #66052 ) ;
#13139 = FACE_OUTER_BOUND ( 'NONE', #26170, .T. ) ;
#13140 = CARTESIAN_POINT ( 'NONE',  ( 125.7224624600519718, -47.70829528212275505, -34.92499999999998295 ) ) ;
#13141 = CARTESIAN_POINT ( 'NONE',  ( -26.99999999999981171, -3.485240976185098649, -4.108735105802460374 ) ) ;
#13143 = VERTEX_POINT ( 'NONE', #129851 ) ;
#13142 =( BOUNDED_CURVE ( )  B_SPLINE_CURVE ( 2, ( #51075, #92404, #62667, #105426, #48940, #116319, #93143, #95273, #28619, #72872, #61965, #136631, #93850 ),
 .UNSPECIFIED., .F., .F. ) 
 B_SPLINE_CURVE_WITH_KNOTS ( ( 3, 2, 2, 2, 2, 2, 3 ),
 ( 0.5333333333333333259, 0.5361111111111110938, 0.5388888888888888618, 0.5416666666666666297, 0.5444444444444443976, 0.5472222222222222765, 0.5500000000000000444 ),
 .UNSPECIFIED. ) 
 CURVE ( )  GEOMETRIC_REPRESENTATION_ITEM ( )  RATIONAL_B_SPLINE_CURVE ( ( 1.000000000000000000, 0.9659258262890683122, 1.000000000000000000, 0.9659258262890683122, 1.000000000000000000, 0.9659258262890683122, 1.000000000000000000, 0.9659258262890683122, 1.000000000000000000, 0.9659258262890683122, 1.000000000000000000, 0.9659258262890683122, 1.000000000000000000 ) ) 
 REPRESENTATION_ITEM ( '' )  );
#13144 = DIRECTION ( 'NONE',  ( 1.000000000000000000, 0.000000000000000000, 0.000000000000000000 ) ) ;
#13145 = DIRECTION ( 'NONE',  ( -0.7071067811865487940, 0.7071067811865463515, -0.000000000000000000 ) ) ;
#13146 = DIRECTION ( 'NONE',  ( -0.6830127018922181881, 0.6830127018922202975, -0.2588190451025214056 ) ) ;
#13147 = AXIS2_PLACEMENT_3D ( 'NONE', #64735, #20489, #76333 ) ;
#13148 = ORIENTED_EDGE ( 'NONE', *, *, #44883, .F. ) ;
#13149 = CARTESIAN_POINT ( 'NONE',  ( -7.499999999999944045, -7.420205493532908037, -2.617629953481270366 ) ) ;
#13150 = VERTEX_POINT ( 'NONE', #41404 ) ;
#13151 = DIRECTION ( 'NONE',  ( 0.000000000000000000, 1.000000000000000000, 0.000000000000000000 ) ) ;
#13152 = EDGE_CURVE ( 'NONE', #33921, #127932, #30552, .T. ) ;
#13154 = VERTEX_POINT ( 'NONE', #74787 ) ;
#13153 = LINE ( 'NONE', #101609, #136645 ) ;
#13156 = VERTEX_POINT ( 'NONE', #100795 ) ;
#13155 = EDGE_CURVE ( 'NONE', #56699, #116635, #19658, .T. ) ;
#13157 = CARTESIAN_POINT ( 'NONE',  ( 15.56310719811854959, 7.173451295978907183, -28.42221963501224025 ) ) ;
#13158 = LINE ( 'NONE', #111036, #13505 ) ;
#13159 = ORIENTED_EDGE ( 'NONE', *, *, #87063, .T. ) ;
#13160 = DIRECTION ( 'NONE',  ( 0.3543493200069162685, -0.000000000000000000, -0.9351131265310288487 ) ) ;
#13161 = DIRECTION ( 'NONE',  ( 0.7071067811865487940, 0.7071067811865463515, 0.000000000000000000 ) ) ;
#13162 = VECTOR ( 'NONE', #56297, 1000.000000000000000 ) ;
#13163 = EDGE_LOOP ( 'NONE', ( #131900, #67205, #120225, #106376, #37906, #53500, #23601, #97238 ) ) ;
#13164 = ADVANCED_FACE ( 'NONE', ( #34839 ), #113079, .F. ) ;
#13165 = DIRECTION ( 'NONE',  ( 0.7071067811865487940, -0.7071067811865463515, 0.000000000000000000 ) ) ;
#13166 = LINE ( 'NONE', #34244, #35116 ) ;
#13167 = CARTESIAN_POINT ( 'NONE',  ( 24.29974487139158867, -27.71228299555223273, 4.000000000000000000 ) ) ;
#13168 = DIRECTION ( 'NONE',  ( -0.000000000000000000, -0.3543493200069152693, 0.9351131265310292928 ) ) ;
#13169 = PLANE ( 'NONE',  #115431 ) ;
#13170 = CARTESIAN_POINT ( 'NONE',  ( 13.49999999999990763, -16.91253812416058722, 4.000000000000000000 ) ) ;
#13171 = VERTEX_POINT ( 'NONE', #33435 ) ;
#13172 = EDGE_CURVE ( 'NONE', #7538, #34146, #77638, .T. ) ;
#13173 = VERTEX_POINT ( 'NONE', #79081 ) ;
#13174 = VERTEX_POINT ( 'NONE', #68904 ) ;
#13175 = CARTESIAN_POINT ( 'NONE',  ( -32.20710678118631876, -14.24070752338413826, 5.000000000000000000 ) ) ;
#13176 = ORIENTED_EDGE ( 'NONE', *, *, #51882, .F. ) ;
#13177 = ORIENTED_EDGE ( 'NONE', *, *, #82115, .F. ) ;
#13178 = EDGE_LOOP ( 'NONE', ( #125419, #135739, #140264, #137351, #45481, #127619 ) ) ;
#13179 = CARTESIAN_POINT ( 'NONE',  ( 1.632902354900489739, -0.3019974585920503496, -6.462097645098976884 ) ) ;
#13180 = LINE ( 'NONE', #101639, #131934 ) ;
#13181 = EDGE_CURVE ( 'NONE', #92161, #82100, #57319, .T. ) ;
#13182 = ORIENTED_EDGE ( 'NONE', *, *, #99759, .T. ) ;
#13183 = DIRECTION ( 'NONE',  ( 1.000000000000000000, 0.000000000000000000, 0.000000000000000000 ) ) ;
#13184 = FACE_OUTER_BOUND ( 'NONE', #108539, .T. ) ;
#13185 = CARTESIAN_POINT ( 'NONE',  ( 22.22840764549667725, 9.139736423841732040E-16, 0.000000000000000000 ) ) ;
#13186 = VECTOR ( 'NONE', #17361, 1000.000000000000000 ) ;
#13187 = LINE ( 'NONE', #33575, #115899 ) ;
#13188 = CARTESIAN_POINT ( 'NONE',  ( 122.3545968585647472, -1.637169565754161615, 6.110000000000000320 ) ) ;
#13189 = EDGE_LOOP ( 'NONE', ( #97611, #89483, #10773, #70595 ) ) ;
#13190 = DIRECTION ( 'NONE',  ( -0.7071067811865486830, 0.7071067811865464625, 0.000000000000000000 ) ) ;
#13191 = CARTESIAN_POINT ( 'NONE',  ( 105.6625270504628844, 7.949999999999998401, 1.460391307983218338E-15 ) ) ;
#13192 = LINE ( 'NONE', #44457, #86592 ) ;
#13193 = CARTESIAN_POINT ( 'NONE',  ( 1.074257766332453956, 4.331830624465606405, 5.540583863682179810 ) ) ;
#13194 = CARTESIAN_POINT ( 'NONE',  ( -28.49999999999981171, -1.592773361805396970, -6.492772025301164263 ) ) ;
#13195 = VECTOR ( 'NONE', #35060, 999.9999999999998863 ) ;
#13196 = DIRECTION ( 'NONE',  ( -0.7071067811865486830, -0.7071067811865464625, 0.000000000000000000 ) ) ;
#13197 = DIRECTION ( 'NONE',  ( 0.6830127018922180770, -0.6830127018922204085, -0.2588190451025213501 ) ) ;
#13199 = CONICAL_SURFACE ( 'NONE', #91865, 2.500000000000000888, 0.9599310885968822538 ) ;
#13198 = AXIS2_PLACEMENT_3D ( 'NONE', #65572, #112604, #110433 ) ;
#13200 = CARTESIAN_POINT ( 'NONE',  ( 46.30836038379622721, 7.949999999999997513, 2.130196079827431088 ) ) ;
#13201 = LINE ( 'NONE', #79960, #72270 ) ;
#13202 = VECTOR ( 'NONE', #116832, 1000.000000000000227 ) ;
#13203 = FACE_OUTER_BOUND ( 'NONE', #50608, .T. ) ;
#13204 = ORIENTED_EDGE ( 'NONE', *, *, #109435, .T. ) ;
#13205 = ORIENTED_EDGE ( 'NONE', *, *, #97654, .F. ) ;
#13206 = CARTESIAN_POINT ( 'NONE',  ( 42.85416666666666430, -2.130196079827425315, -7.950000000000001066 ) ) ;
#13207 = ORIENTED_EDGE ( 'NONE', *, *, #121695, .F. ) ;
#13208 = CARTESIAN_POINT ( 'NONE',  ( 6.940000000000001279, 9.521314400968980422E-16, 0.000000000000000000 ) ) ;
#13209 = EDGE_CURVE ( 'NONE', #142320, #71285, #12341, .T. ) ;
#13210 = VECTOR ( 'NONE', #22245, 1000.000000000000000 ) ;
#13211 = AXIS2_PLACEMENT_3D ( 'NONE', #10368, #54623, #108959 ) ;
#13212 = ORIENTED_EDGE ( 'NONE', *, *, #30257, .F. ) ;
#13213 = CARTESIAN_POINT ( 'NONE',  ( -18.18398860626898994, 28.73617430169800002, 5.000000000000000000 ) ) ;
#13215 = EDGE_CURVE ( 'NONE', #124077, #123774, #10752, .T. ) ;
#13214 = CARTESIAN_POINT ( 'NONE',  ( 10.52840764549667618, 3.061616997868382155E-16, -2.500000000000001332 ) ) ;
#13216 = ADVANCED_FACE ( 'NONE', ( #11601 ), #92040, .F. ) ;
#13217 = CARTESIAN_POINT ( 'NONE',  ( 38.20876352523143282, -7.482591942790329030E-16, 6.110000000000001208 ) ) ;
#13218 = EDGE_LOOP ( 'NONE', ( #4820, #80961, #29837, #50615 ) ) ;
#13219 = DIRECTION ( 'NONE',  ( 0.7071067811865487940, 0.7071067811865463515, 0.000000000000000000 ) ) ;
#13220 = VERTEX_POINT ( 'NONE', #1445 ) ;
#13221 = CARTESIAN_POINT ( 'NONE',  ( 28.49999999999979750, -11.56887692260769640, 4.000000000000000000 ) ) ;
#13222 = ADVANCED_FACE ( 'NONE', ( #13750 ), #102942, .F. ) ;
#13223 = DIRECTION ( 'NONE',  ( 0.6830127018922181881, 0.6830127018922202975, -0.2588190451025214056 ) ) ;
#13224 = CARTESIAN_POINT ( 'NONE',  ( -14.59122188827396549, 7.143407583703162089, 5.000000000000000000 ) ) ;
#13225 = EDGE_LOOP ( 'NONE', ( #138154, #31002, #126380 ) ) ;
#13226 = EDGE_CURVE ( 'NONE', #131513, #130990, #34123, .T. ) ;
#13227 = DIRECTION ( 'NONE',  ( -0.7071067811865486830, -0.7071067811865464625, 0.000000000000000000 ) ) ;
#13228 = VERTEX_POINT ( 'NONE', #102240 ) ;
#13229 = DIRECTION ( 'NONE',  ( -0.7071067811865487940, 0.7071067811865463515, 0.000000000000000000 ) ) ;
#13230 = EDGE_CURVE ( 'NONE', #3922, #115259, #13044, .T. ) ;
#13231 = DIRECTION ( 'NONE',  ( -0.7071067811865486830, -0.7071067811865464625, 0.000000000000000000 ) ) ;
#13232 = PLANE ( 'NONE',  #107880 ) ;
#13233 = CIRCLE ( 'NONE', #142817, 3.999999999999996447 ) ;
#13234 = PLANE ( 'NONE',  #11608 ) ;
#13235 = PLANE ( 'NONE',  #97076 ) ;
#13236 = VERTEX_POINT ( 'NONE', #78334 ) ;
#13237 = VECTOR ( 'NONE', #14134, 1000.000000000000000 ) ;
#13238 = ADVANCED_FACE ( 'NONE', ( #89214 ), #68215, .F. ) ;
#13239 = FACE_OUTER_BOUND ( 'NONE', #33860, .T. ) ;
#13240 = CARTESIAN_POINT ( 'NONE',  ( 60.28709685856478728, 3.054999999999997495, 5.291415217122919401 ) ) ;
#13241 = PLANE ( 'NONE',  #46461 ) ;
#13242 = DIRECTION ( 'NONE',  ( -0.7071067811865486830, 0.7071067811865464625, 0.000000000000000000 ) ) ;
#13244 = ORIENTED_EDGE ( 'NONE', *, *, #100533, .T. ) ;
#13243 = CARTESIAN_POINT ( 'NONE',  ( 57.29974487139158157, -27.71228299555246011, 4.000000000000000000 ) ) ;
#13245 = ORIENTED_EDGE ( 'NONE', *, *, #62266, .T. ) ;
#13246 = VECTOR ( 'NONE', #78168, 999.9999999999998863 ) ;
#13247 = DIRECTION ( 'NONE',  ( 0.000000000000000000, 1.000000000000000000, 0.000000000000000000 ) ) ;
#13248 = EDGE_CURVE ( 'NONE', #141150, #142079, #4347, .T. ) ;
#13249 = ORIENTED_EDGE ( 'NONE', *, *, #115942, .T. ) ;
#13250 = DIRECTION ( 'NONE',  ( -0.7071067811865486830, -0.7071067811865464625, -0.000000000000000000 ) ) ;
#13251 = ORIENTED_EDGE ( 'NONE', *, *, #53464, .F. ) ;
#13252 = CARTESIAN_POINT ( 'NONE',  ( 33.70710678118631165, -0.7407075233842788098, 5.000000000000000000 ) ) ;
#13253 = DIRECTION ( 'NONE',  ( 0.7071067811865486830, -0.7071067811865464625, -0.000000000000000000 ) ) ;
#13254 = VECTOR ( 'NONE', #24625, 1000.000000000000000 ) ;
#13255 = LINE ( 'NONE', #104571, #127572 ) ;
#13256 = AXIS2_PLACEMENT_3D ( 'NONE', #123861, #134007, #2005 ) ;
#13257 = FACE_BOUND ( 'NONE', #32729, .T. ) ;
#13258 = DIRECTION ( 'NONE',  ( -0.7071067811865486830, -0.7071067811865464625, 0.000000000000000000 ) ) ;
#13259 = DIRECTION ( 'NONE',  ( 0.000000000000000000, -0.000000000000000000, -1.000000000000000000 ) ) ;
#13260 = CARTESIAN_POINT ( 'NONE',  ( 39.18398860626899705, 28.73617430169814568, 5.000000000000000000 ) ) ;
#13262 = ORIENTED_EDGE ( 'NONE', *, *, #79213, .T. ) ;
#13261 = DIRECTION ( 'NONE',  ( -1.000000000000000000, -0.000000000000000000, -0.000000000000000000 ) ) ;
#13263 = CARTESIAN_POINT ( 'NONE',  ( -0.1839886062690032631, 28.73617430169787568, 5.000000000000000000 ) ) ;
#13264 = EDGE_LOOP ( 'NONE', ( #109776, #64946, #87468, #112804 ) ) ;
#13265 = EDGE_CURVE ( 'NONE', #67219, #58219, #3584, .T. ) ;
#13266 = EDGE_CURVE ( 'NONE', #10862, #55621, #71040, .T. ) ;
#13267 = VERTEX_POINT ( 'NONE', #18016 ) ;
#13268 = CARTESIAN_POINT ( 'NONE',  ( 77.20376352523145158, 6.109999999999998543, 1.122388791418548911E-15 ) ) ;
#13269 = ORIENTED_EDGE ( 'NONE', *, *, #62855, .T. ) ;
#13270 = VECTOR ( 'NONE', #56838, 1000.000000000000000 ) ;
#13271 = CARTESIAN_POINT ( 'NONE',  ( 2.999999999999999112, 0.000000000000000000, 0.000000000000000000 ) ) ;
#13272 = VERTEX_POINT ( 'NONE', #94176 ) ;
#13273 = FACE_OUTER_BOUND ( 'NONE', #72521, .T. ) ;
#13274 = EDGE_CURVE ( 'NONE', #128563, #118592, #71751, .T. ) ;
#13275 = CARTESIAN_POINT ( 'NONE',  ( 30.79333936457826937, 21.75929247661550647, 4.998822639870708073 ) ) ;
#13276 = VECTOR ( 'NONE', #46055, 1000.000000000000000 ) ;
#13277 = DIRECTION ( 'NONE',  ( -0.6830127018922181881, 0.6830127018922202975, -0.2588190451025214056 ) ) ;
#13278 = CARTESIAN_POINT ( 'NONE',  ( 1.554198618961949885, 0.3999999999999995226, 2.412907390626680026 ) ) ;
#13280 = PRESENTATION_STYLE_ASSIGNMENT (( #69873 ) ) ;
#13279 = FACE_OUTER_BOUND ( 'NONE', #130437, .T. ) ;
#13281 = CARTESIAN_POINT ( 'NONE',  ( 97.25000000000000000, -9.735942053221458872E-16, 7.950000000000000178 ) ) ;
#13282 = CARTESIAN_POINT ( 'NONE',  ( -21.18398860626899349, 28.73617430169802134, 5.000000000000000000 ) ) ;
#13283 = ORIENTED_EDGE ( 'NONE', *, *, #309, .F. ) ;
#13284 = ORIENTED_EDGE ( 'NONE', *, *, #72861, .F. ) ;
#13285 = CARTESIAN_POINT ( 'NONE',  ( -18.40295003975137078, -2.759949774800250832, 4.658785122533365630 ) ) ;
#13286 = VECTOR ( 'NONE', #79707, 1000.000000000000000 ) ;
#13287 = VERTEX_POINT ( 'NONE', #4256 ) ;
#13288 = ORIENTED_EDGE ( 'NONE', *, *, #62660, .T. ) ;
#13290 = ORIENTED_EDGE ( 'NONE', *, *, #117163, .T. ) ;
#13289 = CIRCLE ( 'NONE', #112856, 2.500000000000000888 ) ;
#13291 = DIRECTION ( 'NONE',  ( 0.3543493200069162685, -0.000000000000000000, -0.9351131265310288487 ) ) ;
#13292 = APPLICATION_CONTEXT ( 'automotive_design' ) ;
#13293 = DIRECTION ( 'NONE',  ( -0.7071067811865487940, 0.7071067811865463515, -0.000000000000000000 ) ) ;
#13294 = ORIENTED_EDGE ( 'NONE', *, *, #6635, .F. ) ;
#13295 = FACE_OUTER_BOUND ( 'NONE', #32269, .T. ) ;
#13296 = VECTOR ( 'NONE', #62173, 1000.000000000000000 ) ;
#13297 = AXIS2_PLACEMENT_3D ( 'NONE', #79669, #112943, #70216 ) ;
#13298 = CARTESIAN_POINT ( 'NONE',  ( 43.24586038379622721, 3.974999999999996980, 6.884901960086287964 ) ) ;
#13299 = AXIS2_PLACEMENT_3D ( 'NONE', #133962, #23782, #100634 ) ;
#13300 = CARTESIAN_POINT ( 'NONE',  ( 3.567069808101885897, 2.126176841940952134, -7.934999999999993392 ) ) ;
#13301 = CARTESIAN_POINT ( 'NONE',  ( 16.67979525387081807, 0.3337821591035673441, -30.81818940114110816 ) ) ;
#13302 = VERTEX_POINT ( 'NONE', #26095 ) ;
#13303 = FACE_OUTER_BOUND ( 'NONE', #65799, .T. ) ;
#13305 = EDGE_CURVE ( 'NONE', #110282, #92427, #137719, .T. ) ;
#13304 = CARTESIAN_POINT ( 'NONE',  ( 120.5375270504628844, -9.735942053221456900E-16, 7.949999999999998401 ) ) ;
#13306 = VECTOR ( 'NONE', #92574, 1000.000000000000227 ) ;
#13307 = LINE ( 'NONE', #77884, #12790 ) ;
#13309 = VERTEX_POINT ( 'NONE', #104329 ) ;
#13308 = CARTESIAN_POINT ( 'NONE',  ( -2.510786437626908008, -27.52281430457053446, 5.000000000000000000 ) ) ;
#13310 = ORIENTED_EDGE ( 'NONE', *, *, #67677, .T. ) ;
#13311 = LINE ( 'NONE', #56175, #21827 ) ;
#13312 = CARTESIAN_POINT ( 'NONE',  ( -6.717577386425628738, -21.73023691814492508, 5.000000000000000888 ) ) ;
#13313 = FACE_OUTER_BOUND ( 'NONE', #143259, .T. ) ;
#13314 = ORIENTED_EDGE ( 'NONE', *, *, #130042, .F. ) ;
#13315 = CARTESIAN_POINT ( 'NONE',  ( -35.99451991528749772, 28.92564299267963079, 4.000000000000000000 ) ) ;
#13316 = LINE ( 'NONE', #1705, #122002 ) ;
#13317 = SURFACE_STYLE_FILL_AREA ( #68476 ) ;
#13318 = CARTESIAN_POINT ( 'NONE',  ( 28.85416666666666075, -2.130196079827425759, -7.950000000000000178 ) ) ;
#13319 = LINE ( 'NONE', #133710, #3194 ) ;
#13320 = PLANE ( 'NONE',  #80913 ) ;
#13321 = DIRECTION ( 'NONE',  ( 0.6830127018922181881, 0.6830127018922202975, -0.2588190451025214056 ) ) ;
#13322 = CARTESIAN_POINT ( 'NONE',  ( -2.671830600776449405, -15.74070752338412404, 4.000000000000000000 ) ) ;
#13323 = EDGE_CURVE ( 'NONE', #116320, #71524, #115910, .T. ) ;
#13324 = CARTESIAN_POINT ( 'NONE',  ( -29.99999999999979750, -0.2811185226894580280, -5.995736974527445362 ) ) ;
#13325 = DIRECTION ( 'NONE',  ( -0.3543493200069162685, -0.000000000000000000, -0.9351131265310288487 ) ) ;
#13326 = EDGE_CURVE ( 'NONE', #137801, #100474, #81198, .T. ) ;
#13328 = ORIENTED_EDGE ( 'NONE', *, *, #131117, .T. ) ;
#13327 = EDGE_CURVE ( 'NONE', #119026, #81137, #115189, .T. ) ;
#13329 = ORIENTED_EDGE ( 'NONE', *, *, #99021, .T. ) ;
#13330 = AXIS2_PLACEMENT_3D ( 'NONE', #132290, #122803, #23485 ) ;
#13332 = ADVANCED_FACE ( 'NONE', ( #72490 ), #138418, .F. ) ;
#13331 = CARTESIAN_POINT ( 'NONE',  ( 25.75309147121574327, -1.701477371937609728, -6.350000000000015632 ) ) ;
#13333 = CARTESIAN_POINT ( 'NONE',  ( -5.999999999999960032, -16.60178936734449096, 0.8616154019347350701 ) ) ;
#13334 =( BOUNDED_CURVE ( )  B_SPLINE_CURVE ( 3, ( #120321, #76896, #87029, #121069 ),
 .UNSPECIFIED., .F., .T. ) 
 B_SPLINE_CURVE_WITH_KNOTS ( ( 4, 4 ),
 ( 1.208578181583248368, 1.359146454359429157 ),
 .UNSPECIFIED. ) 
 CURVE ( )  GEOMETRIC_REPRESENTATION_ITEM ( )  RATIONAL_B_SPLINE_CURVE ( ( 1.000000000000000000, 0.9981116584018958626, 0.9981116584018958626, 1.000000000000000000 ) ) 
 REPRESENTATION_ITEM ( '' )  );
#13335 = EDGE_CURVE ( 'NONE', #140981, #41660, #114507, .T. ) ;
#13336 = EDGE_CURVE ( 'NONE', #65177, #46312, #92749, .T. ) ;
#13337 = SURFACE_SIDE_STYLE ('',( #34403 ) ) ;
#13338 = LINE ( 'NONE', #57607, #133906 ) ;
#13339 = ORIENTED_EDGE ( 'NONE', *, *, #140049, .T. ) ;
#13340 = FACE_OUTER_BOUND ( 'NONE', #112986, .T. ) ;
#13341 = CARTESIAN_POINT ( 'NONE',  ( 45.18398860626900415, 28.73617430169818832, 5.000000000000000000 ) ) ;
#13342 = CARTESIAN_POINT ( 'NONE',  ( -10.64175702458853401, 15.75929247661555799, 19.34181609438702054 ) ) ;
#13343 = VERTEX_POINT ( 'NONE', #59459 ) ;
#13344 = ADVANCED_FACE ( 'NONE', ( #81936 ), #105749, .F. ) ;
#13345 = DIRECTION ( 'NONE',  ( -0.000000000000000000, -0.3543493200069152693, 0.9351131265310292928 ) ) ;
#13346 = LINE ( 'NONE', #46025, #72447 ) ;
#13347 =( NAMED_UNIT ( * ) PLANE_ANGLE_UNIT ( ) SI_UNIT ( $, .RADIAN. ) );
#13348 = CARTESIAN_POINT ( 'NONE',  ( 51.97459685856478728, 1.637169565754164280, -6.109999999999997655 ) ) ;
#13349 = CARTESIAN_POINT ( 'NONE',  ( 3.489213562373097322, -27.52281430457057709, 5.000000000000000000 ) ) ;
#13350 = ADVANCED_FACE ( 'NONE', ( #94881 ), #118298, .T. ) ;
#13351 = FACE_OUTER_BOUND ( 'NONE', #65865, .T. ) ;
#13352 = CARTESIAN_POINT ( 'NONE',  ( 14.99451991528749595, 28.92564299267948513, 4.000000000000000000 ) ) ;
#13353 = ORIENTED_EDGE ( 'NONE', *, *, #65784, .F. ) ;
#13354 = PRESENTATION_STYLE_ASSIGNMENT (( #143177 ) ) ;
#13355 = VERTEX_POINT ( 'NONE', #86897 ) ;
#13356 = LINE ( 'NONE', #57625, #22250 ) ;
#13357 = ADVANCED_FACE ( 'NONE', ( #130409 ), #29629, .F. ) ;
#13358 = FACE_OUTER_BOUND ( 'NONE', #47111, .T. ) ;
#13359 =( LENGTH_UNIT ( ) NAMED_UNIT ( * ) SI_UNIT ( .MILLI., .METRE. ) );
#13360 = CARTESIAN_POINT ( 'NONE',  ( 0.000000000000000000, 0.000000000000000000, 0.000000000000000000 ) ) ;
#13361 = CARTESIAN_POINT ( 'NONE',  ( 26.27718569542921401, -21.72499999999999432, 5.000000000000000000 ) ) ;
#13362 = ORIENTED_EDGE ( 'NONE', *, *, #107026, .F. ) ;
#13363 = VERTEX_POINT ( 'NONE', #120184 ) ;
#13364 = LINE ( 'NONE', #2480, #113486 ) ;
#13365 = SURFACE_STYLE_FILL_AREA ( #88108 ) ;
#13366 = EDGE_CURVE ( 'NONE', #46544, #38617, #122978, .T. ) ;
#13367 = CARTESIAN_POINT ( 'NONE',  ( 45.29974487139158867, -27.71228299555237840, 4.000000000000000000 ) ) ;
#13368 = CARTESIAN_POINT ( 'NONE',  ( 12.19999999999999574, -25.33999999999998565, 2.999999999999999112 ) ) ;
#13369 = CARTESIAN_POINT ( 'NONE',  ( 71.68336038379621300, -2.130196079827426203, 7.949999999999997513 ) ) ;
#13370 = FACE_OUTER_BOUND ( 'NONE', #90331, .T. ) ;
#13371 = LINE ( 'NONE', #35182, #124786 ) ;
#13372 = ORIENTED_EDGE ( 'NONE', *, *, #12758, .F. ) ;
#13373 = VECTOR ( 'NONE', #56323, 1000.000000000000000 ) ;
#13374 = CARTESIAN_POINT ( 'NONE',  ( 77.56250000000000000, -5.819803920172572198, -5.819803920172573086 ) ) ;
#13375 = FACE_OUTER_BOUND ( 'NONE', #66691, .T. ) ;
#13376 = PLANE ( 'NONE',  #136487 ) ;
#13377 = CARTESIAN_POINT ( 'NONE',  ( -48.48921356237309510, -27.52281430457089328, 5.000000000000000000 ) ) ;
#13378 = EDGE_CURVE ( 'NONE', #16426, #68681, #80355, .T. ) ;
#13379 = ORIENTED_EDGE ( 'NONE', *, *, #91759, .F. ) ;
#13380 = CARTESIAN_POINT ( 'NONE',  ( -12.18398860626900060, 28.73617430169795739, 5.000000000000000000 ) ) ;
#13381 = EDGE_CURVE ( 'NONE', #44009, #102743, #65889, .T. ) ;
#13382 = VECTOR ( 'NONE', #141609, 1000.000000000000000 ) ;
#13383 = DIRECTION ( 'NONE',  ( 0.000000000000000000, -1.000000000000000000, 0.000000000000000000 ) ) ;
#13384 = CARTESIAN_POINT ( 'NONE',  ( 61.54209685856476852, 5.291415217122923842, -3.054999999999996163 ) ) ;
#13385 = EDGE_CURVE ( 'NONE', #26526, #73071, #43387, .T. ) ;
#13386 = FACE_BOUND ( 'NONE', #79579, .T. ) ;
#13387 = ORIENTED_EDGE ( 'NONE', *, *, #103654, .F. ) ;
#13388 = ORIENTED_EDGE ( 'NONE', *, *, #103315, .T. ) ;
#13389 = EDGE_CURVE ( 'NONE', #85582, #82671, #63024, .T. ) ;
#13390 = CARTESIAN_POINT ( 'NONE',  ( -51.48921356237309510, -27.52281430457091460, 5.000000000000000000 ) ) ;
#13391 = DIRECTION ( 'NONE',  ( 0.7071067811865487940, 0.7071067811865463515, 0.000000000000000000 ) ) ;
#13392 = VECTOR ( 'NONE', #35072, 1000.000000000000000 ) ;
#13393 = LINE ( 'NONE', #56266, #46606 ) ;
#13395 = EDGE_LOOP ( 'NONE', ( #13070, #40647, #92582, #72225 ) ) ;
#13394 = CARTESIAN_POINT ( 'NONE',  ( 85.58333333333332860, 6.884901960086290629, -3.974999999999994316 ) ) ;
#13396 = PLANE ( 'NONE',  #97013 ) ;
#13397 = DIRECTION ( 'NONE',  ( 0.3543493200069162685, -0.000000000000000000, -0.9351131265310288487 ) ) ;
#13398 = CARTESIAN_POINT ( 'NONE',  ( 8.811592354503320124, 9.902892378096218942E-16, 0.000000000000000000 ) ) ;
#13399 = VECTOR ( 'NONE', #53809, 1000.000000000000000 ) ;
#13400 = CIRCLE ( 'NONE', #71295, 2.055000000000000604 ) ;
#13401 = ORIENTED_EDGE ( 'NONE', *, *, #103404, .F. ) ;
#13402 = EDGE_LOOP ( 'NONE', ( #108890, #22579, #137519, #92782 ) ) ;
#13403 = CARTESIAN_POINT ( 'NONE',  ( 58.18793019189811133, 6.110000000000002984, -1.637169565754156730 ) ) ;
#13404 = ORIENTED_EDGE ( 'NONE', *, *, #50372, .T. ) ;
#13405 = EDGE_CURVE ( 'NONE', #28845, #60521, #66576, .T. ) ;
#13406 = LINE ( 'NONE', #113444, #8200 ) ;
#13407 = DIRECTION ( 'NONE',  ( -0.000000000000000000, -0.3543493200069152693, 0.9351131265310292928 ) ) ;
#13408 = CARTESIAN_POINT ( 'NONE',  ( -72.29974487139158157, -27.71228299555256669, 4.000000000000000000 ) ) ;
#13409 = DIRECTION ( 'NONE',  ( -0.6830127018922181881, 0.6830127018922202975, -0.2588190451025214056 ) ) ;
#13410 = LINE ( 'NONE', #3258, #96377 ) ;
#13411 = ORIENTED_EDGE ( 'NONE', *, *, #24714, .F. ) ;
#13412 = VERTEX_POINT ( 'NONE', #112223 ) ;
#13413 = CARTESIAN_POINT ( 'NONE',  ( -8.671830600776404552, 20.25929247661551003, 4.000000000000000000 ) ) ;
#13415 = EDGE_CURVE ( 'NONE', #108674, #132815, #133272, .T. ) ;
#13414 =( NAMED_UNIT ( * ) SI_UNIT ( $, .STERADIAN. ) SOLID_ANGLE_UNIT ( ) );
#13416 = EDGE_LOOP ( 'NONE', ( #50129, #59476, #64925, #89276, #78111 ) ) ;
#13417 = DIRECTION ( 'NONE',  ( 0.7071067811865487940, -0.7071067811865463515, 0.000000000000000000 ) ) ;
#13418 = ORIENTED_EDGE ( 'NONE', *, *, #95955, .F. ) ;
#13419 = VECTOR ( 'NONE', #81506, 1000.000000000000227 ) ;
#13420 = FACE_BOUND ( 'NONE', #37603, .T. ) ;
#13421 = LINE ( 'NONE', #111325, #135827 ) ;
#13422 = EDGE_CURVE ( 'NONE', #87748, #141528, #45564, .T. ) ;
#13423 = DIRECTION ( 'NONE',  ( -0.6830127018922181881, 0.6830127018922202975, -0.2588190451025214056 ) ) ;
#13424 = DIRECTION ( 'NONE',  ( -0.7071067811865486830, -0.7071067811865464625, -0.000000000000000000 ) ) ;
#13425 = VECTOR ( 'NONE', #100850, 999.9999999999998863 ) ;
#13426 = DIRECTION ( 'NONE',  ( -0.7071067811865486830, -0.7071067811865464625, 0.000000000000000000 ) ) ;
#13427 = LINE ( 'NONE', #12729, #4909 ) ;
#13428 = CARTESIAN_POINT ( 'NONE',  ( -78.45649007701877053, 11.12797054829585797, -15.40026855208242473 ) ) ;
#13429 = ORIENTED_EDGE ( 'NONE', *, *, #132764, .T. ) ;
#13430 = EDGE_CURVE ( 'NONE', #76656, #34219, #99157, .T. ) ;
#13431 = ORIENTED_EDGE ( 'NONE', *, *, #41735, .F. ) ;
#13432 = CARTESIAN_POINT ( 'NONE',  ( 99.37043019189812298, -3.055000000000001492, 5.291415217122917625 ) ) ;
#13433 = ORIENTED_EDGE ( 'NONE', *, *, #79927, .F. ) ;
#13434 = CARTESIAN_POINT ( 'NONE',  ( -25.17183060077628909, 18.75929247661552068, 4.000000000000000000 ) ) ;
#13435 = VERTEX_POINT ( 'NONE', #123101 ) ;
#13436 = DIRECTION ( 'NONE',  ( 0.000000000000000000, 0.000000000000000000, 1.000000000000000000 ) ) ;
#13437 = AXIS2_PLACEMENT_3D ( 'NONE', #138485, #94247, #139215 ) ;
#13438 = EDGE_CURVE ( 'NONE', #32782, #29397, #1964, .T. ) ;
#13439 = CARTESIAN_POINT ( 'NONE',  ( 6.793339364578431017, 21.75929247661549226, 4.998822639870705409 ) ) ;
#13440 = VECTOR ( 'NONE', #76512, 1000.000000000000000 ) ;
#13442 = EDGE_CURVE ( 'NONE', #121504, #878, #31797, .T. ) ;
#13441 = CARTESIAN_POINT ( 'NONE',  ( 24.32816939922335564, -9.740707523384184441, 4.000000000000000000 ) ) ;
#13443 = VERTEX_POINT ( 'NONE', #33953 ) ;
#13444 = CARTESIAN_POINT ( 'NONE',  ( 12.93606151716249819, -22.22500000000000142, 23.13634534928430142 ) ) ;
#13445 = DIRECTION ( 'NONE',  ( -1.000000000000000000, -0.000000000000000000, -0.000000000000000000 ) ) ;
#13446 = CARTESIAN_POINT ( 'NONE',  ( 63.18398860626900415, 28.73617430169831621, 5.000000000000000000 ) ) ;
#13448 = PLANE ( 'NONE',  #98329 ) ;
#13447 = CARTESIAN_POINT ( 'NONE',  ( 20.99999999999985789, 16.55218569542900298, 5.000000000000000000 ) ) ;
#13449 = DIRECTION ( 'NONE',  ( -0.6830127018922181881, 0.6830127018922202975, -0.2588190451025214056 ) ) ;
#13450 = CARTESIAN_POINT ( 'NONE',  ( 21.29159235450332233, 3.061616997868380183E-16, -2.500000000000001332 ) ) ;
#13451 = VERTEX_POINT ( 'NONE', #91206 ) ;
#13452 = CARTESIAN_POINT ( 'NONE',  ( -15.70710678118643422, 14.25929247661557042, 5.000000000000000000 ) ) ;
#13453 = PLANE ( 'NONE',  #106704 ) ;
#13454 = EDGE_LOOP ( 'NONE', ( #138559, #99954, #53899, #29412 ) ) ;
#13455 = ORIENTED_EDGE ( 'NONE', *, *, #135501, .T. ) ;
#13456 = ADVANCED_FACE ( 'NONE', ( #34659 ), #78894, .T. ) ;
#13457 = VERTEX_POINT ( 'NONE', #23780 ) ;
#13458 = CARTESIAN_POINT ( 'NONE',  ( 58.47959685856477563, 6.109999999999999432, 1.637169565754164280 ) ) ;
#13459 = ORIENTED_EDGE ( 'NONE', *, *, #44846, .F. ) ;
#13460 = CARTESIAN_POINT ( 'NONE',  ( 8.066639616203771013, 1.633150327867695095, 6.094999999999988205 ) ) ;
#13461 = CARTESIAN_POINT ( 'NONE',  ( 92.16709685856477563, -3.055000000000000160, -5.291415217122921177 ) ) ;
#13462 = CARTESIAN_POINT ( 'NONE',  ( 0.000000000000000000, 21.72500000000000142, 4.500000000000000888 ) ) ;
#13463 = ORIENTED_EDGE ( 'NONE', *, *, #57746, .T. ) ;
#13464 = CARTESIAN_POINT ( 'NONE',  ( -27.48921356237309155, -27.52281430457074762, 5.000000000000000000 ) ) ;
#13465 = ORIENTED_EDGE ( 'NONE', *, *, #27781, .F. ) ;
#13466 = DIRECTION ( 'NONE',  ( -0.3543493200069162685, -0.000000000000000000, -0.9351131265310288487 ) ) ;
#13467 = CARTESIAN_POINT ( 'NONE',  ( 34.92500000000001847, 1.088194295437629318E-14, 0.000000000000000000 ) ) ;
#13468 = EDGE_LOOP ( 'NONE', ( #137241, #135798, #13861, #113131, #118867 ) ) ;
#13469 = PLANE ( 'NONE',  #25923 ) ;
#13470 = LINE ( 'NONE', #92470, #129347 ) ;
#13471 = CARTESIAN_POINT ( 'NONE',  ( 125.9120968585647802, 5.291415217122922066, -3.054999999999995275 ) ) ;
#13472 = ORIENTED_EDGE ( 'NONE', *, *, #43024, .T. ) ;
#13473 = LINE ( 'NONE', #2612, #119764 ) ;
#13474 = ORIENTED_EDGE ( 'NONE', *, *, #136171, .T. ) ;
#13475 = ORIENTED_EDGE ( 'NONE', *, *, #46296, .T. ) ;
#13476 = ORIENTED_EDGE ( 'NONE', *, *, #104229, .F. ) ;
#13477 = ADVANCED_FACE ( 'NONE', ( #88331 ), #99902, .T. ) ;
#13478 = LINE ( 'NONE', #89644, #23933 ) ;
#13479 = AXIS2_PLACEMENT_3D ( 'NONE', #99763, #111342, #434 ) ;
#13480 = VECTOR ( 'NONE', #76851, 1000.000000000000000 ) ;
#13481 = EDGE_CURVE ( 'NONE', #15939, #27153, #110742, .T. ) ;
#13482 = DIRECTION ( 'NONE',  ( -0.7071067811865486830, -0.7071067811865464625, 0.000000000000000000 ) ) ;
#13483 = CARTESIAN_POINT ( 'NONE',  ( -21.29974487139158512, -27.71228299555221142, 4.000000000000000000 ) ) ;
#13484 = DIRECTION ( 'NONE',  ( 0.6830127018922180770, -0.6830127018922204085, -0.2588190451025213501 ) ) ;
#13485 = VECTOR ( 'NONE', #127092, 1000.000000000000000 ) ;
#13486 = EDGE_CURVE ( 'NONE', #17086, #63012, #46276, .T. ) ;
#13487 = EDGE_CURVE ( 'NONE', #131139, #687, #88705, .T. ) ;
#13488 = CARTESIAN_POINT ( 'NONE',  ( -7.499999999999944045, -4.533600742197697819, 5.000000000000000000 ) ) ;
#13489 = ORIENTED_EDGE ( 'NONE', *, *, #121448, .F. ) ;
#13490 = AXIS2_PLACEMENT_3D ( 'NONE', #41296, #55778, #30440 ) ;
#13491 = VECTOR ( 'NONE', #70919, 1000.000000000000000 ) ;
#13492 =( LENGTH_UNIT ( ) NAMED_UNIT ( * ) SI_UNIT ( .MILLI., .METRE. ) );
#13493 = EDGE_CURVE ( 'NONE', #85379, #74078, #90461, .T. ) ;
#13494 = EDGE_CURVE ( 'NONE', #22682, #130801, #112919, .T. ) ;
#13495 = CARTESIAN_POINT ( 'NONE',  ( 18.20790314143522082, -6.871911579029513106, -3.967499999999993587 ) ) ;
#13496 = CARTESIAN_POINT ( 'NONE',  ( 72.18398860626899705, 28.73617430169837661, 5.000000000000000000 ) ) ;
#13497 = EDGE_CURVE ( 'NONE', #136694, #78508, #13579, .T. ) ;
#13498 = CARTESIAN_POINT ( 'NONE',  ( 33.48921356237309510, -27.52281430457078670, 5.000000000000000000 ) ) ;
#13499 = CARTESIAN_POINT ( 'NONE',  ( 48.18398860626899705, 28.73617430169820608, 5.000000000000000000 ) ) ;
#13500 = EDGE_LOOP ( 'NONE', ( #57039, #9518, #101181, #47779, #105390 ) ) ;
#13501 = ORIENTED_EDGE ( 'NONE', *, *, #95832, .T. ) ;
#13502 = EDGE_CURVE ( 'NONE', #18391, #66770, #124405, .T. ) ;
#13503 = ORIENTED_EDGE ( 'NONE', *, *, #133305, .F. ) ;
#13504 = CARTESIAN_POINT ( 'NONE',  ( 58.16666666666665719, 6.884901960086285300, 3.975000000000003642 ) ) ;
#13505 = VECTOR ( 'NONE', #56740, 1000.000000000000000 ) ;
#13506 = EDGE_CURVE ( 'NONE', #18584, #19349, #12170, .T. ) ;
#13507 = CYLINDRICAL_SURFACE ( 'NONE', #72968, 2.500000000000000000 ) ;
#13508 = PLANE ( 'NONE',  #36640 ) ;
#13509 = CARTESIAN_POINT ( 'NONE',  ( 6.399664195087332530, 9.300955700193000553, 1.952836266634600415 ) ) ;
#13510 = EDGE_CURVE ( 'NONE', #54672, #9777, #115023, .T. ) ;
#13512 = CARTESIAN_POINT ( 'NONE',  ( -14.39158342593604623, -0.5643469832421014187, 4.274152510792116111 ) ) ;
#13511 = VECTOR ( 'NONE', #11379, 1000.000000000000000 ) ;
#13513 = CARTESIAN_POINT ( 'NONE',  ( 8.968407645496675684, 3.061616997868382155E-16, -2.500000000000001332 ) ) ;
#13514 = FACE_OUTER_BOUND ( 'NONE', #96052, .T. ) ;
#13515 = DIRECTION ( 'NONE',  ( -0.7071067811865486830, 0.7071067811865464625, 0.000000000000000000 ) ) ;
#13516 = CYLINDRICAL_SURFACE ( 'NONE', #95064, 0.5000000000000004441 ) ;
#13517 = EDGE_LOOP ( 'NONE', ( #110209, #93539, #19478, #104709 ) ) ;
#13518 = VECTOR ( 'NONE', #72454, 1000.000000000000000 ) ;
#13519 = CARTESIAN_POINT ( 'NONE',  ( 19.71979893569068309, -1.560063818677258851, -32.18359520017570219 ) ) ;
#13520 = VERTEX_POINT ( 'NONE', #4815 ) ;
#13521 = AXIS2_PLACEMENT_3D ( 'NONE', #88271, #22254, #34597 ) ;
#13522 = EDGE_CURVE ( 'NONE', #7112, #102959, #136811, .T. ) ;
#13523 = VECTOR ( 'NONE', #44932, 999.9999999999998863 ) ;
#13524 = CARTESIAN_POINT ( 'NONE',  ( 30.32816939922332367, -18.74070752338408852, 4.000000000000000000 ) ) ;
#13526 = ORIENTED_EDGE ( 'NONE', *, *, #45308, .T. ) ;
#13525 = LINE ( 'NONE', #25855, #25600 ) ;
#13527 = CARTESIAN_POINT ( 'NONE',  ( -3.707106781186516375, 2.259292476615692546, 5.000000000000000000 ) ) ;
#13528 = ORIENTED_EDGE ( 'NONE', *, *, #93165, .F. ) ;
#13529 = PLANE ( 'NONE',  #39207 ) ;
#13530 = ORIENTED_EDGE ( 'NONE', *, *, #42040, .F. ) ;
#13531 = DIRECTION ( 'NONE',  ( 0.7071067811865487940, -0.7071067811865463515, 0.000000000000000000 ) ) ;
#13532 = EDGE_LOOP ( 'NONE', ( #11932, #6846, #128096, #1458 ) ) ;
#13533 = EDGE_CURVE ( 'NONE', #74042, #98919, #91874, .T. ) ;
#13534 = DIRECTION ( 'NONE',  ( -0.7071067811865487940, 0.7071067811865463515, -0.000000000000000000 ) ) ;
#13535 = CARTESIAN_POINT ( 'NONE',  ( 107.4125270504628986, -7.949999999999998401, -4.867971026610728450E-16 ) ) ;
#13536 = CARTESIAN_POINT ( 'NONE',  ( -1.828169399223514624, 0.7592924766157069794, 4.000000000000000000 ) ) ;
#13537 = LINE ( 'NONE', #14978, #64451 ) ;
#13538 = VERTEX_POINT ( 'NONE', #27319 ) ;
#13539 = FACE_OUTER_BOUND ( 'NONE', #116193, .T. ) ;
#13540 = PLANE ( 'NONE',  #63539 ) ;
#13541 = CARTESIAN_POINT ( 'NONE',  ( -32.99999999999976552, 10.21212019023806938, -2.019456568337719915 ) ) ;
#13542 = CARTESIAN_POINT ( 'NONE',  ( 17.06250000000000000, 4.461849672132300881, 4.461849672132299105 ) ) ;
#13543 = CARTESIAN_POINT ( 'NONE',  ( 23.16623647476855652, 7.934999999999990727, -1.457635852685135314E-15 ) ) ;
#13544 = VECTOR ( 'NONE', #32260, 1000.000000000000000 ) ;
#13545 = FACE_OUTER_BOUND ( 'NONE', #40539, .T. ) ;
#13546 = DIRECTION ( 'NONE',  ( 0.7071067811865487940, 0.7071067811865463515, 0.000000000000000000 ) ) ;
#13547 = VERTEX_POINT ( 'NONE', #114347 ) ;
#13548 = CIRCLE ( 'NONE', #69165, 3.999999999999989786 ) ;
#13549 = CARTESIAN_POINT ( 'NONE',  ( 17.99451991528748351, 28.92564299267950645, 4.000000000000000000 ) ) ;
#13550 = EDGE_CURVE ( 'NONE', #99716, #118694, #44247, .T. ) ;
#13551 = EDGE_LOOP ( 'NONE', ( #132819, #88899, #28444, #37610 ) ) ;
#13552 = CARTESIAN_POINT ( 'NONE',  ( 98.00043019189810423, -3.055000000000002380, 5.291415217122920289 ) ) ;
#13553 = ADVANCED_FACE ( 'NONE', ( #92571 ), #82447, .F. ) ;
#13554 = CARTESIAN_POINT ( 'NONE',  ( -18.48921356237309510, -27.52281430457068367, 5.000000000000000000 ) ) ;
#13555 = FACE_OUTER_BOUND ( 'NONE', #63579, .T. ) ;
#13556 = CARTESIAN_POINT ( 'NONE',  ( -18.70679250724062470, 20.25929247661551358, 20.83292124670819234 ) ) ;
#13557 = LINE ( 'NONE', #80299, #73379 ) ;
#13558 = ORIENTED_EDGE ( 'NONE', *, *, #102914, .T. ) ;
#13559 = CARTESIAN_POINT ( 'NONE',  ( 2.287690060339692355, -21.73547319004781286, 4.999917730833664642 ) ) ;
#13560 = EDGE_CURVE ( 'NONE', #65963, #124966, #136096, .T. ) ;
#13561 = DIRECTION ( 'NONE',  ( 0.7071067811865486830, 0.7071067811865464625, 0.000000000000000000 ) ) ;
#13562 = ORIENTED_EDGE ( 'NONE', *, *, #58347, .F. ) ;
#13563 = CARTESIAN_POINT ( 'NONE',  ( -19.49999999999986855, 18.43112307739199451, 4.000000000000000000 ) ) ;
#13564 = CARTESIAN_POINT ( 'NONE',  ( -54.48921356237310221, -27.52281430457093236, 5.000000000000000000 ) ) ;
#13566 = ORIENTED_EDGE ( 'NONE', *, *, #99829, .F. ) ;
#13565 = CARTESIAN_POINT ( 'NONE',  ( 4.499999999999979572, -17.94781430457064531, 5.000000000000000000 ) ) ;
#13567 = CARTESIAN_POINT ( 'NONE',  ( 8.999999999999941380, 1.931123077392167264, 4.000000000000000000 ) ) ;
#13568 = DIRECTION ( 'NONE',  ( -0.000000000000000000, 0.3543493200069153248, 0.9351131265310292928 ) ) ;
#13569 = DIRECTION ( 'NONE',  ( 0.6830127018922180770, -0.6830127018922204085, -0.2588190451025213501 ) ) ;
#13570 = CARTESIAN_POINT ( 'NONE',  ( -26.52663903635769671, -5.240707523384225297, 16.25846745537489468 ) ) ;
#13571 = FACE_OUTER_BOUND ( 'NONE', #128853, .T. ) ;
#13572 = EDGE_LOOP ( 'NONE', ( #549, #53587, #83815, #46997, #119073, #61675 ) ) ;
#13573 = EDGE_LOOP ( 'NONE', ( #108344, #43238, #31174, #126100 ) ) ;
#13574 = ORIENTED_EDGE ( 'NONE', *, *, #58519, .F. ) ;
#13575 = CARTESIAN_POINT ( 'NONE',  ( 82.54209685856478984, 5.291415217122923842, -3.054999999999996163 ) ) ;
#13576 = EDGE_LOOP ( 'NONE', ( #118429, #140995, #11000, #69061 ) ) ;
#13577 = EDGE_CURVE ( 'NONE', #35940, #78703, #137542, .T. ) ;
#13578 = DIRECTION ( 'NONE',  ( 0.7071067811865487940, 0.7071067811865463515, 0.000000000000000000 ) ) ;
#13579 = LINE ( 'NONE', #2718, #6275 ) ;
#13580 = CARTESIAN_POINT ( 'NONE',  ( -11.99999999999991651, -21.41253812416053393, 4.000000000000000000 ) ) ;
#13581 = CARTESIAN_POINT ( 'NONE',  ( -51.18398860626899705, 28.73617430169823095, 5.000000000000000000 ) ) ;
#13582 = ORIENTED_EDGE ( 'NONE', *, *, #13942, .T. ) ;
#13583 = LINE ( 'NONE', #36783, #120852 ) ;
#13584 = DIRECTION ( 'NONE',  ( 0.000000000000000000, -0.3543493200069152138, 0.9351131265310292928 ) ) ;
#13585 = DIRECTION ( 'NONE',  ( 0.000000000000000000, -1.000000000000000000, 0.000000000000000000 ) ) ;
#13586 = CARTESIAN_POINT ( 'NONE',  ( 80.55793019189812298, 6.110000000000000320, -1.637169565754156064 ) ) ;
#13587 = ORIENTED_EDGE ( 'NONE', *, *, #94600, .F. ) ;
#13588 = EDGE_CURVE ( 'NONE', #53081, #25946, #104895, .T. ) ;
#13589 = CARTESIAN_POINT ( 'NONE',  ( 24.41161490594814154, 22.22499999999999787, 4.777194822843817690 ) ) ;
#13590 = DIRECTION ( 'NONE',  ( -0.7071067811865486830, -0.7071067811865464625, -0.000000000000000000 ) ) ;
#13591 = VECTOR ( 'NONE', #70048, 1000.000000000000000 ) ;
#13592 = CONICAL_SURFACE ( 'NONE', #101562, 2.500000000000000888, 0.9599310885968822538 ) ;
#13593 = AXIS2_PLACEMENT_3D ( 'NONE', #43588, #119685, #10233 ) ;
#13594 = ORIENTED_EDGE ( 'NONE', *, *, #103479, .F. ) ;
#13595 = ORIENTED_EDGE ( 'NONE', *, *, #9974, .F. ) ;
#13596 = AXIS2_PLACEMENT_3D ( 'NONE', #108638, #96333, #18053 ) ;
#13597 = EDGE_CURVE ( 'NONE', #27998, #66021, #115728, .T. ) ;
#13598 = CARTESIAN_POINT ( 'NONE',  ( 5.994519915287488843, 28.92564299267942118, 4.000000000000000000 ) ) ;
#13599 = CARTESIAN_POINT ( 'NONE',  ( 27.22000000000000242, 2.055000000000001492, 2.516649172247811554E-16 ) ) ;
#13600 = CARTESIAN_POINT ( 'NONE',  ( 23.40040314143521982, -7.934999999999988951, 2.126176841940957907 ) ) ;
#13601 = LINE ( 'NONE', #124536, #141512 ) ;
#13602 = VECTOR ( 'NONE', #31697, 999.9999999999998863 ) ;
#13603 = AXIS2_PLACEMENT_3D ( 'NONE', #30237, #5609, #73747 ) ;
#13604 = SURFACE_SIDE_STYLE ('',( #91225 ) ) ;
#13605 = FACE_OUTER_BOUND ( 'NONE', #23511, .T. ) ;
#13606 = CARTESIAN_POINT ( 'NONE',  ( 30.48921356237309510, -27.52281430457076894, 5.000000000000000000 ) ) ;
#13607 = PRESENTATION_STYLE_ASSIGNMENT (( #113649 ) ) ;
#13608 = EDGE_CURVE ( 'NONE', #118125, #129576, #26627, .T. ) ;
#13609 = ORIENTED_EDGE ( 'NONE', *, *, #72650, .F. ) ;
#13610 = VERTEX_POINT ( 'NONE', #25914 ) ;
#13611 = CARTESIAN_POINT ( 'NONE',  ( 9.604862331875157366, 21.75929247661549937, 21.32995629748184641 ) ) ;
#13612 = ORIENTED_EDGE ( 'NONE', *, *, #74131, .F. ) ;
#13613 = ORIENTED_EDGE ( 'NONE', *, *, #44700, .T. ) ;
#13614 = VECTOR ( 'NONE', #106400, 1000.000000000000227 ) ;
#13615 = ADVANCED_FACE ( 'NONE', ( #59982 ), #22447, .F. ) ;
#13616 = VECTOR ( 'NONE', #141047, 1000.000000000000000 ) ;
#13618 = EDGE_CURVE ( 'NONE', #77659, #39354, #49836, .T. ) ;
#13617 = DIRECTION ( 'NONE',  ( 0.7071067811865487940, 0.7071067811865463515, 0.000000000000000000 ) ) ;
#13619 = EDGE_LOOP ( 'NONE', ( #72457, #112296, #96719, #111880 ) ) ;
#13620 = DIRECTION ( 'NONE',  ( -0.000000000000000000, 0.3543493200069153248, 0.9351131265310292928 ) ) ;
#13621 = CARTESIAN_POINT ( 'NONE',  ( -21.18398860626899349, 28.73617430169802134, 5.000000000000000000 ) ) ;
#13622 = DIRECTION ( 'NONE',  ( -0.6830127018922180770, -0.6830127018922204085, -0.2588190451025213501 ) ) ;
#13623 = VECTOR ( 'NONE', #30513, 999.9999999999998863 ) ;
#13624 = CARTESIAN_POINT ( 'NONE',  ( 12.32816939922344623, 5.259292476615662792, 4.000000000000000000 ) ) ;
#13625 = ORIENTED_EDGE ( 'NONE', *, *, #6036, .T. ) ;
#13626 = CIRCLE ( 'NONE', #94561, 2.500000000000000888 ) ;
#13627 =( LENGTH_UNIT ( ) NAMED_UNIT ( * ) SI_UNIT ( .MILLI., .METRE. ) );
#13628 = DIRECTION ( 'NONE',  ( 0.7071067811865487940, 0.7071067811865463515, 0.000000000000000000 ) ) ;
#13629 = VECTOR ( 'NONE', #2645, 1000.000000000000000 ) ;
#13630 = VERTEX_POINT ( 'NONE', #48375 ) ;
#13631 = DIRECTION ( 'NONE',  ( -1.000000000000000000, -1.224606353822377258E-16, -0.000000000000000000 ) ) ;
#13632 = VERTEX_POINT ( 'NONE', #111975 ) ;
#13633 = DIRECTION ( 'NONE',  ( 0.7071067811865487940, 0.7071067811865463515, 0.000000000000000000 ) ) ;
#13634 = EDGE_CURVE ( 'NONE', #3834, #52633, #12630, .T. ) ;
#13635 = EDGE_LOOP ( 'NONE', ( #52720, #114237, #83354, #142087, #36125, #29417 ) ) ;
#13636 = CARTESIAN_POINT ( 'NONE',  ( -26.70025512860841488, -27.71228299555187391, 4.000000000000000000 ) ) ;
#13637 = ORIENTED_EDGE ( 'NONE', *, *, #59101, .T. ) ;
#13638 = VERTEX_POINT ( 'NONE', #24242 ) ;
#13639 = AXIS2_PLACEMENT_3D ( 'NONE', #121768, #22444, #10851 ) ;
#13640 = ORIENTED_EDGE ( 'NONE', *, *, #106487, .T. ) ;
#13641 = AXIS2_PLACEMENT_3D ( 'NONE', #70418, #106519, #116719 ) ;
#13642 = CARTESIAN_POINT ( 'NONE',  ( 94.47916666666665719, -7.950000000000000178, 2.130196079827424427 ) ) ;
#13643 = CARTESIAN_POINT ( 'NONE',  ( 20.46247294953710849, -7.464222240803106570E-16, -6.094999999999989981 ) ) ;
#13644 = CARTESIAN_POINT ( 'NONE',  ( 116.9587635252314470, 0.000000000000000000, -6.110000000000001208 ) ) ;
#13645 = CARTESIAN_POINT ( 'NONE',  ( 24.48921356237309510, -27.52281430457072631, 5.000000000000000000 ) ) ;
#13646 = CARTESIAN_POINT ( 'NONE',  ( 24.48921356237309510, -27.52281430457072631, 5.000000000000000000 ) ) ;
#13647 = CARTESIAN_POINT ( 'NONE',  ( 3.398789304146613954, 4.202752102959690472E-16, 0.000000000000000000 ) ) ;
#13648 = FACE_OUTER_BOUND ( 'NONE', #17279, .T. ) ;
#13649 = DIRECTION ( 'NONE',  ( -0.6830127018922181881, 0.6830127018922202975, -0.2588190451025214056 ) ) ;
#13650 = ORIENTED_EDGE ( 'NONE', *, *, #63274, .T. ) ;
#13651 = CARTESIAN_POINT ( 'NONE',  ( 32.20710678118632586, -17.24070752338411339, 5.000000000000000000 ) ) ;
#13652 = ORIENTED_EDGE ( 'NONE', *, *, #82126, .F. ) ;
#13653 = ORIENTED_EDGE ( 'NONE', *, *, #110640, .F. ) ;
#13654 = CARTESIAN_POINT ( 'NONE',  ( 0.2997448713915885632, -27.71228299555206220, 4.000000000000000000 ) ) ;
#13655 = ORIENTED_EDGE ( 'NONE', *, *, #49894, .T. ) ;
#13656 = DIRECTION ( 'NONE',  ( 0.6830127018922180770, -0.6830127018922204085, -0.2588190451025213501 ) ) ;
#13657 = LINE ( 'NONE', #55789, #61718 ) ;
#13658 = LINE ( 'NONE', #46366, #3218 ) ;
#13659 = CARTESIAN_POINT ( 'NONE',  ( 6.183988606268994381, 28.73617430169791476, 5.000000000000000000 ) ) ;
#13660 = ORIENTED_EDGE ( 'NONE', *, *, #10590, .T. ) ;
#13661 = ORIENTED_EDGE ( 'NONE', *, *, #82583, .F. ) ;
#13662 = CARTESIAN_POINT ( 'NONE',  ( 0.000000000000000000, 0.000000000000000000, 5.000000000000000000 ) ) ;
#13663 = EDGE_CURVE ( 'NONE', #96600, #136985, #46013, .T. ) ;
#13664 = CARTESIAN_POINT ( 'NONE',  ( 33.02540314143521272, 2.126176841940962348, 7.934999999999989839 ) ) ;
#13665 = ORIENTED_EDGE ( 'NONE', *, *, #35492, .F. ) ;
#13666 = ADVANCED_FACE ( 'NONE', ( #24932 ), #25653, .F. ) ;
#13667 = LINE ( 'NONE', #90563, #64428 ) ;
#13668 = LINE ( 'NONE', #91969, #139147 ) ;
#13669 = EDGE_LOOP ( 'NONE', ( #93020, #21787, #28289, #87597 ) ) ;
#13670 = ORIENTED_EDGE ( 'NONE', *, *, #86033, .T. ) ;
#13671 = EDGE_CURVE ( 'NONE', #59338, #96891, #133028, .T. ) ;
#13672 = ORIENTED_EDGE ( 'NONE', *, *, #56935, .T. ) ;
#13673 = LINE ( 'NONE', #91299, #137555 ) ;
#13674 = CARTESIAN_POINT ( 'NONE',  ( -30.18398860626900060, 28.73617430169808173, 5.000000000000000000 ) ) ;
#13675 = CARTESIAN_POINT ( 'NONE',  ( -63.29974487139158867, -27.71228299555250274, 4.000000000000000000 ) ) ;
#13676 = EDGE_CURVE ( 'NONE', #83993, #46474, #9918, .T. ) ;
#13677 = FACE_OUTER_BOUND ( 'NONE', #5112, .T. ) ;
#13678 = VERTEX_POINT ( 'NONE', #79380 ) ;
#13679 = CARTESIAN_POINT ( 'NONE',  ( -5.999999999999951150, -3.412538124160721331, 4.000000000000000000 ) ) ;
#13680 = ADVANCED_FACE ( 'NONE', ( #56899 ), #1720, .F. ) ;
#13681 = DIRECTION ( 'NONE',  ( -0.000000000000000000, 0.3543493200069153248, 0.9351131265310292928 ) ) ;
#13682 = LINE ( 'NONE', #70293, #113948 ) ;
#13683 = ORIENTED_EDGE ( 'NONE', *, *, #110874, .F. ) ;
#13684 = PRESENTATION_LAYER_ASSIGNMENT (  '', '', ( #39178 ) ) ;
#13685 = VECTOR ( 'NONE', #137254, 1000.000000000000000 ) ;
#13686 = AXIS2_PLACEMENT_3D ( 'NONE', #24693, #89249, #68254 ) ;
#13687 = VECTOR ( 'NONE', #16242, 999.9999999999998863 ) ;
#13688 = DIRECTION ( 'NONE',  ( 0.000000000000000000, 0.000000000000000000, -1.000000000000000000 ) ) ;
#13689 = ORIENTED_EDGE ( 'NONE', *, *, #26821, .F. ) ;
#13690 = CIRCLE ( 'NONE', #110959, 1.000000000000000888 ) ;
#13691 = ADVANCED_FACE ( 'NONE', ( #91634 ), #102533, .F. ) ;
#13692 = VERTEX_POINT ( 'NONE', #44609 ) ;
#13693 = ORIENTED_EDGE ( 'NONE', *, *, #97063, .T. ) ;
#13694 = EDGE_CURVE ( 'NONE', #14168, #74087, #114099, .T. ) ;
#13695 = PLANE ( 'NONE',  #128026 ) ;
#13696 = LINE ( 'NONE', #34784, #110880 ) ;
#13697 = ORIENTED_EDGE ( 'NONE', *, *, #121089, .T. ) ;
#13698 = COLOUR_RGB ( '', 0.40784314, 0.44705882, 0.49803922) ;
#13699 = ORIENTED_EDGE ( 'NONE', *, *, #81396, .T. ) ;
#13700 = EDGE_CURVE ( 'NONE', #32075, #79314, #108125, .T. ) ;
#13701 = CARTESIAN_POINT ( 'NONE',  ( 30.29974487139158867, -27.71228299555227537, 4.000000000000000000 ) ) ;
#13702 = LINE ( 'NONE', #57994, #55504 ) ;
#13703 = CARTESIAN_POINT ( 'NONE',  ( -20.99451991528748707, 28.92564299267952777, 4.000000000000000000 ) ) ;
#13704 =( BOUNDED_CURVE ( )  B_SPLINE_CURVE ( 3, ( #108421, #140378, #9099, #51962 ),
 .UNSPECIFIED., .F., .T. ) 
 B_SPLINE_CURVE_WITH_KNOTS ( ( 4, 4 ),
 ( 5.106027341939279651, 6.645403452391245303 ),
 .UNSPECIFIED. ) 
 CURVE ( )  GEOMETRIC_REPRESENTATION_ITEM ( )  RATIONAL_B_SPLINE_CURVE ( ( 1.000000000000000000, 0.8120851936182276187, 0.8120851936182276187, 1.000000000000000000 ) ) 
 REPRESENTATION_ITEM ( '' )  );
#13705 = LINE ( 'NONE', #2848, #21097 ) ;
#13706 = CARTESIAN_POINT ( 'NONE',  ( 33.48921356237309510, -27.52281430457078670, 5.000000000000000000 ) ) ;
#13707 = CARTESIAN_POINT ( 'NONE',  ( -4.499999999999962697, -4.533600742197694267, 5.000000000000000000 ) ) ;
#13708 = CARTESIAN_POINT ( 'NONE',  ( 15.70710678118643422, -12.74070752338415424, 5.000000000000000000 ) ) ;
#13709 = CARTESIAN_POINT ( 'NONE',  ( 22.87456980810188867, 6.871911579029510442, -3.967499999999998916 ) ) ;
#13711 = STYLED_ITEM ( 'NONE', ( #77425 ), #47657 ) ;
#13710 = CARTESIAN_POINT ( 'NONE',  ( 0.8537364747685527444, -5.808823158059035485, -5.808823158059033709 ) ) ;
#13712 = CARTESIAN_POINT ( 'NONE',  ( 0.000000000000000000, 0.000000000000000000, 5.000000000000000000 ) ) ;
#13713 = VECTOR ( 'NONE', #76362, 999.9999999999998863 ) ;
#13714 = DIRECTION ( 'NONE',  ( -0.6830127018922181881, 0.6830127018922202975, -0.2588190451025214056 ) ) ;
#13715 = LINE ( 'NONE', #15833, #19949 ) ;
#13716 = VERTEX_POINT ( 'NONE', #59057 ) ;
#13717 = VERTEX_POINT ( 'NONE', #135855 ) ;
#13718 = CARTESIAN_POINT ( 'NONE',  ( 93.60416666666665719, 2.130196079827422206, 7.950000000000001954 ) ) ;
#13719 = VERTEX_POINT ( 'NONE', #36538 ) ;
#13720 = EDGE_LOOP ( 'NONE', ( #123956, #34169, #70523, #112338, #38011, #3316 ) ) ;
#13721 = ORIENTED_EDGE ( 'NONE', *, *, #39600, .T. ) ;
#13722 = ADVANCED_FACE ( 'NONE', ( #111219 ), #45694, .T. ) ;
#13723 = CARTESIAN_POINT ( 'NONE',  ( 5.443598275411213550, 0.000000000000000000, 2.500000000000000444 ) ) ;
#13724 = DIRECTION ( 'NONE',  ( 0.3543493200069162685, -0.000000000000000000, -0.9351131265310288487 ) ) ;
#13725 = CARTESIAN_POINT ( 'NONE',  ( 10.32500000000000107, 8.432637487761466488, 4.375000000000001776 ) ) ;
#13726 = EDGE_LOOP ( 'NONE', ( #44913, #5156, #131253, #108157 ) ) ;
#13727 = VECTOR ( 'NONE', #51617, 1000.000000000000000 ) ;
#13728 = CARTESIAN_POINT ( 'NONE',  ( 14.99999999999989342, -16.60178936734447319, 0.8616154019347853632 ) ) ;
#13729 = AXIS2_PLACEMENT_3D ( 'NONE', #106239, #96777, #95391 ) ;
#13730 = CARTESIAN_POINT ( 'NONE',  ( 26.99999999999981171, 17.96639925780207747, 5.000000000000000000 ) ) ;
#13731 = AXIS2_PLACEMENT_3D ( 'NONE', #121059, #100045, #119609 ) ;
#13732 = CARTESIAN_POINT ( 'NONE',  ( 10.99806943317893726, -22.22500000000000142, 4.500000000000000888 ) ) ;
#13733 = CARTESIAN_POINT ( 'NONE',  ( 14.60438740478481989, -0.8081507193758268315, 4.000000000000000000 ) ) ;
#13734 = LINE ( 'NONE', #134867, #67261 ) ;
#13735 = DIRECTION ( 'NONE',  ( 1.734723475976806848E-16, -1.000000000000000000, 0.000000000000000000 ) ) ;
#13736 = DIRECTION ( 'NONE',  ( 0.6830127018922180770, -0.6830127018922204085, -0.2588190451025213501 ) ) ;
#13737 = VECTOR ( 'NONE', #35356, 1000.000000000000227 ) ;
#13738 = CARTESIAN_POINT ( 'NONE',  ( 27.79289321881326913, -11.24070752338417023, 5.000000000000000000 ) ) ;
#13739 = CARTESIAN_POINT ( 'NONE',  ( -29.99451991528749417, 28.92564299267958816, 4.000000000000000000 ) ) ;
#13740 = CARTESIAN_POINT ( 'NONE',  ( -9.183988606268997046, 28.73617430169793607, 5.000000000000000000 ) ) ;
#13741 = CIRCLE ( 'NONE', #39010, 2.247899999999996901 ) ;
#13742 = DIRECTION ( 'NONE',  ( 1.000000000000000000, 1.224606353822377258E-16, 0.000000000000000000 ) ) ;
#13743 = EDGE_CURVE ( 'NONE', #131560, #115494, #19318, .T. ) ;
#13744 = CARTESIAN_POINT ( 'NONE',  ( 53.19685992802467212, -48.66302742222553945, 38.53170190052308186 ) ) ;
#13745 = VERTEX_POINT ( 'NONE', #42530 ) ;
#13746 = ORIENTED_EDGE ( 'NONE', *, *, #135892, .F. ) ;
#13747 = CARTESIAN_POINT ( 'NONE',  ( 108.2087635252314470, -7.482591942790329030E-16, 6.110000000000001208 ) ) ;
#13748 = ORIENTED_EDGE ( 'NONE', *, *, #2885, .T. ) ;
#13749 = ADVANCED_FACE ( 'NONE', ( #64987 ), #107028, .T. ) ;
#13750 = FACE_OUTER_BOUND ( 'NONE', #80209, .T. ) ;
#13751 = COLOUR_RGB ( '', 0.09019608, 0.27058824, 0.51372549) ;
#13752 = PLANE ( 'NONE',  #66531 ) ;
#13753 = PLANE ( 'NONE',  #5029 ) ;
#13754 = LINE ( 'NONE', #102242, #23432 ) ;
#13755 = CARTESIAN_POINT ( 'NONE',  ( 114.2454301918981230, -5.291415217122918513, -3.055000000000000160 ) ) ;
#13756 = ORIENTED_EDGE ( 'NONE', *, *, #110874, .T. ) ;
#13757 = EDGE_CURVE ( 'NONE', #61398, #108329, #94284, .T. ) ;
#13758 = ORIENTED_EDGE ( 'NONE', *, *, #17622, .T. ) ;
#13759 = LINE ( 'NONE', #74975, #105388 ) ;
#13760 = CARTESIAN_POINT ( 'NONE',  ( 97.68750000000000000, -5.819803920172573974, 5.819803920172573086 ) ) ;
#13761 = ORIENTED_EDGE ( 'NONE', *, *, #14537, .T. ) ;
#13762 = ORIENTED_EDGE ( 'NONE', *, *, #114405, .F. ) ;
#13763 = EDGE_CURVE ( 'NONE', #2262, #118592, #30183, .T. ) ;
#13764 = ORIENTED_EDGE ( 'NONE', *, *, #22522, .T. ) ;
#13765 = DIRECTION ( 'NONE',  ( 0.6830127018922180770, -0.6830127018922204085, -0.2588190451025213501 ) ) ;
#13766 = CARTESIAN_POINT ( 'NONE',  ( -24.18398860626899705, 28.73617430169804265, 5.000000000000000000 ) ) ;
#13767 =( BOUNDED_CURVE ( )  B_SPLINE_CURVE ( 3, ( #111235, #142474, #9790, #65665 ),
 .UNSPECIFIED., .F., .T. ) 
 B_SPLINE_CURVE_WITH_KNOTS ( ( 4, 4 ),
 ( 2.779374508378134045, 4.199602562396876237 ),
 .UNSPECIFIED. ) 
 CURVE ( )  GEOMETRIC_REPRESENTATION_ITEM ( )  RATIONAL_B_SPLINE_CURVE ( ( 1.000000000000000000, 0.8388583629366543892, 0.8388583629366543892, 1.000000000000000000 ) ) 
 REPRESENTATION_ITEM ( '' )  );
#13768 = CARTESIAN_POINT ( 'NONE',  ( 30.68293019189811943, -1.637169565754158951, -6.109999999999998543 ) ) ;
#13769 = ORIENTED_EDGE ( 'NONE', *, *, #29455, .F. ) ;
#13770 = ORIENTED_EDGE ( 'NONE', *, *, #39705, .T. ) ;
#13771 = CARTESIAN_POINT ( 'NONE',  ( 45.18398860626900415, 28.73617430169818832, 5.000000000000000000 ) ) ;
#13772 = EDGE_LOOP ( 'NONE', ( #52358, #46249, #62574, #29205 ) ) ;
#13773 = ORIENTED_EDGE ( 'NONE', *, *, #90997, .F. ) ;
#13774 = VERTEX_POINT ( 'NONE', #86001 ) ;
#13775 = PLANE ( 'NONE',  #70291 ) ;
#13776 = LINE ( 'NONE', #100821, #75343 ) ;
#13777 = CARTESIAN_POINT ( 'NONE',  ( 23.99999999999983302, -15.41253812416059432, 4.000000000000000000 ) ) ;
#13778 = EDGE_CURVE ( 'NONE', #125758, #22428, #74433, .T. ) ;
#13779 = ORIENTED_EDGE ( 'NONE', *, *, #76318, .F. ) ;
#13780 = CARTESIAN_POINT ( 'NONE',  ( 13.49999999999990585, 18.43112307739199451, 4.000000000000000000 ) ) ;
#13781 = AXIS2_PLACEMENT_3D ( 'NONE', #73041, #81778, #4837 ) ;
#13782 = DIRECTION ( 'NONE',  ( -0.6830127018922180770, 0.6830127018922202975, -0.2588190451025213501 ) ) ;
#13783 = VECTOR ( 'NONE', #8638, 1000.000000000000000 ) ;
#13784 = VECTOR ( 'NONE', #66157, 999.9999999999998863 ) ;
#13785 = VECTOR ( 'NONE', #124076, 1000.000000000000227 ) ;
#13786 = PLANE ( 'NONE',  #11964 ) ;
#13787 = VECTOR ( 'NONE', #11126, 1000.000000000000000 ) ;
#13788 = EDGE_CURVE ( 'NONE', #53159, #36944, #75853, .T. ) ;
#13789 = FACE_BOUND ( 'NONE', #134068, .T. ) ;
#13790 = ORIENTED_EDGE ( 'NONE', *, *, #52154, .F. ) ;
#13791 = CARTESIAN_POINT ( 'NONE',  ( 63.80836038379621300, 7.949999999999996625, 2.130196079827431088 ) ) ;
#13792 = CARTESIAN_POINT ( 'NONE',  ( 25.97159235450331849, 9.902892378096218942E-16, 0.000000000000000000 ) ) ;
#13793 = FACE_OUTER_BOUND ( 'NONE', #115971, .T. ) ;
#13794 = EDGE_CURVE ( 'NONE', #111985, #121113, #13704, .T. ) ;
#13795 = VERTEX_POINT ( 'NONE', #109176 ) ;
#13796 = CARTESIAN_POINT ( 'NONE',  ( 14.51078643762690490, -27.52281430457045275, 5.000000000000000000 ) ) ;
#13797 = ORIENTED_EDGE ( 'NONE', *, *, #45160, .F. ) ;
#13798 = VERTEX_POINT ( 'NONE', #120017 ) ;
#13799 = VECTOR ( 'NONE', #34790, 999.9999999999998863 ) ;
#13800 = ORIENTED_EDGE ( 'NONE', *, *, #139176, .T. ) ;
#13801 = CARTESIAN_POINT ( 'NONE',  ( 42.64126352523145158, 4.472830434245835818, 4.472830434245840259 ) ) ;
#13802 = ORIENTED_EDGE ( 'NONE', *, *, #7910, .F. ) ;
#13803 = CONICAL_SURFACE ( 'NONE', #85523, 2.500000000000000444, 0.9599310885968830309 ) ;
#13804 = DIRECTION ( 'NONE',  ( -0.6830127018922181881, 0.6830127018922202975, -0.2588190451025214056 ) ) ;
#13805 = LINE ( 'NONE', #102301, #7977 ) ;
#13806 = VERTEX_POINT ( 'NONE', #76582 ) ;
#13807 = FACE_OUTER_BOUND ( 'NONE', #54293, .T. ) ;
#13808 = CARTESIAN_POINT ( 'NONE',  ( -2.700255128608413990, -27.71228299555204089, 4.000000000000000000 ) ) ;
#13809 = AXIS2_PLACEMENT_3D ( 'NONE', #35554, #12318, #44268 ) ;
#13810 = ADVANCED_FACE ( 'NONE', ( #54820 ), #41790, .F. ) ;
#13811 = VECTOR ( 'NONE', #120744, 1000.000000000000227 ) ;
#13812 = CARTESIAN_POINT ( 'NONE',  ( 13.99806943317892127, -22.22500000000000142, 4.500000000000000888 ) ) ;
#13813 = LINE ( 'NONE', #79869, #30097 ) ;
#13814 = DIRECTION ( 'NONE',  ( 0.7071067811865486830, -0.7071067811865464625, -0.000000000000000000 ) ) ;
#13815 = CARTESIAN_POINT ( 'NONE',  ( -33.87485380690745274, -14.24070752338413826, 9.401115078912734901 ) ) ;
#13816 = VERTEX_POINT ( 'NONE', #96141 ) ;
#13817 = VERTEX_POINT ( 'NONE', #119322 ) ;
#13818 = ORIENTED_EDGE ( 'NONE', *, *, #20026, .F. ) ;
#13819 = ORIENTED_EDGE ( 'NONE', *, *, #40600, .T. ) ;
#13820 = CIRCLE ( 'NONE', #124995, 2.999999999999999556 ) ;
#13821 = CARTESIAN_POINT ( 'NONE',  ( -12.48921356237309155, -27.52281430457064104, 5.000000000000000000 ) ) ;
#13822 = VERTEX_POINT ( 'NONE', #53367 ) ;
#13823 = VECTOR ( 'NONE', #34258, 1000.000000000000000 ) ;
#13824 = COLOUR_RGB ( '', 0.40784314, 0.44705882, 0.49803922) ;
#13825 = ORIENTED_EDGE ( 'NONE', *, *, #44319, .T. ) ;
#13826 = DIRECTION ( 'NONE',  ( -1.000000000000000000, 0.000000000000000000, 0.000000000000000000 ) ) ;
#13827 = FACE_OUTER_BOUND ( 'NONE', #135918, .T. ) ;
#13828 = CIRCLE ( 'NONE', #20784, 2.055000000000000604 ) ;
#13829 = PLANE ( 'NONE',  #16161 ) ;
#13830 = ORIENTED_EDGE ( 'NONE', *, *, #64145, .T. ) ;
#13831 = VECTOR ( 'NONE', #56247, 1000.000000000000000 ) ;
#13832 = DIRECTION ( 'NONE',  ( 0.7071067811865486830, -0.7071067811865464625, -0.000000000000000000 ) ) ;
#13833 = EDGE_LOOP ( 'NONE', ( #98500, #8954, #110647, #33143, #86737 ) ) ;
#13834 = CARTESIAN_POINT ( 'NONE',  ( -27.29974487139158512, -27.71228299555225405, 4.000000000000000000 ) ) ;
#13835 = CARTESIAN_POINT ( 'NONE',  ( 29.08790314143522338, 6.871911579029515771, 3.967499999999989146 ) ) ;
#13836 = EDGE_CURVE ( 'NONE', #84892, #51683, #141830, .T. ) ;
#13837 = CARTESIAN_POINT ( 'NONE',  ( 2.546236474768552860, -7.934999999999990727, 4.858786175617117713E-16 ) ) ;
#13838 = ORIENTED_EDGE ( 'NONE', *, *, #22975, .T. ) ;
#13840 = LINE ( 'NONE', #122622, #52241 ) ;
#13839 = CARTESIAN_POINT ( 'NONE',  ( 112.2037635252314516, 6.109999999999999432, 1.122388791418549108E-15 ) ) ;
#13841 = ADVANCED_FACE ( 'NONE', ( #142542 ), #87445, .T. ) ;
#13842 = DIRECTION ( 'NONE',  ( 0.000000000000000000, 0.06845965770171351383, 0.9976538855070752332 ) ) ;
#13843 = FACE_OUTER_BOUND ( 'NONE', #118527, .T. ) ;
#13844 = ORIENTED_EDGE ( 'NONE', *, *, #51208, .F. ) ;
#13845 = CARTESIAN_POINT ( 'NONE',  ( 8.671830600776411657, 8.259292476615629042, 4.000000000000000000 ) ) ;
#13847 = ORIENTED_EDGE ( 'NONE', *, *, #101241, .T. ) ;
#13846 = DIRECTION ( 'NONE',  ( -0.000000000000000000, -0.000000000000000000, 1.000000000000000000 ) ) ;
#13848 = CARTESIAN_POINT ( 'NONE',  ( 5.999999999999967137, 2.966399257802236011, 5.000000000000000000 ) ) ;
#13849 = DIRECTION ( 'NONE',  ( -0.000000000000000000, -0.3543493200069152693, 0.9351131265310292928 ) ) ;
#13850 = PLANE ( 'NONE',  #111809 ) ;
#13851 = EDGE_CURVE ( 'NONE', #106463, #76190, #117444, .T. ) ;
#13852 = EDGE_CURVE ( 'NONE', #93313, #129006, #130958, .T. ) ;
#13853 = DIRECTION ( 'NONE',  ( 0.000000000000000000, 0.000000000000000000, 1.000000000000000000 ) ) ;
#13854 = VERTEX_POINT ( 'NONE', #85269 ) ;
#13855 = FACE_OUTER_BOUND ( 'NONE', #19886, .T. ) ;
#13856 = CARTESIAN_POINT ( 'NONE',  ( -10.17183060077640100, 0.7592924766157104211, 4.000000000000000000 ) ) ;
#13857 = LINE ( 'NONE', #110316, #46752 ) ;
#13858 = ORIENTED_EDGE ( 'NONE', *, *, #105191, .T. ) ;
#13859 = VECTOR ( 'NONE', #35825, 1000.000000000000000 ) ;
#13860 = DIRECTION ( 'NONE',  ( 0.7071067811865487940, 0.7071067811865463515, 0.000000000000000000 ) ) ;
#13861 = ORIENTED_EDGE ( 'NONE', *, *, #125979, .T. ) ;
#13862 = EDGE_CURVE ( 'NONE', #13457, #109156, #110512, .T. ) ;
#13864 = EDGE_LOOP ( 'NONE', ( #84773, #36004, #128833, #14992, #119305 ) ) ;
#13863 = CARTESIAN_POINT ( 'NONE',  ( -18.29974487139159223, -27.71228299555219010, 4.000000000000000000 ) ) ;
#13865 = EDGE_CURVE ( 'NONE', #64348, #91540, #132404, .T. ) ;
#13866 = ORIENTED_EDGE ( 'NONE', *, *, #83858, .F. ) ;
#13867 = DIRECTION ( 'NONE',  ( -1.000000000000000000, -1.224606353822377258E-16, -0.000000000000000000 ) ) ;
#13868 = FACE_OUTER_BOUND ( 'NONE', #82604, .T. ) ;
#13870 = ORIENTED_EDGE ( 'NONE', *, *, #16097, .F. ) ;
#13869 = STYLED_ITEM ( 'NONE', ( #112173 ), #75511 ) ;
#13871 = VECTOR ( 'NONE', #81301, 1000.000000000000000 ) ;
#13872 = ADVANCED_FACE ( 'NONE', ( #18567 ), #62847, .F. ) ;
#13873 = CYLINDRICAL_SURFACE ( 'NONE', #1082, 3.000000000000000000 ) ;
#13874 = EDGE_LOOP ( 'NONE', ( #96226, #119790, #98107, #137963 ) ) ;
#13875 = CARTESIAN_POINT ( 'NONE',  ( 20.36747333860806819, 4.333342374871280669E-31, 2.500000000000000444 ) ) ;
#13876 = LINE ( 'NONE', #56751, #25879 ) ;
#13877 = FILL_AREA_STYLE_COLOUR ( '', #16934 ) ;
#13878 = EDGE_CURVE ( 'NONE', #81140, #63923, #66409, .T. ) ;
#13879 = CARTESIAN_POINT ( 'NONE',  ( 21.48921356237309155, -27.52281430457070499, 5.000000000000000000 ) ) ;
#13880 = PLANE ( 'NONE',  #103853 ) ;
#13881 = DIRECTION ( 'NONE',  ( 0.000000000000000000, 0.000000000000000000, 1.000000000000000000 ) ) ;
#13882 = DIRECTION ( 'NONE',  ( 1.000000000000000000, 0.000000000000000000, 0.000000000000000000 ) ) ;
#13883 = ORIENTED_EDGE ( 'NONE', *, *, #129444, .T. ) ;
#13884 = ORIENTED_EDGE ( 'NONE', *, *, #3784, .F. ) ;
#13885 = VERTEX_POINT ( 'NONE', #14133 ) ;
#13886 = CARTESIAN_POINT ( 'NONE',  ( 120.7291666666666572, 7.950000000000001954, -2.130196079827421762 ) ) ;
#13887 = AXIS2_PLACEMENT_3D ( 'NONE', #93389, #71653, #96215 ) ;
#13888 = ORIENTED_EDGE ( 'NONE', *, *, #33676, .F. ) ;
#13889 = VERTEX_POINT ( 'NONE', #79462 ) ;
#13890 = ORIENTED_EDGE ( 'NONE', *, *, #9300, .F. ) ;
#13891 = VECTOR ( 'NONE', #932, 1000.000000000000000 ) ;
#13892 = ADVANCED_FACE ( 'NONE', ( #89565 ), #91703, .F. ) ;
#13893 = CARTESIAN_POINT ( 'NONE',  ( -75.29974487139158157, -27.71228299555258445, 4.000000000000000000 ) ) ;
#13894 = DIRECTION ( 'NONE',  ( -0.7071067811865487940, 0.7071067811865463515, 0.000000000000000000 ) ) ;
#13895 = VECTOR ( 'NONE', #43633, 999.9999999999998863 ) ;
#13896 = VECTOR ( 'NONE', #123932, 1000.000000000000000 ) ;
#13897 = VECTOR ( 'NONE', #106563, 1000.000000000000227 ) ;
#13898 = ORIENTED_EDGE ( 'NONE', *, *, #42860, .T. ) ;
#13899 = CARTESIAN_POINT ( 'NONE',  ( 23.63159235450331863, 9.902892378096218942E-16, 0.000000000000000000 ) ) ;
#13900 = CARTESIAN_POINT ( 'NONE',  ( 66.18398860626901126, 28.73617430169833753, 5.000000000000000000 ) ) ;
#13901 = VECTOR ( 'NONE', #70, 1000.000000000000000 ) ;
#13902 = CARTESIAN_POINT ( 'NONE',  ( 30.48921356237309510, -27.52281430457076894, 5.000000000000000000 ) ) ;
#13903 = CARTESIAN_POINT ( 'NONE',  ( 4.637538124160942132, 22.22499999999999432, 4.000000000000000000 ) ) ;
#13904 = CARTESIAN_POINT ( 'NONE',  ( 110.3962635252314328, 4.472830434245840259, -4.472830434245839371 ) ) ;
#13905 = ORIENTED_EDGE ( 'NONE', *, *, #103565, .T. ) ;
#13906 = EDGE_CURVE ( 'NONE', #87654, #60505, #133795, .T. ) ;
#13907 = CARTESIAN_POINT ( 'NONE',  ( 18.18398860626898994, 28.73617430169800002, 5.000000000000000000 ) ) ;
#13908 = PLANE ( 'NONE',  #30702 ) ;
#13909 = DIRECTION ( 'NONE',  ( -0.7071067811865487940, 0.7071067811865463515, -0.000000000000000000 ) ) ;
#13910 = AXIS2_PLACEMENT_3D ( 'NONE', #26585, #103407, #4054 ) ;
#13911 = CARTESIAN_POINT ( 'NONE',  ( 34.92499999999998295, 20.18441419595452047, 5.773254242255883462 ) ) ;
#13912 = DIRECTION ( 'NONE',  ( 0.7071067811865486830, 0.7071067811865463515, 0.000000000000000000 ) ) ;
#13913 = DIRECTION ( 'NONE',  ( -0.7071067811865486830, -0.7071067811865464625, -0.000000000000000000 ) ) ;
#13914 = PLANE ( 'NONE',  #131494 ) ;
#13915 = CARTESIAN_POINT ( 'NONE',  ( 47.91252705046289151, -7.949999999999998401, -4.867971026610728450E-16 ) ) ;
#13916 = EDGE_CURVE ( 'NONE', #98260, #97996, #25007, .T. ) ;
#13917 = CARTESIAN_POINT ( 'NONE',  ( -34.92499999999997584, 22.27000000000000668, -7.752744394707050901 ) ) ;
#13918 = CARTESIAN_POINT ( 'NONE',  ( -28.21498419724172280, -3.740707523384244837, 15.76143240460117489 ) ) ;
#13919 = ORIENTED_EDGE ( 'NONE', *, *, #125652, .F. ) ;
#13920 = ORIENTED_EDGE ( 'NONE', *, *, #124626, .T. ) ;
#13921 = CARTESIAN_POINT ( 'NONE',  ( 35.70833333333332860, -3.974999999999999201, -6.884901960086287964 ) ) ;
#13922 = VERTEX_POINT ( 'NONE', #121475 ) ;
#13923 = FACE_OUTER_BOUND ( 'NONE', #8894, .T. ) ;
#13924 = VECTOR ( 'NONE', #128241, 999.9999999999998863 ) ;
#13925 = CARTESIAN_POINT ( 'NONE',  ( -39.18398860626899705, 28.73617430169814568, 5.000000000000000000 ) ) ;
#13926 = ORIENTED_EDGE ( 'NONE', *, *, #30115, .F. ) ;
#13927 = DIRECTION ( 'NONE',  ( -0.7071067811865487940, 0.7071067811865463515, 0.000000000000000000 ) ) ;
#13928 = DIRECTION ( 'NONE',  ( -1.000000000000000000, -0.000000000000000000, -0.000000000000000000 ) ) ;
#13929 = CIRCLE ( 'NONE', #57973, 2.055000000000000604 ) ;
#13930 = CARTESIAN_POINT ( 'NONE',  ( 36.02126352523142572, -4.472830434245839371, -4.472830434245840259 ) ) ;
#13931 = ORIENTED_EDGE ( 'NONE', *, *, #102531, .T. ) ;
#13932 = EDGE_CURVE ( 'NONE', #57920, #12358, #100457, .T. ) ;
#13933 = CIRCLE ( 'NONE', #83745, 25.00000000000002842 ) ;
#13934 = CARTESIAN_POINT ( 'NONE',  ( 1.042387978378689573, 0.3999999999999995781, 2.015694669338588429 ) ) ;
#13935 = VERTEX_POINT ( 'NONE', #12707 ) ;
#13936 = CARTESIAN_POINT ( 'NONE',  ( -7.499999999999944045, 22.22500000000000142, 4.362957392718792349 ) ) ;
#13937 = VECTOR ( 'NONE', #39083, 1000.000000000000000 ) ;
#13938 = DIRECTION ( 'NONE',  ( -1.000000000000000000, 0.000000000000000000, 0.000000000000000000 ) ) ;
#13939 = PLANE ( 'NONE',  #58056 ) ;
#13940 = CARTESIAN_POINT ( 'NONE',  ( 34.92499999999998295, 20.81665438641024224, 4.500000000000000888 ) ) ;
#13941 = ORIENTED_EDGE ( 'NONE', *, *, #138459, .F. ) ;
#13942 = EDGE_CURVE ( 'NONE', #119711, #131795, #46095, .T. ) ;
#13943 = ORIENTED_EDGE ( 'NONE', *, *, #92384, .T. ) ;
#13944 = VECTOR ( 'NONE', #50459, 1000.000000000000000 ) ;
#13945 = CARTESIAN_POINT ( 'NONE',  ( 38.43336038379621300, 2.130196079827431532, -7.949999999999996625 ) ) ;
#13946 = DIRECTION ( 'NONE',  ( 0.000000000000000000, 1.000000000000000000, -0.000000000000000000 ) ) ;
#13947 = DIRECTION ( 'NONE',  ( -0.7071067811865487940, 0.7071067811865463515, 0.000000000000000000 ) ) ;
#13948 = DIRECTION ( 'NONE',  ( 0.7071067811865486830, -0.7071067811865464625, -0.000000000000000000 ) ) ;
#13949 = DIRECTION ( 'NONE',  ( -0.7071067811865487940, 0.7071067811865463515, -0.000000000000000000 ) ) ;
#13950 = AXIS2_PLACEMENT_3D ( 'NONE', #115577, #138824, #113469 ) ;
#13951 = CARTESIAN_POINT ( 'NONE',  ( 54.18398860626899705, 28.73617430169825226, 5.000000000000000000 ) ) ;
#13952 = CARTESIAN_POINT ( 'NONE',  ( 54.45376352523144448, -6.109999999999998543, -3.741295971395162543E-16 ) ) ;
#13953 = CARTESIAN_POINT ( 'NONE',  ( -12.70000000000000462, -22.33999999999998565, 3.000000000000000000 ) ) ;
#13954 = CARTESIAN_POINT ( 'NONE',  ( -29.99999999999979394, -8.731860332648867740, -2.120594902707606533 ) ) ;
#13955 = VERTEX_POINT ( 'NONE', #11259 ) ;
#13956 = EDGE_CURVE ( 'NONE', #125316, #104580, #99722, .T. ) ;
#13957 = VERTEX_POINT ( 'NONE', #393 ) ;
#13958 = AXIS2_PLACEMENT_3D ( 'NONE', #29953, #107524, #108202 ) ;
#13959 = CARTESIAN_POINT ( 'NONE',  ( 7.171830600776422315, 0.7592924766157069794, 4.000000000000000000 ) ) ;
#13960 = ORIENTED_EDGE ( 'NONE', *, *, #124570, .F. ) ;
#13961 = CARTESIAN_POINT ( 'NONE',  ( 34.62665285692208528, 22.27000000000001023, -11.14529726906961749 ) ) ;
#13962 = ADVANCED_FACE ( 'NONE', ( #1108 ), #101867, .T. ) ;
#13963 = ORIENTED_EDGE ( 'NONE', *, *, #88550, .F. ) ;
#13964 = PLANE ( 'NONE',  #123314 ) ;
#13965 = LINE ( 'NONE', #26306, #80997 ) ;
#13966 = VECTOR ( 'NONE', #15097, 1000.000000000000227 ) ;
#13967 = DIRECTION ( 'NONE',  ( -0.6830127018922180770, -0.6830127018922204085, -0.2588190451025213501 ) ) ;
#13968 = EDGE_CURVE ( 'NONE', #142261, #115779, #3255, .T. ) ;
#13969 = FACE_BOUND ( 'NONE', #49679, .T. ) ;
#13970 = CARTESIAN_POINT ( 'NONE',  ( -29.99451991528749417, 28.92564299267958816, 4.000000000000000000 ) ) ;
#13971 = CARTESIAN_POINT ( 'NONE',  ( 25.39999999999999858, -5.520864266206504263E-14, -33.92499999999998295 ) ) ;
#13972 = EDGE_CURVE ( 'NONE', #41631, #42123, #69263, .T. ) ;
#13973 = CARTESIAN_POINT ( 'NONE',  ( 26.99451991528749417, 28.92564299267956685, 4.000000000000000000 ) ) ;
#13975 = ORIENTED_EDGE ( 'NONE', *, *, #39040, .F. ) ;
#13974 = CARTESIAN_POINT ( 'NONE',  ( -39.48921356237310221, -27.52281430457082934, 5.000000000000000000 ) ) ;
#13976 =( GEOMETRIC_REPRESENTATION_CONTEXT ( 3 ) GLOBAL_UNCERTAINTY_ASSIGNED_CONTEXT ( ( #49068 ) ) GLOBAL_UNIT_ASSIGNED_CONTEXT ( ( #46955, #124457, #1221 ) ) REPRESENTATION_CONTEXT ( 'NONE', 'WORKASPACE' ) );
#13978 = VERTEX_POINT ( 'NONE', #33787 ) ;
#13977 = VECTOR ( 'NONE', #116755, 1000.000000000000000 ) ;
#13979 = CARTESIAN_POINT ( 'NONE',  ( 9.060110710440143933, -9.740707523384184441, 10.89222023123378591 ) ) ;
#13980 = ORIENTED_EDGE ( 'NONE', *, *, #39549, .T. ) ;
#13981 = EDGE_LOOP ( 'NONE', ( #7963, #96249, #55701, #136259 ) ) ;
#13982 = CARTESIAN_POINT ( 'NONE',  ( 68.30793019189810877, -6.109999999999998543, 1.637169565754158507 ) ) ;
#13983 = VERTEX_POINT ( 'NONE', #67864 ) ;
#13984 = EDGE_CURVE ( 'NONE', #25649, #94899, #56338, .T. ) ;
#13985 = CARTESIAN_POINT ( 'NONE',  ( -51.48921356237309510, -27.52281430457091460, 5.000000000000000000 ) ) ;
#13986 = VERTEX_POINT ( 'NONE', #111303 ) ;
#13987 = DIRECTION ( 'NONE',  ( -0.000000000000000000, 0.3543493200069153248, 0.9351131265310292928 ) ) ;
#13988 = CIRCLE ( 'NONE', #76549, 3.000000000000002665 ) ;
#13989 = EDGE_CURVE ( 'NONE', #18457, #131858, #88882, .T. ) ;
#13990 =( BOUNDED_CURVE ( )  B_SPLINE_CURVE ( 2, ( #60755, #107057, #6265, #73718, #49854, #94031, #83924, #138270, #38954, #83177, #85288, #117196, #139725 ),
 .UNSPECIFIED., .F., .F. ) 
 B_SPLINE_CURVE_WITH_KNOTS ( ( 3, 2, 2, 2, 2, 2, 3 ),
 ( 0.7166666666666666741, 0.7194444444444444420, 0.7222222222222222099, 0.7249999999999999778, 0.7277777777777777457, 0.7305555555555555136, 0.7333333333333332815 ),
 .UNSPECIFIED. ) 
 CURVE ( )  GEOMETRIC_REPRESENTATION_ITEM ( )  RATIONAL_B_SPLINE_CURVE ( ( 1.000000000000000000, 0.9659258262890683122, 1.000000000000000000, 0.9659258262890683122, 1.000000000000000000, 0.9659258262890683122, 1.000000000000000000, 0.9659258262890683122, 1.000000000000000000, 0.9659258262890683122, 1.000000000000000000, 0.9659258262890683122, 1.000000000000000000 ) ) 
 REPRESENTATION_ITEM ( '' )  );
#13991 = CARTESIAN_POINT ( 'NONE',  ( 13.49999999999991829, -20.94781430457062044, 5.000000000000000000 ) ) ;
#13992 = CIRCLE ( 'NONE', #92758, 2.999999999999999112 ) ;
#13993 = DIRECTION ( 'NONE',  ( -0.7071067811865487940, -0.7071067811865463515, -0.000000000000000000 ) ) ;
#13994 = LINE ( 'NONE', #79330, #119943 ) ;
#13996 = FILL_AREA_STYLE_COLOUR ( '', #26405 ) ;
#13995 = LINE ( 'NONE', #92273, #92153 ) ;
#13997 = LINE ( 'NONE', #102483, #123426 ) ;
#13998 = LINE ( 'NONE', #12584, #53235 ) ;
#13999 = ORIENTED_EDGE ( 'NONE', *, *, #122910, .T. ) ;
#14000 = VECTOR ( 'NONE', #123188, 999.9999999999998863 ) ;
#14001 = AXIS2_PLACEMENT_3D ( 'NONE', #133909, #78829, #123039 ) ;
#14002 = EDGE_LOOP ( 'NONE', ( #133211, #43593, #38466, #106196 ) ) ;
#14003 = VECTOR ( 'NONE', #71941, 1000.000000000000000 ) ;
#14004 = DIRECTION ( 'NONE',  ( -0.5735764363510507113, 0.8191520442889885789, 1.003171929053520926E-16 ) ) ;
#14005 = FACE_OUTER_BOUND ( 'NONE', #112117, .T. ) ;
#14006 = ORIENTED_EDGE ( 'NONE', *, *, #13757, .T. ) ;
#14007 = VERTEX_POINT ( 'NONE', #77997 ) ;
#14008 = ORIENTED_EDGE ( 'NONE', *, *, #14768, .F. ) ;
#14009 = CARTESIAN_POINT ( 'NONE',  ( 29.31293019189811133, -1.637169565754159617, -6.110000000000001208 ) ) ;
#14010 = ORIENTED_EDGE ( 'NONE', *, *, #137772, .T. ) ;
#14011 = AXIS2_PLACEMENT_3D ( 'NONE', #71024, #84051, #17997 ) ;
#14012 = PLANE ( 'NONE',  #2260 ) ;
#14014 = EDGE_CURVE ( 'NONE', #133571, #11328, #58425, .T. ) ;
#14013 =( NAMED_UNIT ( * ) PLANE_ANGLE_UNIT ( ) SI_UNIT ( $, .RADIAN. ) );
#14015 = CARTESIAN_POINT ( 'NONE',  ( 0.2129031414352194063, 3.967499999999992699, -6.871911579029513994 ) ) ;
#14016 = EDGE_CURVE ( 'NONE', #22013, #108744, #53549, .T. ) ;
#14017 = CARTESIAN_POINT ( 'NONE',  ( -6.299744871391586898, -27.71228299555210484, 4.000000000000000000 ) ) ;
#14018 = ORIENTED_EDGE ( 'NONE', *, *, #48887, .F. ) ;
#14019 = CARTESIAN_POINT ( 'NONE',  ( -34.49999999999976552, -4.216083040037284846, -7.486842126848578083 ) ) ;
#14020 = EDGE_CURVE ( 'NONE', #96788, #120651, #122177, .T. ) ;
#14021 = DIRECTION ( 'NONE',  ( -0.000000000000000000, 0.3543493200069153248, 0.9351131265310292928 ) ) ;
#14022 = VECTOR ( 'NONE', #86837, 1000.000000000000000 ) ;
#14023 = LINE ( 'NONE', #135147, #31349 ) ;
#14025 = VERTEX_POINT ( 'NONE', #25733 ) ;
#14024 = DIRECTION ( 'NONE',  ( -0.6830127018922180770, -0.6830127018922204085, -0.2588190451025213501 ) ) ;
#14026 = EDGE_LOOP ( 'NONE', ( #130116, #8122, #5334, #107631 ) ) ;
#14027 = LINE ( 'NONE', #67011, #38090 ) ;
#14028 = CARTESIAN_POINT ( 'NONE',  ( -35.99451991528749772, 28.92564299267963079, 4.000000000000000000 ) ) ;
#14029 = EDGE_CURVE ( 'NONE', #35412, #110682, #16247, .T. ) ;
#14030 = EDGE_CURVE ( 'NONE', #37148, #21299, #114169, .T. ) ;
#14031 = LINE ( 'NONE', #114077, #118863 ) ;
#14032 = EDGE_LOOP ( 'NONE', ( #57574, #61078, #77249, #125256 ) ) ;
#14033 = VECTOR ( 'NONE', #29313, 1000.000000000000227 ) ;
#14034 = SURFACE_STYLE_FILL_AREA ( #80066 ) ;
#14035 = CARTESIAN_POINT ( 'NONE',  ( -17.99999999999987566, 20.70535890316559957, 1.956823837851957792 ) ) ;
#14036 = VECTOR ( 'NONE', #82159, 1000.000000000000000 ) ;
#14037 = AXIS2_PLACEMENT_3D ( 'NONE', #99486, #10346, #130742 ) ;
#14038 = CARTESIAN_POINT ( 'NONE',  ( 25.39999999999999858, 0.000000000000000000, 0.000000000000000000 ) ) ;
#14039 = DIRECTION ( 'NONE',  ( 0.3543493200069162685, -0.000000000000000000, -0.9351131265310288487 ) ) ;
#14040 = ORIENTED_EDGE ( 'NONE', *, *, #62124, .F. ) ;
#14041 = CARTESIAN_POINT ( 'NONE',  ( -24.79289321881327623, 6.759292476615645917, 5.000000000000000000 ) ) ;
#14043 = EDGE_CURVE ( 'NONE', #79351, #28576, #92400, .T. ) ;
#14042 = AXIS2_PLACEMENT_3D ( 'NONE', #125725, #59757, #58366 ) ;
#14044 = DIRECTION ( 'NONE',  ( -0.2399999999999971323, 0.000000000000000000, 0.9707728879609286432 ) ) ;
#14045 = DIRECTION ( 'NONE',  ( 0.6830127018922180770, -0.6830127018922204085, -0.2588190451025213501 ) ) ;
#14046 = CARTESIAN_POINT ( 'NONE',  ( 22.37176554955601659, -8.240707523384196875, 11.38925528200747372 ) ) ;
#14047 = EDGE_CURVE ( 'NONE', #57383, #100719, #114854, .T. ) ;
#14048 = CARTESIAN_POINT ( 'NONE',  ( 12.08840764549667668, 9.139736423841732040E-16, 0.000000000000000000 ) ) ;
#14049 = ORIENTED_EDGE ( 'NONE', *, *, #13048, .T. ) ;
#14050 = VECTOR ( 'NONE', #13345, 1000.000000000000000 ) ;
#14051 = EDGE_CURVE ( 'NONE', #84066, #116794, #15531, .T. ) ;
#14052 = VERTEX_POINT ( 'NONE', #37340 ) ;
#14053 = CARTESIAN_POINT ( 'NONE',  ( 127.0000000000000000, 0.000000000000000000, 0.000000000000000000 ) ) ;
#14054 = DIRECTION ( 'NONE',  ( -0.000000000000000000, -0.3543493200069152693, 0.9351131265310292928 ) ) ;
#14055 = FACE_OUTER_BOUND ( 'NONE', #70107, .T. ) ;
#14056 = DIRECTION ( 'NONE',  ( 0.000000000000000000, 0.000000000000000000, 1.000000000000000000 ) ) ;
#14057 = EDGE_CURVE ( 'NONE', #89964, #46947, #3931, .T. ) ;
#14058 = AXIS2_PLACEMENT_3D ( 'NONE', #86672, #106231, #32286 ) ;
#14059 = DIRECTION ( 'NONE',  ( -0.3543493200069162685, -0.000000000000000000, -0.9351131265310288487 ) ) ;
#14060 = DIRECTION ( 'NONE',  ( -0.7071067811865487940, -0.7071067811865463515, -0.000000000000000000 ) ) ;
#14061 = EDGE_CURVE ( 'NONE', #79922, #49159, #60547, .T. ) ;
#14062 = DIRECTION ( 'NONE',  ( 1.000000000000000000, 1.224606353822377258E-16, 0.000000000000000000 ) ) ;
#14063 = EDGE_LOOP ( 'NONE', ( #117598, #86310, #38216, #128693 ) ) ;
#14064 = DIRECTION ( 'NONE',  ( -0.000000000000000000, -0.3543493200069152693, 0.9351131265310292928 ) ) ;
#14065 = STYLED_ITEM ( 'NONE', ( #139314 ), #22381 ) ;
#14066 = LINE ( 'NONE', #26400, #118747 ) ;
#14067 = ADVANCED_FACE ( 'NONE', ( #26458 ), #138073, .F. ) ;
#14068 = LINE ( 'NONE', #68500, #27326 ) ;
#14069 = CARTESIAN_POINT ( 'NONE',  ( 55.18293019189810877, -1.637169565754159173, -6.109999999999999432 ) ) ;
#14070 = CARTESIAN_POINT ( 'NONE',  ( 183.7627343495646812, -51.96230815476841514, -39.57541490114648042 ) ) ;
#14071 = FILL_AREA_STYLE_COLOUR ( '', #90457 ) ;
#14072 = ORIENTED_EDGE ( 'NONE', *, *, #57791, .T. ) ;
#14073 = ORIENTED_EDGE ( 'NONE', *, *, #125143, .F. ) ;
#14074 = EDGE_CURVE ( 'NONE', #143369, #11170, #51073, .T. ) ;
#14075 = STYLED_ITEM ( 'NONE', ( #104240 ), #27794 ) ;
#14076 = DIRECTION ( 'NONE',  ( 1.000000000000000000, 1.224606353822377258E-16, 0.000000000000000000 ) ) ;
#14077 = CARTESIAN_POINT ( 'NONE',  ( 0.000000000000000000, 0.000000000000000000, 5.000000000000000000 ) ) ;
#14078 = CARTESIAN_POINT ( 'NONE',  ( 15.32816939922342669, 20.25929247661551358, 4.000000000000000000 ) ) ;
#14079 = CARTESIAN_POINT ( 'NONE',  ( 8.585466709768445170, 3.061616997868383634E-16, -2.500000000000000444 ) ) ;
#14080 = CARTESIAN_POINT ( 'NONE',  ( 17.22995720542194675, 21.73644205237997795, 5.000000000000000888 ) ) ;
#14081 = DIRECTION ( 'NONE',  ( 0.7071067811865487940, 0.7071067811865463515, -0.000000000000000000 ) ) ;
#14082 = VERTEX_POINT ( 'NONE', #117023 ) ;
#14083 = ORIENTED_EDGE ( 'NONE', *, *, #8361, .F. ) ;
#14084 = CARTESIAN_POINT ( 'NONE',  ( 68.99451991528748351, 28.92564299267986172, 4.000000000000000000 ) ) ;
#14085 = DIRECTION ( 'NONE',  ( -0.7071067811865487940, 0.7071067811865463515, 0.000000000000000000 ) ) ;
#14086 = UNCERTAINTY_MEASURE_WITH_UNIT (LENGTH_MEASURE( 1.000000000000000082E-05 ), #43043, 'distance_accuracy_value', 'NONE');
#14087 = EDGE_CURVE ( 'NONE', #22506, #2401, #13992, .T. ) ;
#14088 = VECTOR ( 'NONE', #123445, 999.9999999999998863 ) ;
#14089 = CARTESIAN_POINT ( 'NONE',  ( 0.000000000000000000, 0.000000000000000000, 5.000000000000000000 ) ) ;
#14090 = CARTESIAN_POINT ( 'NONE',  ( -34.47516574401892342, 12.02806734111569575, 4.998110765256835286 ) ) ;
#14091 = CARTESIAN_POINT ( 'NONE',  ( 75.18336038379624142, -2.130196079827426203, 7.949999999999997513 ) ) ;
#14093 = ADVANCED_FACE ( 'NONE', ( #17690 ), #71396, .F. ) ;
#14092 = CARTESIAN_POINT ( 'NONE',  ( 22.07159235450331991, 9.902892378096218942E-16, 0.000000000000000000 ) ) ;
#14094 = DIRECTION ( 'NONE',  ( 1.000000000000000000, 0.000000000000000000, 0.000000000000000000 ) ) ;
#14095 = ORIENTED_EDGE ( 'NONE', *, *, #108090, .F. ) ;
#14096 = CARTESIAN_POINT ( 'NONE',  ( 74.06249999999998579, -5.819803920172572198, -5.819803920172573086 ) ) ;
#14097 = DIRECTION ( 'NONE',  ( -0.6830127018922180770, -0.6830127018922204085, -0.2588190451025213501 ) ) ;
#14098 = CARTESIAN_POINT ( 'NONE',  ( -5.816011393731002066, 28.73617430169783304, 5.000000000000000000 ) ) ;
#14099 = CARTESIAN_POINT ( 'NONE',  ( 60.29974487139158867, -27.71228299555248142, 4.000000000000000000 ) ) ;
#14100 = ORIENTED_EDGE ( 'NONE', *, *, #6917, .T. ) ;
#14102 = EDGE_CURVE ( 'NONE', #102488, #10646, #5386, .T. ) ;
#14101 = VECTOR ( 'NONE', #113727, 1000.000000000000000 ) ;
#14103 = CARTESIAN_POINT ( 'NONE',  ( 9.618384906019905145, -2.240707523384264377, 13.37739548510237242 ) ) ;
#14104 = VECTOR ( 'NONE', #80898, 1000.000000000000000 ) ;
#14105 = AXIS2_PLACEMENT_3D ( 'NONE', #142028, #57885, #23044 ) ;
#14106 = FACE_OUTER_BOUND ( 'NONE', #101461, .T. ) ;
#14107 = CARTESIAN_POINT ( 'NONE',  ( 67.08376352523143282, -6.110000000000001208, -3.741295971395164515E-16 ) ) ;
#14108 = CARTESIAN_POINT ( 'NONE',  ( 37.58990935480144913, 9.759292476615621936, 11.28811694763787443 ) ) ;
#14109 = ORIENTED_EDGE ( 'NONE', *, *, #71373, .T. ) ;
#14111 = VERTEX_POINT ( 'NONE', #17007 ) ;
#14110 = VECTOR ( 'NONE', #34949, 999.9999999999998863 ) ;
#14112 = AXIS2_PLACEMENT_3D ( 'NONE', #31579, #8349, #75804 ) ;
#14113 = AXIS2_PLACEMENT_3D ( 'NONE', #70479, #95740, #84867 ) ;
#14114 = VECTOR ( 'NONE', #51601, 1000.000000000000227 ) ;
#14116 = DIRECTION ( 'NONE',  ( -0.7071067811865486830, -0.7071067811865464625, -0.000000000000000000 ) ) ;
#14115 = VECTOR ( 'NONE', #9562, 1000.000000000000227 ) ;
#14117 = CARTESIAN_POINT ( 'NONE',  ( 22.82816939922337696, 15.75929247661555976, 4.000000000000000000 ) ) ;
#14118 = LINE ( 'NONE', #88866, #122707 ) ;
#14119 = CARTESIAN_POINT ( 'NONE',  ( -2.999999999999979128, 16.55218569542900298, 5.000000000000000000 ) ) ;
#14121 = ORIENTED_EDGE ( 'NONE', *, *, #79753, .T. ) ;
#14120 = CARTESIAN_POINT ( 'NONE',  ( -4.499999999999976019, -9.462702396501018853, -9.474982329943506087 ) ) ;
#14122 = CARTESIAN_POINT ( 'NONE',  ( 9.748407645496676821, 9.139736423841732040E-16, 0.000000000000000000 ) ) ;
#14123 = DIRECTION ( 'NONE',  ( -1.000000000000000000, -1.224606353822377258E-16, -0.000000000000000000 ) ) ;
#14124 = CARTESIAN_POINT ( 'NONE',  ( -24.07469600201483928, -0.04978799960962446841, 4.760162856047368329 ) ) ;
#14125 = AXIS2_PLACEMENT_3D ( 'NONE', #51232, #15680, #40370 ) ;
#14126 = DIRECTION ( 'NONE',  ( -0.3543493200069162685, -0.000000000000000000, -0.9351131265310288487 ) ) ;
#14127 = EDGE_LOOP ( 'NONE', ( #42742, #105498, #86359, #59431 ) ) ;
#14128 = ORIENTED_EDGE ( 'NONE', *, *, #4066, .T. ) ;
#14129 = CARTESIAN_POINT ( 'NONE',  ( 58.04209685856477563, 5.291415217122923842, -3.054999999999996163 ) ) ;
#14130 = ORIENTED_EDGE ( 'NONE', *, *, #102636, .F. ) ;
#14131 = AXIS2_PLACEMENT_3D ( 'NONE', #102637, #70037, #70737 ) ;
#14132 = LINE ( 'NONE', #135245, #24478 ) ;
#14133 = CARTESIAN_POINT ( 'NONE',  ( 16.49999999999988276, -11.56887692260769640, 4.000000000000000000 ) ) ;
#14134 = DIRECTION ( 'NONE',  ( -0.7071067811865486830, -0.7071067811865464625, 0.000000000000000000 ) ) ;
#14135 = AXIS2_PLACEMENT_3D ( 'NONE', #6547, #51555, #70655 ) ;
#14136 = CARTESIAN_POINT ( 'NONE',  ( 0.5166543864104510275, 22.22500000000000142, 4.500000000000000888 ) ) ;
#14137 = CARTESIAN_POINT ( 'NONE',  ( 54.37499999999999289, 7.950000000000000178, 1.460391307983218535E-15 ) ) ;
#14138 = EDGE_LOOP ( 'NONE', ( #106849, #67321, #26184, #48568 ) ) ;
#14139 = ORIENTED_EDGE ( 'NONE', *, *, #7135, .T. ) ;
#14140 = LINE ( 'NONE', #26463, #77022 ) ;
#14141 = VECTOR ( 'NONE', #83557, 1000.000000000000000 ) ;
#14142 = VERTEX_POINT ( 'NONE', #106118 ) ;
#14143 = VECTOR ( 'NONE', #9665, 1000.000000000000000 ) ;
#14144 = PLANE ( 'NONE',  #99942 ) ;
#14145 = EDGE_CURVE ( 'NONE', #103206, #77014, #115557, .T. ) ;
#14146 = ORIENTED_EDGE ( 'NONE', *, *, #12879, .F. ) ;
#14147 = VECTOR ( 'NONE', #57923, 999.9999999999998863 ) ;
#14148 = CARTESIAN_POINT ( 'NONE',  ( 181.1500000000000057, -3.180000000000061444, 34.92499999999998295 ) ) ;
#14149 = FACE_OUTER_BOUND ( 'NONE', #61684, .T. ) ;
#14150 = VECTOR ( 'NONE', #74749, 1000.000000000000000 ) ;
#14151 = ORIENTED_EDGE ( 'NONE', *, *, #58797, .T. ) ;
#14152 = ADVANCED_FACE ( 'NONE', ( #93847 ), #125782, .F. ) ;
#14153 = EDGE_CURVE ( 'NONE', #94289, #127411, #70709, .T. ) ;
#14154 = FACE_BOUND ( 'NONE', #42195, .T. ) ;
#14155 = VECTOR ( 'NONE', #91325, 1000.000000000000000 ) ;
#14156 = LINE ( 'NONE', #110597, #6216 ) ;
#14157 = DIRECTION ( 'NONE',  ( 0.7071067811865487940, 0.7071067811865463515, 0.000000000000000000 ) ) ;
#14158 = CARTESIAN_POINT ( 'NONE',  ( 37.55836038379621300, -7.949999999999996625, -2.130196079827426203 ) ) ;
#14159 = CARTESIAN_POINT ( 'NONE',  ( 19.05000000000000071, 3.174999999999997158, 5.000000000000000000 ) ) ;
#14160 = EDGE_CURVE ( 'NONE', #3762, #14833, #38760, .T. ) ;
#14161 = EDGE_CURVE ( 'NONE', #131125, #82818, #18642, .T. ) ;
#14162 = SURFACE_STYLE_USAGE ( .BOTH. , #83009 ) ;
#14163 = DIRECTION ( 'NONE',  ( 0.09876088199217400443, 0.4890202883836731740, -0.8666633981755988980 ) ) ;
#14164 = ORIENTED_EDGE ( 'NONE', *, *, #50279, .F. ) ;
#14165 = VECTOR ( 'NONE', #24333, 1000.000000000000000 ) ;
#14166 = ORIENTED_EDGE ( 'NONE', *, *, #108460, .F. ) ;
#14167 = CARTESIAN_POINT ( 'NONE',  ( 104.4745968585647802, 1.637169565754164280, -6.109999999999996767 ) ) ;
#14168 = VERTEX_POINT ( 'NONE', #105424 ) ;
#14169 = EDGE_CURVE ( 'NONE', #115165, #46818, #6081, .T. ) ;
#14170 = DIRECTION ( 'NONE',  ( -0.7071067811865486830, -0.7071067811865464625, -0.000000000000000000 ) ) ;
#14171 = EDGE_LOOP ( 'NONE', ( #128003, #119524, #63939, #19895 ) ) ;
#14172 = VECTOR ( 'NONE', #65710, 1000.000000000000000 ) ;
#14173 = DIRECTION ( 'NONE',  ( -0.7071067811865487940, 0.7071067811865463515, -0.000000000000000000 ) ) ;
#14174 = PRESENTATION_LAYER_ASSIGNMENT (  '', '', ( #97470 ) ) ;
#14175 = PLANE ( 'NONE',  #20017 ) ;
#14176 = ADVANCED_FACE ( 'NONE', ( #64082 ), #43063, .F. ) ;
#14177 = DIRECTION ( 'NONE',  ( -0.7071067811865486830, -0.7071067811865464625, 0.000000000000000000 ) ) ;
#14178 = ORIENTED_EDGE ( 'NONE', *, *, #15796, .F. ) ;
#14179 = DIRECTION ( 'NONE',  ( -0.3543493200069163240, 0.000000000000000000, 0.9351131265310288487 ) ) ;
#14180 = LINE ( 'NONE', #112784, #107941 ) ;
#14181 = FACE_OUTER_BOUND ( 'NONE', #118700, .T. ) ;
#14182 = DIRECTION ( 'NONE',  ( 0.6830127018922181881, 0.6830127018922202975, -0.2588190451025214056 ) ) ;
#14183 = AXIS2_PLACEMENT_3D ( 'NONE', #30849, #119242, #31546 ) ;
#14184 = EDGE_CURVE ( 'NONE', #12102, #88761, #8232, .T. ) ;
#14185 = DIRECTION ( 'NONE',  ( -0.7071067811865486830, 0.7071067811865464625, 0.000000000000000000 ) ) ;
#14186 = ORIENTED_EDGE ( 'NONE', *, *, #32028, .T. ) ;
#14187 = DIRECTION ( 'NONE',  ( -1.000000000000000000, -0.000000000000000000, -0.000000000000000000 ) ) ;
#14188 = LINE ( 'NONE', #102655, #32664 ) ;
#14189 = ORIENTED_EDGE ( 'NONE', *, *, #113989, .F. ) ;
#14190 = ORIENTED_EDGE ( 'NONE', *, *, #30200, .T. ) ;
#14191 = ORIENTED_EDGE ( 'NONE', *, *, #50563, .T. ) ;
#14192 = CARTESIAN_POINT ( 'NONE',  ( 51.33376352523143282, 6.110000000000001208, 1.122388791418549305E-15 ) ) ;
#14193 = ADVANCED_FACE ( 'NONE', ( #29299 ), #41606, .F. ) ;
#14194 = AXIS2_PLACEMENT_3D ( 'NONE', #49977, #134866, #123970 ) ;
#14195 = VERTEX_POINT ( 'NONE', #63405 ) ;
#14196 =( BOUNDED_CURVE ( )  B_SPLINE_CURVE ( 3, ( #86464, #129957, #141549, #64703 ),
 .UNSPECIFIED., .F., .T. ) 
 B_SPLINE_CURVE_WITH_KNOTS ( ( 4, 4 ),
 ( 2.972453342939734622, 3.211474374380908436 ),
 .UNSPECIFIED. ) 
 CURVE ( )  GEOMETRIC_REPRESENTATION_ITEM ( )  RATIONAL_B_SPLINE_CURVE ( ( 1.000000000000000000, 0.9952447427727515450, 0.9952447427727515450, 1.000000000000000000 ) ) 
 REPRESENTATION_ITEM ( '' )  );
#14197 = CARTESIAN_POINT ( 'NONE',  ( 3.254139616203772345, 3.047499999999993214, -5.278424836066146320 ) ) ;
#14198 = CARTESIAN_POINT ( 'NONE',  ( 93.18793019189809002, 6.110000000000002984, -1.637169565754156730 ) ) ;
#14199 = DIRECTION ( 'NONE',  ( 0.000000000000000000, 0.000000000000000000, -1.000000000000000000 ) ) ;
#14200 = ORIENTED_EDGE ( 'NONE', *, *, #43858, .F. ) ;
#14201 = PLANE ( 'NONE',  #45680 ) ;
#14202 = ADVANCED_FACE ( 'NONE', ( #9680 ), #42352, .T. ) ;
#14203 = VERTEX_POINT ( 'NONE', #84433 ) ;
#14204 = DIRECTION ( 'NONE',  ( -0.6830127018922180770, -0.6830127018922204085, -0.2588190451025213501 ) ) ;
#14205 = COLOUR_RGB ( '', 0.08235294, 0.09019608, 0.10196078) ;
#14206 = DIRECTION ( 'NONE',  ( -1.000000000000000000, -0.000000000000000000, -0.000000000000000000 ) ) ;
#14207 = ORIENTED_EDGE ( 'NONE', *, *, #112084, .T. ) ;
#14208 = DIRECTION ( 'NONE',  ( -1.000000000000000000, -0.000000000000000000, -0.000000000000000000 ) ) ;
#14209 = CARTESIAN_POINT ( 'NONE',  ( -11.67183060077639212, 14.25929247661557575, 4.000000000000000000 ) ) ;
#14210 = EDGE_CURVE ( 'NONE', #60839, #96439, #97389, .T. ) ;
#14213 = ADVANCED_FACE ( 'NONE', ( #119161 ), #98145, .T. ) ;
#14212 = CARTESIAN_POINT ( 'NONE',  ( -0.7928932188134442116, 12.75929247661558463, 5.000000000000000000 ) ) ;
#14211 = AXIS2_PLACEMENT_3D ( 'NONE', #70597, #93732, #72017 ) ;
#14215 = ORIENTED_EDGE ( 'NONE', *, *, #47148, .T. ) ;
#14214 = VECTOR ( 'NONE', #23439, 1000.000000000000000 ) ;
#14216 = CARTESIAN_POINT ( 'NONE',  ( -1.362461875839014791, 22.22500000000000142, 4.000000000000000000 ) ) ;
#14217 = ORIENTED_EDGE ( 'NONE', *, *, #87630, .T. ) ;
#14218 = ORIENTED_EDGE ( 'NONE', *, *, #102662, .F. ) ;
#14219 = ORIENTED_EDGE ( 'NONE', *, *, #87211, .F. ) ;
#14220 = DIRECTION ( 'NONE',  ( -0.000000000000000000, -0.3543493200069152693, 0.9351131265310292928 ) ) ;
#14221 = VECTOR ( 'NONE', #112326, 1000.000000000000000 ) ;
#14222 = AXIS2_PLACEMENT_3D ( 'NONE', #13900, #68354, #56768 ) ;
#14223 = MECHANICAL_DESIGN_GEOMETRIC_PRESENTATION_REPRESENTATION (  '', ( #35064 ), #92984 ) ;
#14224 = AXIS2_PLACEMENT_3D ( 'NONE', #51423, #29633, #118048 ) ;
#14225 = EDGE_CURVE ( 'NONE', #137919, #3888, #128626, .T. ) ;
#14226 = AXIS2_PLACEMENT_3D ( 'NONE', #64514, #108690, #140632 ) ;
#14227 = DIRECTION ( 'NONE',  ( 0.000000000000000000, 0.000000000000000000, 1.000000000000000000 ) ) ;
#14228 = DIRECTION ( 'NONE',  ( 0.7071067811865487940, 0.7071067811865463515, 0.000000000000000000 ) ) ;
#14229 = EDGE_CURVE ( 'NONE', #64283, #52993, #141408, .T. ) ;
#14230 = CARTESIAN_POINT ( 'NONE',  ( -27.48921356237309155, -27.52281430457074762, 5.000000000000000000 ) ) ;
#14231 = CARTESIAN_POINT ( 'NONE',  ( -26.20710678118636139, 15.75929247661556687, 5.000000000000000000 ) ) ;
#14233 = ORIENTED_EDGE ( 'NONE', *, *, #35438, .T. ) ;
#14232 = VECTOR ( 'NONE', #87245, 1000.000000000000000 ) ;
#14234 = DIRECTION ( 'NONE',  ( 0.7071067811865486830, -0.7071067811865464625, -0.000000000000000000 ) ) ;
#14235 = CARTESIAN_POINT ( 'NONE',  ( 26.37456980810188867, 6.871911579029510442, -3.967499999999998916 ) ) ;
#14236 = CARTESIAN_POINT ( 'NONE',  ( -31.82816939922330235, -14.24070752338413648, 4.000000000000000000 ) ) ;
#14237 = LINE ( 'NONE', #124427, #127018 ) ;
#14239 = EDGE_CURVE ( 'NONE', #43122, #138950, #86563, .T. ) ;
#14238 = CIRCLE ( 'NONE', #125406, 0.5000000000000000000 ) ;
#14240 = CARTESIAN_POINT ( 'NONE',  ( -30.48921356237309510, -27.52281430457076894, 5.000000000000000000 ) ) ;
#14241 = ORIENTED_EDGE ( 'NONE', *, *, #53020, .T. ) ;
#14242 = ORIENTED_EDGE ( 'NONE', *, *, #63952, .T. ) ;
#14243 = VERTEX_POINT ( 'NONE', #76399 ) ;
#14244 = SURFACE_STYLE_FILL_AREA ( #1889 ) ;
#14245 = DIRECTION ( 'NONE',  ( 0.000000000000000000, -1.000000000000000000, 0.000000000000000000 ) ) ;
#14246 = UNCERTAINTY_MEASURE_WITH_UNIT (LENGTH_MEASURE( 1.000000000000000082E-05 ), #5974, 'distance_accuracy_value', 'NONE');
#14247 = CARTESIAN_POINT ( 'NONE',  ( -34.92500000000001137, -22.22500000000000142, 4.500000000000000888 ) ) ;
#14248 = ADVANCED_FACE ( 'NONE', ( #130058 ), #140221, .F. ) ;
#14249 = LINE ( 'NONE', #2641, #73744 ) ;
#14250 = CARTESIAN_POINT ( 'NONE',  ( 6.093169818762517842, 9.434785192573073687, 1.147133048873354211 ) ) ;
#14251 = VECTOR ( 'NONE', #74443, 1000.000000000000000 ) ;
#14252 = DIRECTION ( 'NONE',  ( -0.7071067811865487940, 0.7071067811865463515, -0.000000000000000000 ) ) ;
#14253 = CARTESIAN_POINT ( 'NONE',  ( 0.000000000000000000, -4.870000000000014317, -40.00000000000000000 ) ) ;
#14254 = FACE_OUTER_BOUND ( 'NONE', #72038, .T. ) ;
#14255 = CARTESIAN_POINT ( 'NONE',  ( 128.9683591370937563, -52.14999999999999147, 41.64499999999997470 ) ) ;
#14256 = VECTOR ( 'NONE', #111755, 1000.000000000000000 ) ;
#14257 = LINE ( 'NONE', #24420, #23341 ) ;
#14258 = EDGE_LOOP ( 'NONE', ( #94366, #41111, #119017, #8212 ) ) ;
#14260 = VECTOR ( 'NONE', #128923, 1000.000000000000000 ) ;
#14259 = CARTESIAN_POINT ( 'NONE',  ( 16.99081895618983751, -0.8493047346644202467, -35.56339853354601388 ) ) ;
#14261 = ORIENTED_EDGE ( 'NONE', *, *, #34666, .T. ) ;
#14262 = FACE_OUTER_BOUND ( 'NONE', #73366, .T. ) ;
#14264 = ORIENTED_EDGE ( 'NONE', *, *, #114991, .T. ) ;
#14263 = LINE ( 'NONE', #80265, #115808 ) ;
#14265 = DIRECTION ( 'NONE',  ( -0.6830127018922181881, 0.6830127018922202975, -0.2588190451025214056 ) ) ;
#14266 = CARTESIAN_POINT ( 'NONE',  ( 26.22995720542188991, 21.73644205237998150, 5.000000000000000888 ) ) ;
#14267 = ORIENTED_EDGE ( 'NONE', *, *, #137661, .T. ) ;
#14268 = CARTESIAN_POINT ( 'NONE',  ( -19.82816939922338761, -17.24070752338410983, 4.000000000000000000 ) ) ;
#14269 = VERTEX_POINT ( 'NONE', #117704 ) ;
#14270 = LINE ( 'NONE', #93968, #49132 ) ;
#14271 = VERTEX_POINT ( 'NONE', #54648 ) ;
#14272 = CARTESIAN_POINT ( 'NONE',  ( -21.60769999999998703, 3.130000000000008331, -22.35000000000000142 ) ) ;
#14273 = EDGE_CURVE ( 'NONE', #54563, #51456, #19846, .T. ) ;
#14274 = CARTESIAN_POINT ( 'NONE',  ( 106.1000270504628986, 5.819803920172570422, 5.819803920172574863 ) ) ;
#14275 = DIRECTION ( 'NONE',  ( -1.000000000000000000, -0.000000000000000000, -0.000000000000000000 ) ) ;
#14276 = DIRECTION ( 'NONE',  ( -0.000000000000000000, -0.000000000000000000, -1.000000000000000000 ) ) ;
#14277 = ORIENTED_EDGE ( 'NONE', *, *, #117154, .T. ) ;
#14278 = DIRECTION ( 'NONE',  ( -0.7071067811865486830, -0.7071067811865464625, 0.000000000000000000 ) ) ;
#14279 = FACE_OUTER_BOUND ( 'NONE', #91220, .T. ) ;
#14280 = CARTESIAN_POINT ( 'NONE',  ( -23.84387692260742142, -22.22500000000000142, 4.000000000000000000 ) ) ;
#14282 = VECTOR ( 'NONE', #132748, 1000.000000000000000 ) ;
#14281 = CARTESIAN_POINT ( 'NONE',  ( 24.79166666666667140, -3.047499999999994547, 5.278424836066145431 ) ) ;
#14283 = CARTESIAN_POINT ( 'NONE',  ( 23.89540314143522437, 2.126176841940962348, 7.934999999999988951 ) ) ;
#14285 = VECTOR ( 'NONE', #29071, 1000.000000000000000 ) ;
#14284 = CARTESIAN_POINT ( 'NONE',  ( 12.18398860626900060, 28.73617430169795739, 5.000000000000000000 ) ) ;
#14286 = CARTESIAN_POINT ( 'NONE',  ( 0.1839886062690032631, 28.73617430169787568, 5.000000000000000000 ) ) ;
#14287 = ORIENTED_EDGE ( 'NONE', *, *, #25908, .T. ) ;
#14288 = DIRECTION ( 'NONE',  ( -1.000000000000000000, -0.000000000000000000, -0.000000000000000000 ) ) ;
#14289 = ORIENTED_EDGE ( 'NONE', *, *, #48765, .F. ) ;
#14291 = VECTOR ( 'NONE', #104952, 999.9999999999998863 ) ;
#14290 = CARTESIAN_POINT ( 'NONE',  ( 94.79209685856476142, -5.291415217122921177, 3.054999999999999272 ) ) ;
#14292 = PLANE ( 'NONE',  #10651 ) ;
#14293 = CARTESIAN_POINT ( 'NONE',  ( 12.48921356237309155, -27.52281430457064104, 5.000000000000000000 ) ) ;
#14295 = VECTOR ( 'NONE', #17603, 1000.000000000000000 ) ;
#14294 = PLANE ( 'NONE',  #58581 ) ;
#14296 = CARTESIAN_POINT ( 'NONE',  ( -8.816011393731004731, 28.73617430169781173, 5.000000000000000000 ) ) ;
#14297 = VERTEX_POINT ( 'NONE', #118445 ) ;
#14298 = CARTESIAN_POINT ( 'NONE',  ( -27.18398860626900060, 28.73617430169806042, 5.000000000000000000 ) ) ;
#14299 = ORIENTED_EDGE ( 'NONE', *, *, #60631, .T. ) ;
#14300 = LINE ( 'NONE', #15002, #16083 ) ;
#14301 = CARTESIAN_POINT ( 'NONE',  ( 45.18398860626900415, 28.73617430169818832, 5.000000000000000000 ) ) ;
#14303 = ORIENTED_EDGE ( 'NONE', *, *, #109516, .F. ) ;
#14302 = LINE ( 'NONE', #15004, #24277 ) ;
#14304 = DIRECTION ( 'NONE',  ( 0.7071067811865487940, 0.7071067811865463515, -0.000000000000000000 ) ) ;
#14305 = LINE ( 'NONE', #11414, #82280 ) ;
#14306 = VECTOR ( 'NONE', #118188, 1000.000000000000000 ) ;
#14307 = DIRECTION ( 'NONE',  ( 0.7071067811865487940, 0.7071067811865463515, 0.000000000000000000 ) ) ;
#14308 = FACE_OUTER_BOUND ( 'NONE', #62462, .T. ) ;
#14309 = VERTEX_POINT ( 'NONE', #108250 ) ;
#14310 = EDGE_LOOP ( 'NONE', ( #46702, #44515, #45633, #52805 ) ) ;
#14311 = EDGE_LOOP ( 'NONE', ( #3738, #20252, #100141, #130496 ) ) ;
#14312 = CARTESIAN_POINT ( 'NONE',  ( 82.97959685856476142, 6.109999999999999432, 1.637169565754164280 ) ) ;
#14313 = ORIENTED_EDGE ( 'NONE', *, *, #55459, .F. ) ;
#14314 = DIRECTION ( 'NONE',  ( -0.7071067811865486830, -0.7071067811865464625, -0.000000000000000000 ) ) ;
#14315 = CARTESIAN_POINT ( 'NONE',  ( -23.99999999999982947, -0.1606350220013114671, 4.664761815935120737 ) ) ;
#14316 = DIRECTION ( 'NONE',  ( -0.3543493200069162685, -0.000000000000000000, -0.9351131265310288487 ) ) ;
#14317 = CARTESIAN_POINT ( 'NONE',  ( 38.99451991528749062, 28.92564299267965211, 4.000000000000000000 ) ) ;
#14318 = ORIENTED_EDGE ( 'NONE', *, *, #136296, .T. ) ;
#14319 = VECTOR ( 'NONE', #8164, 1000.000000000000000 ) ;
#14320 = CIRCLE ( 'NONE', #58363, 2.055000000000000604 ) ;
#14321 = FACE_OUTER_BOUND ( 'NONE', #71899, .T. ) ;
#14322 = DIRECTION ( 'NONE',  ( -0.7071067811865487940, 0.7071067811865463515, 0.000000000000000000 ) ) ;
#14323 = VECTOR ( 'NONE', #79536, 1000.000000000000227 ) ;
#14325 = VECTOR ( 'NONE', #100133, 999.9999999999998863 ) ;
#14324 = DIRECTION ( 'NONE',  ( -0.000000000000000000, 0.3543493200069153248, 0.9351131265310292928 ) ) ;
#14326 = CARTESIAN_POINT ( 'NONE',  ( 74.87043019189812298, -3.055000000000001492, 5.291415217122917625 ) ) ;
#14327 = ORIENTED_EDGE ( 'NONE', *, *, #78354, .T. ) ;
#14328 = CARTESIAN_POINT ( 'NONE',  ( 33.32816939922329880, 17.25929247661554555, 4.000000000000000000 ) ) ;
#14329 = EDGE_CURVE ( 'NONE', #117767, #60012, #39501, .T. ) ;
#14331 = DIRECTION ( 'NONE',  ( -0.000000000000000000, -0.3543493200069152693, 0.9351131265310292928 ) ) ;
#14330 = VECTOR ( 'NONE', #75826, 1000.000000000000000 ) ;
#14332 = DIRECTION ( 'NONE',  ( 0.7071067811865487940, 0.7071067811865463515, -0.000000000000000000 ) ) ;
#14333 =( GEOMETRIC_REPRESENTATION_CONTEXT ( 3 ) GLOBAL_UNCERTAINTY_ASSIGNED_CONTEXT ( ( #86851 ) ) GLOBAL_UNIT_ASSIGNED_CONTEXT ( ( #47663, #91824, #4047 ) ) REPRESENTATION_CONTEXT ( 'NONE', 'WORKASPACE' ) );
#14334 = VECTOR ( 'NONE', #74440, 999.9999999999998863 ) ;
#14335 = EDGE_LOOP ( 'NONE', ( #18034, #129148, #111491, #817 ) ) ;
#14336 = EDGE_LOOP ( 'NONE', ( #85534, #1151, #130551, #61330, #21181 ) ) ;
#14337 = ADVANCED_FACE ( 'NONE', ( #32164 ), #108983, .F. ) ;
#14338 = CARTESIAN_POINT ( 'NONE',  ( -42.48921356237308800, -27.52281430457085065, 5.000000000000000000 ) ) ;
#14339 = ADVANCED_FACE ( 'NONE', ( #7532 ), #142371, .F. ) ;
#14340 = EDGE_CURVE ( 'NONE', #135705, #117224, #104326, .T. ) ;
#14341 = CARTESIAN_POINT ( 'NONE',  ( -8.994519915287490619, 28.92564299267944250, 4.000000000000000000 ) ) ;
#14342 = B_SPLINE_CURVE_WITH_KNOTS ( 'NONE', 3,
 ( #126962, #116090, #106621, #73335, #26945, #83495, #115342, #137152, #29790, #118219, #28393, #72653, #18925, #16033, #17494, #61748, #105910, #103768, #139320, #8028, #85597, #75468, #9445, #63191, #41390, #52965, #65327, #53724, #108756, #97927, #142854, #88491, #21059, #86349, #131993, #96452, #97163, #130569, #10184, #42139, #109509, #54448, #32685, #107362, #132731, #141427 ),
 .UNSPECIFIED., .F., .F.,
 ( 4, 2, 2, 2, 2, 2, 2, 2, 2, 2, 2, 2, 2, 2, 2, 2, 2, 2, 2, 2, 2, 2, 4 ),
 ( 0.000000000000000000, 0.002810485862540013525, 0.005620971725080024448, 0.007026214656350030993, 0.008431457587620039273, 0.01124194345016004543, 0.01264718638143005197, 0.01405242931270006025, 0.01686291517524007855, 0.01826815810651008856, 0.01967340103778009511, 0.02248388690032011861, 0.02388912983159013209, 0.02529437276286013864, 0.02810485862540016214, 0.02951010155667016868, 0.03091534448794018217, 0.03372583035048019873, 0.03653631621302021876, 0.03934680207556023879, 0.04075204500683024533, 0.04215728793810025188, 0.04496777380064026497 ),
 .UNSPECIFIED. ) ;
#14343 = DIRECTION ( 'NONE',  ( 0.7071067811865487940, -0.7071067811865463515, 0.000000000000000000 ) ) ;
#14344 = LINE ( 'NONE', #136115, #105793 ) ;
#14345 = FACE_OUTER_BOUND ( 'NONE', #32304, .T. ) ;
#14346 = EDGE_CURVE ( 'NONE', #3387, #41073, #74260, .T. ) ;
#14347 = EDGE_CURVE ( 'NONE', #53397, #47033, #24852, .T. ) ;
#14348 = DIRECTION ( 'NONE',  ( 0.6830127018922181881, 0.6830127018922202975, -0.2588190451025214056 ) ) ;
#14349 = VERTEX_POINT ( 'NONE', #21988 ) ;
#14350 = ORIENTED_EDGE ( 'NONE', *, *, #106333, .T. ) ;
#14352 = EDGE_CURVE ( 'NONE', #109349, #87614, #4745, .T. ) ;
#14351 = DIRECTION ( 'NONE',  ( -1.000000000000000000, -0.000000000000000000, -0.000000000000000000 ) ) ;
#14353 = ORIENTED_EDGE ( 'NONE', *, *, #68660, .F. ) ;
#14354 = VECTOR ( 'NONE', #51293, 1000.000000000000114 ) ;
#14355 = EDGE_CURVE ( 'NONE', #96152, #85530, #87972, .T. ) ;
#14356 = VECTOR ( 'NONE', #64092, 1000.000000000000000 ) ;
#14357 = CARTESIAN_POINT ( 'NONE',  ( 77.99451991528749772, 28.92564299267992567, 4.000000000000000000 ) ) ;
#14358 = ORIENTED_EDGE ( 'NONE', *, *, #142085, .F. ) ;
#14359 = LINE ( 'NONE', #115766, #96874 ) ;
#14360 = CARTESIAN_POINT ( 'NONE',  ( -15.29974487139158867, -27.71228299555216879, 4.000000000000000000 ) ) ;
#14361 = VECTOR ( 'NONE', #45634, 1000.000000000000000 ) ;
#14362 = LINE ( 'NONE', #136133, #61948 ) ;
#14363 = LINE ( 'NONE', #91914, #136449 ) ;
#14364 = AXIS2_PLACEMENT_3D ( 'NONE', #128072, #10354, #126598 ) ;
#14365 = DIRECTION ( 'NONE',  ( -1.000000000000000000, -0.000000000000000000, -0.000000000000000000 ) ) ;
#14366 = ORIENTED_EDGE ( 'NONE', *, *, #48641, .F. ) ;
#14367 = DIRECTION ( 'NONE',  ( 0.7071067811865486830, -0.7071067811865464625, -0.000000000000000000 ) ) ;
#14368 = CARTESIAN_POINT ( 'NONE',  ( 0.000000000000000000, -34.64999999999999147, 17.49210858042621908 ) ) ;
#14369 = ORIENTED_EDGE ( 'NONE', *, *, #52665, .F. ) ;
#14370 = PLANE ( 'NONE',  #48109 ) ;
#14371 = ORIENTED_EDGE ( 'NONE', *, *, #68145, .T. ) ;
#14372 = ORIENTED_EDGE ( 'NONE', *, *, #69941, .F. ) ;
#14373 = DIRECTION ( 'NONE',  ( -1.000000000000000000, -1.224606353822377258E-16, -0.000000000000000000 ) ) ;
#14374 = VERTEX_POINT ( 'NONE', #23414 ) ;
#14375 = VERTEX_POINT ( 'NONE', #35775 ) ;
#14376 = DIRECTION ( 'NONE',  ( -1.000000000000000000, -1.224606353822377258E-16, -0.000000000000000000 ) ) ;
#14377 = EDGE_CURVE ( 'NONE', #138876, #121112, #57511, .T. ) ;
#14378 = AXIS2_PLACEMENT_3D ( 'NONE', #28479, #41461, #62535 ) ;
#14379 = VERTEX_POINT ( 'NONE', #90854 ) ;
#14380 = CARTESIAN_POINT ( 'NONE',  ( 3.299744871391591339, -27.71228299555208352, 4.000000000000000000 ) ) ;
#14381 = LINE ( 'NONE', #103504, #49594 ) ;
#14382 = CARTESIAN_POINT ( 'NONE',  ( 118.8545968585647756, -1.637169565754161615, 6.110000000000000320 ) ) ;
#14383 = LINE ( 'NONE', #102836, #61343 ) ;
#14384 = FACE_OUTER_BOUND ( 'NONE', #10183, .T. ) ;
#14386 = DIRECTION ( 'NONE',  ( -0.7071067811865486830, 0.7071067811865464625, 0.000000000000000000 ) ) ;
#14385 = VECTOR ( 'NONE', #44114, 1000.000000000000000 ) ;
#14387 = EDGE_CURVE ( 'NONE', #122233, #13272, #32551, .T. ) ;
#14388 = CARTESIAN_POINT ( 'NONE',  ( 1.553349423367815563, 2.259292476615697876, 14.86850063742354067 ) ) ;
#14389 = VECTOR ( 'NONE', #58734, 1000.000000000000000 ) ;
#14390 = DIRECTION ( 'NONE',  ( -0.3543493200069162685, -0.000000000000000000, -0.9351131265310288487 ) ) ;
#14392 = EDGE_CURVE ( 'NONE', #103662, #84513, #22673, .T. ) ;
#14391 =( LENGTH_UNIT ( ) NAMED_UNIT ( * ) SI_UNIT ( .MILLI., .METRE. ) );
#14393 = ORIENTED_EDGE ( 'NONE', *, *, #130521, .F. ) ;
#14394 = LINE ( 'NONE', #101395, #129103 ) ;
#14395 = CARTESIAN_POINT ( 'NONE',  ( 34.49999999999975842, 1.464255608400477415, 4.994342998332161443 ) ) ;
#14396 = ORIENTED_EDGE ( 'NONE', *, *, #7467, .F. ) ;
#14397 = ADVANCED_FACE ( 'NONE', ( #1637 ), #111877, .F. ) ;
#14398 = ORIENTED_EDGE ( 'NONE', *, *, #77044, .F. ) ;
#14399 = CARTESIAN_POINT ( 'NONE',  ( 30.18398860626900060, 28.73617430169808173, 5.000000000000000000 ) ) ;
#14400 = EDGE_LOOP ( 'NONE', ( #23097, #74515, #133501, #65818 ) ) ;
#14401 = EDGE_CURVE ( 'NONE', #31895, #68079, #121306, .T. ) ;
#14402 = ADVANCED_FACE ( 'NONE', ( #2353 ), #88126, .T. ) ;
#14403 = CARTESIAN_POINT ( 'NONE',  ( 33.29974487139158867, -27.71228299555229313, 4.000000000000000000 ) ) ;
#14404 = DIRECTION ( 'NONE',  ( -0.000000000000000000, -1.000000000000000000, -0.000000000000000000 ) ) ;
#14405 = DIRECTION ( 'NONE',  ( -1.000000000000000000, -8.718663809566799855E-16, 0.000000000000000000 ) ) ;
#14406 = DIRECTION ( 'NONE',  ( -0.7071067811865486830, 0.7071067811865464625, 0.000000000000000000 ) ) ;
#14407 = ORIENTED_EDGE ( 'NONE', *, *, #51778, .F. ) ;
#14408 = CARTESIAN_POINT ( 'NONE',  ( 45.18398860626900415, 28.73617430169818832, 5.000000000000000000 ) ) ;
#14409 = VECTOR ( 'NONE', #77781, 1000.000000000000000 ) ;
#14410 = VERTEX_POINT ( 'NONE', #43756 ) ;
#14411 = ADVANCED_FACE ( 'NONE', ( #134349 ), #35047, .F. ) ;
#14412 = CARTESIAN_POINT ( 'NONE',  ( -4.499999999999970690, 3.431123077392153053, 4.000000000000000000 ) ) ;
#14413 = CARTESIAN_POINT ( 'NONE',  ( 23.83790314143521982, -6.871911579029513106, -3.967499999999993587 ) ) ;
#14414 = EDGE_LOOP ( 'NONE', ( #2010, #94234, #111645 ) ) ;
#14415 = CYLINDRICAL_SURFACE ( 'NONE', #94525, 2.500000000000000000 ) ;
#14416 = EDGE_CURVE ( 'NONE', #22488, #103049, #77132, .T. ) ;
#14417 = LINE ( 'NONE', #45651, #23421 ) ;
#14418 = EDGE_LOOP ( 'NONE', ( #32748, #99347, #66030 ) ) ;
#14419 = VERTEX_POINT ( 'NONE', #55360 ) ;
#14420 = ORIENTED_EDGE ( 'NONE', *, *, #50861, .T. ) ;
#14421 = DIRECTION ( 'NONE',  ( 0.7071067811865486830, -0.7071067811865464625, -0.000000000000000000 ) ) ;
#14422 = DIRECTION ( 'NONE',  ( 0.000000000000000000, 2.775557561562888827E-14, 1.000000000000000000 ) ) ;
#14423 = AXIS2_PLACEMENT_3D ( 'NONE', #141198, #98426, #86846 ) ;
#14425 = PLANE ( 'NONE',  #3376 ) ;
#14424 = AXIS2_PLACEMENT_3D ( 'NONE', #101410, #57957, #68131 ) ;
#14426 = VECTOR ( 'NONE', #19674, 999.9999999999998863 ) ;
#14427 = DIRECTION ( 'NONE',  ( 0.7071067811865487940, -0.7071067811865463515, 0.000000000000000000 ) ) ;
#14429 = ORIENTED_EDGE ( 'NONE', *, *, #61867, .F. ) ;
#14428 =( BOUNDED_CURVE ( )  B_SPLINE_CURVE ( 3, ( #45353, #54782, #34440, #89529 ),
 .UNSPECIFIED., .F., .F. ) 
 B_SPLINE_CURVE_WITH_KNOTS ( ( 4, 4 ),
 ( 5.920967161967927161, 7.341195215986644484 ),
 .UNSPECIFIED. ) 
 CURVE ( )  GEOMETRIC_REPRESENTATION_ITEM ( )  RATIONAL_B_SPLINE_CURVE ( ( 1.000000000000000000, 0.8388583629366599403, 0.8388583629366599403, 1.000000000000000000 ) ) 
 REPRESENTATION_ITEM ( '' )  );
#14430 = CARTESIAN_POINT ( 'NONE',  ( 39.18398860626899705, 28.73617430169814568, 5.000000000000000000 ) ) ;
#14431 = AXIS2_PLACEMENT_3D ( 'NONE', #98216, #30832, #87340 ) ;
#14432 = CARTESIAN_POINT ( 'NONE',  ( 15.32816939922342137, -18.74070752338409562, 4.000000000000000000 ) ) ;
#14433 = AXIS2_PLACEMENT_3D ( 'NONE', #89251, #21844, #45775 ) ;
#14434 = ADVANCED_FACE ( 'NONE', ( #204 ), #108879, .T. ) ;
#14435 = LINE ( 'NONE', #104995, #99804 ) ;
#14436 = DIRECTION ( 'NONE',  ( -0.000000000000000000, 0.000000000000000000, 1.000000000000000000 ) ) ;
#14437 = ORIENTED_EDGE ( 'NONE', *, *, #73781, .F. ) ;
#14438 = VECTOR ( 'NONE', #119134, 1000.000000000000000 ) ;
#14439 = VECTOR ( 'NONE', #27110, 1000.000000000000000 ) ;
#14440 = DIRECTION ( 'NONE',  ( 0.000000000000000000, 0.000000000000000000, 1.000000000000000000 ) ) ;
#14441 = EDGE_LOOP ( 'NONE', ( #88165, #85452, #4274, #16927 ) ) ;
#14444 = EDGE_CURVE ( 'NONE', #95280, #69167, #11810, .T. ) ;
#14443 = ORIENTED_EDGE ( 'NONE', *, *, #86309, .T. ) ;
#14442 = FACE_OUTER_BOUND ( 'NONE', #13551, .T. ) ;
#14445 = VERTEX_POINT ( 'NONE', #100287 ) ;
#14446 = DIRECTION ( 'NONE',  ( -0.000000000000000000, 0.000000000000000000, 1.000000000000000000 ) ) ;
#14447 = LINE ( 'NONE', #39047, #138667 ) ;
#14448 = ORIENTED_EDGE ( 'NONE', *, *, #95271, .T. ) ;
#14449 = UNCERTAINTY_MEASURE_WITH_UNIT (LENGTH_MEASURE( 1.000000000000000082E-05 ), #74958, 'distance_accuracy_value', 'NONE');
#14450 = CARTESIAN_POINT ( 'NONE',  ( 16.04515773336655826, -21.74070752338406365, 21.72585301388588519 ) ) ;
#14451 = CARTESIAN_POINT ( 'NONE',  ( 20.99451991528748707, 28.92564299267952777, 4.000000000000000000 ) ) ;
#14452 = LINE ( 'NONE', #68173, #122578 ) ;
#14453 = DIRECTION ( 'NONE',  ( -0.7071067811865487940, 0.7071067811865463515, 0.000000000000000000 ) ) ;
#14454 = LINE ( 'NONE', #123239, #120625 ) ;
#14455 = DIRECTION ( 'NONE',  ( -0.7071067811865486830, -0.7071067811865464625, 0.000000000000000000 ) ) ;
#14456 = LINE ( 'NONE', #58735, #75013 ) ;
#14457 = CARTESIAN_POINT ( 'NONE',  ( 23.89540314143522437, 2.126176841940962348, 7.934999999999989839 ) ) ;
#14458 = LINE ( 'NONE', #12305, #106910 ) ;
#14459 = PLANE ( 'NONE',  #15767 ) ;
#14460 = DIRECTION ( 'NONE',  ( -0.7071067811865486830, -0.7071067811865464625, -0.000000000000000000 ) ) ;
#14461 = CARTESIAN_POINT ( 'NONE',  ( 0.000000000000000000, 0.000000000000000000, 5.000000000000000000 ) ) ;
#14462 = VERTEX_POINT ( 'NONE', #68403 ) ;
#14463 = ADVANCED_FACE ( 'NONE', ( #112582 ), #13241, .T. ) ;
#14464 = VECTOR ( 'NONE', #66283, 1000.000000000000000 ) ;
#14465 = ORIENTED_EDGE ( 'NONE', *, *, #78870, .T. ) ;
#14466 = CARTESIAN_POINT ( 'NONE',  ( 92.58333333333332860, 6.884901960086290629, -3.974999999999994316 ) ) ;
#14467 = EDGE_CURVE ( 'NONE', #134641, #135641, #36453, .T. ) ;
#14468 = ORIENTED_EDGE ( 'NONE', *, *, #42970, .F. ) ;
#14469 = ORIENTED_EDGE ( 'NONE', *, *, #127623, .F. ) ;
#14470 = AXIS2_PLACEMENT_3D ( 'NONE', #75071, #63486, #27964 ) ;
#14471 = LINE ( 'NONE', #127509, #94293 ) ;
#14472 = LINE ( 'NONE', #126102, #11631 ) ;
#14473 = VECTOR ( 'NONE', #108584, 1000.000000000000000 ) ;
#14474 = CARTESIAN_POINT ( 'NONE',  ( 11.47583603616349102, 8.506184923238587103, 4.230711047486125587 ) ) ;
#14475 = ORIENTED_EDGE ( 'NONE', *, *, #113763, .F. ) ;
#14476 = DIRECTION ( 'NONE',  ( -0.000000000000000000, 0.000000000000000000, 1.000000000000000000 ) ) ;
#14477 = DIRECTION ( 'NONE',  ( -0.000000000000000000, 0.3543493200069152138, -0.9351131265310292928 ) ) ;
#14478 = PLANE ( 'NONE',  #39518 ) ;
#14479 = CARTESIAN_POINT ( 'NONE',  ( 125.7014274047528488, -0.5088013136202494957, -7.748369483595296536 ) ) ;
#14480 = EDGE_CURVE ( 'NONE', #61706, #133114, #92968, .T. ) ;
#14481 = CARTESIAN_POINT ( 'NONE',  ( -69.48921356237309510, -27.52281430457103895, 5.000000000000000000 ) ) ;
#14482 = PLANE ( 'NONE',  #119155 ) ;
#14483 = CARTESIAN_POINT ( 'NONE',  ( 31.17183060077626067, -8.240707523384196875, 4.000000000000000000 ) ) ;
#14484 = CARTESIAN_POINT ( 'NONE',  ( -12.69999999999998153, 0.000000000000000000, 0.000000000000000000 ) ) ;
#14485 = LINE ( 'NONE', #58031, #14512 ) ;
#14486 = LINE ( 'NONE', #122517, #40775 ) ;
#14487 = CARTESIAN_POINT ( 'NONE',  ( 5.994519915287488843, 28.92564299267942118, 4.000000000000000000 ) ) ;
#14488 = ORIENTED_EDGE ( 'NONE', *, *, #108616, .T. ) ;
#14489 = ORIENTED_EDGE ( 'NONE', *, *, #32406, .T. ) ;
#14490 = CARTESIAN_POINT ( 'NONE',  ( 112.8754301918981042, -5.291415217122920289, -3.055000000000001492 ) ) ;
#14491 = ORIENTED_EDGE ( 'NONE', *, *, #108980, .F. ) ;
#14492 = AXIS2_PLACEMENT_3D ( 'NONE', #25014, #3262, #12715 ) ;
#14493 = DIRECTION ( 'NONE',  ( 0.7071067811865486830, -0.7071067811865464625, -0.000000000000000000 ) ) ;
#14494 = AXIS2_PLACEMENT_3D ( 'NONE', #25872, #49804, #93977 ) ;
#14495 = CARTESIAN_POINT ( 'NONE',  ( 29.35681257248243980, -20.24070752338406720, 21.22881796311219560 ) ) ;
#14496 = ORIENTED_EDGE ( 'NONE', *, *, #28252, .T. ) ;
#14497 = CARTESIAN_POINT ( 'NONE',  ( -18.18398860626898994, 28.73617430169800002, 5.000000000000000000 ) ) ;
#14498 = CARTESIAN_POINT ( 'NONE',  ( -45.48921356237309510, -27.52281430457087197, 5.000000000000000000 ) ) ;
#14499 = CARTESIAN_POINT ( 'NONE',  ( 107.5370968585647944, -3.054999999999998828, -5.291415217122919401 ) ) ;
#14500 = ORIENTED_EDGE ( 'NONE', *, *, #45738, .T. ) ;
#14501 = EDGE_CURVE ( 'NONE', #53245, #127371, #37900, .T. ) ;
#14502 = ORIENTED_EDGE ( 'NONE', *, *, #53805, .F. ) ;
#14503 = CARTESIAN_POINT ( 'NONE',  ( 19.05000000000000071, 3.174999999999997158, 4.000000000000000000 ) ) ;
#14504 = VECTOR ( 'NONE', #57875, 1000.000000000000000 ) ;
#14505 = CARTESIAN_POINT ( 'NONE',  ( -33.98911971346028338, -22.02621442084248216, 4.990779571109225543 ) ) ;
#14506 = ORIENTED_EDGE ( 'NONE', *, *, #4183, .F. ) ;
#14507 = VERTEX_POINT ( 'NONE', #82829 ) ;
#14508 = ORIENTED_EDGE ( 'NONE', *, *, #20555, .F. ) ;
#14509 = LINE ( 'NONE', #23969, #49121 ) ;
#14510 = EDGE_CURVE ( 'NONE', #86215, #81446, #26994, .T. ) ;
#14511 = SURFACE_STYLE_USAGE ( .BOTH. , #111692 ) ;
#14512 = VECTOR ( 'NONE', #114492, 1000.000000000000000 ) ;
#14513 = EDGE_CURVE ( 'NONE', #37639, #106934, #116859, .T. ) ;
#14514 = EDGE_CURVE ( 'NONE', #5941, #72014, #59654, .T. ) ;
#14515 = CARTESIAN_POINT ( 'NONE',  ( -21.29974487139158512, -27.71228299555221142, 4.000000000000000000 ) ) ;
#14516 = EDGE_CURVE ( 'NONE', #86498, #25409, #3096, .T. ) ;
#14517 = ORIENTED_EDGE ( 'NONE', *, *, #13506, .T. ) ;
#14518 = VERTEX_POINT ( 'NONE', #3770 ) ;
#14520 = ADVANCED_FACE ( 'NONE', ( #25560 ), #50195, .T. ) ;
#14519 = CARTESIAN_POINT ( 'NONE',  ( -1.499999999999987566, -9.462702396501011748, -9.474982329943509640 ) ) ;
#14521 = EDGE_LOOP ( 'NONE', ( #78282, #3813, #30355, #16773 ) ) ;
#14522 = EDGE_LOOP ( 'NONE', ( #3302, #58503, #101827, #92395 ) ) ;
#14523 = VECTOR ( 'NONE', #77738, 999.9999999999998863 ) ;
#14524 = PRESENTATION_LAYER_ASSIGNMENT (  '', '', ( #77059 ) ) ;
#14525 = EDGE_CURVE ( 'NONE', #123401, #35122, #81413, .T. ) ;
#14526 = VECTOR ( 'NONE', #39211, 1000.000000000000000 ) ;
#14527 = CARTESIAN_POINT ( 'NONE',  ( 6.489213562373093325, -27.52281430457059841, 5.000000000000000000 ) ) ;
#14528 = AXIS2_PLACEMENT_3D ( 'NONE', #52521, #121344, #22030 ) ;
#14529 = ADVANCED_FACE ( 'NONE', ( #5218 ), #135767, .T. ) ;
#14530 = FACE_OUTER_BOUND ( 'NONE', #120294, .T. ) ;
#14531 = CARTESIAN_POINT ( 'NONE',  ( -17.99999999999987566, -0.2811185226894475919, -5.995736974527472896 ) ) ;
#14532 = ORIENTED_EDGE ( 'NONE', *, *, #54480, .F. ) ;
#14533 = DIRECTION ( 'NONE',  ( -0.000000000000000000, 0.000000000000000000, 1.000000000000000000 ) ) ;
#14534 = VECTOR ( 'NONE', #70607, 1000.000000000000000 ) ;
#14535 = AXIS2_PLACEMENT_3D ( 'NONE', #60706, #104874, #5539 ) ;
#14536 = DIRECTION ( 'NONE',  ( 0.6830127018922180770, -0.6830127018922204085, -0.2588190451025213501 ) ) ;
#14537 = EDGE_CURVE ( 'NONE', #99617, #82100, #72702, .T. ) ;
#14538 = FACE_BOUND ( 'NONE', #99936, .T. ) ;
#14539 = ORIENTED_EDGE ( 'NONE', *, *, #7796, .T. ) ;
#14540 = EDGE_CURVE ( 'NONE', #74280, #24706, #98831, .T. ) ;
#14541 = CARTESIAN_POINT ( 'NONE',  ( -2.999999999999975131, 10.93112307739207267, 4.000000000000000000 ) ) ;
#14542 = CARTESIAN_POINT ( 'NONE',  ( 12.48921356237309155, -27.52281430457064104, 5.000000000000000000 ) ) ;
#14543 =( NAMED_UNIT ( * ) SI_UNIT ( $, .STERADIAN. ) SOLID_ANGLE_UNIT ( ) );
#14544 = VERTEX_POINT ( 'NONE', #27702 ) ;
#14545 = DIRECTION ( 'NONE',  ( 0.7071067811865487940, 0.7071067811865463515, 0.000000000000000000 ) ) ;
#14546 = ORIENTED_EDGE ( 'NONE', *, *, #69663, .F. ) ;
#14547 = ORIENTED_EDGE ( 'NONE', *, *, #80357, .F. ) ;
#14548 = EDGE_CURVE ( 'NONE', #63812, #76671, #114699, .T. ) ;
#14549 = ORIENTED_EDGE ( 'NONE', *, *, #26664, .T. ) ;
#14550 = CARTESIAN_POINT ( 'NONE',  ( 37.39126352523144448, -4.472830434245838482, -4.472830434245838482 ) ) ;
#14551 = VERTEX_POINT ( 'NONE', #116139 ) ;
#14552 = CONICAL_SURFACE ( 'NONE', #56203, 2.500000000000000888, 0.9599310885968822538 ) ;
#14553 = CARTESIAN_POINT ( 'NONE',  ( 15.18398860626900237, 28.73617430169797871, 5.000000000000000000 ) ) ;
#14554 = FILL_AREA_STYLE_COLOUR ( '', #25197 ) ;
#14555 = DIRECTION ( 'NONE',  ( 0.7071067811865487940, 0.7071067811865463515, 0.000000000000000000 ) ) ;
#14556 = ORIENTED_EDGE ( 'NONE', *, *, #35382, .F. ) ;
#14557 = CARTESIAN_POINT ( 'NONE',  ( -34.42500000000001137, -22.22500000000000142, 4.500000000000000888 ) ) ;
#14558 = AXIS2_PLACEMENT_3D ( 'NONE', #84649, #73082, #17239 ) ;
#14559 = CARTESIAN_POINT ( 'NONE',  ( 29.99999999999979039, 4.931123077392140175, 4.000000000000000000 ) ) ;
#14560 = LINE ( 'NONE', #37763, #57882 ) ;
#14561 = DIRECTION ( 'NONE',  ( 0.000000000000000000, 0.000000000000000000, 1.000000000000000000 ) ) ;
#14562 =( GEOMETRIC_REPRESENTATION_CONTEXT ( 3 ) GLOBAL_UNCERTAINTY_ASSIGNED_CONTEXT ( ( #22798 ) ) GLOBAL_UNIT_ASSIGNED_CONTEXT ( ( #9007, #132309, #88791 ) ) REPRESENTATION_CONTEXT ( 'NONE', 'WORKASPACE' ) );
#14563 = LINE ( 'NONE', #71111, #14632 ) ;
#14564 = VERTEX_POINT ( 'NONE', #61118 ) ;
#14565 = EDGE_CURVE ( 'NONE', #116655, #89946, #138629, .T. ) ;
#14566 = VERTEX_POINT ( 'NONE', #55724 ) ;
#14567 = ORIENTED_EDGE ( 'NONE', *, *, #84109, .F. ) ;
#14568 = ORIENTED_EDGE ( 'NONE', *, *, #60003, .T. ) ;
#14569 = DIRECTION ( 'NONE',  ( -0.000000000000000000, -0.3543493200069152693, 0.9351131265310292928 ) ) ;
#14570 = ORIENTED_EDGE ( 'NONE', *, *, #104781, .T. ) ;
#14571 = VERTEX_POINT ( 'NONE', #109369 ) ;
#14572 = CARTESIAN_POINT ( 'NONE',  ( 39.18398860626899705, 28.73617430169814568, 5.000000000000000000 ) ) ;
#14573 = CARTESIAN_POINT ( 'NONE',  ( -8.939889289559747709, -9.740707523384184441, 10.89222023123382854 ) ) ;
#14574 = ORIENTED_EDGE ( 'NONE', *, *, #53157, .F. ) ;
#14575 = DIRECTION ( 'NONE',  ( 0.000000000000000000, 0.000000000000000000, 1.000000000000000000 ) ) ;
#14576 = VERTEX_POINT ( 'NONE', #121655 ) ;
#14577 = EDGE_CURVE ( 'NONE', #139420, #72096, #21659, .T. ) ;
#14579 = CIRCLE ( 'NONE', #90981, 2.500000000000000888 ) ;
#14578 = CARTESIAN_POINT ( 'NONE',  ( -4.671406296382802914, 22.22500000000000142, -6.464217593021417407 ) ) ;
#14580 = DIRECTION ( 'NONE',  ( -0.6830127018922180770, -0.6830127018922204085, -0.2588190451025213501 ) ) ;
#14581 = CARTESIAN_POINT ( 'NONE',  ( 1.671236474768553082, 0.000000000000000000, 7.934999999999990727 ) ) ;
#14582 = EDGE_LOOP ( 'NONE', ( #132986, #134344, #84140, #24506, #117202, #56825, #140975, #138544, #100601, #105520, #41571, #53147, #115803, #141978, #89867, #61818, #15295, #131992, #105543, #55071, #60578, #23722, #21829, #8018, #125584, #123313, #13919, #3027, #102496, #109837, #119298, #112820, #126662, #97785, #42999, #64224, #136658, #25792, #45175, #82177, #10278, #101342, #34891, #110289, #102920, #133976, #25162, #98541, #91003, #118809, #34293, #103337, #75573, #67899, #92800, #9832, #4509, #93407, #28082, #27841, #20985, #75449, #55418, #73513, #138828, #79026, #125552, #32384, #78819, #88940, #141776, #139941, #1202, #5863, #25661, #121580, #136231, #78318, #130761, #90099, #76805, #89277, #118138, #11473, #65983, #84889, #129717, #107249, #115070, #89235, #74103, #111606, #49486, #109901, #72591, #38050, #19048, #111242, #51264, #118523, #74808, #23379, #123336, #93821, #1919 ) ) ;
#14584 = DIRECTION ( 'NONE',  ( 0.3543493200069162685, -0.000000000000000000, -0.9351131265310288487 ) ) ;
#14583 = CARTESIAN_POINT ( 'NONE',  ( 102.2870968585647802, 3.054999999999997939, 5.291415217122920289 ) ) ;
#14585 =( BOUNDED_CURVE ( )  B_SPLINE_CURVE ( 3, ( #46432, #67453, #88481, #79782 ),
 .UNSPECIFIED., .F., .T. ) 
 B_SPLINE_CURVE_WITH_KNOTS ( ( 4, 4 ),
 ( 1.208578181583238820, 1.359146454359468237 ),
 .UNSPECIFIED. ) 
 CURVE ( )  GEOMETRIC_REPRESENTATION_ITEM ( )  RATIONAL_B_SPLINE_CURVE ( ( 1.000000000000000000, 0.9981116584018945304, 0.9981116584018945304, 1.000000000000000000 ) ) 
 REPRESENTATION_ITEM ( '' )  );
#14587 = EDGE_CURVE ( 'NONE', #98903, #6676, #22325, .T. ) ;
#14586 = DIRECTION ( 'NONE',  ( -0.7071067811865487940, 0.7071067811865463515, -0.000000000000000000 ) ) ;
#14588 = LINE ( 'NONE', #59549, #9527 ) ;
#14589 = VECTOR ( 'NONE', #60583, 1000.000000000000000 ) ;
#14590 = VERTEX_POINT ( 'NONE', #18221 ) ;
#14591 = SURFACE_STYLE_USAGE ( .BOTH. , #92853 ) ;
#14592 = VERTEX_POINT ( 'NONE', #131130 ) ;
#14594 = VECTOR ( 'NONE', #125753, 1000.000000000000000 ) ;
#14593 = PLANE ( 'NONE',  #16060 ) ;
#14595 = LINE ( 'NONE', #93588, #94906 ) ;
#14596 = DIRECTION ( 'NONE',  ( -0.6830127018922180770, -0.6830127018922204085, -0.2588190451025213501 ) ) ;
#14597 = DIRECTION ( 'NONE',  ( -0.3543493200069162685, -0.000000000000000000, -0.9351131265310288487 ) ) ;
#14598 = CARTESIAN_POINT ( 'NONE',  ( 180.8090197240767054, -49.02095135882321131, -39.67421197283155720 ) ) ;
#14599 = ORIENTED_EDGE ( 'NONE', *, *, #85632, .F. ) ;
#14600 = DIRECTION ( 'NONE',  ( -0.6830127018922181881, 0.6830127018922202975, -0.2588190451025214056 ) ) ;
#14601 = ADVANCED_FACE ( 'NONE', ( #117544 ), #62498, .F. ) ;
#14602 = DIRECTION ( 'NONE',  ( -0.7071067811865486830, -0.7071067811865464625, 0.000000000000000000 ) ) ;
#14603 = DIRECTION ( 'NONE',  ( 0.7071067811865487940, 0.7071067811865463515, -0.000000000000000000 ) ) ;
#14604 = EDGE_LOOP ( 'NONE', ( #71627, #52128, #70863, #4227 ) ) ;
#14605 = CARTESIAN_POINT ( 'NONE',  ( 36.48921356237310221, -27.52281430457080802, 5.000000000000000000 ) ) ;
#14606 = CIRCLE ( 'NONE', #135099, 2.999999999999992450 ) ;
#14607 = LINE ( 'NONE', #112493, #26120 ) ;
#14608 = ORIENTED_EDGE ( 'NONE', *, *, #8588, .F. ) ;
#14611 = EDGE_CURVE ( 'NONE', #94430, #15705, #87620, .T. ) ;
#14610 = ORIENTED_EDGE ( 'NONE', *, *, #11600, .F. ) ;
#14609 = DIRECTION ( 'NONE',  ( 0.6830127018922180770, -0.6830127018922204085, -0.2588190451025213501 ) ) ;
#14612 = ORIENTED_EDGE ( 'NONE', *, *, #100181, .F. ) ;
#14613 = VECTOR ( 'NONE', #63719, 999.9999999999998863 ) ;
#14614 = CARTESIAN_POINT ( 'NONE',  ( -12.59816835436673621, 9.780221332989524896, -27.05079659061421182 ) ) ;
#14615 = DIRECTION ( 'NONE',  ( -1.000000000000000000, 0.000000000000000000, 0.000000000000000000 ) ) ;
#14616 = EDGE_LOOP ( 'NONE', ( #121587, #57220, #44910 ) ) ;
#14617 = CARTESIAN_POINT ( 'NONE',  ( 52.33333333333332860, -6.884901960086287964, 3.974999999999998312 ) ) ;
#14618 = EDGE_CURVE ( 'NONE', #131061, #76695, #10740, .T. ) ;
#14619 = LINE ( 'NONE', #78461, #69319 ) ;
#14620 = ORIENTED_EDGE ( 'NONE', *, *, #41209, .F. ) ;
#14621 = CARTESIAN_POINT ( 'NONE',  ( 5.207106781186507050, -8.240707523384198652, 5.000000000000000000 ) ) ;
#14622 = CARTESIAN_POINT ( 'NONE',  ( 17.29298673570682254, -21.74070752338406720, 4.999753212805220670 ) ) ;
#14623 = PLANE ( 'NONE',  #125438 ) ;
#14624 = DIRECTION ( 'NONE',  ( -0.7071067811865486830, 0.7071067811865464625, 0.000000000000000000 ) ) ;
#14625 = AXIS2_PLACEMENT_3D ( 'NONE', #128207, #126736, #115131 ) ;
#14626 = LINE ( 'NONE', #58906, #100302 ) ;
#14627 = FACE_OUTER_BOUND ( 'NONE', #121326, .T. ) ;
#14628 = DIRECTION ( 'NONE',  ( -0.7071067811865486830, 0.7071067811865464625, 0.000000000000000000 ) ) ;
#14629 = EDGE_CURVE ( 'NONE', #37516, #31371, #32535, .T. ) ;
#14630 = CARTESIAN_POINT ( 'NONE',  ( -60.29974487139158867, -27.71228299555248142, 4.000000000000000000 ) ) ;
#14631 = EDGE_LOOP ( 'NONE', ( #64050, #7888, #132003 ) ) ;
#14632 = VECTOR ( 'NONE', #58844, 1000.000000000000114 ) ;
#14633 = EDGE_LOOP ( 'NONE', ( #113114, #86401, #34936, #24023 ) ) ;
#14634 = VERTEX_POINT ( 'NONE', #86918 ) ;
#14635 = CARTESIAN_POINT ( 'NONE',  ( 120.5833333333333286, 6.884901960086290629, -3.974999999999994316 ) ) ;
#14636 = EDGE_CURVE ( 'NONE', #14590, #9641, #66596, .T. ) ;
#14637 = ORIENTED_EDGE ( 'NONE', *, *, #139102, .F. ) ;
#14638 = ORIENTED_EDGE ( 'NONE', *, *, #136235, .T. ) ;
#14639 = VERTEX_POINT ( 'NONE', #65182 ) ;
#14640 = VECTOR ( 'NONE', #127746, 1000.000000000000000 ) ;
#14641 = CARTESIAN_POINT ( 'NONE',  ( 19.05000000000000071, 3.174999999999997158, 5.000000000000000000 ) ) ;
#14642 = AXIS2_PLACEMENT_3D ( 'NONE', #34502, #78727, #112769 ) ;
#14643 = PLANE ( 'NONE',  #23116 ) ;
#14644 = ORIENTED_EDGE ( 'NONE', *, *, #41566, .T. ) ;
#14645 = STYLED_ITEM ( 'NONE', ( #103010 ), #43643 ) ;
#14646 = DIRECTION ( 'NONE',  ( -0.7071067811865486830, -0.7071067811865464625, 0.000000000000000000 ) ) ;
#14647 = CARTESIAN_POINT ( 'NONE',  ( 34.92499999999998295, -17.33753812416080464, 4.000000000000000000 ) ) ;
#14648 = CARTESIAN_POINT ( 'NONE',  ( 33.18398860626899705, 28.73617430169810305, 5.000000000000000000 ) ) ;
#14649 = CARTESIAN_POINT ( 'NONE',  ( 112.1462635252314328, -4.472830434245840259, 4.472830434245839371 ) ) ;
#14650 = VERTEX_POINT ( 'NONE', #591 ) ;
#14651 = EDGE_CURVE ( 'NONE', #22333, #102502, #40053, .T. ) ;
#14652 = DIRECTION ( 'NONE',  ( 0.6830127018922180770, -0.6830127018922204085, -0.2588190451025213501 ) ) ;
#14653 = CARTESIAN_POINT ( 'NONE',  ( 29.99999999999979394, 17.96639925780207747, 5.000000000000000000 ) ) ;
#14654 = CARTESIAN_POINT ( 'NONE',  ( 45.48921356237309510, -27.52281430457087197, 5.000000000000000000 ) ) ;
#14655 = LINE ( 'NONE', #13911, #54943 ) ;
#14656 = DIRECTION ( 'NONE',  ( 0.7071067811865486830, -0.7071067811865464625, -0.000000000000000000 ) ) ;
#14657 = CARTESIAN_POINT ( 'NONE',  ( 2.139447441471317823, -2.500000000000000000, 3.061616997868383634E-16 ) ) ;
#14658 = PRODUCT_DEFINITION ( 'UNKNOWN', '', #47199, #50204 ) ;
#14659 = CARTESIAN_POINT ( 'NONE',  ( 49.37086038379622011, 6.884901960086289741, -3.974999999999993427 ) ) ;
#14660 = DIRECTION ( 'NONE',  ( 0.7071067811865486830, -0.7071067811865464625, -0.000000000000000000 ) ) ;
#14662 = PRESENTATION_STYLE_ASSIGNMENT (( #93659 ) ) ;
#14661 = VECTOR ( 'NONE', #10325, 1000.000000000000000 ) ;
#14663 = ORIENTED_EDGE ( 'NONE', *, *, #116922, .F. ) ;
#14664 = ORIENTED_EDGE ( 'NONE', *, *, #40412, .F. ) ;
#14665 = CARTESIAN_POINT ( 'NONE',  ( 40.52083333333332860, 7.949999999999999289, 2.130196079827431532 ) ) ;
#14666 = VERTEX_POINT ( 'NONE', #142718 ) ;
#14667 = EDGE_LOOP ( 'NONE', ( #35487, #36498, #72551, #15198 ) ) ;
#14668 = CARTESIAN_POINT ( 'NONE',  ( -30.00000000000000355, -2.375000000000000000, 0.000000000000000000 ) ) ;
#14669 = DIRECTION ( 'NONE',  ( -0.6830127018922181881, 0.6830127018922202975, -0.2588190451025214056 ) ) ;
#14670 = CARTESIAN_POINT ( 'NONE',  ( -32.99451991528749062, 28.92564299267960948, 4.000000000000000000 ) ) ;
#14671 = ORIENTED_EDGE ( 'NONE', *, *, #69941, .T. ) ;
#14672 = CARTESIAN_POINT ( 'NONE',  ( 0.000000000000000000, 0.000000000000000000, 0.000000000000000000 ) ) ;
#14673 = VECTOR ( 'NONE', #25798, 1000.000000000000000 ) ;
#14674 = DIRECTION ( 'NONE',  ( 1.000000000000000000, 0.000000000000000000, 0.000000000000000000 ) ) ;
#14675 = CARTESIAN_POINT ( 'NONE',  ( -13.88982677111779296, -22.22500000000000497, 4.785647885939354751 ) ) ;
#14676 = CARTESIAN_POINT ( 'NONE',  ( 31.64626352523143638, -4.472830434245840259, 4.472830434245839371 ) ) ;
#14677 = AXIS2_PLACEMENT_3D ( 'NONE', #89466, #23495, #3161 ) ;
#14678 = ORIENTED_EDGE ( 'NONE', *, *, #84019, .F. ) ;
#14679 = DIRECTION ( 'NONE',  ( 0.7071067811865487940, -0.7071067811865463515, 0.000000000000000000 ) ) ;
#14680 = EDGE_LOOP ( 'NONE', ( #88582, #66648, #101418, #40806 ) ) ;
#14681 = DIRECTION ( 'NONE',  ( 0.000000000000000000, 0.000000000000000000, -1.000000000000000000 ) ) ;
#14682 = DIRECTION ( 'NONE',  ( -0.000000000000000000, 0.3543493200069153248, 0.9351131265310292928 ) ) ;
#14683 =( NAMED_UNIT ( * ) PLANE_ANGLE_UNIT ( ) SI_UNIT ( $, .RADIAN. ) );
#14684 = AXIS2_PLACEMENT_3D ( 'NONE', #59206, #92484, #24391 ) ;
#14685 = CARTESIAN_POINT ( 'NONE',  ( 62.25000000000000000, -9.735942053221458872E-16, 7.950000000000000178 ) ) ;
#14686 = EDGE_LOOP ( 'NONE', ( #29095, #91055, #37837 ) ) ;
#14687 = ORIENTED_EDGE ( 'NONE', *, *, #139934, .F. ) ;
#14688 = PLANE ( 'NONE',  #139683 ) ;
#14689 = CARTESIAN_POINT ( 'NONE',  ( -29.99999999999978328, -15.03360074219758857, 5.000000000000000000 ) ) ;
#14690 = CARTESIAN_POINT ( 'NONE',  ( -2.994519915287485734, 28.92564299267940342, 4.000000000000000000 ) ) ;
#14691 = VECTOR ( 'NONE', #138111, 1000.000000000000000 ) ;
#14692 = ADVANCED_FACE ( 'NONE', ( #33288 ), #128464, .T. ) ;
#14693 = PRESENTATION_LAYER_ASSIGNMENT (  '', '', ( #56340 ) ) ;
#14694 = CARTESIAN_POINT ( 'NONE',  ( 53.87043019189811588, -3.055000000000001492, 5.291415217122917625 ) ) ;
#14695 = EDGE_CURVE ( 'NONE', #136110, #84461, #20917, .T. ) ;
#14696 = CARTESIAN_POINT ( 'NONE',  ( 124.0833333333333428, 6.884901960086290629, -3.974999999999994316 ) ) ;
#14698 = ADVANCED_FACE ( 'NONE', ( #53577 ), #120951, .T. ) ;
#14697 = DIRECTION ( 'NONE',  ( -1.000000000000000000, -0.000000000000000000, -0.000000000000000000 ) ) ;
#14699 = ORIENTED_EDGE ( 'NONE', *, *, #222, .F. ) ;
#14700 = EDGE_LOOP ( 'NONE', ( #106079, #50304, #90858, #136400, #35050, #11010 ) ) ;
#14701 = CARTESIAN_POINT ( 'NONE',  ( -27.32816939922333432, -9.740707523384180888, 4.000000000000000000 ) ) ;
#14702 = ORIENTED_EDGE ( 'NONE', *, *, #108832, .T. ) ;
#14703 = ADVANCED_FACE ( 'NONE', ( #105955 ), #65906, .T. ) ;
#14704 = CARTESIAN_POINT ( 'NONE',  ( 34.55179764501523465, 22.26999999999999957, -11.48108961241408998 ) ) ;
#14705 = ORIENTED_EDGE ( 'NONE', *, *, #45745, .T. ) ;
#14706 = FACE_OUTER_BOUND ( 'NONE', #114473, .T. ) ;
#14707 = VECTOR ( 'NONE', #111963, 1000.000000000000227 ) ;
#14708 = FILL_AREA_STYLE ('',( #27006 ) ) ;
#14709 = EDGE_CURVE ( 'NONE', #68652, #139204, #44130, .T. ) ;
#14710 = FACE_BOUND ( 'NONE', #28499, .T. ) ;
#14711 = EDGE_CURVE ( 'NONE', #44187, #91404, #97780, .T. ) ;
#14712 = DIRECTION ( 'NONE',  ( -1.000000000000000000, -1.224606353822377258E-16, -0.000000000000000000 ) ) ;
#14713 = DIRECTION ( 'NONE',  ( -0.7071067811865486830, -0.7071067811865464625, 0.000000000000000000 ) ) ;
#14714 = DIRECTION ( 'NONE',  ( -0.6830127018922181881, 0.6830127018922202975, -0.2588190451025214056 ) ) ;
#14715 = VECTOR ( 'NONE', #72859, 999.9999999999998863 ) ;
#14716 = DIRECTION ( 'NONE',  ( 0.6830127018922180770, -0.6830127018922204085, -0.2588190451025213501 ) ) ;
#14718 = VERTEX_POINT ( 'NONE', #77489 ) ;
#14717 = LINE ( 'NONE', #78558, #27269 ) ;
#14719 = CARTESIAN_POINT ( 'NONE',  ( 0.000000000000000000, 0.000000000000000000, 10.00000000000000000 ) ) ;
#14720 = ADVANCED_FACE ( 'NONE', ( #11452 ), #29140, .T. ) ;
#14721 = ORIENTED_EDGE ( 'NONE', *, *, #57904, .T. ) ;
#14722 = ORIENTED_EDGE ( 'NONE', *, *, #8112, .T. ) ;
#14723 = CARTESIAN_POINT ( 'NONE',  ( 66.12043019189812298, 3.055000000000001936, -5.291415217122916737 ) ) ;
#14725 = ORIENTED_EDGE ( 'NONE', *, *, #47773, .F. ) ;
#14724 = STYLED_ITEM ( 'NONE', ( #128682 ), #19464 ) ;
#14726 = DIRECTION ( 'NONE',  ( 0.3543493200069162685, -0.000000000000000000, -0.9351131265310288487 ) ) ;
#14727 = ORIENTED_EDGE ( 'NONE', *, *, #60055, .T. ) ;
#14728 = CARTESIAN_POINT ( 'NONE',  ( 47.99451991528749062, 28.92564299267971251, 4.000000000000000000 ) ) ;
#14729 = EDGE_CURVE ( 'NONE', #88325, #117852, #68067, .T. ) ;
#14730 = CIRCLE ( 'NONE', #114279, 2.500000000000000444 ) ;
#14731 = CARTESIAN_POINT ( 'NONE',  ( 28.49999999999981171, -2.947814304570794075, 5.000000000000000000 ) ) ;
#14732 = DIRECTION ( 'NONE',  ( 0.000000000000000000, 0.2631995976047524777, 0.9647414015272156584 ) ) ;
#14733 = CARTESIAN_POINT ( 'NONE',  ( 102.3541666666666714, -2.130196079827387567, -7.950000000000023270 ) ) ;
#14734 = CARTESIAN_POINT ( 'NONE',  ( 21.75860074219781382, 21.72500000000000142, 5.000000000000000000 ) ) ;
#14735 = LINE ( 'NONE', #3806, #12235 ) ;
#14736 = CARTESIAN_POINT ( 'NONE',  ( 33.29974487139158867, -27.71228299555229313, 4.000000000000000000 ) ) ;
#14737 = VERTEX_POINT ( 'NONE', #25941 ) ;
#14738 = EDGE_CURVE ( 'NONE', #46867, #45528, #69464, .T. ) ;
#14739 = ORIENTED_EDGE ( 'NONE', *, *, #10382, .F. ) ;
#14740 = CARTESIAN_POINT ( 'NONE',  ( 14.86920357848291196, 3.061616997868383634E-16, -2.500000000000000444 ) ) ;
#14741 = LINE ( 'NONE', #59018, #11927 ) ;
#14742 = ORIENTED_EDGE ( 'NONE', *, *, #89505, .F. ) ;
#14743 = ORIENTED_EDGE ( 'NONE', *, *, #46676, .F. ) ;
#14744 = ORIENTED_EDGE ( 'NONE', *, *, #81342, .F. ) ;
#14745 = CARTESIAN_POINT ( 'NONE',  ( 36.18398860626899705, 28.73617430169812437, 5.000000000000000000 ) ) ;
#14746 = ORIENTED_EDGE ( 'NONE', *, *, #100350, .T. ) ;
#14747 = CARTESIAN_POINT ( 'NONE',  ( 2.924914550060625285, 3.061616997868382648E-16, -2.500000000000000444 ) ) ;
#14748 = VECTOR ( 'NONE', #18999, 1000.000000000000000 ) ;
#14749 = ADVANCED_FACE ( 'NONE', ( #59314, #35423 ), #134732, .F. ) ;
#14750 = DIRECTION ( 'NONE',  ( -0.7071067811865486830, -0.7071067811865464625, -0.000000000000000000 ) ) ;
#14751 = VECTOR ( 'NONE', #45690, 1000.000000000000000 ) ;
#14752 = CARTESIAN_POINT ( 'NONE',  ( 3.712903141435219379, 3.967499999999992699, -6.871911579029513994 ) ) ;
#14753 = CARTESIAN_POINT ( 'NONE',  ( 34.92499999999998295, -0.2815095627957336921, 4.759050581649326261 ) ) ;
#14754 = ORIENTED_EDGE ( 'NONE', *, *, #85006, .T. ) ;
#14755 = DIRECTION ( 'NONE',  ( -0.6830127018922181881, 0.6830127018922202975, -0.2588190451025214056 ) ) ;
#14757 = ADVANCED_FACE ( 'NONE', ( #91224 ), #24496, .F. ) ;
#14756 = DIRECTION ( 'NONE',  ( -0.7071067811865486830, -0.7071067811865464625, -0.000000000000000000 ) ) ;
#14758 = DIRECTION ( 'NONE',  ( 0.000000000000000000, 0.000000000000000000, 1.000000000000000000 ) ) ;
#14760 = VERTEX_POINT ( 'NONE', #58627 ) ;
#14759 = CARTESIAN_POINT ( 'NONE',  ( 13.92145407031093818, 4.584330080086930965E-16, 0.000000000000000000 ) ) ;
#14761 = ORIENTED_EDGE ( 'NONE', *, *, #137874, .F. ) ;
#14762 = LINE ( 'NONE', #59039, #137635 ) ;
#14763 = CARTESIAN_POINT ( 'NONE',  ( 0.000000000000000000, -6.108550654416962544, -3.114665004254967950 ) ) ;
#14764 = VECTOR ( 'NONE', #86460, 1000.000000000000000 ) ;
#14765 = DIRECTION ( 'NONE',  ( 0.000000000000000000, -1.000000000000000000, 0.000000000000000000 ) ) ;
#14766 = EDGE_LOOP ( 'NONE', ( #127644, #78010, #96208, #42375 ) ) ;
#14767 = LINE ( 'NONE', #73968, #85307 ) ;
#14768 = EDGE_CURVE ( 'NONE', #121120, #128690, #102799, .T. ) ;
#14769 = CARTESIAN_POINT ( 'NONE',  ( 0.000000000000000000, 0.000000000000000000, 0.000000000000000000 ) ) ;
#14770 = PLANE ( 'NONE',  #83586 ) ;
#14771 = DIRECTION ( 'NONE',  ( -0.7071067811865486830, 0.7071067811865464625, 0.000000000000000000 ) ) ;
#14772 = VERTEX_POINT ( 'NONE', #125247 ) ;
#14773 = LINE ( 'NONE', #112659, #99393 ) ;
#14774 = CARTESIAN_POINT ( 'NONE',  ( -34.92500000000001137, 22.22500000000000142, 4.500000000000000888 ) ) ;
#14776 = VECTOR ( 'NONE', #95181, 1000.000000000000000 ) ;
#14775 = CARTESIAN_POINT ( 'NONE',  ( -11.20710678118646619, 0.7592924766157138627, 5.000000000000000000 ) ) ;
#14777 = LINE ( 'NONE', #89479, #7721 ) ;
#14778 = FILL_AREA_STYLE ('',( #5306 ) ) ;
#14780 = EDGE_CURVE ( 'NONE', #103353, #60630, #2741, .T. ) ;
#14779 = ORIENTED_EDGE ( 'NONE', *, *, #8270, .F. ) ;
#14781 = ORIENTED_EDGE ( 'NONE', *, *, #122242, .F. ) ;
#14782 = CARTESIAN_POINT ( 'NONE',  ( 25.46142480454906121, -4.648522628062372597, -4.648522628062373485 ) ) ;
#14783 = VECTOR ( 'NONE', #26566, 1000.000000000000000 ) ;
#14784 = LINE ( 'NONE', #308, #135083 ) ;
#14785 = VECTOR ( 'NONE', #36485, 1000.000000000000000 ) ;
#14786 = CARTESIAN_POINT ( 'NONE',  ( 8.728736474768551190, 5.808823158059031044, -5.808823158059038150 ) ) ;
#14787 = CARTESIAN_POINT ( 'NONE',  ( 65.70419371712955581, -6.884901960086285300, -3.975000000000000089 ) ) ;
#14788 = CARTESIAN_POINT ( 'NONE',  ( 27.29974487139158512, -27.71228299555225405, 4.000000000000000000 ) ) ;
#14789 = CARTESIAN_POINT ( 'NONE',  ( -30.18398860626900060, 28.73617430169808173, 5.000000000000000000 ) ) ;
#14790 = CARTESIAN_POINT ( 'NONE',  ( 47.99451991528749062, 28.92564299267971251, 4.000000000000000000 ) ) ;
#14791 = VERTEX_POINT ( 'NONE', #100652 ) ;
#14792 = DIRECTION ( 'NONE',  ( -0.7071067811865486830, 0.7071067811865463515, 0.000000000000000000 ) ) ;
#14793 = DIRECTION ( 'NONE',  ( -0.7071067811865486830, -0.7071067811865464625, 0.000000000000000000 ) ) ;
#14794 = VECTOR ( 'NONE', #125175, 1000.000000000000000 ) ;
#14795 = FACE_OUTER_BOUND ( 'NONE', #119232, .T. ) ;
#14796 = CARTESIAN_POINT ( 'NONE',  ( 60.72459685856477307, -1.637169565754161171, 6.109999999999998543 ) ) ;
#14797 = LINE ( 'NONE', #59071, #9358 ) ;
#14798 = DIRECTION ( 'NONE',  ( -0.000000000000000000, 0.000000000000000000, 1.000000000000000000 ) ) ;
#14799 = EDGE_CURVE ( 'NONE', #57263, #68516, #106705, .T. ) ;
#14800 = ORIENTED_EDGE ( 'NONE', *, *, #143025, .F. ) ;
#14801 = CARTESIAN_POINT ( 'NONE',  ( 12.19999999999999574, -39.93000000000001393, 19.45086547876359617 ) ) ;
#14802 = VERTEX_POINT ( 'NONE', #136829 ) ;
#14803 = CIRCLE ( 'NONE', #123607, 2.500000000000000888 ) ;
#14804 = CARTESIAN_POINT ( 'NONE',  ( 151.4000000000000057, -18.48000000000005372, -33.92499999999998295 ) ) ;
#14805 = SURFACE_STYLE_FILL_AREA ( #56921 ) ;
#14806 = CARTESIAN_POINT ( 'NONE',  ( -48.18398860626899705, 28.73617430169820608, 5.000000000000000000 ) ) ;
#14807 = CARTESIAN_POINT ( 'NONE',  ( 2.292893218813435219, 11.25929247661560773, 5.000000000000000000 ) ) ;
#14808 = EDGE_CURVE ( 'NONE', #137770, #53831, #13601, .T. ) ;
#14809 = DIRECTION ( 'NONE',  ( 0.6830127018922181881, 0.6830127018922202975, -0.2588190451025214056 ) ) ;
#14810 =( NAMED_UNIT ( * ) SI_UNIT ( $, .STERADIAN. ) SOLID_ANGLE_UNIT ( ) );
#14811 = VERTEX_POINT ( 'NONE', #90481 ) ;
#14812 = EDGE_CURVE ( 'NONE', #15122, #110128, #56474, .T. ) ;
#14813 = ORIENTED_EDGE ( 'NONE', *, *, #6013, .T. ) ;
#14814 = LINE ( 'NONE', #90976, #125091 ) ;
#14815 = LINE ( 'NONE', #35894, #109328 ) ;
#14816 = DIRECTION ( 'NONE',  ( -1.000000000000000000, 0.000000000000000000, 0.000000000000000000 ) ) ;
#14817 = CARTESIAN_POINT ( 'NONE',  ( 23.00840764549667483, -3.851859888774471706E-31, 2.500000000000001332 ) ) ;
#14818 = CARTESIAN_POINT ( 'NONE',  ( 78.10002705046289861, 5.819803920172570422, 5.819803920172574863 ) ) ;
#14819 = VECTOR ( 'NONE', #62557, 1000.000000000000227 ) ;
#14820 = DIRECTION ( 'NONE',  ( 0.000000000000000000, -1.000000000000000000, 0.000000000000000000 ) ) ;
#14821 = ORIENTED_EDGE ( 'NONE', *, *, #74053, .F. ) ;
#14822 = CARTESIAN_POINT ( 'NONE',  ( 65.75000000000000000, -9.735942053221458872E-16, 7.950000000000000178 ) ) ;
#14823 = LINE ( 'NONE', #59095, #51656 ) ;
#14824 = CARTESIAN_POINT ( 'NONE',  ( -15.00548008471250228, 28.92564299267927552, 4.000000000000000000 ) ) ;
#14825 = DIRECTION ( 'NONE',  ( 2.781805975412905274E-17, -0.3543493200069152138, 0.9351131265310292928 ) ) ;
#14826 = EDGE_LOOP ( 'NONE', ( #31792, #113385, #126374, #19664, #139919, #3177 ) ) ;
#14827 = ADVANCED_FACE ( 'NONE', ( #135435 ), #47729, .F. ) ;
#14828 = AXIS2_PLACEMENT_3D ( 'NONE', #128498, #5251, #105297 ) ;
#14829 = CARTESIAN_POINT ( 'NONE',  ( 39.48921356237310221, -27.52281430457082934, 5.000000000000000000 ) ) ;
#14830 = LINE ( 'NONE', #137347, #67531 ) ;
#14831 = CARTESIAN_POINT ( 'NONE',  ( 53.81293019189810423, -1.637169565754159617, -6.110000000000001208 ) ) ;
#14832 = CARTESIAN_POINT ( 'NONE',  ( 20.70025512860841133, -27.71228299555191654, 4.000000000000000000 ) ) ;
#14833 = VERTEX_POINT ( 'NONE', #36802 ) ;
#14834 = EDGE_LOOP ( 'NONE', ( #20923, #97916, #95663, #130014 ) ) ;
#14835 = DIRECTION ( 'NONE',  ( 0.000000000000000000, -1.000000000000000000, 0.000000000000000000 ) ) ;
#14836 = LINE ( 'NONE', #59111, #126240 ) ;
#14837 = PLANE ( 'NONE',  #88355 ) ;
#14838 = CARTESIAN_POINT ( 'NONE',  ( 16.49999999999988987, -8.947814304570730570, 5.000000000000000000 ) ) ;
#14839 = DIRECTION ( 'NONE',  ( 0.000000000000000000, -1.000000000000000000, 0.000000000000000000 ) ) ;
#14841 = VERTEX_POINT ( 'NONE', #114366 ) ;
#14840 = DIRECTION ( 'NONE',  ( -0.3543493200069162685, -0.000000000000000000, -0.9351131265310288487 ) ) ;
#14842 = FACE_OUTER_BOUND ( 'NONE', #101970, .T. ) ;
#14843 = CARTESIAN_POINT ( 'NONE',  ( -34.92500000000001137, 21.72500000000000142, 5.000000000000000000 ) ) ;
#14844 = CARTESIAN_POINT ( 'NONE',  ( 3.000000000000000000, -49.85820393249939286, 34.92500000000001847 ) ) ;
#14845 = AXIS2_PLACEMENT_3D ( 'NONE', #43276, #65773, #54869 ) ;
#14846 = DIRECTION ( 'NONE',  ( -0.000000000000000000, 0.3543493200069153248, 0.9351131265310292928 ) ) ;
#14847 = ORIENTED_EDGE ( 'NONE', *, *, #18719, .F. ) ;
#14848 = CIRCLE ( 'NONE', #126013, 2.500000000000000888 ) ;
#14849 = EDGE_CURVE ( 'NONE', #88219, #8957, #125260, .T. ) ;
#14850 = EDGE_LOOP ( 'NONE', ( #52008, #41064, #35573, #102886 ) ) ;
#14851 = DIRECTION ( 'NONE',  ( 0.000000000000000000, 1.000000000000000000, 0.000000000000000000 ) ) ;
#14852 = EDGE_CURVE ( 'NONE', #48269, #673, #1298, .T. ) ;
#14853 = CARTESIAN_POINT ( 'NONE',  ( 30.47336096364196223, -5.240707523384228850, 16.25846745537502969 ) ) ;
#14854 = DIRECTION ( 'NONE',  ( 0.7071067811865487940, -0.7071067811865463515, 0.000000000000000000 ) ) ;
#14855 = CARTESIAN_POINT ( 'NONE',  ( -54.29974487139159578, -27.71228299555243879, 4.000000000000000000 ) ) ;
#14856 = ORIENTED_EDGE ( 'NONE', *, *, #103078, .F. ) ;
#14857 = VERTEX_POINT ( 'NONE', #81779 ) ;
#14858 = CARTESIAN_POINT ( 'NONE',  ( -12.29974487139158512, -27.71228299555214747, 4.000000000000000000 ) ) ;
#14859 = DIRECTION ( 'NONE',  ( 0.7071067811865486830, -0.7071067811865464625, -0.000000000000000000 ) ) ;
#14860 = EDGE_CURVE ( 'NONE', #91475, #51456, #45582, .T. ) ;
#14861 = EDGE_CURVE ( 'NONE', #128057, #32169, #23799, .T. ) ;
#14862 = VERTEX_POINT ( 'NONE', #112241 ) ;
#14863 = VECTOR ( 'NONE', #121036, 1000.000000000000000 ) ;
#14864 = CARTESIAN_POINT ( 'NONE',  ( -4.019877749285451607, -17.24070752338410273, 20.23474786156468497 ) ) ;
#14865 = ORIENTED_EDGE ( 'NONE', *, *, #95070, .F. ) ;
#14866 = DIRECTION ( 'NONE',  ( 1.000000000000000000, 0.000000000000000000, 0.000000000000000000 ) ) ;
#14867 = PLANE ( 'NONE',  #139743 ) ;
#14868 =( BOUNDED_CURVE ( )  B_SPLINE_CURVE ( 2, ( #140160, #18322, #62596, #87192, #28545, #96593, #31388, #86492, #106782, #140833, #85748, #53111, #97311 ),
 .UNSPECIFIED., .F., .T. ) 
 B_SPLINE_CURVE_WITH_KNOTS ( ( 3, 2, 2, 2, 2, 2, 3 ),
 ( 0.2000000000000000666, 0.2083333333333333981, 0.2166666666666667018, 0.2250000000000000333, 0.2333333333333333648, 0.2416666666666666963, 0.2500000000000000000 ),
 .UNSPECIFIED. ) 
 CURVE ( )  GEOMETRIC_REPRESENTATION_ITEM ( )  RATIONAL_B_SPLINE_CURVE ( ( 0.9999999999999997780, 0.9659258262890685343, 1.000000000000000000, 0.9659258262890683122, 1.000000000000000000, 0.9659258262890683122, 1.000000000000000000, 0.9659258262890683122, 1.000000000000000000, 0.9659258262890683122, 1.000000000000000000, 0.9659258262890683122, 1.000000000000000000 ) ) 
 REPRESENTATION_ITEM ( '' )  );
#14869 = ORIENTED_EDGE ( 'NONE', *, *, #130400, .F. ) ;
#14870 = EDGE_CURVE ( 'NONE', #37393, #36041, #2862, .T. ) ;
#14871 = VECTOR ( 'NONE', #25447, 1000.000000000000000 ) ;
#14872 = FACE_BOUND ( 'NONE', #46012, .T. ) ;
#14873 = EDGE_CURVE ( 'NONE', #110076, #59821, #95462, .T. ) ;
#14874 = DIRECTION ( 'NONE',  ( -0.7071067811865486830, 0.7071067811865464625, 0.000000000000000000 ) ) ;
#14875 = DIRECTION ( 'NONE',  ( 0.6830127018922180770, -0.6830127018922204085, -0.2588190451025213501 ) ) ;
#14876 = DIRECTION ( 'NONE',  ( 0.7071067811865487940, 0.7071067811865463515, 0.000000000000000000 ) ) ;
#14877 = LINE ( 'NONE', #135946, #17930 ) ;
#14878 = AXIS2_PLACEMENT_3D ( 'NONE', #97856, #30460, #31182 ) ;
#14879 = DIRECTION ( 'NONE',  ( 0.4153784070974592124, 0.7373070763208220413, 0.5327654776019358218 ) ) ;
#14880 = ORIENTED_EDGE ( 'NONE', *, *, #106291, .T. ) ;
#14881 = AXIS2_PLACEMENT_3D ( 'NONE', #37965, #69905, #48121 ) ;
#14882 = ORIENTED_EDGE ( 'NONE', *, *, #38940, .F. ) ;
#14883 = CARTESIAN_POINT ( 'NONE',  ( 91.49543019189812298, 5.291415217122916737, 3.055000000000001936 ) ) ;
#14884 = ORIENTED_EDGE ( 'NONE', *, *, #115141, .T. ) ;
#14885 = EDGE_CURVE ( 'NONE', #66262, #20118, #62144, .T. ) ;
#14886 = CARTESIAN_POINT ( 'NONE',  ( -51.48921356237309510, -27.52281430457091460, 5.000000000000000000 ) ) ;
#14887 = CARTESIAN_POINT ( 'NONE',  ( -57.29974487139158157, -27.71228299555246011, 4.000000000000000000 ) ) ;
#14888 = EDGE_CURVE ( 'NONE', #140709, #14666, #111377, .T. ) ;
#14889 = CARTESIAN_POINT ( 'NONE',  ( -19.49999999999986500, -13.53360074219760101, 5.000000000000000000 ) ) ;
#14890 = CARTESIAN_POINT ( 'NONE',  ( -9.328169399223465774, 8.259292476615632594, 4.000000000000000000 ) ) ;
#14891 = ORIENTED_EDGE ( 'NONE', *, *, #131385, .T. ) ;
#14892 = DIRECTION ( 'NONE',  ( 0.000000000000000000, 0.000000000000000000, 1.000000000000000000 ) ) ;
#14893 =( LENGTH_UNIT ( ) NAMED_UNIT ( * ) SI_UNIT ( .MILLI., .METRE. ) );
#14894 = CARTESIAN_POINT ( 'NONE',  ( 25.40000000000000213, 7.917808315101192207, 0.6621923558222658768 ) ) ;
#14895 = CARTESIAN_POINT ( 'NONE',  ( 1.589909354801671171, 9.759292476615625489, 11.28811694763778917 ) ) ;
#14896 = EDGE_CURVE ( 'NONE', #95968, #78911, #27337, .T. ) ;
#14897 = CARTESIAN_POINT ( 'NONE',  ( 28.49999999999980460, 4.466399257802221356, 5.000000000000000000 ) ) ;
#14898 = ORIENTED_EDGE ( 'NONE', *, *, #36665, .F. ) ;
#14899 = LINE ( 'NONE', #28665, #19502 ) ;
#14900 = CARTESIAN_POINT ( 'NONE',  ( 18.18398860626898994, 28.73617430169800002, 5.000000000000000000 ) ) ;
#14901 = ORIENTED_EDGE ( 'NONE', *, *, #101781, .T. ) ;
#14902 = VERTEX_POINT ( 'NONE', #140399 ) ;
#14903 = VERTEX_POINT ( 'NONE', #128117 ) ;
#14904 = EDGE_CURVE ( 'NONE', #31251, #74191, #104915, .T. ) ;
#14905 = CARTESIAN_POINT ( 'NONE',  ( 45.64626352523142572, -4.472830434245840259, 4.472830434245838482 ) ) ;
#14906 = EDGE_CURVE ( 'NONE', #94849, #96996, #125975, .T. ) ;
#14907 = ORIENTED_EDGE ( 'NONE', *, *, #62044, .T. ) ;
#14908 = EDGE_CURVE ( 'NONE', #134689, #141054, #128804, .T. ) ;
#14909 = CARTESIAN_POINT ( 'NONE',  ( 5.149972949537104938, -4.461849672132299105, 4.461849672132299993 ) ) ;
#14910 = VERTEX_POINT ( 'NONE', #72343 ) ;
#14911 = DIRECTION ( 'NONE',  ( 0.7071067811865486830, -0.7071067811865464625, -0.000000000000000000 ) ) ;
#14912 = VERTEX_POINT ( 'NONE', #105603 ) ;
#14913 = DIRECTION ( 'NONE',  ( -0.7071067811865486830, -0.7071067811865464625, 0.000000000000000000 ) ) ;
#14914 = CARTESIAN_POINT ( 'NONE',  ( 34.92499999999998295, -3.281509562795708934, 4.759050581649326261 ) ) ;
#14916 = ORIENTED_EDGE ( 'NONE', *, *, #95497, .F. ) ;
#14915 = FACE_OUTER_BOUND ( 'NONE', #75733, .T. ) ;
#14917 = EDGE_LOOP ( 'NONE', ( #84322, #126542, #26760, #100109 ) ) ;
#14918 = AXIS2_PLACEMENT_3D ( 'NONE', #83390, #61657, #105128 ) ;
#14919 = DIRECTION ( 'NONE',  ( -0.7071067811865486830, -0.7071067811865464625, -0.000000000000000000 ) ) ;
#14920 = PLANE ( 'NONE',  #39132 ) ;
#14921 = CARTESIAN_POINT ( 'NONE',  ( 124.8912635252314516, -4.472830434245839371, -4.472830434245839371 ) ) ;
#14922 = ORIENTED_EDGE ( 'NONE', *, *, #122586, .F. ) ;
#14923 = FACE_OUTER_BOUND ( 'NONE', #19536, .T. ) ;
#14924 = ORIENTED_EDGE ( 'NONE', *, *, #107260, .F. ) ;
#14925 = ORIENTED_EDGE ( 'NONE', *, *, #4452, .F. ) ;
#14926 = ORIENTED_EDGE ( 'NONE', *, *, #24125, .F. ) ;
#14927 = ORIENTED_EDGE ( 'NONE', *, *, #36879, .T. ) ;
#14928 = SURFACE_STYLE_USAGE ( .BOTH. , #70089 ) ;
#14929 = FACE_OUTER_BOUND ( 'NONE', #138940, .T. ) ;
#14930 = CARTESIAN_POINT ( 'NONE',  ( -0.3281693992235289459, 11.25929247661561305, 4.000000000000000000 ) ) ;
#14931 = LINE ( 'NONE', #101233, #115700 ) ;
#14932 = CARTESIAN_POINT ( 'NONE',  ( -11.99999999999990585, -8.151047557385080466, -8.977947279169770312 ) ) ;
#14933 = ORIENTED_EDGE ( 'NONE', *, *, #58807, .F. ) ;
#14934 = AXIS2_PLACEMENT_3D ( 'NONE', #5264, #15412, #127058 ) ;
#14935 = DIRECTION ( 'NONE',  ( -0.000000000000000000, 0.000000000000000000, 1.000000000000000000 ) ) ;
#14936 = AXIS2_PLACEMENT_3D ( 'NONE', #5164, #92922, #49461 ) ;
#14937 = CARTESIAN_POINT ( 'NONE',  ( 18.64540314143522437, -2.126176841940958351, -7.934999999999989839 ) ) ;
#14938 = LINE ( 'NONE', #90368, #136538 ) ;
#14939 = CARTESIAN_POINT ( 'NONE',  ( 11.99999999999991296, -12.03360074219761700, 5.000000000000000000 ) ) ;
#14940 = ORIENTED_EDGE ( 'NONE', *, *, #29800, .F. ) ;
#14941 = AXIS2_PLACEMENT_3D ( 'NONE', #51028, #6041, #105385 ) ;
#14942 = ORIENTED_EDGE ( 'NONE', *, *, #42892, .T. ) ;
#14943 = EDGE_CURVE ( 'NONE', #90863, #82492, #117891, .T. ) ;
#14944 = EDGE_LOOP ( 'NONE', ( #56018, #119212, #80529, #85160 ) ) ;
#14945 = DIRECTION ( 'NONE',  ( 0.000000000000000000, 0.000000000000000000, -1.000000000000000000 ) ) ;
#14946 = DIRECTION ( 'NONE',  ( -0.7071067811865486830, -0.7071067811865464625, -0.000000000000000000 ) ) ;
#14947 = DIRECTION ( 'NONE',  ( -1.000000000000000000, 0.000000000000000000, 0.000000000000000000 ) ) ;
#14948 = DIRECTION ( 'NONE',  ( -0.7071067811865486830, -0.7071067811865464625, -0.000000000000000000 ) ) ;
#14949 = DIRECTION ( 'NONE',  ( 1.000000000000000000, 1.224606353822377258E-16, 0.000000000000000000 ) ) ;
#14950 = CARTESIAN_POINT ( 'NONE',  ( -14.67183060077637080, -12.74070752338415602, 4.000000000000000000 ) ) ;
#14951 = FACE_OUTER_BOUND ( 'NONE', #128698, .T. ) ;
#14952 = DIRECTION ( 'NONE',  ( 0.7071067811865487940, 0.7071067811865463515, 0.000000000000000000 ) ) ;
#14953 = VECTOR ( 'NONE', #85205, 1000.000000000000114 ) ;
#14954 = DIRECTION ( 'NONE',  ( 0.3543493200069163240, -0.000000000000000000, 0.9351131265310288487 ) ) ;
#14955 = CARTESIAN_POINT ( 'NONE',  ( 17.85999999999999943, 2.055000000000001492, 2.516649172247811554E-16 ) ) ;
#14956 = CARTESIAN_POINT ( 'NONE',  ( -27.12147316337130221, -20.24070752338407075, 7.412974875817854858 ) ) ;
#14957 = VERTEX_POINT ( 'NONE', #71590 ) ;
#14958 = CARTESIAN_POINT ( 'NONE',  ( 19.39435622689822480, 0.5802795747914162305, -30.75303128506508088 ) ) ;
#14959 = EDGE_LOOP ( 'NONE', ( #16524, #136120, #116740, #142683 ) ) ;
#14960 = LINE ( 'NONE', #81700, #2011 ) ;
#14962 = ORIENTED_EDGE ( 'NONE', *, *, #15351, .F. ) ;
#14961 = CARTESIAN_POINT ( 'NONE',  ( -1.499999999999984013, 3.052185695429136647, 5.000000000000000000 ) ) ;
#14963 = EDGE_CURVE ( 'NONE', #19198, #133116, #17199, .T. ) ;
#14964 = CARTESIAN_POINT ( 'NONE',  ( 18.32266436734346726, -2.055000000000000160, 0.000000000000000000 ) ) ;
#14965 = DIRECTION ( 'NONE',  ( 0.000000000000000000, 0.06845965770171351383, 0.9976538855070752332 ) ) ;
#14966 = EDGE_LOOP ( 'NONE', ( #104057, #131918, #31732, #124404, #16257, #62113 ) ) ;
#14967 = EDGE_CURVE ( 'NONE', #73784, #106314, #15714, .T. ) ;
#14968 = CARTESIAN_POINT ( 'NONE',  ( 45.48921356237309510, -27.52281430457087197, 5.000000000000000000 ) ) ;
#14969 = ORIENTED_EDGE ( 'NONE', *, *, #43848, .F. ) ;
#14970 = DIRECTION ( 'NONE',  ( 0.7071067811865486830, -0.7071067811865464625, -0.000000000000000000 ) ) ;
#14971 = ORIENTED_EDGE ( 'NONE', *, *, #104059, .F. ) ;
#14972 = DIRECTION ( 'NONE',  ( -0.7071067811865486830, -0.7071067811865464625, 0.000000000000000000 ) ) ;
#14973 = AXIS2_PLACEMENT_3D ( 'NONE', #58395, #102578, #136599 ) ;
#14974 = CARTESIAN_POINT ( 'NONE',  ( 102.4541937171295700, 6.884901960086283523, 3.975000000000002753 ) ) ;
#14976 = AXIS2_PLACEMENT_3D ( 'NONE', #89305, #22575, #112484 ) ;
#14975 = DIRECTION ( 'NONE',  ( -0.7071067811865487940, 0.7071067811865463515, 0.000000000000000000 ) ) ;
#14977 = AXIS2_PLACEMENT_3D ( 'NONE', #76499, #21389, #61534 ) ;
#14978 = CARTESIAN_POINT ( 'NONE',  ( 63.18398860626900415, 28.73617430169831621, 5.000000000000000000 ) ) ;
#14979 = ORIENTED_EDGE ( 'NONE', *, *, #65120, .F. ) ;
#14981 = EDGE_CURVE ( 'NONE', #61902, #34556, #94029, .T. ) ;
#14980 = VECTOR ( 'NONE', #54330, 1000.000000000000000 ) ;
#14982 = CARTESIAN_POINT ( 'NONE',  ( -23.99999999999982592, -22.06887692260758982, 4.000000000000000000 ) ) ;
#14983 = CARTESIAN_POINT ( 'NONE',  ( 2.510786437626908008, -27.52281430457053446, 5.000000000000000000 ) ) ;
#14984 = CARTESIAN_POINT ( 'NONE',  ( 20.20710678118641113, -8.240707523384191546, 5.000000000000000000 ) ) ;
#14985 = CARTESIAN_POINT ( 'NONE',  ( 26.68750000000000355, 4.461849672132297329, -4.461849672132302658 ) ) ;
#14986 = CARTESIAN_POINT ( 'NONE',  ( -9.489213562373095101, -27.52281430457062328, 5.000000000000000000 ) ) ;
#14987 = DIRECTION ( 'NONE',  ( 0.7071067811865486830, -0.7071067811865464625, -0.000000000000000000 ) ) ;
#14988 = PLANE ( 'NONE',  #43264 ) ;
#14989 = ORIENTED_EDGE ( 'NONE', *, *, #124322, .F. ) ;
#14990 = EDGE_CURVE ( 'NONE', #65015, #3074, #38952, .T. ) ;
#14991 = DIRECTION ( 'NONE',  ( -0.7071067811865486830, -0.7071067811865464625, 0.000000000000000000 ) ) ;
#14992 = ORIENTED_EDGE ( 'NONE', *, *, #116380, .F. ) ;
#14993 = CARTESIAN_POINT ( 'NONE',  ( 96.54209685856477563, 5.291415217122923842, -3.054999999999996163 ) ) ;
#14994 = LINE ( 'NONE', #61423, #33877 ) ;
#14995 = FACE_OUTER_BOUND ( 'NONE', #69529, .T. ) ;
#14996 = FACE_OUTER_BOUND ( 'NONE', #140776, .T. ) ;
#14997 = EDGE_LOOP ( 'NONE', ( #120596, #131543, #107022 ) ) ;
#14998 = EDGE_CURVE ( 'NONE', #13363, #86911, #117194, .T. ) ;
#14999 = CARTESIAN_POINT ( 'NONE',  ( 0.3605397743886045170, -0.4000000000000003553, 2.166563419957292513 ) ) ;
#15000 = CARTESIAN_POINT ( 'NONE',  ( 8.510786437626906675, -27.52281430457049183, 5.000000000000000000 ) ) ;
#15001 = ORIENTED_EDGE ( 'NONE', *, *, #121744, .T. ) ;
#15002 = CARTESIAN_POINT ( 'NONE',  ( -10.49999999999992895, -2.173586137069142499, -4.605770156576136642 ) ) ;
#15003 = PLANE ( 'NONE',  #7735 ) ;
#15005 = EDGE_LOOP ( 'NONE', ( #61823, #103645, #46896 ) ) ;
#15004 = CARTESIAN_POINT ( 'NONE',  ( -25.39999999999996305, 3.061616997868383141E-16, -2.500000000000000000 ) ) ;
#15006 = CARTESIAN_POINT ( 'NONE',  ( 29.99999999999979039, 20.70535890316563865, 1.956823837851847214 ) ) ;
#15007 = EDGE_CURVE ( 'NONE', #104985, #45577, #6984, .T. ) ;
#15008 = CARTESIAN_POINT ( 'NONE',  ( 24.39999999999999858, 1.194621026894846283, 17.40906030209848510 ) ) ;
#15009 = DIRECTION ( 'NONE',  ( -0.7071067811865486830, -0.7071067811865464625, -0.000000000000000000 ) ) ;
#15010 = DIRECTION ( 'NONE',  ( 0.000000000000000000, 1.000000000000000000, 0.000000000000000000 ) ) ;
#15011 = ORIENTED_EDGE ( 'NONE', *, *, #112706, .T. ) ;
#15012 = ORIENTED_EDGE ( 'NONE', *, *, #113395, .F. ) ;
#15013 = ORIENTED_EDGE ( 'NONE', *, *, #67381, .T. ) ;
#15014 = CARTESIAN_POINT ( 'NONE',  ( 85.45876352523143282, 0.000000000000000000, -6.110000000000001208 ) ) ;
#15015 = EDGE_LOOP ( 'NONE', ( #139587, #61648, #88616, #27870 ) ) ;
#15016 = CYLINDRICAL_SURFACE ( 'NONE', #123851, 0.5000000000000004441 ) ;
#15017 = EDGE_CURVE ( 'NONE', #105758, #100682, #137563, .T. ) ;
#15018 = DIRECTION ( 'NONE',  ( -0.7071067811865486830, -0.7071067811865464625, -0.000000000000000000 ) ) ;
#15019 = CARTESIAN_POINT ( 'NONE',  ( -18.18398860626898994, 28.73617430169800002, 5.000000000000000000 ) ) ;
#15020 = DIRECTION ( 'NONE',  ( 0.7071067811865486830, -0.7071067811865464625, -0.000000000000000000 ) ) ;
#15021 = ORIENTED_EDGE ( 'NONE', *, *, #84871, .F. ) ;
#15022 = CARTESIAN_POINT ( 'NONE',  ( 0.000000000000000000, 0.000000000000000000, 5.000000000000000000 ) ) ;
#15023 = DIRECTION ( 'NONE',  ( -0.7071067811865486830, -0.7071067811865464625, 0.000000000000000000 ) ) ;
#15024 = EDGE_CURVE ( 'NONE', #106541, #47360, #17872, .T. ) ;
#15025 = ADVANCED_FACE ( 'NONE', ( #109910 ), #2499, .T. ) ;
#15026 = CARTESIAN_POINT ( 'NONE',  ( 75.59959685856478018, -6.109999999999997655, -1.637169565754160283 ) ) ;
#15027 = ORIENTED_EDGE ( 'NONE', *, *, #51417, .F. ) ;
#15028 = CARTESIAN_POINT ( 'NONE',  ( -25.49999999999982947, 22.22500000000000853, 4.362957392718830540 ) ) ;
#15029 = LINE ( 'NONE', #72334, #1494 ) ;
#15030 = CARTESIAN_POINT ( 'NONE',  ( 51.18398860626899705, 28.73617430169823095, 5.000000000000000000 ) ) ;
#15031 = EDGE_CURVE ( 'NONE', #133316, #83142, #68399, .T. ) ;
#15032 = EDGE_LOOP ( 'NONE', ( #63072, #69489, #55944, #59862 ) ) ;
#15033 = EDGE_LOOP ( 'NONE', ( #141267, #131669, #9013, #77609 ) ) ;
#15034 = CARTESIAN_POINT ( 'NONE',  ( 24.71230993966010914, -21.73547319004781997, 4.999917730833664642 ) ) ;
#15035 = EDGE_CURVE ( 'NONE', #128295, #76093, #9119, .T. ) ;
#15036 = ADVANCED_FACE ( 'NONE', ( #54148 ), #65747, .F. ) ;
#15037 = DIRECTION ( 'NONE',  ( 1.000000000000000000, -0.000000000000000000, 0.000000000000000000 ) ) ;
#15038 = CARTESIAN_POINT ( 'NONE',  ( -15.51168605928422295, 6.759292476615645917, 16.35960578974473023 ) ) ;
#15039 = CYLINDRICAL_SURFACE ( 'NONE', #73555, 34.93000000000001393 ) ;
#15040 = CARTESIAN_POINT ( 'NONE',  ( 11.34328999833780394, 3.759292476615688550, 13.27625715073267898 ) ) ;
#15041 = LINE ( 'NONE', #125251, #118366 ) ;
#15042 = VECTOR ( 'NONE', #129478, 999.9999999999998863 ) ;
#15043 = ORIENTED_EDGE ( 'NONE', *, *, #119802, .T. ) ;
#15044 = ORIENTED_EDGE ( 'NONE', *, *, #73043, .T. ) ;
#15045 = EDGE_CURVE ( 'NONE', #59700, #62370, #65009, .T. ) ;
#15046 = PRESENTATION_LAYER_ASSIGNMENT (  '', '', ( #21987 ) ) ;
#15047 = DIRECTION ( 'NONE',  ( 0.7071067811865486830, -0.7071067811865464625, -0.000000000000000000 ) ) ;
#15048 = VERTEX_POINT ( 'NONE', #131679 ) ;
#15049 = EDGE_CURVE ( 'NONE', #17476, #118799, #10573, .T. ) ;
#15050 = CARTESIAN_POINT ( 'NONE',  ( -7.499999999999944045, -10.53360074219763121, 5.000000000000000000 ) ) ;
#15051 = ORIENTED_EDGE ( 'NONE', *, *, #117649, .F. ) ;
#15052 = VECTOR ( 'NONE', #100745, 1000.000000000000000 ) ;
#15053 = DIRECTION ( 'NONE',  ( -0.7071067811865486830, 0.7071067811865464625, 0.000000000000000000 ) ) ;
#15054 = PLANE ( 'NONE',  #142146 ) ;
#15055 = DIRECTION ( 'NONE',  ( -0.6830127018922180770, -0.6830127018922204085, -0.2588190451025213501 ) ) ;
#15056 = DIRECTION ( 'NONE',  ( 0.6830127018922180770, -0.6830127018922204085, -0.2588190451025213501 ) ) ;
#15057 = ORIENTED_EDGE ( 'NONE', *, *, #56308, .F. ) ;
#15058 = LINE ( 'NONE', #126675, #84228 ) ;
#15059 = LINE ( 'NONE', #70914, #72002 ) ;
#15060 = ORIENTED_EDGE ( 'NONE', *, *, #75996, .T. ) ;
#15061 = CARTESIAN_POINT ( 'NONE',  ( -32.28769006033950006, -21.73547319004780576, 4.999917730833664642 ) ) ;
#15062 = EDGE_LOOP ( 'NONE', ( #104055, #88309, #66520, #59457, #17516 ) ) ;
#15063 = ORIENTED_EDGE ( 'NONE', *, *, #99659, .T. ) ;
#15064 = FACE_OUTER_BOUND ( 'NONE', #131516, .T. ) ;
#15065 = VERTEX_POINT ( 'NONE', #42549 ) ;
#15066 = EDGE_LOOP ( 'NONE', ( #48630, #24483, #89181, #137375 ) ) ;
#15067 = CARTESIAN_POINT ( 'NONE',  ( -75.18398860626899705, 28.73617430169839793, 5.000000000000000000 ) ) ;
#15068 = ORIENTED_EDGE ( 'NONE', *, *, #68907, .F. ) ;
#15069 = VECTOR ( 'NONE', #23185, 1000.000000000000000 ) ;
#15070 = EDGE_CURVE ( 'NONE', #121941, #129287, #22166, .T. ) ;
#15071 = DIRECTION ( 'NONE',  ( 0.7071067811865486830, -0.7071067811865464625, -0.000000000000000000 ) ) ;
#15073 = EDGE_CURVE ( 'NONE', #57955, #51470, #30950, .T. ) ;
#15072 = AXIS2_PLACEMENT_3D ( 'NONE', #70767, #136696, #114914 ) ;
#15074 = AXIS2_PLACEMENT_3D ( 'NONE', #110643, #20802, #66480 ) ;
#15075 = CARTESIAN_POINT ( 'NONE',  ( -15.48921356237309510, -27.52281430457066236, 5.000000000000000000 ) ) ;
#15076 = CARTESIAN_POINT ( 'NONE',  ( 120.4587635252314328, 0.000000000000000000, -6.110000000000001208 ) ) ;
#15077 = CYLINDRICAL_SURFACE ( 'NONE', #81934, 7.950000000000000178 ) ;
#15078 = AXIS2_PLACEMENT_3D ( 'NONE', #57349, #34152, #111704 ) ;
#15079 = FACE_OUTER_BOUND ( 'NONE', #133185, .T. ) ;
#15080 = DIRECTION ( 'NONE',  ( -0.3543493200069162685, -0.000000000000000000, -0.9351131265310288487 ) ) ;
#15081 = CARTESIAN_POINT ( 'NONE',  ( -26.41358365631583993, -22.22500000000000142, 8.225293826072885395 ) ) ;
#15082 = DIRECTION ( 'NONE',  ( 0.7071067811865487940, -0.7071067811865463515, 0.000000000000000000 ) ) ;
#15083 = SURFACE_STYLE_FILL_AREA ( #105652 ) ;
#15084 = LINE ( 'NONE', #60058, #19652 ) ;
#15085 = ORIENTED_EDGE ( 'NONE', *, *, #79005, .T. ) ;
#15086 = DIRECTION ( 'NONE',  ( 0.3543493200069163240, -0.000000000000000000, 0.9351131265310288487 ) ) ;
#15087 = FACE_OUTER_BOUND ( 'NONE', #127601, .T. ) ;
#15088 = ORIENTED_EDGE ( 'NONE', *, *, #46116, .F. ) ;
#15089 = EDGE_LOOP ( 'NONE', ( #142651, #72666, #135057, #3495, #22723 ) ) ;
#15090 = CYLINDRICAL_SURFACE ( 'NONE', #116615, 2.500000000000000444 ) ;
#15091 = ORIENTED_EDGE ( 'NONE', *, *, #38859, .F. ) ;
#15092 = DIRECTION ( 'NONE',  ( -0.6830127018922181881, 0.6830127018922202975, -0.2588190451025214056 ) ) ;
#15093 = CARTESIAN_POINT ( 'NONE',  ( -84.48921356237309510, -27.52281430457114197, 5.000000000000000000 ) ) ;
#15094 = DIRECTION ( 'NONE',  ( -0.7071067811865487940, 0.7071067811865463515, -0.000000000000000000 ) ) ;
#15095 = PLANE ( 'NONE',  #101985 ) ;
#15096 = ORIENTED_EDGE ( 'NONE', *, *, #49554, .F. ) ;
#15097 = DIRECTION ( 'NONE',  ( -0.3543493200069162685, -0.000000000000000000, -0.9351131265310288487 ) ) ;
#15098 = ORIENTED_EDGE ( 'NONE', *, *, #96479, .T. ) ;
#15099 = DIRECTION ( 'NONE',  ( 0.7071067811865487940, 0.7071067811865463515, 0.000000000000000000 ) ) ;
#15100 = CARTESIAN_POINT ( 'NONE',  ( 29.23373647476855552, 5.808823158059036373, 5.808823158059032821 ) ) ;
#15101 = DIRECTION ( 'NONE',  ( 0.000000000000000000, 0.000000000000000000, 1.000000000000000000 ) ) ;
#15102 = CARTESIAN_POINT ( 'NONE',  ( 14.55624338558763853, -9.434519525233701742, 1.149922814568643981 ) ) ;
#15103 = VERTEX_POINT ( 'NONE', #32362 ) ;
#15104 = VERTEX_POINT ( 'NONE', #132427 ) ;
#15105 = ORIENTED_EDGE ( 'NONE', *, *, #138313, .F. ) ;
#15106 = CARTESIAN_POINT ( 'NONE',  ( 0.000000000000000000, 0.000000000000000000, 9.407735506486140764 ) ) ;
#15107 = DIRECTION ( 'NONE',  ( 1.000000000000000000, -0.000000000000000000, -0.000000000000000000 ) ) ;
#15108 = DIRECTION ( 'NONE',  ( -0.3543493200069163240, 0.000000000000000000, 0.9351131265310288487 ) ) ;
#15109 = FACE_OUTER_BOUND ( 'NONE', #34531, .T. ) ;
#15110 = VERTEX_POINT ( 'NONE', #30206 ) ;
#15111 = LINE ( 'NONE', #93414, #138859 ) ;
#15112 = DIRECTION ( 'NONE',  ( 1.000000000000000000, 0.000000000000000000, 0.000000000000000000 ) ) ;
#15113 = CARTESIAN_POINT ( 'NONE',  ( 57.18398860626899705, 28.73617430169827358, 5.000000000000000000 ) ) ;
#15114 = LINE ( 'NONE', #70971, #53563 ) ;
#15115 = PLANE ( 'NONE',  #12105 ) ;
#15116 = ORIENTED_EDGE ( 'NONE', *, *, #119010, .T. ) ;
#15117 = CARTESIAN_POINT ( 'NONE',  ( -57.18398860626899705, 28.73617430169827358, 5.000000000000000000 ) ) ;
#15118 = VERTEX_POINT ( 'NONE', #99745 ) ;
#15119 = EDGE_CURVE ( 'NONE', #68468, #140795, #141097, .T. ) ;
#15121 = ORIENTED_EDGE ( 'NONE', *, *, #50073, .T. ) ;
#15120 =( NAMED_UNIT ( * ) PLANE_ANGLE_UNIT ( ) SI_UNIT ( $, .RADIAN. ) );
#15122 = VERTEX_POINT ( 'NONE', #120033 ) ;
#15123 = EDGE_CURVE ( 'NONE', #10977, #114516, #41809, .T. ) ;
#15124 = ADVANCED_FACE ( 'NONE', ( #130261 ), #75180, .F. ) ;
#15125 = LINE ( 'NONE', #121227, #104757 ) ;
#15126 = CARTESIAN_POINT ( 'NONE',  ( -25.49999999999981881, 6.277155672890249782, -3.510561720658882834 ) ) ;
#15127 = DIRECTION ( 'NONE',  ( 0.7071067811865487940, 0.7071067811865463515, 0.000000000000000000 ) ) ;
#15128 = EDGE_LOOP ( 'NONE', ( #88686, #80502, #66759, #97087, #106301 ) ) ;
#15129 = DIRECTION ( 'NONE',  ( -1.000000000000000000, -0.000000000000000000, 0.000000000000000000 ) ) ;
#15130 = ORIENTED_EDGE ( 'NONE', *, *, #67320, .F. ) ;
#15131 = EDGE_CURVE ( 'NONE', #42602, #62992, #412, .T. ) ;
#15132 = EDGE_CURVE ( 'NONE', #44266, #129569, #85286, .T. ) ;
#15133 = DIRECTION ( 'NONE',  ( 0.000000000000000000, -1.000000000000000000, 0.000000000000000000 ) ) ;
#15134 = LINE ( 'NONE', #4210, #62433 ) ;
#15135 = VECTOR ( 'NONE', #66225, 1000.000000000000114 ) ;
#15136 = CARTESIAN_POINT ( 'NONE',  ( 29.22459685856478018, -1.637169565754161171, 6.109999999999998543 ) ) ;
#15137 = DIRECTION ( 'NONE',  ( 0.6830127018922181881, 0.6830127018922202975, -0.2588190451025214056 ) ) ;
#15138 = LINE ( 'NONE', #2847, #113085 ) ;
#15139 = VECTOR ( 'NONE', #1107, 1000.000000000000000 ) ;
#15140 = ADVANCED_FACE ( 'NONE', ( #142561 ), #107753, .T. ) ;
#15141 = CARTESIAN_POINT ( 'NONE',  ( 53.99451991528749062, 28.92564299267975869, 4.000000000000000000 ) ) ;
#15142 = DIRECTION ( 'NONE',  ( -0.7071067811865487940, 0.7071067811865463515, -0.000000000000000000 ) ) ;
#15143 = LINE ( 'NONE', #58001, #85355 ) ;
#15144 = CARTESIAN_POINT ( 'NONE',  ( 26.81206980810188512, 7.934999999999993392, 2.126176841940951689 ) ) ;
#15145 = DIRECTION ( 'NONE',  ( 1.000000000000000000, 0.000000000000000000, 0.000000000000000000 ) ) ;
#15146 = CARTESIAN_POINT ( 'NONE',  ( 0.7071067811865398012, -6.740707523384219968, 5.000000000000000000 ) ) ;
#15147 = DIRECTION ( 'NONE',  ( -0.6830127018922181881, 0.6830127018922202975, -0.2588190451025214056 ) ) ;
#15148 = CARTESIAN_POINT ( 'NONE',  ( -29.24139925780183091, 21.72500000000000853, 5.000000000000000000 ) ) ;
#15149 = ORIENTED_EDGE ( 'NONE', *, *, #86582, .T. ) ;
#15150 = ORIENTED_EDGE ( 'NONE', *, *, #28617, .T. ) ;
#15151 =( BOUNDED_CURVE ( )  B_SPLINE_CURVE ( 2, ( #63290, #29185, #16134, #106726, #127812, #74129, #61844, #27042, #129199, #116908, #6674, #29886, #118323 ),
 .UNSPECIFIED., .F., .T. ) 
 B_SPLINE_CURVE_WITH_KNOTS ( ( 3, 2, 2, 2, 2, 2, 3 ),
 ( 0.6999999999999999556, 0.7027777777777777235, 0.7055555555555556024, 0.7083333333333333703, 0.7111111111111111382, 0.7138888888888889062, 0.7166666666666666741 ),
 .UNSPECIFIED. ) 
 CURVE ( )  GEOMETRIC_REPRESENTATION_ITEM ( )  RATIONAL_B_SPLINE_CURVE ( ( 1.000000000000000000, 0.9659258262890683122, 1.000000000000000000, 0.9659258262890683122, 1.000000000000000000, 0.9659258262890683122, 1.000000000000000000, 0.9659258262890683122, 1.000000000000000000, 0.9659258262890683122, 1.000000000000000000, 0.9659258262890683122, 1.000000000000000000 ) ) 
 REPRESENTATION_ITEM ( '' )  );
#15153 = ADVANCED_FACE ( 'NONE', ( #25029 ), #59148, .F. ) ;
#15152 = CARTESIAN_POINT ( 'NONE',  ( 87.91666666666667140, -6.884901960086287076, -3.975000000000000977 ) ) ;
#15154 = ORIENTED_EDGE ( 'NONE', *, *, #140228, .T. ) ;
#15155 = VECTOR ( 'NONE', #28744, 999.9999999999998863 ) ;
#15156 = VERTEX_POINT ( 'NONE', #25754 ) ;
#15157 = CARTESIAN_POINT ( 'NONE',  ( -10.49999999999992184, 22.01701374228154862, 2.453858888625655599 ) ) ;
#15158 = CARTESIAN_POINT ( 'NONE',  ( 23.23330628287043709, -6.094999999999989981, -1.633150327867689322 ) ) ;
#15159 = CARTESIAN_POINT ( 'NONE',  ( -21.48921356237309155, -27.52281430457070499, 5.000000000000000000 ) ) ;
#15160 = ORIENTED_EDGE ( 'NONE', *, *, #25989, .F. ) ;
#15161 = EDGE_CURVE ( 'NONE', #116464, #124871, #89581, .T. ) ;
#15162 = LINE ( 'NONE', #89190, #124997 ) ;
#15163 = CARTESIAN_POINT ( 'NONE',  ( 0.000000000000000000, 0.000000000000000000, 5.000000000000000000 ) ) ;
#15164 = CARTESIAN_POINT ( 'NONE',  ( 24.29974487139158867, -27.71228299555223273, 4.000000000000000000 ) ) ;
#15165 = DIRECTION ( 'NONE',  ( -1.000000000000000000, -0.000000000000000000, -0.000000000000000000 ) ) ;
#15166 = LINE ( 'NONE', #81921, #49402 ) ;
#15167 = DIRECTION ( 'NONE',  ( -0.000000000000000000, 0.000000000000000000, 1.000000000000000000 ) ) ;
#15168 = DIRECTION ( 'NONE',  ( -0.6830127018922180770, -0.6830127018922204085, -0.2588190451025213501 ) ) ;
#15169 = EDGE_CURVE ( 'NONE', #108750, #129128, #36625, .T. ) ;
#15170 = DIRECTION ( 'NONE',  ( 0.6830127018922181881, 0.6830127018922202975, -0.2588190451025214056 ) ) ;
#15171 = CARTESIAN_POINT ( 'NONE',  ( 34.49999999999975131, 9.431123077392088661, 4.000000000000000000 ) ) ;
#15172 = CARTESIAN_POINT ( 'NONE',  ( 34.45011844616452379, 9.002304141593850062, 4.999999999999999112 ) ) ;
#15173 = CARTESIAN_POINT ( 'NONE',  ( -30.18398860626900060, 28.73617430169808173, 5.000000000000000000 ) ) ;
#15174 = AXIS2_PLACEMENT_3D ( 'NONE', #560, #89042, #44852 ) ;
#15175 = FACE_OUTER_BOUND ( 'NONE', #39786, .T. ) ;
#15176 = ORIENTED_EDGE ( 'NONE', *, *, #42565, .T. ) ;
#15177 = EDGE_LOOP ( 'NONE', ( #7585, #25003, #24204, #12135 ) ) ;
#15178 = AXIS2_PLACEMENT_3D ( 'NONE', #137710, #70347, #127526 ) ;
#15179 = CARTESIAN_POINT ( 'NONE',  ( 109.8129301918981042, -1.637169565754159617, -6.110000000000001208 ) ) ;
#15180 = VERTEX_POINT ( 'NONE', #56994 ) ;
#15181 = VECTOR ( 'NONE', #2792, 1000.000000000000000 ) ;
#15182 = EDGE_CURVE ( 'NONE', #103350, #330, #35954, .T. ) ;
#15183 = DIRECTION ( 'NONE',  ( 1.000000000000000000, 0.000000000000000000, 0.000000000000000000 ) ) ;
#15184 = AXIS2_PLACEMENT_3D ( 'NONE', #42641, #86839, #77416 ) ;
#15185 = DIRECTION ( 'NONE',  ( 0.7071067811865487940, 0.7071067811865463515, -0.000000000000000000 ) ) ;
#15186 = ORIENTED_EDGE ( 'NONE', *, *, #131358, .T. ) ;
#15187 = CARTESIAN_POINT ( 'NONE',  ( 0.000000000000000000, 0.000000000000000000, 5.000000000000000000 ) ) ;
#15188 = CARTESIAN_POINT ( 'NONE',  ( 1.353980332882009252, 4.584330080086930965E-16, 0.000000000000000000 ) ) ;
#15189 = ADVANCED_FACE ( 'NONE', ( #103300 ), #58447, .F. ) ;
#15190 = CARTESIAN_POINT ( 'NONE',  ( 108.1204301918981230, 3.055000000000001936, -5.291415217122916737 ) ) ;
#15191 = VERTEX_POINT ( 'NONE', #12726 ) ;
#15192 = ADVANCED_FACE ( 'NONE', ( #88904 ), #68577, .F. ) ;
#15193 = ORIENTED_EDGE ( 'NONE', *, *, #54951, .T. ) ;
#15194 = LINE ( 'NONE', #15880, #112542 ) ;
#15195 = DIRECTION ( 'NONE',  ( -0.6830127018922181881, 0.6830127018922202975, -0.2588190451025214056 ) ) ;
#15196 = EDGE_CURVE ( 'NONE', #142313, #48699, #122194, .T. ) ;
#15197 = ORIENTED_EDGE ( 'NONE', *, *, #114829, .T. ) ;
#15198 = ORIENTED_EDGE ( 'NONE', *, *, #36598, .T. ) ;
#15199 = EDGE_LOOP ( 'NONE', ( #76837, #15837, #18483, #10609 ) ) ;
#15200 = DIRECTION ( 'NONE',  ( -0.7071067811865487940, 0.7071067811865463515, 0.000000000000000000 ) ) ;
#15201 = CARTESIAN_POINT ( 'NONE',  ( 2.983736474768552860, -5.808823158059035485, -5.808823158059033709 ) ) ;
#15202 = SURFACE_SIDE_STYLE ('',( #115940 ) ) ;
#15203 = ORIENTED_EDGE ( 'NONE', *, *, #70044, .T. ) ;
#15204 = ORIENTED_EDGE ( 'NONE', *, *, #57198, .F. ) ;
#15205 = EDGE_CURVE ( 'NONE', #128869, #34223, #33802, .T. ) ;
#15206 = DIRECTION ( 'NONE',  ( 0.7071067811865487940, 0.7071067811865463515, -0.000000000000000000 ) ) ;
#15207 = ORIENTED_EDGE ( 'NONE', *, *, #102808, .F. ) ;
#15208 = EDGE_LOOP ( 'NONE', ( #38756, #45143, #117362, #9382 ) ) ;
#15209 = FACE_OUTER_BOUND ( 'NONE', #732, .T. ) ;
#15210 = DIRECTION ( 'NONE',  ( 0.7071067811865486830, -0.7071067811865464625, -0.000000000000000000 ) ) ;
#15211 = EDGE_LOOP ( 'NONE', ( #40459, #99159, #98147, #88160 ) ) ;
#15212 = PLANE ( 'NONE',  #66818 ) ;
#15213 = CARTESIAN_POINT ( 'NONE',  ( 151.4000000000000057, -16.48000000000005016, 0.000000000000000000 ) ) ;
#15214 = FACE_OUTER_BOUND ( 'NONE', #126886, .T. ) ;
#15215 = CARTESIAN_POINT ( 'NONE',  ( 15.05159235450332034, 9.902892378096218942E-16, 0.000000000000000000 ) ) ;
#15216 = ADVANCED_FACE ( 'NONE', ( #67134 ), #23614, .F. ) ;
#15217 = FACE_BOUND ( 'NONE', #55286, .T. ) ;
#15218 = VERTEX_POINT ( 'NONE', #100480 ) ;
#15219 = DIRECTION ( 'NONE',  ( -0.000000000000000000, 0.3543493200069153248, 0.9351131265310292928 ) ) ;
#15220 = CARTESIAN_POINT ( 'NONE',  ( 0.9387689034200080718, -0.4000000000000003553, 2.166563668000045961 ) ) ;
#15221 = DIRECTION ( 'NONE',  ( 0.7071067811865486830, -0.7071067811865464625, -0.000000000000000000 ) ) ;
#15222 = ORIENTED_EDGE ( 'NONE', *, *, #130896, .T. ) ;
#15223 = CARTESIAN_POINT ( 'NONE',  ( 1.199999999999999956, 0.000000000000000000, 0.000000000000000000 ) ) ;
#15224 = ORIENTED_EDGE ( 'NONE', *, *, #8422, .T. ) ;
#15225 = ORIENTED_EDGE ( 'NONE', *, *, #125237, .F. ) ;
#15226 = ORIENTED_EDGE ( 'NONE', *, *, #10804, .F. ) ;
#15227 = AXIS2_PLACEMENT_3D ( 'NONE', #138905, #136023, #61378 ) ;
#15228 = EDGE_CURVE ( 'NONE', #99670, #36919, #1128, .T. ) ;
#15229 = CARTESIAN_POINT ( 'NONE',  ( 39.87043019189810877, -3.055000000000001492, 5.291415217122917625 ) ) ;
#15230 = ORIENTED_EDGE ( 'NONE', *, *, #85897, .F. ) ;
#15231 = CARTESIAN_POINT ( 'NONE',  ( 7.499999999999951150, 8.319652575858395238, -8.582050562765809687 ) ) ;
#15232 = MECHANICAL_DESIGN_GEOMETRIC_PRESENTATION_REPRESENTATION (  '', ( #98562 ), #57005 ) ;
#15233 = DIRECTION ( 'NONE',  ( 0.6830127018922181881, 0.6830127018922202975, -0.2588190451025214056 ) ) ;
#15234 = CARTESIAN_POINT ( 'NONE',  ( 8.423184310185783730, 2.500000000000000444, 0.000000000000000000 ) ) ;
#15235 = ORIENTED_EDGE ( 'NONE', *, *, #2526, .T. ) ;
#15236 = LINE ( 'NONE', #36318, #125533 ) ;
#15237 = FACE_OUTER_BOUND ( 'NONE', #7983, .T. ) ;
#15238 = DIRECTION ( 'NONE',  ( -0.7071067811865486830, -0.7071067811865464625, 0.000000000000000000 ) ) ;
#15239 = ADVANCED_FACE ( 'NONE', ( #133812 ), #34498, .T. ) ;
#15240 = DIRECTION ( 'NONE',  ( 1.000000000000000000, 0.000000000000000000, 0.000000000000000000 ) ) ;
#15241 = CARTESIAN_POINT ( 'NONE',  ( 12.79289321881337038, -14.24070752338414003, 5.000000000000000000 ) ) ;
#15242 = FACE_OUTER_BOUND ( 'NONE', #55535, .T. ) ;
#15243 = DIRECTION ( 'NONE',  ( -0.7071067811865487940, 0.7071067811865463515, 0.000000000000000000 ) ) ;
#15244 = EDGE_LOOP ( 'NONE', ( #13844, #112031, #89544, #102454 ) ) ;
#15245 = EDGE_LOOP ( 'NONE', ( #11463, #44643, #137019, #8292 ) ) ;
#15246 = ORIENTED_EDGE ( 'NONE', *, *, #68640, .T. ) ;
#15247 = ORIENTED_EDGE ( 'NONE', *, *, #92296, .T. ) ;
#15248 = EDGE_LOOP ( 'NONE', ( #130288, #105074, #48002, #21915 ) ) ;
#15249 = ORIENTED_EDGE ( 'NONE', *, *, #112108, .F. ) ;
#15250 = CARTESIAN_POINT ( 'NONE',  ( 45.48921356237309510, -27.52281430457087197, 5.000000000000000000 ) ) ;
#15251 = EDGE_CURVE ( 'NONE', #54369, #7225, #67886, .T. ) ;
#15252 = FACE_OUTER_BOUND ( 'NONE', #35552, .T. ) ;
#15253 = VERTEX_POINT ( 'NONE', #102628 ) ;
#15254 = DIRECTION ( 'NONE',  ( 0.000000000000000000, 0.000000000000000000, 1.000000000000000000 ) ) ;
#15255 = ORIENTED_EDGE ( 'NONE', *, *, #12907, .F. ) ;
#15256 = CARTESIAN_POINT ( 'NONE',  ( -15.71757738642556568, -21.73023691814493219, 5.000000000000000000 ) ) ;
#15257 = CARTESIAN_POINT ( 'NONE',  ( 23.78840764549667597, 9.139736423841732040E-16, 0.000000000000000000 ) ) ;
#15258 = VECTOR ( 'NONE', #16992, 999.9999999999998863 ) ;
#15259 = EDGE_LOOP ( 'NONE', ( #123639, #108229, #116736, #53927 ) ) ;
#15260 = CARTESIAN_POINT ( 'NONE',  ( 97.47459685856478018, 1.637169565754164280, -6.109999999999997655 ) ) ;
#15261 = DIRECTION ( 'NONE',  ( -0.000000000000000000, -0.000000000000000000, 1.000000000000000000 ) ) ;
#15262 = DIRECTION ( 'NONE',  ( -0.000000000000000000, 1.000000000000000000, -0.000000000000000000 ) ) ;
#15263 = ORIENTED_EDGE ( 'NONE', *, *, #70212, .F. ) ;
#15264 = ORIENTED_EDGE ( 'NONE', *, *, #40405, .F. ) ;
#15265 = DIRECTION ( 'NONE',  ( -0.6830127018922181881, 0.6830127018922202975, -0.2588190451025214056 ) ) ;
#15266 = ORIENTED_EDGE ( 'NONE', *, *, #117510, .F. ) ;
#15267 = CARTESIAN_POINT ( 'NONE',  ( -36.48921356237310221, -27.52281430457080802, 5.000000000000000000 ) ) ;
#15268 = VECTOR ( 'NONE', #73310, 1000.000000000000000 ) ;
#15269 = DIRECTION ( 'NONE',  ( -1.000000000000000000, -1.224606353822377258E-16, -0.000000000000000000 ) ) ;
#15270 = DIRECTION ( 'NONE',  ( 0.7071067811865487940, 0.7071067811865463515, 0.000000000000000000 ) ) ;
#15271 = SURFACE_STYLE_FILL_AREA ( #49406 ) ;
#15272 = ORIENTED_EDGE ( 'NONE', *, *, #23042, .T. ) ;
#15273 = CARTESIAN_POINT ( 'NONE',  ( 4.171830600776448961, 6.759292476615649470, 4.000000000000000000 ) ) ;
#15274 = ADVANCED_BREP_SHAPE_REPRESENTATION ( '', ( #46161, #127880 ), #97842 ) ;
#15275 = CARTESIAN_POINT ( 'NONE',  ( 23.99451991528749062, 28.92564299267954908, 4.000000000000000000 ) ) ;
#15276 = DIRECTION ( 'NONE',  ( 1.000000000000000000, 0.000000000000000000, 0.000000000000000000 ) ) ;
#15277 = VERTEX_POINT ( 'NONE', #46112 ) ;
#15278 = CARTESIAN_POINT ( 'NONE',  ( 0.000000000000000000, 0.000000000000000000, 5.000000000000000000 ) ) ;
#15279 = CARTESIAN_POINT ( 'NONE',  ( -33.29974487139158867, -27.71228299555229313, 4.000000000000000000 ) ) ;
#15280 = VERTEX_POINT ( 'NONE', #35241 ) ;
#15282 = VERTEX_POINT ( 'NONE', #112764 ) ;
#15281 = PLANE ( 'NONE',  #141298 ) ;
#15283 = ADVANCED_FACE ( 'NONE', ( #91047 ), #79485, .F. ) ;
#15284 = ADVANCED_FACE ( 'NONE', ( #124360 ), #2552, .F. ) ;
#15285 = EDGE_LOOP ( 'NONE', ( #24096, #17969, #24122, #137167 ) ) ;
#15286 = CARTESIAN_POINT ( 'NONE',  ( -78.18398860626899705, 28.73617430169841924, 5.000000000000000000 ) ) ;
#15287 = CARTESIAN_POINT ( 'NONE',  ( -18.70710678118640402, -3.740707523384248390, 5.000000000000000000 ) ) ;
#15288 = ORIENTED_EDGE ( 'NONE', *, *, #24083, .T. ) ;
#15289 = PLANE ( 'NONE',  #92869 ) ;
#15290 = EDGE_CURVE ( 'NONE', #22900, #73261, #24742, .T. ) ;
#15291 = EDGE_CURVE ( 'NONE', #40384, #134578, #97609, .T. ) ;
#15292 = LINE ( 'NONE', #83455, #61474 ) ;
#15293 =( NAMED_UNIT ( * ) PLANE_ANGLE_UNIT ( ) SI_UNIT ( $, .RADIAN. ) );
#15294 = ADVANCED_FACE ( 'NONE', ( #3949 ), #105441, .T. ) ;
#15295 = ORIENTED_EDGE ( 'NONE', *, *, #45204, .T. ) ;
#15296 = DIRECTION ( 'NONE',  ( 0.7071067811865487940, 0.7071067811865463515, 0.000000000000000000 ) ) ;
#15297 = CARTESIAN_POINT ( 'NONE',  ( 0.4892135623730947680, -27.52281430457055578, 5.000000000000000000 ) ) ;
#15298 = ADVANCED_FACE ( 'NONE', ( #50378 ), #59833, .F. ) ;
#15299 = DIRECTION ( 'NONE',  ( 0.7071067811865487940, -0.7071067811865463515, 0.000000000000000000 ) ) ;
#15300 = FACE_OUTER_BOUND ( 'NONE', #25737, .T. ) ;
#15302 = VECTOR ( 'NONE', #28758, 1000.000000000000000 ) ;
#15301 = DIRECTION ( 'NONE',  ( -0.9707728879609287542, 0.000000000000000000, -0.2399999999999954392 ) ) ;
#15303 = DIRECTION ( 'NONE',  ( 0.7071067811865487940, -0.7071067811865463515, 0.000000000000000000 ) ) ;
#15304 = ADVANCED_FACE ( 'NONE', ( #81595 ), #128644, .F. ) ;
#15305 = CARTESIAN_POINT ( 'NONE',  ( -34.92500000000001137, 4.800094516027155755, 4.759050581649336031 ) ) ;
#15306 = LINE ( 'NONE', #126940, #128724 ) ;
#15307 = ORIENTED_EDGE ( 'NONE', *, *, #106316, .F. ) ;
#15308 = ORIENTED_EDGE ( 'NONE', *, *, #70247, .F. ) ;
#15309 = VERTEX_POINT ( 'NONE', #117726 ) ;
#15311 = ADVANCED_FACE ( 'NONE', ( #27899 ), #6813, .F. ) ;
#15310 = CARTESIAN_POINT ( 'NONE',  ( 121.6041666666666430, 2.130196079827422206, 7.950000000000001954 ) ) ;
#15312 = VERTEX_POINT ( 'NONE', #73558 ) ;
#15313 = ORIENTED_EDGE ( 'NONE', *, *, #31755, .F. ) ;
#15314 = ORIENTED_EDGE ( 'NONE', *, *, #61087, .T. ) ;
#15315 = CIRCLE ( 'NONE', #133443, 9.119999999999999218 ) ;
#15316 = PLANE ( 'NONE',  #57190 ) ;
#15317 = CARTESIAN_POINT ( 'NONE',  ( -34.42500000000001137, -22.22500000000000142, 0.4999999999999995559 ) ) ;
#15318 = VERTEX_POINT ( 'NONE', #17030 ) ;
#15319 = DIRECTION ( 'NONE',  ( -0.000000000000000000, 0.000000000000000000, 1.000000000000000000 ) ) ;
#15320 = ADVANCED_FACE ( 'NONE', ( #16270 ), #115574, .F. ) ;
#15321 = LINE ( 'NONE', #58202, #11565 ) ;
#15322 = CARTESIAN_POINT ( 'NONE',  ( -12.18398860626900060, 28.73617430169795739, 5.000000000000000000 ) ) ;
#15323 = CARTESIAN_POINT ( 'NONE',  ( 110.8337635252314470, 6.110000000000001208, 1.122388791418549305E-15 ) ) ;
#15324 = ORIENTED_EDGE ( 'NONE', *, *, #94215, .T. ) ;
#15325 = CARTESIAN_POINT ( 'NONE',  ( -38.99451991528749062, 28.92564299267965211, 4.000000000000000000 ) ) ;
#15326 = LINE ( 'NONE', #73336, #125697 ) ;
#15327 = LINE ( 'NONE', #48019, #17141 ) ;
#15328 = LINE ( 'NONE', #13194, #142270 ) ;
#15329 = EDGE_CURVE ( 'NONE', #118822, #76747, #5405, .T. ) ;
#15330 = DIRECTION ( 'NONE',  ( -0.7071067811865487940, 0.7071067811865463515, -0.000000000000000000 ) ) ;
#15331 = DIRECTION ( 'NONE',  ( -0.7071067811865486830, -0.7071067811865464625, 0.000000000000000000 ) ) ;
#15332 = CARTESIAN_POINT ( 'NONE',  ( 41.05836038379621300, -7.949999999999997513, -2.130196079827425759 ) ) ;
#15333 = CIRCLE ( 'NONE', #31624, 0.5000000000000004441 ) ;
#15334 = CARTESIAN_POINT ( 'NONE',  ( 17.99451991528748351, 28.92564299267950645, 4.000000000000000000 ) ) ;
#15335 = CARTESIAN_POINT ( 'NONE',  ( 24.39999999999999858, -2.599999999999908606, 1.319531433729349815E-14 ) ) ;
#15336 = ORIENTED_EDGE ( 'NONE', *, *, #33676, .T. ) ;
#15337 = VERTEX_POINT ( 'NONE', #60570 ) ;
#15338 = CARTESIAN_POINT ( 'NONE',  ( 37.31250000000000000, 5.819803920172571310, 5.819803920172575751 ) ) ;
#15339 = VERTEX_POINT ( 'NONE', #49685 ) ;
#15340 = VECTOR ( 'NONE', #6262, 999.9999999999998863 ) ;
#15341 = ORIENTED_EDGE ( 'NONE', *, *, #134623, .F. ) ;
#15342 = LINE ( 'NONE', #138596, #41704 ) ;
#15343 = DIRECTION ( 'NONE',  ( 0.7071067811865486830, -0.7071067811865464625, -0.000000000000000000 ) ) ;
#15344 = ORIENTED_EDGE ( 'NONE', *, *, #110987, .T. ) ;
#15345 = CARTESIAN_POINT ( 'NONE',  ( 17.51078643762690845, -27.52281430457043143, 5.000000000000000000 ) ) ;
#15346 = CARTESIAN_POINT ( 'NONE',  ( 65.99451991528749772, 28.92564299267984396, 4.000000000000000000 ) ) ;
#15347 = DIRECTION ( 'NONE',  ( -0.7071067811865486830, -0.7071067811865464625, 0.000000000000000000 ) ) ;
#15348 = CARTESIAN_POINT ( 'NONE',  ( 33.39626352523143993, 4.472830434245840259, -4.472830434245839371 ) ) ;
#15350 = ORIENTED_EDGE ( 'NONE', *, *, #128077, .F. ) ;
#15349 = MECHANICAL_DESIGN_GEOMETRIC_PRESENTATION_REPRESENTATION (  '', ( #1477 ), #121836 ) ;
#15351 = EDGE_CURVE ( 'NONE', #52228, #103613, #26476, .T. ) ;
#15352 = CARTESIAN_POINT ( 'NONE',  ( -42.29974487139158157, -27.71228299555235708, 4.000000000000000000 ) ) ;
#15353 = ORIENTED_EDGE ( 'NONE', *, *, #50259, .F. ) ;
#15354 = CARTESIAN_POINT ( 'NONE',  ( -57.48921356237308800, -27.52281430457095368, 5.000000000000000000 ) ) ;
#15355 = CARTESIAN_POINT ( 'NONE',  ( -31.49999999999977973, -4.912538124160701791, 4.000000000000000000 ) ) ;
#15356 = EDGE_CURVE ( 'NONE', #97811, #111424, #138095, .T. ) ;
#15357 = DIRECTION ( 'NONE',  ( 0.6830127018922180770, -0.6830127018922204085, -0.2588190451025213501 ) ) ;
#15358 = VERTEX_POINT ( 'NONE', #117042 ) ;
#15359 = ORIENTED_EDGE ( 'NONE', *, *, #76985, .F. ) ;
#15360 = DIRECTION ( 'NONE',  ( 0.6830127018922180770, -0.6830127018922204085, -0.2588190451025213501 ) ) ;
#15361 = CARTESIAN_POINT ( 'NONE',  ( -14.51078643762690490, -27.52281430457045275, 5.000000000000000000 ) ) ;
#15362 = CARTESIAN_POINT ( 'NONE',  ( -18.79289321881332242, 12.75929247661558819, 5.000000000000000000 ) ) ;
#15363 = EDGE_CURVE ( 'NONE', #132813, #128314, #114872, .T. ) ;
#15364 = AXIS2_PLACEMENT_3D ( 'NONE', #74979, #61954, #51786 ) ;
#15365 = VECTOR ( 'NONE', #30759, 1000.000000000000000 ) ;
#15366 = AXIS2_PLACEMENT_3D ( 'NONE', #76202, #43565, #21815 ) ;
#15367 = CARTESIAN_POINT ( 'NONE',  ( 44.53709685856478728, -3.054999999999998828, -5.291415217122919401 ) ) ;
#15368 = ORIENTED_EDGE ( 'NONE', *, *, #124552, .F. ) ;
#15369 = DIRECTION ( 'NONE',  ( -0.7071067811865486830, -0.7071067811865464625, -0.000000000000000000 ) ) ;
#15370 = EDGE_CURVE ( 'NONE', #5088, #117466, #92977, .T. ) ;
#15371 = PLANE ( 'NONE',  #98690 ) ;
#15372 = ORIENTED_EDGE ( 'NONE', *, *, #140821, .T. ) ;
#15373 = ORIENTED_EDGE ( 'NONE', *, *, #97145, .T. ) ;
#15374 = CONICAL_SURFACE ( 'NONE', #107991, 2.500000000000000444, 0.9599310885968830309 ) ;
#15375 = DIRECTION ( 'NONE',  ( -0.000000000000000000, -0.000000000000000000, 1.000000000000000000 ) ) ;
#15376 = ORIENTED_EDGE ( 'NONE', *, *, #123795, .F. ) ;
#15377 = CARTESIAN_POINT ( 'NONE',  ( 28.00000000000002487, -57.14999999999999147, 34.92500000000003268 ) ) ;
#15378 = EDGE_CURVE ( 'NONE', #110710, #5966, #126482, .T. ) ;
#15379 = EDGE_LOOP ( 'NONE', ( #132397, #21798, #9511, #34737 ) ) ;
#15380 = FACE_OUTER_BOUND ( 'NONE', #66183, .T. ) ;
#15381 = SURFACE_STYLE_USAGE ( .BOTH. , #103141 ) ;
#15382 = EDGE_CURVE ( 'NONE', #87580, #102653, #106136, .T. ) ;
#15383 = FACE_BOUND ( 'NONE', #86105, .T. ) ;
#15384 = LINE ( 'NONE', #137218, #85004 ) ;
#15385 = EDGE_CURVE ( 'NONE', #49616, #45081, #35158, .T. ) ;
#15386 = DIRECTION ( 'NONE',  ( 0.3543493200069163240, 0.000000000000000000, -0.9351131265310288487 ) ) ;
#15387 = DIRECTION ( 'NONE',  ( 1.192622389734054877E-16, -1.000000000000000000, 0.000000000000000000 ) ) ;
#15388 = EDGE_CURVE ( 'NONE', #1058, #108205, #32188, .T. ) ;
#15389 = CARTESIAN_POINT ( 'NONE',  ( 26.99999999999982236, -3.412538124160717778, 4.000000000000000000 ) ) ;
#15391 = ORIENTED_EDGE ( 'NONE', *, *, #73426, .T. ) ;
#15390 = LINE ( 'NONE', #39346, #15848 ) ;
#15392 = CARTESIAN_POINT ( 'NONE',  ( 7.499999999999951150, 22.22500000000000142, 4.362957392718792349 ) ) ;
#15393 = ORIENTED_EDGE ( 'NONE', *, *, #25342, .F. ) ;
#15394 = ADVANCED_FACE ( 'NONE', ( #53967 ), #43779, .F. ) ;
#15395 = ORIENTED_EDGE ( 'NONE', *, *, #122396, .F. ) ;
#15396 = CARTESIAN_POINT ( 'NONE',  ( 70.20376352523143737, 6.109999999999998543, 1.122388791418548911E-15 ) ) ;
#15397 = ORIENTED_EDGE ( 'NONE', *, *, #93138, .F. ) ;
#15398 = CARTESIAN_POINT ( 'NONE',  ( 10.49999999999993605, 19.08746187583904330, 4.000000000000000000 ) ) ;
#15399 = CARTESIAN_POINT ( 'NONE',  ( 58.42753753994784205, -47.70829528212276927, -34.92499999999998295 ) ) ;
#15400 = VERTEX_POINT ( 'NONE', #75701 ) ;
#15401 = CARTESIAN_POINT ( 'NONE',  ( 24.20969143188526118, 6.176090689687629975, 5.000000000000000000 ) ) ;
#15402 = AXIS2_PLACEMENT_3D ( 'NONE', #62467, #115361, #6591 ) ;
#15403 = EDGE_CURVE ( 'NONE', #141686, #64292, #97511, .T. ) ;
#15404 = EDGE_CURVE ( 'NONE', #8256, #82515, #98851, .T. ) ;
#15405 = CARTESIAN_POINT ( 'NONE',  ( 25.49999999999982592, 9.431123077392085108, 4.000000000000000000 ) ) ;
#15406 = PLANE ( 'NONE',  #71364 ) ;
#15407 = DIRECTION ( 'NONE',  ( -0.7071067811865486830, -0.7071067811865464625, -0.000000000000000000 ) ) ;
#15408 = DIRECTION ( 'NONE',  ( -0.7071067811865486830, -0.7071067811865464625, -0.000000000000000000 ) ) ;
#15409 = CARTESIAN_POINT ( 'NONE',  ( -45.48921356237309510, -27.52281430457087197, 5.000000000000000000 ) ) ;
#15410 = ORIENTED_EDGE ( 'NONE', *, *, #75777, .F. ) ;
#15411 = ORIENTED_EDGE ( 'NONE', *, *, #69630, .F. ) ;
#15412 = DIRECTION ( 'NONE',  ( -1.000000000000000000, -1.224606353822377258E-16, -0.000000000000000000 ) ) ;
#15413 = CARTESIAN_POINT ( 'NONE',  ( 18.04658813629533043, 14.25929247661557042, 18.84478104361323503 ) ) ;
#15414 = ORIENTED_EDGE ( 'NONE', *, *, #24417, .T. ) ;
#15415 = ORIENTED_EDGE ( 'NONE', *, *, #135373, .F. ) ;
#15416 = ORIENTED_EDGE ( 'NONE', *, *, #23546, .T. ) ;
#15417 = CARTESIAN_POINT ( 'NONE',  ( -54.18398860626899705, 28.73617430169825226, 5.000000000000000000 ) ) ;
#15418 = AXIS2_PLACEMENT_3D ( 'NONE', #10759, #20211, #32556 ) ;
#15419 = EDGE_CURVE ( 'NONE', #57964, #86807, #85841, .T. ) ;
#15420 = LINE ( 'NONE', #81466, #50769 ) ;
#15421 = ORIENTED_EDGE ( 'NONE', *, *, #55307, .F. ) ;
#15422 = DIRECTION ( 'NONE',  ( -0.3543493200069163240, 0.000000000000000000, -0.9351131265310288487 ) ) ;
#15423 = CIRCLE ( 'NONE', #131271, 0.5000000000000004441 ) ;
#15424 = CARTESIAN_POINT ( 'NONE',  ( 9.837903141435219823, -6.871911579029513106, -3.967499999999993587 ) ) ;
#15425 = LINE ( 'NONE', #93746, #102802 ) ;
#15426 = ORIENTED_EDGE ( 'NONE', *, *, #31913, .T. ) ;
#15427 = VECTOR ( 'NONE', #114871, 1000.000000000000000 ) ;
#15428 = PLANE ( 'NONE',  #119808 ) ;
#15429 = CARTESIAN_POINT ( 'NONE',  ( 119.9541937171295700, 6.884901960086283523, 3.975000000000002753 ) ) ;
#15430 = LINE ( 'NONE', #136522, #61406 ) ;
#15432 = ORIENTED_EDGE ( 'NONE', *, *, #123711, .T. ) ;
#15431 = LINE ( 'NONE', #93035, #70387 ) ;
#15433 = PLANE ( 'NONE',  #35589 ) ;
#15434 = ORIENTED_EDGE ( 'NONE', *, *, #84917, .F. ) ;
#15435 = CARTESIAN_POINT ( 'NONE',  ( 0.000000000000000000, 0.000000000000000000, 5.000000000000000000 ) ) ;
#15436 = CARTESIAN_POINT ( 'NONE',  ( -35.99451991528749772, 28.92564299267963079, 4.000000000000000000 ) ) ;
#15437 = PLANE ( 'NONE',  #84137 ) ;
#15438 = VERTEX_POINT ( 'NONE', #130812 ) ;
#15439 = B_SPLINE_CURVE_WITH_KNOTS ( 'NONE', 3,
 ( #21258, #32880, #134319, #123465 ),
 .UNSPECIFIED., .F., .F.,
 ( 4, 4 ),
 ( 0.001975484284630000132, 0.002273591611137678378 ),
 .UNSPECIFIED. ) ;
#15440 = FACE_OUTER_BOUND ( 'NONE', #132918, .T. ) ;
#15441 = FACE_OUTER_BOUND ( 'NONE', #116538, .T. ) ;
#15443 = ADVANCED_FACE ( 'NONE', ( #118467 ), #107593, .F. ) ;
#15442 = FACE_OUTER_BOUND ( 'NONE', #77158, .T. ) ;
#15444 = EDGE_LOOP ( 'NONE', ( #62133, #61120, #142942, #109634 ) ) ;
#15445 = LINE ( 'NONE', #59734, #55558 ) ;
#15446 = DIRECTION ( 'NONE',  ( -0.7071067811865486830, -0.7071067811865464625, 0.000000000000000000 ) ) ;
#15447 = CARTESIAN_POINT ( 'NONE',  ( 6.899972949537105826, 4.461849672132297329, -4.461849672132302658 ) ) ;
#15448 = DIRECTION ( 'NONE',  ( -0.6830127018922180770, -0.6830127018922204085, -0.2588190451025213501 ) ) ;
#15449 = VECTOR ( 'NONE', #122180, 1000.000000000000000 ) ;
#15450 = CYLINDRICAL_SURFACE ( 'NONE', #57579, 6.349999999999999645 ) ;
#15451 = EDGE_LOOP ( 'NONE', ( #3645, #22840, #54968, #71558 ) ) ;
#15452 = ORIENTED_EDGE ( 'NONE', *, *, #108130, .T. ) ;
#15453 = DIRECTION ( 'NONE',  ( -0.7071067811865486830, 0.7071067811865464625, 0.000000000000000000 ) ) ;
#15454 = CARTESIAN_POINT ( 'NONE',  ( 10.49999999999993250, -2.947814304570795851, 5.000000000000000000 ) ) ;
#15455 = CIRCLE ( 'NONE', #17743, 3.999999999999996447 ) ;
#15457 = EDGE_CURVE ( 'NONE', #84629, #64882, #64102, .T. ) ;
#15456 = VECTOR ( 'NONE', #103640, 999.9999999999998863 ) ;
#15458 = CARTESIAN_POINT ( 'NONE',  ( 9.166236474768552966, 7.934999999999990727, -1.457635852685135314E-15 ) ) ;
#15459 = LINE ( 'NONE', #124262, #71414 ) ;
#15461 = ADVANCED_FACE ( 'NONE', ( #40927 ), #86584, .F. ) ;
#15460 = AXIS2_PLACEMENT_3D ( 'NONE', #548, #136074, #113599 ) ;
#15462 = LINE ( 'NONE', #93067, #141090 ) ;
#15463 = DIRECTION ( 'NONE',  ( -0.7071067811865486830, -0.7071067811865464625, 0.000000000000000000 ) ) ;
#15464 = DIRECTION ( 'NONE',  ( 1.000000000000000000, 1.224606353822377258E-16, 0.000000000000000000 ) ) ;
#15465 = EDGE_CURVE ( 'NONE', #60580, #126231, #31479, .T. ) ;
#15466 = EDGE_LOOP ( 'NONE', ( #133658, #119771, #135127, #95629 ) ) ;
#15467 = CARTESIAN_POINT ( 'NONE',  ( 34.92499999999998295, 6.856123077392344278, 4.000000000000000000 ) ) ;
#15468 = VECTOR ( 'NONE', #499, 1000.000000000000227 ) ;
#15469 = EDGE_CURVE ( 'NONE', #25609, #75083, #120589, .T. ) ;
#15470 = DIRECTION ( 'NONE',  ( -0.7071067811865486830, 0.7071067811865464625, 0.000000000000000000 ) ) ;
#15471 = VECTOR ( 'NONE', #126989, 999.9999999999998863 ) ;
#15472 = PLANE ( 'NONE',  #8758 ) ;
#15473 = EDGE_CURVE ( 'NONE', #77841, #44481, #134598, .T. ) ;
#15474 = CARTESIAN_POINT ( 'NONE',  ( 45.99543019189810877, 5.291415217122917625, 3.055000000000002380 ) ) ;
#15475 = CARTESIAN_POINT ( 'NONE',  ( -26.00492477221178689, -5.240707523384232402, 12.38332538355501811 ) ) ;
#15476 = EDGE_LOOP ( 'NONE', ( #131384, #2479, #124770, #134830 ) ) ;
#15477 = CYLINDRICAL_SURFACE ( 'NONE', #169, 28.00000000000002487 ) ;
#15478 = VERTEX_POINT ( 'NONE', #7553 ) ;
#15479 = EDGE_CURVE ( 'NONE', #122031, #20842, #98162, .T. ) ;
#15480 = CARTESIAN_POINT ( 'NONE',  ( 24.18398860626899705, 28.73617430169804265, 5.000000000000000000 ) ) ;
#15481 = ORIENTED_EDGE ( 'NONE', *, *, #78375, .F. ) ;
#15482 = PLANE ( 'NONE',  #63996 ) ;
#15483 = CARTESIAN_POINT ( 'NONE',  ( 17.67183060077635304, -12.74070752338415247, 4.000000000000000000 ) ) ;
#15484 = DIRECTION ( 'NONE',  ( -0.7071067811865487940, 0.7071067811865463515, 0.000000000000000000 ) ) ;
#15485 = EDGE_CURVE ( 'NONE', #93941, #13015, #38728, .T. ) ;
#15486 = DIRECTION ( 'NONE',  ( -0.7071067811865486830, 0.7071067811865464625, 0.000000000000000000 ) ) ;
#15487 = EDGE_CURVE ( 'NONE', #130884, #16482, #129342, .T. ) ;
#15488 = DIRECTION ( 'NONE',  ( 1.000000000000000000, 0.000000000000000000, 0.000000000000000000 ) ) ;
#15489 = EDGE_LOOP ( 'NONE', ( #113541, #89443, #79077, #66892 ) ) ;
#15490 = DIRECTION ( 'NONE',  ( 0.6830127018922181881, 0.6830127018922202975, -0.2588190451025214056 ) ) ;
#15491 = UNCERTAINTY_MEASURE_WITH_UNIT (LENGTH_MEASURE( 1.000000000000000082E-05 ), #83953, 'distance_accuracy_value', 'NONE');
#15492 = VECTOR ( 'NONE', #54535, 1000.000000000000227 ) ;
#15493 = DIRECTION ( 'NONE',  ( 0.7071067811865487940, -0.7071067811865463515, 0.000000000000000000 ) ) ;
#15494 = EDGE_CURVE ( 'NONE', #88116, #90172, #11104, .T. ) ;
#15495 = CARTESIAN_POINT ( 'NONE',  ( -34.45011844616455221, 12.00230414159383407, 5.000000000000000888 ) ) ;
#15496 = CARTESIAN_POINT ( 'NONE',  ( 65.99586038379622721, -3.974999999999998312, -6.884901960086286188 ) ) ;
#15497 = VECTOR ( 'NONE', #117024, 1000.000000000000114 ) ;
#15498 = LINE ( 'NONE', #138761, #87836 ) ;
#15499 = VERTEX_POINT ( 'NONE', #80706 ) ;
#15500 = ORIENTED_EDGE ( 'NONE', *, *, #8726, .T. ) ;
#15501 = CARTESIAN_POINT ( 'NONE',  ( 59.91666666666665719, -6.884901960086287076, -3.975000000000000977 ) ) ;
#15502 = CARTESIAN_POINT ( 'NONE',  ( -0.5166543864104510275, 22.22500000000000142, 4.500000000000000888 ) ) ;
#15503 = DIRECTION ( 'NONE',  ( 0.7071067811865487940, 0.7071067811865463515, 0.000000000000000000 ) ) ;
#15504 = FACE_OUTER_BOUND ( 'NONE', #72211, .T. ) ;
#15505 = AXIS2_PLACEMENT_3D ( 'NONE', #94007, #59296, #15698 ) ;
#15506 = ORIENTED_EDGE ( 'NONE', *, *, #81886, .F. ) ;
#15507 = CARTESIAN_POINT ( 'NONE',  ( 0.000000000000000000, 0.000000000000000000, 5.000000000000000000 ) ) ;
#15508 = LINE ( 'NONE', #82263, #97596 ) ;
#15509 = CARTESIAN_POINT ( 'NONE',  ( 56.29209685856477563, -5.291415217122921177, 3.054999999999999272 ) ) ;
#15510 = EDGE_CURVE ( 'NONE', #127280, #61991, #35791, .T. ) ;
#15511 = AXIS2_PLACEMENT_3D ( 'NONE', #79054, #10864, #55131 ) ;
#15512 = DIRECTION ( 'NONE',  ( -0.7071067811865486830, 0.7071067811865464625, 0.000000000000000000 ) ) ;
#15513 = VERTEX_POINT ( 'NONE', #66964 ) ;
#15514 = ORIENTED_EDGE ( 'NONE', *, *, #89035, .T. ) ;
#15515 = SURFACE_STYLE_FILL_AREA ( #137353 ) ;
#15516 = DIRECTION ( 'NONE',  ( 0.5735764363510453823, -0.8191520442889923537, 1.003171929053525486E-16 ) ) ;
#15517 = CARTESIAN_POINT ( 'NONE',  ( 4.499999999999962697, -4.912538124160703568, 4.000000000000000000 ) ) ;
#15518 = AXIS2_PLACEMENT_3D ( 'NONE', #8432, #66453, #75198 ) ;
#15519 = CARTESIAN_POINT ( 'NONE',  ( 0.000000000000000000, -43.14999999999999147, -34.92499999999998295 ) ) ;
#15520 = DIRECTION ( 'NONE',  ( -0.6830127018922180770, -0.6830127018922204085, -0.2588190451025213501 ) ) ;
#15522 = VERTEX_POINT ( 'NONE', #135784 ) ;
#15521 = CARTESIAN_POINT ( 'NONE',  ( -10.49999999999992895, 12.43112307739206024, 4.000000000000000000 ) ) ;
#15523 = CARTESIAN_POINT ( 'NONE',  ( -24.18398860626899705, 28.73617430169804265, 5.000000000000000000 ) ) ;
#15524 = DIRECTION ( 'NONE',  ( 0.000000000000000000, -1.000000000000000000, 0.000000000000000000 ) ) ;
#15525 = CARTESIAN_POINT ( 'NONE',  ( 51.18398860626899705, 28.73617430169823095, 5.000000000000000000 ) ) ;
#15526 = DIRECTION ( 'NONE',  ( 0.000000000000000000, 0.000000000000000000, 1.000000000000000000 ) ) ;
#15527 = ORIENTED_EDGE ( 'NONE', *, *, #75952, .T. ) ;
#15528 = ORIENTED_EDGE ( 'NONE', *, *, #113028, .F. ) ;
#15529 = VECTOR ( 'NONE', #37175, 1000.000000000000000 ) ;
#15530 = LINE ( 'NONE', #38758, #98473 ) ;
#15531 = LINE ( 'NONE', #49669, #85828 ) ;
#15532 = EDGE_CURVE ( 'NONE', #37315, #4279, #57531, .T. ) ;
#15533 = CARTESIAN_POINT ( 'NONE',  ( 110.0375270504628986, -9.735942053221456900E-16, 7.949999999999998401 ) ) ;
#15534 = CARTESIAN_POINT ( 'NONE',  ( -34.92500000000001137, 14.81665438641027777, 4.500000000000000888 ) ) ;
#15535 = VERTEX_POINT ( 'NONE', #66255 ) ;
#15536 = ORIENTED_EDGE ( 'NONE', *, *, #38363, .F. ) ;
#15537 = DIRECTION ( 'NONE',  ( 0.6830127018922180770, -0.6830127018922204085, -0.2588190451025213501 ) ) ;
#15538 = LINE ( 'NONE', #81587, #72337 ) ;
#15539 = ORIENTED_EDGE ( 'NONE', *, *, #14870, .F. ) ;
#15540 = EDGE_CURVE ( 'NONE', #68539, #59824, #80013, .T. ) ;
#15541 = LINE ( 'NONE', #59823, #118455 ) ;
#15542 = ORIENTED_EDGE ( 'NONE', *, *, #42849, .F. ) ;
#15543 = CARTESIAN_POINT ( 'NONE',  ( 62.05836038379622011, -7.949999999999996625, -2.130196079827426203 ) ) ;
#15544 = DIRECTION ( 'NONE',  ( 0.6830127018922180770, -0.6830127018922204085, -0.2588190451025213501 ) ) ;
#15545 = AXIS2_PLACEMENT_3D ( 'NONE', #56822, #100984, #79997 ) ;
#15546 = EDGE_CURVE ( 'NONE', #6620, #86768, #67711, .T. ) ;
#15547 = FACE_BOUND ( 'NONE', #84302, .T. ) ;
#15548 = DIRECTION ( 'NONE',  ( -1.000000000000000000, -0.000000000000000000, -0.000000000000000000 ) ) ;
#15549 = DIRECTION ( 'NONE',  ( 0.6830127018922181881, 0.6830127018922202975, -0.2588190451025214056 ) ) ;
#15550 = LINE ( 'NONE', #29843, #22788 ) ;
#15551 = FACE_OUTER_BOUND ( 'NONE', #131961, .T. ) ;
#15552 = VECTOR ( 'NONE', #51810, 1000.000000000000114 ) ;
#15553 = AXIS2_PLACEMENT_3D ( 'NONE', #13260, #22007, #35792 ) ;
#15554 = PRODUCT_CONTEXT ( 'NONE', #45749, 'mechanical' ) ;
#15555 = EDGE_LOOP ( 'NONE', ( #81322, #95138, #94211, #5333 ) ) ;
#15556 = VECTOR ( 'NONE', #114509, 1000.000000000000000 ) ;
#15557 = EDGE_LOOP ( 'NONE', ( #47965, #62750, #92957, #84494, #60242 ) ) ;
#15558 = CARTESIAN_POINT ( 'NONE',  ( 94.70376352523145158, 6.109999999999998543, 1.122388791418548911E-15 ) ) ;
#15559 = EDGE_LOOP ( 'NONE', ( #40652, #73120, #46849, #6586 ) ) ;
#15560 = CARTESIAN_POINT ( 'NONE',  ( 3.872664058232598183, 3.821174125832445049E-16, 0.000000000000000000 ) ) ;
#15561 = VECTOR ( 'NONE', #126631, 1000.000000000000227 ) ;
#15562 = CARTESIAN_POINT ( 'NONE',  ( -1.499999999999990452, 21.05218569542895679, 5.000000000000000000 ) ) ;
#15563 = LINE ( 'NONE', #106153, #124246 ) ;
#15564 = DIRECTION ( 'NONE',  ( -0.7071067811865486830, -0.7071067811865464625, -0.000000000000000000 ) ) ;
#15565 = VERTEX_POINT ( 'NONE', #124188 ) ;
#15566 = LINE ( 'NONE', #50398, #22891 ) ;
#15567 = ADVANCED_FACE ( 'NONE', ( #90872 ), #112603, .F. ) ;
#15568 = CARTESIAN_POINT ( 'NONE',  ( 14.70025512860841133, -27.71228299555195917, 4.000000000000000000 ) ) ;
#15569 = LINE ( 'NONE', #104017, #133762 ) ;
#15571 = CARTESIAN_POINT ( 'NONE',  ( 26.99451991528749417, 28.92564299267956685, 4.000000000000000000 ) ) ;
#15570 = DIRECTION ( 'NONE',  ( 0.000000000000000000, -1.000000000000000000, 0.000000000000000000 ) ) ;
#15572 = CARTESIAN_POINT ( 'NONE',  ( 34.49999999999976552, 22.08746187583902554, 4.000000000000000000 ) ) ;
#15573 = CARTESIAN_POINT ( 'NONE',  ( -10.49999999999992006, -10.91253812416064584, 4.000000000000000000 ) ) ;
#15574 = EDGE_LOOP ( 'NONE', ( #124025, #15587, #4572, #25270 ) ) ;
#15575 = FACE_OUTER_BOUND ( 'NONE', #15285, .T. ) ;
#15576 = LINE ( 'NONE', #38112, #69728 ) ;
#15577 = ORIENTED_EDGE ( 'NONE', *, *, #86580, .F. ) ;
#15578 = ADVANCED_FACE ( 'NONE', ( #11834 ), #56839, .T. ) ;
#15579 = ORIENTED_EDGE ( 'NONE', *, *, #84953, .F. ) ;
#15580 = ADVANCED_FACE ( 'NONE', ( #77837 ), #111897, .F. ) ;
#15581 = VERTEX_POINT ( 'NONE', #45240 ) ;
#15582 = CARTESIAN_POINT ( 'NONE',  ( 44.62543019189810423, 5.291415217122919401, 3.055000000000002824 ) ) ;
#15583 = EDGE_LOOP ( 'NONE', ( #46035, #47606, #61467, #25881, #101766 ) ) ;
#15584 = VECTOR ( 'NONE', #35509, 1000.000000000000000 ) ;
#15585 = CARTESIAN_POINT ( 'NONE',  ( 13.60830628287044064, 1.633150327867687324, -6.094999999999991758 ) ) ;
#15586 = CARTESIAN_POINT ( 'NONE',  ( -12.52134243846371398, 7.306103351283218750, -30.66480774954007416 ) ) ;
#15587 = ORIENTED_EDGE ( 'NONE', *, *, #44846, .T. ) ;
#15588 = DIRECTION ( 'NONE',  ( -0.6830127018922180770, -0.6830127018922204085, -0.2588190451025213501 ) ) ;
#15589 = VERTEX_POINT ( 'NONE', #122023 ) ;
#15590 = DIRECTION ( 'NONE',  ( -0.5735764363510503783, -0.8191520442889886899, 0.000000000000000000 ) ) ;
#15591 = AXIS2_PLACEMENT_3D ( 'NONE', #22847, #67114, #36605 ) ;
#15592 = LINE ( 'NONE', #37400, #26682 ) ;
#15594 = VERTEX_POINT ( 'NONE', #958 ) ;
#15593 = DIRECTION ( 'NONE',  ( 0.7071067811865487940, 0.7071067811865463515, 0.000000000000000000 ) ) ;
#15595 = EDGE_LOOP ( 'NONE', ( #62373, #114538, #108145, #87338 ) ) ;
#15596 = EDGE_CURVE ( 'NONE', #57246, #141239, #22692, .T. ) ;
#15597 = CARTESIAN_POINT ( 'NONE',  ( -51.18398860626899705, 28.73617430169823095, 5.000000000000000000 ) ) ;
#15598 = DIRECTION ( 'NONE',  ( -0.7071067811865487940, 0.7071067811865463515, -0.000000000000000000 ) ) ;
#15599 = ORIENTED_EDGE ( 'NONE', *, *, #16096, .T. ) ;
#15600 = CARTESIAN_POINT ( 'NONE',  ( -7.940000000000001279, -60.26999999999998892, -10.00000000000000178 ) ) ;
#15601 = ORIENTED_EDGE ( 'NONE', *, *, #43557, .T. ) ;
#15602 = PRODUCT_DEFINITION_SHAPE ( 'NONE', 'NONE',  #37749 ) ;
#15603 = EDGE_LOOP ( 'NONE', ( #39635, #119117, #27905, #49087 ) ) ;
#15604 = ORIENTED_EDGE ( 'NONE', *, *, #128014, .F. ) ;
#15605 = VERTEX_POINT ( 'NONE', #99556 ) ;
#15606 = DIRECTION ( 'NONE',  ( -1.000000000000000000, -1.224606353822377258E-16, -0.000000000000000000 ) ) ;
#15607 = CARTESIAN_POINT ( 'NONE',  ( 20.70025512860841133, -27.71228299555191654, 4.000000000000000000 ) ) ;
#15608 = LINE ( 'NONE', #78789, #56435 ) ;
#15609 = CARTESIAN_POINT ( 'NONE',  ( -14.70822291016943240, -15.74070752338411694, 19.73771281079093853 ) ) ;
#15610 = LINE ( 'NONE', #58514, #55823 ) ;
#15611 = ORIENTED_EDGE ( 'NONE', *, *, #110546, .T. ) ;
#15612 = PLANE ( 'NONE',  #77228 ) ;
#15613 = CARTESIAN_POINT ( 'NONE',  ( 24.77040314143521726, -7.934999999999989839, 2.126176841940957907 ) ) ;
#15614 = CARTESIAN_POINT ( 'NONE',  ( 34.82816939922329169, 18.75929247661552424, 4.000000000000000000 ) ) ;
#15615 = ADVANCED_FACE ( 'NONE', ( #111141 ), #55381, .F. ) ;
#15616 = DIRECTION ( 'NONE',  ( -0.000000000000000000, 0.3543493200069153248, 0.9351131265310292928 ) ) ;
#15617 = VECTOR ( 'NONE', #18804, 999.9999999999998863 ) ;
#15618 = LINE ( 'NONE', #70794, #136951 ) ;
#15619 = ORIENTED_EDGE ( 'NONE', *, *, #58860, .F. ) ;
#15620 = EDGE_CURVE ( 'NONE', #25494, #82607, #137055, .T. ) ;
#15621 = EDGE_LOOP ( 'NONE', ( #24071, #124112, #130015, #100593 ) ) ;
#15622 = ORIENTED_EDGE ( 'NONE', *, *, #21670, .T. ) ;
#15623 = FACE_OUTER_BOUND ( 'NONE', #49963, .T. ) ;
#15624 = FACE_OUTER_BOUND ( 'NONE', #1502, .T. ) ;
#15625 = UNCERTAINTY_MEASURE_WITH_UNIT (LENGTH_MEASURE( 1.000000000000000082E-05 ), #51391, 'distance_accuracy_value', 'NONE');
#15626 = CARTESIAN_POINT ( 'NONE',  ( 18.48921356237309510, -27.52281430457068367, 5.000000000000000000 ) ) ;
#15627 = LINE ( 'NONE', #49042, #28846 ) ;
#15628 = FACE_OUTER_BOUND ( 'NONE', #30931, .T. ) ;
#15629 = EDGE_CURVE ( 'NONE', #28732, #18685, #123512, .T. ) ;
#15631 = ADVANCED_FACE ( 'NONE', ( #3111 ), #134369, .F. ) ;
#15630 = CARTESIAN_POINT ( 'NONE',  ( 77.34959685856478018, 6.109999999999997655, 1.637169565754163836 ) ) ;
#15632 = CARTESIAN_POINT ( 'NONE',  ( 74.74586038379622721, 3.974999999999996980, 6.884901960086287964 ) ) ;
#15634 = VECTOR ( 'NONE', #133068, 999.9999999999998863 ) ;
#15633 = CARTESIAN_POINT ( 'NONE',  ( 4.495848767239241539, 2.500000000000000444, 0.000000000000000000 ) ) ;
#15635 = DIRECTION ( 'NONE',  ( -0.6830127018922180770, -0.6830127018922204085, -0.2588190451025213501 ) ) ;
#15636 = CARTESIAN_POINT ( 'NONE',  ( -2.999999999999969802, -1.447814304570815169, 5.000000000000000000 ) ) ;
#15637 = DIRECTION ( 'NONE',  ( -0.7071067811865487940, 0.7071067811865463515, -0.000000000000000000 ) ) ;
#15638 = EDGE_LOOP ( 'NONE', ( #51746, #58305, #47434, #67401 ) ) ;
#15639 = CARTESIAN_POINT ( 'NONE',  ( 17.01022479757872219, -0.9324317514308457788, -36.05569165383651153 ) ) ;
#15640 = ORIENTED_EDGE ( 'NONE', *, *, #130594, .T. ) ;
#15641 = AXIS2_PLACEMENT_3D ( 'NONE', #70084, #114248, #60628 ) ;
#15642 = CARTESIAN_POINT ( 'NONE',  ( 11.99999999999992362, 4.552185695429119328, 5.000000000000000000 ) ) ;
#15644 = ORIENTED_EDGE ( 'NONE', *, *, #55401, .F. ) ;
#15643 = FACE_OUTER_BOUND ( 'NONE', #65132, .T. ) ;
#15645 = EDGE_CURVE ( 'NONE', #59338, #18319, #79265, .T. ) ;
#15646 = EDGE_CURVE ( 'NONE', #38043, #19525, #127762, .T. ) ;
#15647 = PLANE ( 'NONE',  #104206 ) ;
#15648 = DIRECTION ( 'NONE',  ( -0.3543493200069162685, -0.000000000000000000, -0.9351131265310288487 ) ) ;
#15649 = EDGE_LOOP ( 'NONE', ( #50438, #43600, #87061, #78003 ) ) ;
#15650 = PLANE ( 'NONE',  #110983 ) ;
#15651 = EDGE_LOOP ( 'NONE', ( #143069, #49667, #33818, #96759 ) ) ;
#15652 = CARTESIAN_POINT ( 'NONE',  ( 121.7041937171295700, -6.884901960086285300, -3.975000000000000089 ) ) ;
#15653 = EDGE_LOOP ( 'NONE', ( #105804, #45277, #59698, #88455 ) ) ;
#15654 = VECTOR ( 'NONE', #5773, 1000.000000000000000 ) ;
#15655 = VECTOR ( 'NONE', #45779, 1000.000000000000000 ) ;
#15656 = CARTESIAN_POINT ( 'NONE',  ( 18.48921356237309510, -27.52281430457068367, 5.000000000000000000 ) ) ;
#15657 = EDGE_CURVE ( 'NONE', #10245, #104418, #74573, .T. ) ;
#15658 = CARTESIAN_POINT ( 'NONE',  ( 103.0375270504628986, -9.735942053221456900E-16, 7.949999999999998401 ) ) ;
#15659 = PLANE ( 'NONE',  #13910 ) ;
#15660 = LINE ( 'NONE', #38196, #94651 ) ;
#15661 = ORIENTED_EDGE ( 'NONE', *, *, #119085, .T. ) ;
#15662 = CARTESIAN_POINT ( 'NONE',  ( 39.18398860626899705, 28.73617430169814568, 5.000000000000000000 ) ) ;
#15663 = DIRECTION ( 'NONE',  ( -0.7071067811865486830, 0.7071067811865464625, 0.000000000000000000 ) ) ;
#15664 = LINE ( 'NONE', #59953, #6677 ) ;
#15665 = CARTESIAN_POINT ( 'NONE',  ( 27.12500000000000355, 6.094999999999989981, -1.119633336120465690E-15 ) ) ;
#15666 = CARTESIAN_POINT ( 'NONE',  ( -15.44591897758377108, -1.592173378680612927, 4.204195949441833946 ) ) ;
#15667 = ADVANCED_FACE ( 'NONE', ( #4477 ), #40071, .F. ) ;
#15668 = CARTESIAN_POINT ( 'NONE',  ( -39.48921356237310221, -27.52281430457082934, 5.000000000000000000 ) ) ;
#15669 = ORIENTED_EDGE ( 'NONE', *, *, #9985, .T. ) ;
#15670 = LINE ( 'NONE', #59957, #28207 ) ;
#15671 = ORIENTED_EDGE ( 'NONE', *, *, #123003, .F. ) ;
#15672 = CARTESIAN_POINT ( 'NONE',  ( 81.37543019189810423, -5.291415217122920289, -3.055000000000001492 ) ) ;
#15673 = FACE_OUTER_BOUND ( 'NONE', #67810, .T. ) ;
#15674 = ADVANCED_FACE ( 'NONE', ( #27009 ), #25574, .F. ) ;
#15675 = DIRECTION ( 'NONE',  ( -0.3543493200069162685, -0.000000000000000000, -0.9351131265310288487 ) ) ;
#15676 = LINE ( 'NONE', #104126, #66435 ) ;
#15677 = ORIENTED_EDGE ( 'NONE', *, *, #124962, .F. ) ;
#15678 = CARTESIAN_POINT ( 'NONE',  ( -2.994519915287485734, 28.92564299267940342, 4.000000000000000000 ) ) ;
#15679 =( BOUNDED_CURVE ( )  B_SPLINE_CURVE ( 2, ( #38668, #139443, #61185, #93042, #17598, #137272, #50973, #37970, #60448, #59726, #18298, #105335, #103886 ),
 .UNSPECIFIED., .F., .T. ) 
 B_SPLINE_CURVE_WITH_KNOTS ( ( 3, 2, 2, 2, 2, 2, 3 ),
 ( 0.1666666666666666574, 0.1694444444444444531, 0.1722222222222222210, 0.1749999999999999889, 0.1777777777777778123, 0.1805555555555555802, 0.1833333333333333481 ),
 .UNSPECIFIED. ) 
 CURVE ( )  GEOMETRIC_REPRESENTATION_ITEM ( )  RATIONAL_B_SPLINE_CURVE ( ( 1.000000000000000000, 0.9659258262890683122, 1.000000000000000000, 0.9659258262890683122, 1.000000000000000000, 0.9659258262890683122, 1.000000000000000000, 0.9659258262890683122, 1.000000000000000000, 0.9659258262890683122, 1.000000000000000000, 0.9659258262890679791, 1.000000000000000444 ) ) 
 REPRESENTATION_ITEM ( '' )  );
#15680 = DIRECTION ( 'NONE',  ( -0.6830127018922180770, -0.6830127018922204085, -0.2588190451025213501 ) ) ;
#15681 = CARTESIAN_POINT ( 'NONE',  ( 25.49999999999982236, 13.08746187583911436, 4.000000000000000000 ) ) ;
#15682 = CARTESIAN_POINT ( 'NONE',  ( -14.67183060077636370, -21.74070752338405299, 4.000000000000000000 ) ) ;
#15685 = EDGE_CURVE ( 'NONE', #12429, #39954, #37176, .T. ) ;
#15684 = ORIENTED_EDGE ( 'NONE', *, *, #25938, .T. ) ;
#15683 = CARTESIAN_POINT ( 'NONE',  ( 5.292986735706907808, -21.74070752338406365, 4.999753212805221558 ) ) ;
#15687 = AXIS2_PLACEMENT_3D ( 'NONE', #97060, #129729, #40606 ) ;
#15686 = CARTESIAN_POINT ( 'NONE',  ( -29.27718569542920335, -21.72500000000000142, 5.000000000000000000 ) ) ;
#15688 = FACE_OUTER_BOUND ( 'NONE', #44218, .T. ) ;
#15689 = CARTESIAN_POINT ( 'NONE',  ( 9.183988606268997046, 28.73617430169793607, 5.000000000000000000 ) ) ;
#15690 = DIRECTION ( 'NONE',  ( -1.000000000000000000, -0.000000000000000000, -0.000000000000000000 ) ) ;
#15691 = VERTEX_POINT ( 'NONE', #70569 ) ;
#15692 = ADVANCED_FACE ( 'NONE', ( #103145 ), #116256, .T. ) ;
#15693 = ORIENTED_EDGE ( 'NONE', *, *, #1862, .F. ) ;
#15694 = ORIENTED_EDGE ( 'NONE', *, *, #5491, .T. ) ;
#15695 = CARTESIAN_POINT ( 'NONE',  ( 80.64626352523141861, -4.472830434245840259, 4.472830434245839371 ) ) ;
#15696 = VERTEX_POINT ( 'NONE', #26311 ) ;
#15697 = DIRECTION ( 'NONE',  ( -0.6830127018922181881, 0.6830127018922202975, -0.2588190451025214056 ) ) ;
#15698 = DIRECTION ( 'NONE',  ( 0.7071067811865487940, 0.7071067811865463515, 0.000000000000000000 ) ) ;
#15699 = DIRECTION ( 'NONE',  ( 0.000000000000000000, -1.000000000000000000, 0.000000000000000000 ) ) ;
#15700 = DIRECTION ( 'NONE',  ( -0.7071067811865486830, 0.7071067811865464625, 0.000000000000000000 ) ) ;
#15701 = ORIENTED_EDGE ( 'NONE', *, *, #65583, .F. ) ;
#15702 = CARTESIAN_POINT ( 'NONE',  ( 34.92499999999998295, 10.33457404400606450, 0.4942731178106110068 ) ) ;
#15703 = CARTESIAN_POINT ( 'NONE',  ( -33.79289321881321939, 15.75929247661555976, 5.000000000000000000 ) ) ;
#15704 = CARTESIAN_POINT ( 'NONE',  ( 75.16209685856478018, -5.291415217122919401, 3.054999999999997939 ) ) ;
#15705 = VERTEX_POINT ( 'NONE', #6637 ) ;
#15706 = DIRECTION ( 'NONE',  ( 0.7071067811865486830, -0.7071067811865464625, -0.000000000000000000 ) ) ;
#15707 = DIRECTION ( 'NONE',  ( 0.7071067811865487940, 0.7071067811865463515, 0.000000000000000000 ) ) ;
#15708 = LINE ( 'NONE', #123835, #93249 ) ;
#15709 = EDGE_LOOP ( 'NONE', ( #41225, #73345, #24701, #63052 ) ) ;
#15710 = ORIENTED_EDGE ( 'NONE', *, *, #128128, .T. ) ;
#15711 = CARTESIAN_POINT ( 'NONE',  ( 64.87499999999998579, 7.950000000000000178, 1.460391307983218535E-15 ) ) ;
#15712 = CARTESIAN_POINT ( 'NONE',  ( -34.92500000000001137, 22.22500000000000142, 4.000000000000000000 ) ) ;
#15713 = PLANE ( 'NONE',  #122559 ) ;
#15714 = LINE ( 'NONE', #50540, #41973 ) ;
#15715 = DIRECTION ( 'NONE',  ( -0.6830127018922181881, 0.6830127018922202975, -0.2588190451025214056 ) ) ;
#15716 = DIRECTION ( 'NONE',  ( 0.7071067811865487940, 0.7071067811865463515, 0.000000000000000000 ) ) ;
#15717 = DIRECTION ( 'NONE',  ( -0.7071067811865486830, -0.7071067811865464625, -0.000000000000000000 ) ) ;
#15718 =( LENGTH_UNIT ( ) NAMED_UNIT ( * ) SI_UNIT ( .MILLI., .METRE. ) );
#15719 = ORIENTED_EDGE ( 'NONE', *, *, #131425, .F. ) ;
#15720 = VECTOR ( 'NONE', #13109, 1000.000000000000000 ) ;
#15721 = ORIENTED_EDGE ( 'NONE', *, *, #24865, .T. ) ;
#15722 = VERTEX_POINT ( 'NONE', #71255 ) ;
#15723 = EDGE_CURVE ( 'NONE', #111351, #19902, #138647, .T. ) ;
#15724 = CARTESIAN_POINT ( 'NONE',  ( 11.99999999999991829, -18.41253812416056945, 4.000000000000000000 ) ) ;
#15725 =( NAMED_UNIT ( * ) PLANE_ANGLE_UNIT ( ) SI_UNIT ( $, .RADIAN. ) );
#15726 = ORIENTED_EDGE ( 'NONE', *, *, #74130, .T. ) ;
#15727 = CARTESIAN_POINT ( 'NONE',  ( 2.999999999999999112, 0.000000000000000000, 0.000000000000000000 ) ) ;
#15728 = CARTESIAN_POINT ( 'NONE',  ( -8.700255128608413102, -27.71228299555199825, 4.000000000000000000 ) ) ;
#15729 = DIRECTION ( 'NONE',  ( -0.3543493200069162685, -0.000000000000000000, -0.9351131265310288487 ) ) ;
#15730 = AXIS2_PLACEMENT_3D ( 'NONE', #84840, #29719, #95707 ) ;
#15731 = DIRECTION ( 'NONE',  ( 0.7071067811865487940, 0.7071067811865463515, 0.000000000000000000 ) ) ;
#15732 = ORIENTED_EDGE ( 'NONE', *, *, #78242, .T. ) ;
#15733 = CARTESIAN_POINT ( 'NONE',  ( 34.92499999999998295, 22.22500000000000142, 4.000000000000000000 ) ) ;
#15734 = VECTOR ( 'NONE', #48073, 1000.000000000000000 ) ;
#15735 = ORIENTED_EDGE ( 'NONE', *, *, #1926, .T. ) ;
#15736 = EDGE_CURVE ( 'NONE', #40291, #123040, #50210, .T. ) ;
#15737 = DIRECTION ( 'NONE',  ( -0.000000000000000000, 0.3543493200069153248, 0.9351131265310292928 ) ) ;
#15738 = EDGE_LOOP ( 'NONE', ( #81946, #120299, #87573, #60609 ) ) ;
#15739 = ORIENTED_EDGE ( 'NONE', *, *, #64994, .F. ) ;
#15741 = EDGE_CURVE ( 'NONE', #3283, #126278, #93706, .T. ) ;
#15740 = CARTESIAN_POINT ( 'NONE',  ( -48.29974487139158867, -27.71228299555239971, 4.000000000000000000 ) ) ;
#15742 = ORIENTED_EDGE ( 'NONE', *, *, #74351, .T. ) ;
#15743 = VERTEX_POINT ( 'NONE', #16861 ) ;
#15744 = CARTESIAN_POINT ( 'NONE',  ( 74.52126352523143282, -4.472830434245838482, -4.472830434245840259 ) ) ;
#15745 = VECTOR ( 'NONE', #69136, 1000.000000000000000 ) ;
#15746 = ORIENTED_EDGE ( 'NONE', *, *, #125818, .F. ) ;
#15747 = VECTOR ( 'NONE', #17390, 1000.000000000000000 ) ;
#15748 = FILL_AREA_STYLE ('',( #70925 ) ) ;
#15749 = DIRECTION ( 'NONE',  ( -1.000000000000000000, -0.000000000000000000, -0.000000000000000000 ) ) ;
#15750 = CARTESIAN_POINT ( 'NONE',  ( 110.2504301918981042, 3.055000000000002824, -5.291415217122919401 ) ) ;
#15751 = CARTESIAN_POINT ( 'NONE',  ( 127.0000000000000000, 1.864289179696898779, 6.174700466780991270 ) ) ;
#15752 = EDGE_CURVE ( 'NONE', #12370, #141174, #59671, .T. ) ;
#15753 = CARTESIAN_POINT ( 'NONE',  ( 19.49999999999987210, -12.08601207473287253, -10.46905243149098474 ) ) ;
#15754 = LINE ( 'NONE', #36155, #44444 ) ;
#15755 = DIRECTION ( 'NONE',  ( -0.7071067811865486830, -0.7071067811865464625, -0.000000000000000000 ) ) ;
#15756 = DIRECTION ( 'NONE',  ( 0.3543493200069162685, -0.000000000000000000, -0.9351131265310288487 ) ) ;
#15757 =( GEOMETRIC_REPRESENTATION_CONTEXT ( 3 ) GLOBAL_UNCERTAINTY_ASSIGNED_CONTEXT ( ( #88459 ) ) GLOBAL_UNIT_ASSIGNED_CONTEXT ( ( #123409, #113194, #58170 ) ) REPRESENTATION_CONTEXT ( 'NONE', 'WORKASPACE' ) );
#15758 = DIRECTION ( 'NONE',  ( 1.000000000000000000, 0.000000000000000000, 0.000000000000000000 ) ) ;
#15759 = EDGE_CURVE ( 'NONE', #38066, #132490, #82146, .T. ) ;
#15760 = FILL_AREA_STYLE_COLOUR ( '', #46776 ) ;
#15761 = CARTESIAN_POINT ( 'NONE',  ( 24.66594027184343219, -22.22500000000000142, -17.58123489532666639 ) ) ;
#15762 = VERTEX_POINT ( 'NONE', #39342 ) ;
#15763 = CARTESIAN_POINT ( 'NONE',  ( 0.000000000000000000, 0.000000000000000000, 5.000000000000000000 ) ) ;
#15764 = LINE ( 'NONE', #104225, #86925 ) ;
#15765 = ORIENTED_EDGE ( 'NONE', *, *, #81814, .T. ) ;
#15766 = ORIENTED_EDGE ( 'NONE', *, *, #97030, .T. ) ;
#15767 = AXIS2_PLACEMENT_3D ( 'NONE', #58739, #15830, #115156 ) ;
#15768 = CARTESIAN_POINT ( 'NONE',  ( -28.49999999999980815, 14.14708470758588632, -0.5283514160165899698 ) ) ;
#15769 = ADVANCED_FACE ( 'NONE', ( #83561 ), #127774, .T. ) ;
#15770 = VERTEX_POINT ( 'NONE', #18238 ) ;
#15771 = VECTOR ( 'NONE', #60468, 1000.000000000000000 ) ;
#15772 = CARTESIAN_POINT ( 'NONE',  ( 0.7307956238753654521, 3.821174125832445049E-16, 0.000000000000000000 ) ) ;
#15773 = CARTESIAN_POINT ( 'NONE',  ( -11.48334561358947070, 22.22500000000000142, 4.500000000000000888 ) ) ;
#15774 = AXIS2_PLACEMENT_3D ( 'NONE', #55776, #77536, #110811 ) ;
#15775 = FACE_OUTER_BOUND ( 'NONE', #32601, .T. ) ;
#15776 = CARTESIAN_POINT ( 'NONE',  ( -14.99999999999990230, 7.559798855135676732, 4.979909187984716823 ) ) ;
#15777 = ORIENTED_EDGE ( 'NONE', *, *, #70554, .T. ) ;
#15778 = ORIENTED_EDGE ( 'NONE', *, *, #38962, .F. ) ;
#15779 = CARTESIAN_POINT ( 'NONE',  ( -30.00000000000000355, 2.375000000000000000, 0.000000000000000000 ) ) ;
#15780 = CARTESIAN_POINT ( 'NONE',  ( 27.92123647476855197, -9.717572351234235426E-16, -7.934999999999990727 ) ) ;
#15781 = DIRECTION ( 'NONE',  ( -0.6830127018922181881, 0.6830127018922202975, -0.2588190451025214056 ) ) ;
#15782 = DIRECTION ( 'NONE',  ( 0.000000000000000000, 0.000000000000000000, -1.000000000000000000 ) ) ;
#15783 = CARTESIAN_POINT ( 'NONE',  ( 13.21415715735881058, -8.911859315205598264, -3.297485585150703002 ) ) ;
#15784 = VERTEX_POINT ( 'NONE', #29853 ) ;
#15785 = EDGE_CURVE ( 'NONE', #29858, #46809, #120156, .T. ) ;
#15786 = ORIENTED_EDGE ( 'NONE', *, *, #19290, .F. ) ;
#15787 = ORIENTED_EDGE ( 'NONE', *, *, #136655, .T. ) ;
#15788 = CARTESIAN_POINT ( 'NONE',  ( 1.180000000000000604, -6.391994993740214959, 10.00000000000000000 ) ) ;
#15789 = LINE ( 'NONE', #37614, #46470 ) ;
#15791 = VECTOR ( 'NONE', #23840, 1000.000000000000000 ) ;
#15790 = PLANE ( 'NONE',  #105237 ) ;
#15792 = FACE_OUTER_BOUND ( 'NONE', #109042, .T. ) ;
#15793 = CARTESIAN_POINT ( 'NONE',  ( -34.92500000000001137, 21.00612307739172024, 4.000000000000000000 ) ) ;
#15795 = EDGE_CURVE ( 'NONE', #73287, #137211, #141732, .T. ) ;
#15794 = VECTOR ( 'NONE', #321, 1000.000000000000000 ) ;
#15796 = EDGE_CURVE ( 'NONE', #103206, #54270, #63937, .T. ) ;
#15797 = DIRECTION ( 'NONE',  ( -0.7071067811865487940, 0.7071067811865463515, -0.000000000000000000 ) ) ;
#15798 = DIRECTION ( 'NONE',  ( 0.3543493200069162685, -0.000000000000000000, -0.9351131265310288487 ) ) ;
#15799 = DIRECTION ( 'NONE',  ( 0.6830127018922180770, -0.6830127018922204085, -0.2588190451025213501 ) ) ;
#15800 = CARTESIAN_POINT ( 'NONE',  ( -7.499999999999951150, 6.277155672890267546, -3.510561720658922802 ) ) ;
#15801 = ORIENTED_EDGE ( 'NONE', *, *, #27864, .T. ) ;
#15802 = CARTESIAN_POINT ( 'NONE',  ( -8.510786437626906675, -27.52281430457049183, 5.000000000000000000 ) ) ;
#15804 = ADVANCED_FACE ( 'NONE', ( #142226 ), #54502, .F. ) ;
#15803 = DIRECTION ( 'NONE',  ( 0.3543493200069163240, -0.000000000000000000, 0.9351131265310288487 ) ) ;
#15805 = ORIENTED_EDGE ( 'NONE', *, *, #1110, .T. ) ;
#15806 = FACE_OUTER_BOUND ( 'NONE', #127568, .T. ) ;
#15808 = EDGE_LOOP ( 'NONE', ( #114681, #70304, #38984, #25529, #1229, #14754 ) ) ;
#15807 = DIRECTION ( 'NONE',  ( -1.000000000000000000, 0.000000000000000000, 0.000000000000000000 ) ) ;
#15810 = ORIENTED_EDGE ( 'NONE', *, *, #9440, .T. ) ;
#15809 = ADVANCED_FACE ( 'NONE', ( #108107 ), #8771, .F. ) ;
#15811 = ADVANCED_FACE ( 'NONE', ( #98681 ), #53029, .F. ) ;
#15812 = LINE ( 'NONE', #49240, #125591 ) ;
#15813 = CARTESIAN_POINT ( 'NONE',  ( 97.78752705046289861, 0.000000000000000000, -7.949999999999998401 ) ) ;
#15814 = CARTESIAN_POINT ( 'NONE',  ( 17.67183060077634593, -18.74070752338409918, 4.000000000000000000 ) ) ;
#15815 = VERTEX_POINT ( 'NONE', #119013 ) ;
#15816 = DIRECTION ( 'NONE',  ( -0.000000000000000000, 0.3543493200069153248, 0.9351131265310292928 ) ) ;
#15817 = UNCERTAINTY_MEASURE_WITH_UNIT (LENGTH_MEASURE( 1.000000000000000082E-05 ), #94570, 'distance_accuracy_value', 'NONE');
#15818 = DIRECTION ( 'NONE',  ( 0.7071067811865487940, 0.7071067811865463515, 0.000000000000000000 ) ) ;
#15819 = CARTESIAN_POINT ( 'NONE',  ( 106.2916666666666714, 3.975000000000003642, -6.884901960086285300 ) ) ;
#15820 = CARTESIAN_POINT ( 'NONE',  ( 27.32876352523144803, 0.000000000000000000, -6.109999999999999432 ) ) ;
#15821 = EDGE_CURVE ( 'NONE', #103560, #142252, #116150, .T. ) ;
#15822 = CARTESIAN_POINT ( 'NONE',  ( -23.70025512860841133, -27.71228299555189523, 4.000000000000000000 ) ) ;
#15823 = EDGE_CURVE ( 'NONE', #32577, #77379, #18993, .T. ) ;
#15824 = LINE ( 'NONE', #6370, #113391 ) ;
#15825 = DIRECTION ( 'NONE',  ( 0.7071067811865487940, 0.7071067811865463515, 0.000000000000000000 ) ) ;
#15826 = PLANE ( 'NONE',  #51822 ) ;
#15827 = CARTESIAN_POINT ( 'NONE',  ( -4.499999999999970690, 18.05218569542898521, 5.000000000000000000 ) ) ;
#15828 = CARTESIAN_POINT ( 'NONE',  ( 29.72873647476855297, 5.808823158059031044, -5.808823158059038150 ) ) ;
#15829 = CARTESIAN_POINT ( 'NONE',  ( 7.270403141435218153, -7.934999999999988951, 2.126176841940957907 ) ) ;
#15830 = DIRECTION ( 'NONE',  ( -0.6830127018922181881, 0.6830127018922202975, -0.2588190451025214056 ) ) ;
#15831 = EDGE_CURVE ( 'NONE', #40891, #44308, #53670, .T. ) ;
#15832 = DIRECTION ( 'NONE',  ( 0.6830127018922180770, -0.6830127018922204085, -0.2588190451025213501 ) ) ;
#15833 = CARTESIAN_POINT ( 'NONE',  ( -31.49999999999977973, 22.01701374228153085, 2.453858888625704004 ) ) ;
#15834 = ORIENTED_EDGE ( 'NONE', *, *, #123252, .F. ) ;
#15835 = ORIENTED_EDGE ( 'NONE', *, *, #44736, .F. ) ;
#15836 = CARTESIAN_POINT ( 'NONE',  ( 94.18749999999998579, -5.819803920172573086, 5.819803920172572198 ) ) ;
#15837 = ORIENTED_EDGE ( 'NONE', *, *, #131598, .T. ) ;
#15838 = VERTEX_POINT ( 'NONE', #40760 ) ;
#15839 = FACE_OUTER_BOUND ( 'NONE', #123541, .T. ) ;
#15840 = DIRECTION ( 'NONE',  ( 0.7071067811865486830, -0.7071067811865464625, -0.000000000000000000 ) ) ;
#15841 = FACE_OUTER_BOUND ( 'NONE', #102912, .T. ) ;
#15842 = ORIENTED_EDGE ( 'NONE', *, *, #3432, .F. ) ;
#15843 = VECTOR ( 'NONE', #13620, 1000.000000000000000 ) ;
#15844 = AXIS2_PLACEMENT_3D ( 'NONE', #9947, #21555, #65816 ) ;
#15846 = LINE ( 'NONE', #6391, #34775 ) ;
#15845 = VECTOR ( 'NONE', #115396, 1000.000000000000000 ) ;
#15847 = PLANE ( 'NONE',  #125111 ) ;
#15848 = VECTOR ( 'NONE', #94404, 1000.000000000000000 ) ;
#15849 = DIRECTION ( 'NONE',  ( -0.7071067811865486830, -0.7071067811865464625, 0.000000000000000000 ) ) ;
#15850 = CARTESIAN_POINT ( 'NONE',  ( 126.7599512408517057, 4.946259330407210442, 4.511684350628299534 ) ) ;
#15851 = AXIS2_PLACEMENT_3D ( 'NONE', #99831, #131041, #42631 ) ;
#15852 = FACE_OUTER_BOUND ( 'NONE', #36394, .T. ) ;
#15853 = CARTESIAN_POINT ( 'NONE',  ( 1.499999999999994449, -13.53360074219760456, 5.000000000000000000 ) ) ;
#15854 = PLANE ( 'NONE',  #114232 ) ;
#15855 = EDGE_CURVE ( 'NONE', #138242, #128760, #129895, .T. ) ;
#15856 = DIRECTION ( 'NONE',  ( -0.6830127018922180770, -0.6830127018922204085, -0.2588190451025213501 ) ) ;
#15857 = CARTESIAN_POINT ( 'NONE',  ( 160.0000000000000000, 0.000000000000000000, 6.349999999999997868 ) ) ;
#15858 = DIRECTION ( 'NONE',  ( 0.6830127018922181881, 0.6830127018922202975, -0.2588190451025214056 ) ) ;
#15859 = VECTOR ( 'NONE', #93120, 1000.000000000000227 ) ;
#15860 = CARTESIAN_POINT ( 'NONE',  ( 14.99999999999989519, 10.21212019023810491, -2.019456568337833602 ) ) ;
#15861 = CARTESIAN_POINT ( 'NONE',  ( 52.60764783923757903, -49.05583548141700589, 39.86617647058822200 ) ) ;
#15862 = EDGE_CURVE ( 'NONE', #54899, #113725, #141491, .T. ) ;
#15863 = EDGE_CURVE ( 'NONE', #116077, #140375, #118286, .T. ) ;
#15864 = VERTEX_POINT ( 'NONE', #96515 ) ;
#15865 = ORIENTED_EDGE ( 'NONE', *, *, #1269, .T. ) ;
#15866 = CARTESIAN_POINT ( 'NONE',  ( 114.6254301918981042, 5.291415217122919401, 3.055000000000002824 ) ) ;
#15867 = VERTEX_POINT ( 'NONE', #140753 ) ;
#15868 = FILL_AREA_STYLE_COLOUR ( '', #87268 ) ;
#15869 = AXIS2_PLACEMENT_3D ( 'NONE', #140189, #128595, #83692 ) ;
#15870 = PRESENTATION_STYLE_ASSIGNMENT (( #48556 ) ) ;
#15871 = VERTEX_POINT ( 'NONE', #85660 ) ;
#15872 = EDGE_CURVE ( 'NONE', #91794, #25131, #19697, .T. ) ;
#15873 = LINE ( 'NONE', #103621, #39766 ) ;
#15874 = DIRECTION ( 'NONE',  ( -0.000000000000000000, 0.3543493200069153248, 0.9351131265310292928 ) ) ;
#15875 = VECTOR ( 'NONE', #68526, 1000.000000000000000 ) ;
#15876 = CARTESIAN_POINT ( 'NONE',  ( 100.0995968585647944, -6.109999999999997655, -1.637169565754160283 ) ) ;
#15877 = ORIENTED_EDGE ( 'NONE', *, *, #73001, .T. ) ;
#15878 = CARTESIAN_POINT ( 'NONE',  ( -12.29974487139158512, -27.71228299555214747, 4.000000000000000000 ) ) ;
#15879 = ORIENTED_EDGE ( 'NONE', *, *, #33602, .F. ) ;
#15880 = CARTESIAN_POINT ( 'NONE',  ( 3.489213562373097322, -27.52281430457057709, 5.000000000000000000 ) ) ;
#15881 = VECTOR ( 'NONE', #21769, 1000.000000000000227 ) ;
#15882 = PLANE ( 'NONE',  #17098 ) ;
#15883 = CARTESIAN_POINT ( 'NONE',  ( -24.62910658713767731, 1.050808743928695277, 4.662926800793053772 ) ) ;
#15884 = AXIS2_PLACEMENT_3D ( 'NONE', #117517, #107377, #51593 ) ;
#15885 = VECTOR ( 'NONE', #38335, 999.9999999999998863 ) ;
#15886 = VECTOR ( 'NONE', #110673, 1000.000000000000000 ) ;
#15887 = ORIENTED_EDGE ( 'NONE', *, *, #128931, .T. ) ;
#15888 = ORIENTED_EDGE ( 'NONE', *, *, #140873, .F. ) ;
#15889 = EDGE_LOOP ( 'NONE', ( #31574, #67961, #122767, #89448 ) ) ;
#15890 = DIRECTION ( 'NONE',  ( 0.7071067811865487940, 0.7071067811865463515, -0.000000000000000000 ) ) ;
#15891 = CARTESIAN_POINT ( 'NONE',  ( 8.525403141435219823, 2.126176841940962348, 7.934999999999988951 ) ) ;
#15892 = AXIS2_PLACEMENT_3D ( 'NONE', #126764, #105023, #94138 ) ;
#15893 = VECTOR ( 'NONE', #139925, 1000.000000000000000 ) ;
#15894 = DIRECTION ( 'NONE',  ( -0.7071067811865487940, 0.7071067811865463515, -0.000000000000000000 ) ) ;
#15895 = SURFACE_STYLE_USAGE ( .BOTH. , #15202 ) ;
#15896 = ORIENTED_EDGE ( 'NONE', *, *, #43829, .F. ) ;
#15897 = ORIENTED_EDGE ( 'NONE', *, *, #51537, .T. ) ;
#15898 = FACE_OUTER_BOUND ( 'NONE', #76357, .T. ) ;
#15900 = EDGE_CURVE ( 'NONE', #4623, #101006, #20394, .T. ) ;
#15899 = ORIENTED_EDGE ( 'NONE', *, *, #122102, .F. ) ;
#15901 = EDGE_CURVE ( 'NONE', #71584, #76991, #99375, .T. ) ;
#15902 = ORIENTED_EDGE ( 'NONE', *, *, #135201, .F. ) ;
#15903 = AXIS2_PLACEMENT_3D ( 'NONE', #30846, #64176, #119934 ) ;
#15904 = DIRECTION ( 'NONE',  ( 0.7071067811865487940, 0.7071067811865463515, 0.000000000000000000 ) ) ;
#15905 = CARTESIAN_POINT ( 'NONE',  ( 0.000000000000000000, 0.000000000000000000, 5.000000000000000000 ) ) ;
#15906 = ORIENTED_EDGE ( 'NONE', *, *, #103119, .T. ) ;
#15907 = CARTESIAN_POINT ( 'NONE',  ( 5.250000000000000000, -7.464222240803106570E-16, -6.094999999999989981 ) ) ;
#15908 = CARTESIAN_POINT ( 'NONE',  ( 12.29974487139158512, -27.71228299555214747, 4.000000000000000000 ) ) ;
#15909 = CARTESIAN_POINT ( 'NONE',  ( -14.14994871458967474, -8.240707523384186217, 17.25253755692235558 ) ) ;
#15910 = EDGE_CURVE ( 'NONE', #108316, #48577, #66087, .T. ) ;
#15911 = LINE ( 'NONE', #6458, #46460 ) ;
#15912 = FACE_BOUND ( 'NONE', #4223, .T. ) ;
#15913 = ORIENTED_EDGE ( 'NONE', *, *, #84694, .T. ) ;
#15914 = DIRECTION ( 'NONE',  ( 0.3543493200069162685, -0.000000000000000000, -0.9351131265310288487 ) ) ;
#15915 = ADVANCED_FACE ( 'NONE', ( #13086 ), #77674, .F. ) ;
#15916 = PLANE ( 'NONE',  #85134 ) ;
#15917 = SURFACE_STYLE_USAGE ( .BOTH. , #136311 ) ;
#15918 = VERTEX_POINT ( 'NONE', #112431 ) ;
#15919 = DIRECTION ( 'NONE',  ( 0.7071067811865487940, 0.7071067811865463515, 0.000000000000000000 ) ) ;
#15920 = ORIENTED_EDGE ( 'NONE', *, *, #126161, .T. ) ;
#15921 = EDGE_LOOP ( 'NONE', ( #58284, #68166, #136066, #54622 ) ) ;
#15922 = ORIENTED_EDGE ( 'NONE', *, *, #124910, .F. ) ;
#15923 = EDGE_CURVE ( 'NONE', #4732, #53545, #123331, .T. ) ;
#15924 = ADVANCED_FACE ( 'NONE', ( #13793 ), #78381, .F. ) ;
#15925 = CARTESIAN_POINT ( 'NONE',  ( 36.51626352523145158, -4.472830434245838482, 4.472830434245838482 ) ) ;
#15926 = ORIENTED_EDGE ( 'NONE', *, *, #107582, .T. ) ;
#15927 = LINE ( 'NONE', #4308, #6679 ) ;
#15928 = CARTESIAN_POINT ( 'NONE',  ( -28.49999999999979039, -14.94781430457067906, 5.000000000000000000 ) ) ;
#15929 = FACE_OUTER_BOUND ( 'NONE', #70759, .T. ) ;
#15930 = EDGE_CURVE ( 'NONE', #27998, #68281, #79125, .T. ) ;
#15931 = ORIENTED_EDGE ( 'NONE', *, *, #102498, .T. ) ;
#15932 = PLANE ( 'NONE',  #69068 ) ;
#15933 = DIRECTION ( 'NONE',  ( -0.6830127018922181881, 0.6830127018922202975, -0.2588190451025214056 ) ) ;
#15934 = EDGE_CURVE ( 'NONE', #24150, #98637, #55201, .T. ) ;
#15935 = CARTESIAN_POINT ( 'NONE',  ( -34.49999999999975131, 19.46425560840030400, 4.994342998332171213 ) ) ;
#15936 = CARTESIAN_POINT ( 'NONE',  ( 63.18398860626900415, 28.73617430169831621, 5.000000000000000000 ) ) ;
#15937 = CARTESIAN_POINT ( 'NONE',  ( -24.18398860626899705, 28.73617430169804265, 5.000000000000000000 ) ) ;
#15938 = CARTESIAN_POINT ( 'NONE',  ( 0.1839886062690032631, 28.73617430169787568, 5.000000000000000000 ) ) ;
#15939 = VERTEX_POINT ( 'NONE', #76979 ) ;
#15940 = ORIENTED_EDGE ( 'NONE', *, *, #68289, .T. ) ;
#15941 = AXIS2_PLACEMENT_3D ( 'NONE', #133454, #110938, #108082 ) ;
#15942 = ORIENTED_EDGE ( 'NONE', *, *, #7701, .T. ) ;
#15943 = ORIENTED_EDGE ( 'NONE', *, *, #84424, .F. ) ;
#15944 = FACE_OUTER_BOUND ( 'NONE', #25192, .T. ) ;
#15946 = EDGE_CURVE ( 'NONE', #12209, #59656, #110256, .T. ) ;
#15945 = VECTOR ( 'NONE', #127972, 1000.000000000000000 ) ;
#15947 = AXIS2_PLACEMENT_3D ( 'NONE', #111982, #101074, #1725 ) ;
#15948 = EDGE_LOOP ( 'NONE', ( #79407, #27347, #71353, #102016 ) ) ;
#15949 = VECTOR ( 'NONE', #128618, 1000.000000000000000 ) ;
#15951 = VERTEX_POINT ( 'NONE', #11648 ) ;
#15950 = AXIS2_PLACEMENT_3D ( 'NONE', #611, #77510, #22348 ) ;
#15952 = LINE ( 'NONE', #137071, #106969 ) ;
#15953 = B_SPLINE_CURVE_WITH_KNOTS ( 'NONE', 3,
 ( #13934, #90833, #48041, #103115 ),
 .UNSPECIFIED., .F., .F.,
 ( 4, 4 ),
 ( 0.008853860144884173958, 0.009403245473020183098 ),
 .UNSPECIFIED. ) ;
#15954 = DIRECTION ( 'NONE',  ( -0.000000000000000000, 0.3543493200069153248, 0.9351131265310292928 ) ) ;
#15955 = ORIENTED_EDGE ( 'NONE', *, *, #126042, .T. ) ;
#15956 = CARTESIAN_POINT ( 'NONE',  ( -45.18398860626900415, 28.73617430169818832, 5.000000000000000000 ) ) ;
#15957 = EDGE_CURVE ( 'NONE', #124568, #40245, #51390, .T. ) ;
#15959 = ORIENTED_EDGE ( 'NONE', *, *, #54328, .F. ) ;
#15958 = MECHANICAL_DESIGN_GEOMETRIC_PRESENTATION_REPRESENTATION (  '', ( #25208 ), #136349 ) ;
#15960 = CARTESIAN_POINT ( 'NONE',  ( 1.179999999999999272, 10.00000000000000178, 6.750000000000000888 ) ) ;
#15961 = FACE_OUTER_BOUND ( 'NONE', #3058, .T. ) ;
#15962 = CARTESIAN_POINT ( 'NONE',  ( 3.712903141435219379, 3.967499999999992699, -6.871911579029513994 ) ) ;
#15963 = EDGE_LOOP ( 'NONE', ( #10213, #111816, #125433 ) ) ;
#15965 = LINE ( 'NONE', #60257, #100876 ) ;
#15964 = CARTESIAN_POINT ( 'NONE',  ( 100.6829301918981230, -1.637169565754159173, -6.109999999999999432 ) ) ;
#15966 = DIRECTION ( 'NONE',  ( -0.7071067811865486830, -0.7071067811865464625, 0.000000000000000000 ) ) ;
#15967 = LINE ( 'NONE', #118148, #92857 ) ;
#15968 = ORIENTED_EDGE ( 'NONE', *, *, #21836, .F. ) ;
#15969 = ADVANCED_FACE ( 'NONE', ( #113124 ), #111720, .F. ) ;
#15970 = ORIENTED_EDGE ( 'NONE', *, *, #97633, .F. ) ;
#15971 = CARTESIAN_POINT ( 'NONE',  ( -39.48921356237310221, -27.52281430457082934, 5.000000000000000000 ) ) ;
#15972 = EDGE_LOOP ( 'NONE', ( #678, #93222, #86308, #127397 ) ) ;
#15973 = AXIS2_PLACEMENT_3D ( 'NONE', #118174, #64540, #97124 ) ;
#15974 = LINE ( 'NONE', #82716, #62577 ) ;
#15976 = PLANE ( 'NONE',  #6922 ) ;
#15975 = VECTOR ( 'NONE', #88677, 999.9999999999998863 ) ;
#15977 = CARTESIAN_POINT ( 'NONE',  ( -6.299744871391586898, -27.71228299555210484, 4.000000000000000000 ) ) ;
#15978 = CARTESIAN_POINT ( 'NONE',  ( 19.88840764549667384, 2.500000000000003553, 3.061616997868386099E-16 ) ) ;
#15979 = LINE ( 'NONE', #138524, #7810 ) ;
#15980 = EDGE_LOOP ( 'NONE', ( #6077, #108307, #76296, #79937, #127755 ) ) ;
#15981 = EDGE_CURVE ( 'NONE', #23291, #113319, #22526, .T. ) ;
#15982 = LINE ( 'NONE', #104448, #127012 ) ;
#15983 = VECTOR ( 'NONE', #59091, 1000.000000000000000 ) ;
#15984 = EDGE_CURVE ( 'NONE', #113440, #71320, #783, .T. ) ;
#15985 = DIRECTION ( 'NONE',  ( -0.7071067811865487940, 0.7071067811865463515, -0.000000000000000000 ) ) ;
#15986 = DIRECTION ( 'NONE',  ( 0.000000000000000000, -1.000000000000000000, 0.000000000000000000 ) ) ;
#15987 = ORIENTED_EDGE ( 'NONE', *, *, #121896, .F. ) ;
#15988 = CARTESIAN_POINT ( 'NONE',  ( -23.99999999999982592, 11.96639925780213964, 5.000000000000000000 ) ) ;
#15989 = MECHANICAL_DESIGN_GEOMETRIC_PRESENTATION_REPRESENTATION (  '', ( #80836 ), #78548 ) ;
#15992 = EDGE_CURVE ( 'NONE', #3604, #29061, #106929, .T. ) ;
#15991 = VECTOR ( 'NONE', #102556, 1000.000000000000000 ) ;
#15990 = CARTESIAN_POINT ( 'NONE',  ( 14.99451991528749595, 28.92564299267948513, 4.000000000000000000 ) ) ;
#15993 = ORIENTED_EDGE ( 'NONE', *, *, #77275, .F. ) ;
#15994 = VECTOR ( 'NONE', #45687, 999.9999999999998863 ) ;
#15996 = ORIENTED_EDGE ( 'NONE', *, *, #52146, .T. ) ;
#15995 = DIRECTION ( 'NONE',  ( -0.3543493200069162685, -0.000000000000000000, -0.9351131265310288487 ) ) ;
#15997 = VERTEX_POINT ( 'NONE', #12386 ) ;
#15998 = FACE_OUTER_BOUND ( 'NONE', #29789, .T. ) ;
#15999 = AXIS2_PLACEMENT_3D ( 'NONE', #67246, #47674, #133926 ) ;
#16000 = SURFACE_STYLE_FILL_AREA ( #115302 ) ;
#16001 = EDGE_LOOP ( 'NONE', ( #131871, #119552, #61149, #29924 ) ) ;
#16002 = CARTESIAN_POINT ( 'NONE',  ( 36.29974487139159578, -27.71228299555231445, 4.000000000000000000 ) ) ;
#16003 = VECTOR ( 'NONE', #55244, 1000.000000000000000 ) ;
#16004 = DIRECTION ( 'NONE',  ( -0.7071067811865487940, 0.7071067811865463515, -0.000000000000000000 ) ) ;
#16005 = PRESENTATION_STYLE_ASSIGNMENT (( #116779 ) ) ;
#16006 = VERTEX_POINT ( 'NONE', #79850 ) ;
#16007 = EDGE_CURVE ( 'NONE', #141150, #76474, #58089, .T. ) ;
#16008 = DIRECTION ( 'NONE',  ( -0.8571673007021110013, 1.049727191138617093E-16, 0.5150380749100563760 ) ) ;
#16009 = DIRECTION ( 'NONE',  ( 0.3543493200069162685, -0.000000000000000000, -0.9351131265310288487 ) ) ;
#16010 = LINE ( 'NONE', #69200, #20930 ) ;
#16011 = CARTESIAN_POINT ( 'NONE',  ( 26.29289321881327623, 14.25929247661557753, 5.000000000000000000 ) ) ;
#16012 = PRESENTATION_LAYER_ASSIGNMENT (  '', '', ( #76294 ) ) ;
#16013 = DIRECTION ( 'NONE',  ( -1.000000000000000000, -1.224606353822377258E-16, -0.000000000000000000 ) ) ;
#16014 = DIRECTION ( 'NONE',  ( 0.3543493200069162685, -0.000000000000000000, -0.9351131265310288487 ) ) ;
#16015 = ADVANCED_FACE ( 'NONE', ( #100833 ), #134930, .T. ) ;
#16016 = LINE ( 'NONE', #5140, #132274 ) ;
#16017 = CARTESIAN_POINT ( 'NONE',  ( -56.99451991528749062, 28.92564299267978001, 4.000000000000000000 ) ) ;
#16018 = ORIENTED_EDGE ( 'NONE', *, *, #7796, .F. ) ;
#16019 = VERTEX_POINT ( 'NONE', #102289 ) ;
#16020 = ORIENTED_EDGE ( 'NONE', *, *, #20401, .F. ) ;
#16021 = CARTESIAN_POINT ( 'NONE',  ( 123.6458333333333286, 2.130196079827431976, -7.949999999999999289 ) ) ;
#16022 = VERTEX_POINT ( 'NONE', #132055 ) ;
#16023 = ORIENTED_EDGE ( 'NONE', *, *, #12577, .F. ) ;
#16024 = VERTEX_POINT ( 'NONE', #32745 ) ;
#16025 = DIRECTION ( 'NONE',  ( -0.7071067811865486830, -0.7071067811865464625, -0.000000000000000000 ) ) ;
#16026 = ORIENTED_EDGE ( 'NONE', *, *, #75182, .F. ) ;
#16027 = DIRECTION ( 'NONE',  ( 0.7071067811865487940, 0.7071067811865463515, 0.000000000000000000 ) ) ;
#16028 = DIRECTION ( 'NONE',  ( 0.6830127018922181881, 0.6830127018922202975, -0.2588190451025214056 ) ) ;
#16029 = DIRECTION ( 'NONE',  ( -0.6830127018922181881, 0.6830127018922202975, -0.2588190451025214056 ) ) ;
#16030 = CARTESIAN_POINT ( 'NONE',  ( 117.3962635252314470, 4.472830434245840259, -4.472830434245839371 ) ) ;
#16031 = ORIENTED_EDGE ( 'NONE', *, *, #94382, .T. ) ;
#16033 = CARTESIAN_POINT ( 'NONE',  ( -8.782784137141019798, 10.22668762134568077, -28.70197684735530075 ) ) ;
#16032 = APPLICATION_CONTEXT ( 'automotive_design' ) ;
#16034 = CARTESIAN_POINT ( 'NONE',  ( 32.99451991528749062, 28.92564299267960948, 4.000000000000000000 ) ) ;
#16035 = CARTESIAN_POINT ( 'NONE',  ( 1.500000000000001332, 4.087461875839200509, 4.000000000000000000 ) ) ;
#16036 = CARTESIAN_POINT ( 'NONE',  ( 56.99451991528749062, 28.92564299267978001, 4.000000000000000000 ) ) ;
#16037 = PLANE ( 'NONE',  #126432 ) ;
#16038 = CARTESIAN_POINT ( 'NONE',  ( 38.72502705046289151, 5.819803920172573086, -5.819803920172572198 ) ) ;
#16039 = CARTESIAN_POINT ( 'NONE',  ( 13.49159235450332162, 9.902892378096218942E-16, 0.000000000000000000 ) ) ;
#16040 = EDGE_CURVE ( 'NONE', #113241, #96641, #10933, .T. ) ;
#16041 = SURFACE_SIDE_STYLE ('',( #36418 ) ) ;
#16042 = ORIENTED_EDGE ( 'NONE', *, *, #129738, .T. ) ;
#16043 = ORIENTED_EDGE ( 'NONE', *, *, #123732, .F. ) ;
#16044 = CARTESIAN_POINT ( 'NONE',  ( 38.47916666666665009, -7.950000000000001066, 2.130196079827424427 ) ) ;
#16045 = ORIENTED_EDGE ( 'NONE', *, *, #1162, .F. ) ;
#16046 = VERTEX_POINT ( 'NONE', #125454 ) ;
#16047 = PLANE ( 'NONE',  #90008 ) ;
#16048 = DIRECTION ( 'NONE',  ( -0.6830127018922181881, 0.6830127018922202975, -0.2588190451025214056 ) ) ;
#16049 = ORIENTED_EDGE ( 'NONE', *, *, #44502, .F. ) ;
#16050 = DIRECTION ( 'NONE',  ( -1.000000000000000000, 0.000000000000000000, 0.000000000000000000 ) ) ;
#16051 = PRESENTATION_STYLE_ASSIGNMENT (( #26967 ) ) ;
#16052 = LINE ( 'NONE', #122155, #118372 ) ;
#16053 = CARTESIAN_POINT ( 'NONE',  ( 33.25043019189810423, 3.055000000000002824, -5.291415217122919401 ) ) ;
#16054 = ORIENTED_EDGE ( 'NONE', *, *, #50542, .T. ) ;
#16055 = DIRECTION ( 'NONE',  ( 0.6830127018922180770, -0.6830127018922204085, -0.2588190451025213501 ) ) ;
#16056 = VERTEX_POINT ( 'NONE', #47917 ) ;
#16057 = CARTESIAN_POINT ( 'NONE',  ( 48.18398860626899705, 28.73617430169820608, 5.000000000000000000 ) ) ;
#16058 = VECTOR ( 'NONE', #9551, 1000.000000000000000 ) ;
#16059 = VECTOR ( 'NONE', #134617, 1000.000000000000000 ) ;
#16060 = AXIS2_PLACEMENT_3D ( 'NONE', #78432, #67579, #24750 ) ;
#16061 = CARTESIAN_POINT ( 'NONE',  ( -17.01088028653936490, -22.02621442084248216, 4.990779571109221990 ) ) ;
#16062 = CARTESIAN_POINT ( 'NONE',  ( -15.18398860626900237, 28.73617430169797871, 5.000000000000000000 ) ) ;
#16063 = VECTOR ( 'NONE', #105622, 1000.000000000000000 ) ;
#16064 = FACE_OUTER_BOUND ( 'NONE', #28336, .T. ) ;
#16065 = ORIENTED_EDGE ( 'NONE', *, *, #86789, .T. ) ;
#16066 = ORIENTED_EDGE ( 'NONE', *, *, #13430, .F. ) ;
#16067 = CARTESIAN_POINT ( 'NONE',  ( 0.000000000000000000, 0.000000000000000000, 5.000000000000000000 ) ) ;
#16068 = CARTESIAN_POINT ( 'NONE',  ( -38.39513766812456197, 21.75929247661549226, 21.32995629748195299 ) ) ;
#16069 = DIRECTION ( 'NONE',  ( -0.7071067811865487940, 0.7071067811865463515, -0.000000000000000000 ) ) ;
#16070 = CARTESIAN_POINT ( 'NONE',  ( -10.49999999999992184, -16.53360074219757081, 5.000000000000000000 ) ) ;
#16071 = AXIS2_PLACEMENT_3D ( 'NONE', #523, #11378, #33221 ) ;
#16072 = VECTOR ( 'NONE', #80423, 1000.000000000000227 ) ;
#16073 = CARTESIAN_POINT ( 'NONE',  ( 52.70376352523144448, 6.109999999999998543, 1.122388791418548911E-15 ) ) ;
#16074 = ORIENTED_EDGE ( 'NONE', *, *, #103559, .F. ) ;
#16075 = CARTESIAN_POINT ( 'NONE',  ( 124.9583333333333428, 3.974999999999997424, 6.884901960086288852 ) ) ;
#16076 = DIRECTION ( 'NONE',  ( -0.000000000000000000, 0.000000000000000000, 1.000000000000000000 ) ) ;
#16077 = ORIENTED_EDGE ( 'NONE', *, *, #135002, .T. ) ;
#16078 = VERTEX_POINT ( 'NONE', #61643 ) ;
#16079 = VECTOR ( 'NONE', #54272, 1000.000000000000227 ) ;
#16080 = CARTESIAN_POINT ( 'NONE',  ( 0.000000000000000000, 0.000000000000000000, 5.000000000000000000 ) ) ;
#16081 = VERTEX_POINT ( 'NONE', #71087 ) ;
#16082 =( BOUNDED_CURVE ( )  B_SPLINE_CURVE ( 3, ( #2632, #45478, #101965, #89655 ),
 .UNSPECIFIED., .F., .F. ) 
 B_SPLINE_CURVE_WITH_KNOTS ( ( 4, 4 ),
 ( 1.502886732431669481, 1.547827028402603444 ),
 .UNSPECIFIED. ) 
 CURVE ( )  GEOMETRIC_REPRESENTATION_ITEM ( )  RATIONAL_B_SPLINE_CURVE ( ( 1.000000000000000000, 0.9998317045644854462, 0.9998317045644854462, 1.000000000000000000 ) ) 
 REPRESENTATION_ITEM ( '' )  );
#16083 = VECTOR ( 'NONE', #68028, 1000.000000000000000 ) ;
#16084 = LINE ( 'NONE', #38604, #74285 ) ;
#16085 = EDGE_LOOP ( 'NONE', ( #96094, #142214, #32431, #95338 ) ) ;
#16086 = PRESENTATION_STYLE_ASSIGNMENT (( #47392 ) ) ;
#16087 = EDGE_CURVE ( 'NONE', #100461, #109420, #115231, .T. ) ;
#16088 = CARTESIAN_POINT ( 'NONE',  ( -39.29974487139159578, -27.71228299555233576, 4.000000000000000000 ) ) ;
#16089 = VECTOR ( 'NONE', #130049, 1000.000000000000227 ) ;
#16090 = AXIS2_PLACEMENT_3D ( 'NONE', #95766, #137869, #5872 ) ;
#16092 = AXIS2_PLACEMENT_3D ( 'NONE', #43350, #10676, #85396 ) ;
#16091 =( LENGTH_UNIT ( ) NAMED_UNIT ( * ) SI_UNIT ( .MILLI., .METRE. ) );
#16093 = ADVANCED_FACE ( 'NONE', ( #126166 ), #126848, .F. ) ;
#16094 = FACE_BOUND ( 'NONE', #102277, .T. ) ;
#16095 = DIRECTION ( 'NONE',  ( 0.000000000000000000, -1.000000000000000000, 0.000000000000000000 ) ) ;
#16096 = EDGE_CURVE ( 'NONE', #95958, #135598, #36302, .T. ) ;
#16097 = EDGE_CURVE ( 'NONE', #62156, #42914, #72545, .T. ) ;
#16098 = VECTOR ( 'NONE', #1507, 999.9999999999998863 ) ;
#16099 = CARTESIAN_POINT ( 'NONE',  ( -18.18398860626898994, 28.73617430169800002, 5.000000000000000000 ) ) ;
#16100 = VERTEX_POINT ( 'NONE', #48601 ) ;
#16101 = LINE ( 'NONE', #5939, #110572 ) ;
#16103 = VERTEX_POINT ( 'NONE', #5048 ) ;
#16102 = LINE ( 'NONE', #92993, #52915 ) ;
#16104 = AXIS2_PLACEMENT_3D ( 'NONE', #82953, #81550, #51039 ) ;
#16105 = DIRECTION ( 'NONE',  ( 0.7071067811865486830, -0.7071067811865464625, -0.000000000000000000 ) ) ;
#16106 = EDGE_LOOP ( 'NONE', ( #54586, #56183, #38311 ) ) ;
#16107 = EDGE_CURVE ( 'NONE', #70402, #27000, #135616, .T. ) ;
#16108 = ADVANCED_FACE ( 'NONE', ( #27536 ), #137036, .F. ) ;
#16109 = ORIENTED_EDGE ( 'NONE', *, *, #135904, .T. ) ;
#16110 = CARTESIAN_POINT ( 'NONE',  ( 68.45376352523143737, -6.109999999999998543, -3.741295971395162543E-16 ) ) ;
#16111 = EDGE_LOOP ( 'NONE', ( #137898, #121790, #22098, #116284 ) ) ;
#16112 = DIRECTION ( 'NONE',  ( 0.7071067811865487940, 0.7071067811865463515, 0.000000000000000000 ) ) ;
#16113 = LINE ( 'NONE', #12034, #42702 ) ;
#16114 = ADVANCED_FACE ( 'NONE', ( #137766 ), #116707, .F. ) ;
#16115 = ORIENTED_EDGE ( 'NONE', *, *, #20089, .T. ) ;
#16116 = CYLINDRICAL_SURFACE ( 'NONE', #97673, 6.000000000000000000 ) ;
#16117 = VECTOR ( 'NONE', #101448, 1000.000000000000000 ) ;
#16118 = EDGE_CURVE ( 'NONE', #65821, #13457, #80532, .T. ) ;
#16119 = EDGE_CURVE ( 'NONE', #92930, #39160, #82665, .T. ) ;
#16120 = CARTESIAN_POINT ( 'NONE',  ( -20.99999999999984368, 8.816494571476647835, 4.604407763760409722 ) ) ;
#16121 = CARTESIAN_POINT ( 'NONE',  ( 0.000000000000000000, 0.000000000000000000, 5.000000000000000000 ) ) ;
#16122 = DIRECTION ( 'NONE',  ( 0.7071067811865487940, 0.7071067811865463515, 0.000000000000000000 ) ) ;
#16123 = CARTESIAN_POINT ( 'NONE',  ( 31.82816939922330235, 12.75929247661557930, 4.000000000000000000 ) ) ;
#16124 = FILL_AREA_STYLE ('',( #95137 ) ) ;
#16125 = EDGE_LOOP ( 'NONE', ( #62876, #23900, #108585, #114920 ) ) ;
#16126 = ORIENTED_EDGE ( 'NONE', *, *, #23529, .F. ) ;
#16127 = LINE ( 'NONE', #93731, #52007 ) ;
#16128 = DIRECTION ( 'NONE',  ( 0.3543493200069162685, -0.000000000000000000, -0.9351131265310288487 ) ) ;
#16129 = VERTEX_POINT ( 'NONE', #69669 ) ;
#16130 = ADVANCED_FACE ( 'NONE', ( #113846 ), #138471, .F. ) ;
#16131 = EDGE_LOOP ( 'NONE', ( #11174, #28695, #133507, #138448 ) ) ;
#16132 = VERTEX_POINT ( 'NONE', #63777 ) ;
#16133 = CARTESIAN_POINT ( 'NONE',  ( -51.29974487139158867, -27.71228299555242103, 4.000000000000000000 ) ) ;
#16134 = CARTESIAN_POINT ( 'NONE',  ( 55.49586038379622721, -3.974999999999998312, -6.884901960086286188 ) ) ;
#16135 = DIRECTION ( 'NONE',  ( -1.000000000000000000, 1.242409592863268950E-14, 0.000000000000000000 ) ) ;
#16136 = ORIENTED_EDGE ( 'NONE', *, *, #83954, .F. ) ;
#16137 = DIRECTION ( 'NONE',  ( 0.3543493200069162685, -0.000000000000000000, -0.9351131265310288487 ) ) ;
#16138 = EDGE_CURVE ( 'NONE', #96656, #71407, #75361, .T. ) ;
#16139 = FACE_OUTER_BOUND ( 'NONE', #77895, .T. ) ;
#16140 = CARTESIAN_POINT ( 'NONE',  ( 7.358736474768553748, 5.808823158059031044, -5.808823158059038150 ) ) ;
#16141 = DIRECTION ( 'NONE',  ( -0.7071067811865487940, 0.7071067811865463515, -0.000000000000000000 ) ) ;
#16142 = VERTEX_POINT ( 'NONE', #120230 ) ;
#16143 = DIRECTION ( 'NONE',  ( -0.7071067811865486830, -0.7071067811865464625, 0.000000000000000000 ) ) ;
#16144 = FACE_OUTER_BOUND ( 'NONE', #104632, .T. ) ;
#16145 = EDGE_CURVE ( 'NONE', #92724, #81113, #52162, .T. ) ;
#16146 = CARTESIAN_POINT ( 'NONE',  ( -34.92500000000001137, 9.759292476615614831, 4.255531930566240462 ) ) ;
#16148 = ORIENTED_EDGE ( 'NONE', *, *, #109856, .T. ) ;
#16147 = CARTESIAN_POINT ( 'NONE',  ( 19.88840764549667384, 9.139736423841732040E-16, 0.000000000000000000 ) ) ;
#16149 = CARTESIAN_POINT ( 'NONE',  ( 45.48921356237309510, -27.52281430457087197, 5.000000000000000000 ) ) ;
#16150 = EDGE_LOOP ( 'NONE', ( #102820, #59770, #119214, #54096 ) ) ;
#16151 = CARTESIAN_POINT ( 'NONE',  ( 14.99451991528749595, 28.92564299267948513, 4.000000000000000000 ) ) ;
#16152 = DIRECTION ( 'NONE',  ( 0.3543493200069162685, -0.000000000000000000, -0.9351131265310288487 ) ) ;
#16153 = ORIENTED_EDGE ( 'NONE', *, *, #36259, .T. ) ;
#16154 = ADVANCED_FACE ( 'NONE', ( #52852 ), #119525, .F. ) ;
#16155 = VECTOR ( 'NONE', #36172, 1000.000000000000227 ) ;
#16156 = EDGE_CURVE ( 'NONE', #125554, #128057, #129003, .T. ) ;
#16157 = CARTESIAN_POINT ( 'NONE',  ( -28.49999999999979394, -11.94781430457070392, 5.000000000000000000 ) ) ;
#16158 = DIRECTION ( 'NONE',  ( -0.7071067811865486830, -0.7071067811865464625, -0.000000000000000000 ) ) ;
#16159 = FACE_OUTER_BOUND ( 'NONE', #111935, .T. ) ;
#16160 = ORIENTED_EDGE ( 'NONE', *, *, #19312, .F. ) ;
#16161 = AXIS2_PLACEMENT_3D ( 'NONE', #27573, #16710, #59535 ) ;
#16162 = VECTOR ( 'NONE', #67200, 1000.000000000000000 ) ;
#16163 = AXIS2_PLACEMENT_3D ( 'NONE', #6514, #95715, #51522 ) ;
#16164 = PLANE ( 'NONE',  #115612 ) ;
#16165 = LINE ( 'NONE', #103643, #60878 ) ;
#16166 = EDGE_CURVE ( 'NONE', #32877, #22044, #18807, .T. ) ;
#16168 = EDGE_CURVE ( 'NONE', #13363, #42048, #41277, .T. ) ;
#16167 = CARTESIAN_POINT ( 'NONE',  ( -20.99999999999985079, 12.83542986846995149, -1.025386466790322304 ) ) ;
#16169 = MECHANICAL_DESIGN_GEOMETRIC_PRESENTATION_REPRESENTATION (  '', ( #134295 ), #27793 ) ;
#16170 = CARTESIAN_POINT ( 'NONE',  ( -33.48921356237309510, -27.52281430457078670, 5.000000000000000000 ) ) ;
#16171 = CARTESIAN_POINT ( 'NONE',  ( -12.69999999999998153, 3.061616997868383634E-16, -2.500000000000000444 ) ) ;
#16172 = VERTEX_POINT ( 'NONE', #62351 ) ;
#16173 = VERTEX_POINT ( 'NONE', #140586 ) ;
#16174 = CARTESIAN_POINT ( 'NONE',  ( 2.924914550060625285, 4.584330080086930965E-16, 0.000000000000000000 ) ) ;
#16175 = AXIS2_PLACEMENT_3D ( 'NONE', #128749, #19280, #43190 ) ;
#16176 = LINE ( 'NONE', #125710, #99189 ) ;
#16177 = CARTESIAN_POINT ( 'NONE',  ( 4.499569808101886892, -3.967499999999998028, -6.871911579029511330 ) ) ;
#16178 = CARTESIAN_POINT ( 'NONE',  ( 34.92499999999998295, 19.44114312045510218, 6.054907437694465600 ) ) ;
#16179 = DIRECTION ( 'NONE',  ( -0.7071067811865487940, 0.7071067811865463515, 0.000000000000000000 ) ) ;
#16180 = CARTESIAN_POINT ( 'NONE',  ( 34.45011844616451668, -13.48371918836236638, 5.000000000000000000 ) ) ;
#16181 = CARTESIAN_POINT ( 'NONE',  ( 5.691592354503320905, 9.902892378096218942E-16, 0.000000000000000000 ) ) ;
#16182 = ORIENTED_EDGE ( 'NONE', *, *, #135695, .F. ) ;
#16183 = ADVANCED_FACE ( 'NONE', ( #129712 ), #84794, .T. ) ;
#16184 = DIRECTION ( 'NONE',  ( -0.6830127018922181881, 0.6830127018922202975, -0.2588190451025214056 ) ) ;
#16185 = CARTESIAN_POINT ( 'NONE',  ( 4.600000000000001421, 9.521314400968980422E-16, 0.000000000000000000 ) ) ;
#16186 = VECTOR ( 'NONE', #34990, 1000.000000000000000 ) ;
#16187 = VECTOR ( 'NONE', #36072, 1000.000000000000000 ) ;
#16188 = LINE ( 'NONE', #18323, #143245 ) ;
#16189 = CARTESIAN_POINT ( 'NONE',  ( 47.45376352523145158, -6.109999999999999432, -3.741295971395163529E-16 ) ) ;
#16190 = DIRECTION ( 'NONE',  ( 0.7071067811865487940, -0.7071067811865463515, 0.000000000000000000 ) ) ;
#16191 = VECTOR ( 'NONE', #98815, 999.9999999999998863 ) ;
#16192 = ORIENTED_EDGE ( 'NONE', *, *, #44118, .F. ) ;
#16193 = EDGE_CURVE ( 'NONE', #111746, #10669, #29679, .T. ) ;
#16194 = ORIENTED_EDGE ( 'NONE', *, *, #124096, .T. ) ;
#16195 = CIRCLE ( 'NONE', #44083, 2.500000000000000444 ) ;
#16196 = VERTEX_POINT ( 'NONE', #73919 ) ;
#16197 = DIRECTION ( 'NONE',  ( -0.7071067811865486830, -0.7071067811865464625, 0.000000000000000000 ) ) ;
#16198 = VECTOR ( 'NONE', #4235, 1000.000000000000000 ) ;
#16199 = LINE ( 'NONE', #125735, #16473 ) ;
#16200 = FACE_OUTER_BOUND ( 'NONE', #13619, .T. ) ;
#16201 = EDGE_CURVE ( 'NONE', #54027, #116082, #118098, .T. ) ;
#16202 = CARTESIAN_POINT ( 'NONE',  ( -57.48921356237308800, -27.52281430457095368, 5.000000000000000000 ) ) ;
#16203 = SURFACE_STYLE_USAGE ( .BOTH. , #39446 ) ;
#16204 = VECTOR ( 'NONE', #49226, 1000.000000000000227 ) ;
#16205 = ORIENTED_EDGE ( 'NONE', *, *, #130583, .F. ) ;
#16206 = CARTESIAN_POINT ( 'NONE',  ( -2.999999999999978240, -8.731860332648842871, -2.120594902707545693 ) ) ;
#16207 = DIRECTION ( 'NONE',  ( -0.7071067811865486830, -0.7071067811865464625, 0.000000000000000000 ) ) ;
#16208 = CIRCLE ( 'NONE', #97233, 2.500000000000000444 ) ;
#16209 = CARTESIAN_POINT ( 'NONE',  ( 34.92499999999998295, -22.22500000000000142, 4.500000000000000888 ) ) ;
#16210 = DIRECTION ( 'NONE',  ( -1.000000000000000000, -1.224606353822377258E-16, -0.000000000000000000 ) ) ;
#16211 = CARTESIAN_POINT ( 'NONE',  ( 116.7916666666666714, 3.975000000000003642, -6.884901960086285300 ) ) ;
#16212 = CARTESIAN_POINT ( 'NONE',  ( 63.07919371712955581, 3.975000000000002753, -6.884901960086283523 ) ) ;
#16213 = LINE ( 'NONE', #3898, #110780 ) ;
#16214 = VECTOR ( 'NONE', #32194, 1000.000000000000000 ) ;
#16215 = EDGE_LOOP ( 'NONE', ( #129024, #134222, #35659, #85921 ) ) ;
#16216 = EDGE_LOOP ( 'NONE', ( #139615, #127709, #83449, #77657 ) ) ;
#16217 = CARTESIAN_POINT ( 'NONE',  ( 65.02083333333334281, 7.949999999999999289, 2.130196079827431532 ) ) ;
#16218 = DIRECTION ( 'NONE',  ( -0.7071067811865486830, -0.7071067811865464625, 0.000000000000000000 ) ) ;
#16219 = DIRECTION ( 'NONE',  ( 0.7071067811865487940, 0.7071067811865463515, 0.000000000000000000 ) ) ;
#16220 = AXIS2_PLACEMENT_3D ( 'NONE', #111826, #121251, #44451 ) ;
#16221 = ORIENTED_EDGE ( 'NONE', *, *, #108591, .T. ) ;
#16222 = EDGE_CURVE ( 'NONE', #46584, #98313, #18062, .T. ) ;
#16223 = EDGE_CURVE ( 'NONE', #107048, #83184, #51466, .T. ) ;
#16224 = DIRECTION ( 'NONE',  ( -1.000000000000000000, -1.224606353822377258E-16, -0.000000000000000000 ) ) ;
#16225 = CARTESIAN_POINT ( 'NONE',  ( 59.06293019189809712, 1.637169565754157174, 6.110000000000002984 ) ) ;
#16226 = DIRECTION ( 'NONE',  ( -0.6830127018922181881, 0.6830127018922202975, -0.2588190451025214056 ) ) ;
#16227 = ORIENTED_EDGE ( 'NONE', *, *, #51792, .F. ) ;
#16228 = ORIENTED_EDGE ( 'NONE', *, *, #6261, .T. ) ;
#16229 = VECTOR ( 'NONE', #88766, 1000.000000000000000 ) ;
#16230 = CARTESIAN_POINT ( 'NONE',  ( -21.29974487139158512, -27.71228299555221142, 4.000000000000000000 ) ) ;
#16231 = DIRECTION ( 'NONE',  ( 0.7071067811865487940, 0.7071067811865463515, 0.000000000000000000 ) ) ;
#16232 = CARTESIAN_POINT ( 'NONE',  ( 18.52400138585436551, 22.03583458319438648, 4.979811245910089390 ) ) ;
#16233 = DIRECTION ( 'NONE',  ( -1.000000000000000000, 0.000000000000000000, 0.000000000000000000 ) ) ;
#16234 = EDGE_CURVE ( 'NONE', #68584, #90591, #86942, .T. ) ;
#16235 = CARTESIAN_POINT ( 'NONE',  ( -28.36246187583881806, 22.22500000000000853, 4.000000000000000000 ) ) ;
#16237 = VERTEX_POINT ( 'NONE', #107248 ) ;
#16236 = CARTESIAN_POINT ( 'NONE',  ( 100.8500270504628986, -5.819803920172573086, -5.819803920172573086 ) ) ;
#16238 = CARTESIAN_POINT ( 'NONE',  ( -42.29974487139158157, -27.71228299555235708, 4.000000000000000000 ) ) ;
#16239 = CARTESIAN_POINT ( 'NONE',  ( 8.585466709768445170, -2.500000000000001776, 0.000000000000000000 ) ) ;
#16240 = CARTESIAN_POINT ( 'NONE',  ( 6.639999999999993463, -34.64999999999999858, -40.00000000000000000 ) ) ;
#16241 = VECTOR ( 'NONE', #49788, 1000.000000000000000 ) ;
#16242 = DIRECTION ( 'NONE',  ( 0.7071067811865487940, 0.7071067811865463515, 0.000000000000000000 ) ) ;
#16243 = CLOSED_SHELL ( 'NONE', ( #76042, #99156, #50442, #118200, #139262, #142524, #105420, #56673, #115495, #11111, #83621, #4747, #137523, #96623, #73242, #134531, #121584, #23425, #76383, #96450, #47704, #42737, #142729, #17124, #11168, #56831, #11817, #105467, #27455, #94205, #46810, #120649, #96166, #101250, #13477, #52568, #21289, #107295, #271, #19012, #87371, #23548, #30814, #84662, #107683, #70386, #117176, #87070, #82338, #16784, #69023, #70725, #42009, #111567, #128495, #85358, #66574, #65558, #24677, #21220, #7659, #61379, #45230, #77103, #124193, #138400, #54329, #52034, #39587, #20528, #139788, #78070, #68674, #135521, #141131, #45469, #46128, #77455, #75125, #89296, #134571, #36602, #44142, #135791, #41658, #24164, #14720, #105366, #141910, #60734, #107810, #142042, #94065, #20077, #70903, #131472, #70115, #13749, #28701, #95019, #105755, #66056, #78371, #106173, #90323, #31763, #123855, #34856, #18582, #2454, #142132, #19788, #65897, #134649, #114931, #108246, #70027, #53339, #32614, #8583, #62495, #79933, #54838, #91785, #118272, #103493, #43823, #29496, #97796, #63780, #140402, #134216, #107799, #31294, #51717, #26610, #62561, #50072, #86572, #50063, #139737, #9738, #61716, #120386, #48293, #41505, #111617, #122704, #39927, #92396, #2582, #101415, #112160, #127492, #59200, #89559, #143207, #10886, #46518, #31224, #121182, #49184, #36946, #142031, #79971, #58101, #127385, #30731, #15025, #75002, #60556, #17641, #90820, #115847, #134367, #124856, #120219, #93054, #14434, #46875, #36858, #10602 ) ) ;
#16244 = EDGE_LOOP ( 'NONE', ( #86637, #119742, #104921, #111558 ) ) ;
#16245 = ORIENTED_EDGE ( 'NONE', *, *, #131670, .F. ) ;
#16246 =( BOUNDED_CURVE ( )  B_SPLINE_CURVE ( 3, ( #36983, #92793, #125445, #37732 ),
 .UNSPECIFIED., .F., .T. ) 
 B_SPLINE_CURVE_WITH_KNOTS ( ( 4, 4 ),
 ( 1.864375635226959815, 1.933014472006526763 ),
 .UNSPECIFIED. ) 
 CURVE ( )  GEOMETRIC_REPRESENTATION_ITEM ( )  RATIONAL_B_SPLINE_CURVE ( ( 1.000000000000000000, 0.9996074310407769836, 0.9996074310407769836, 1.000000000000000000 ) ) 
 REPRESENTATION_ITEM ( '' )  );
#16247 = LINE ( 'NONE', #127180, #122887 ) ;
#16248 = CARTESIAN_POINT ( 'NONE',  ( -8.999999999999932498, 8.966399257802164513, 5.000000000000000000 ) ) ;
#16249 = CARTESIAN_POINT ( 'NONE',  ( 54.18398860626899705, 28.73617430169825226, 5.000000000000000000 ) ) ;
#16250 = ORIENTED_EDGE ( 'NONE', *, *, #49554, .T. ) ;
#16251 = ORIENTED_EDGE ( 'NONE', *, *, #52673, .F. ) ;
#16252 = DIRECTION ( 'NONE',  ( 0.7071067811865487940, -0.7071067811865463515, 0.000000000000000000 ) ) ;
#16253 = VECTOR ( 'NONE', #23705, 999.9999999999998863 ) ;
#16254 = ORIENTED_EDGE ( 'NONE', *, *, #66618, .F. ) ;
#16255 = VECTOR ( 'NONE', #85479, 1000.000000000000114 ) ;
#16257 = ORIENTED_EDGE ( 'NONE', *, *, #76140, .F. ) ;
#16256 = AXIS2_PLACEMENT_3D ( 'NONE', #137371, #82984, #61281 ) ;
#16258 = CARTESIAN_POINT ( 'NONE',  ( -25.39999999999996305, 3.061616997868383141E-16, -2.500000000000000000 ) ) ;
#16259 = ORIENTED_EDGE ( 'NONE', *, *, #21008, .F. ) ;
#16260 = ADVANCED_FACE ( 'NONE', ( #89096 ), #89777, .F. ) ;
#16261 = LINE ( 'NONE', #104735, #122064 ) ;
#16262 = CARTESIAN_POINT ( 'NONE',  ( 32.99999999999977973, 12.25461709320624060, -10.07315571508689622 ) ) ;
#16263 = MECHANICAL_DESIGN_GEOMETRIC_PRESENTATION_REPRESENTATION (  '', ( #69517 ), #25498 ) ;
#16264 = AXIS2_PLACEMENT_3D ( 'NONE', #102359, #26908, #137833 ) ;
#16265 = AXIS2_PLACEMENT_3D ( 'NONE', #69082, #115374, #136448 ) ;
#16266 = VECTOR ( 'NONE', #52353, 999.9999999999998863 ) ;
#16267 = FACE_BOUND ( 'NONE', #115775, .T. ) ;
#16268 = DIRECTION ( 'NONE',  ( -0.7071067811865487940, 0.7071067811865463515, -0.000000000000000000 ) ) ;
#16269 = EDGE_CURVE ( 'NONE', #116931, #32517, #77517, .T. ) ;
#16270 = FACE_OUTER_BOUND ( 'NONE', #48268, .T. ) ;
#16271 = LINE ( 'NONE', #53021, #129301 ) ;
#16272 = VECTOR ( 'NONE', #97158, 1000.000000000000000 ) ;
#16274 = VERTEX_POINT ( 'NONE', #134020 ) ;
#16273 = DIRECTION ( 'NONE',  ( 0.7071067811865487940, 0.7071067811865463515, -0.000000000000000000 ) ) ;
#16275 =( BOUNDED_CURVE ( )  B_SPLINE_CURVE ( 2, ( #40063, #61805, #95106, #127016, #16853, #18230, #84281, #96507, #105278, #7371, #52319, #128476, #29148 ),
 .UNSPECIFIED., .F., .T. ) 
 B_SPLINE_CURVE_WITH_KNOTS ( ( 3, 2, 2, 2, 2, 2, 3 ),
 ( 0.8000000000000000444, 0.8027777777777778123, 0.8055555555555555802, 0.8083333333333333481, 0.8111111111111111160, 0.8138888888888888840, 0.8166666666666666519 ),
 .UNSPECIFIED. ) 
 CURVE ( )  GEOMETRIC_REPRESENTATION_ITEM ( )  RATIONAL_B_SPLINE_CURVE ( ( 1.000000000000000000, 0.9659258262890683122, 1.000000000000000000, 0.9659258262890683122, 1.000000000000000000, 0.9659258262890683122, 1.000000000000000000, 0.9659258262890683122, 1.000000000000000000, 0.9659258262890683122, 1.000000000000000000, 0.9659258262890683122, 1.000000000000000000 ) ) 
 REPRESENTATION_ITEM ( '' )  );
#16276 = CARTESIAN_POINT ( 'NONE',  ( 2.700255128608413990, -27.71228299555204089, 4.000000000000000000 ) ) ;
#16277 = APPLICATION_PROTOCOL_DEFINITION ( 'draft international standard', 'automotive_design', 1998, #104973 ) ;
#16278 = ORIENTED_EDGE ( 'NONE', *, *, #84434, .F. ) ;
#16279 = EDGE_CURVE ( 'NONE', #26178, #53860, #35452, .T. ) ;
#16280 = ADVANCED_FACE ( 'NONE', ( #66624 ), #34709, .T. ) ;
#16281 = ORIENTED_EDGE ( 'NONE', *, *, #24647, .T. ) ;
#16282 = CARTESIAN_POINT ( 'NONE',  ( 91.93293019189812298, 1.637169565754156508, 6.110000000000000320 ) ) ;
#16283 = ORIENTED_EDGE ( 'NONE', *, *, #75771, .F. ) ;
#16284 = EDGE_CURVE ( 'NONE', #43072, #93569, #122402, .T. ) ;
#16285 = DIRECTION ( 'NONE',  ( 1.000000000000000000, 0.000000000000000000, 0.000000000000000000 ) ) ;
#16286 = EDGE_CURVE ( 'NONE', #79882, #83402, #34931, .T. ) ;
#16287 = DIRECTION ( 'NONE',  ( 0.6830127018922181881, 0.6830127018922202975, -0.2588190451025214056 ) ) ;
#16288 = EDGE_CURVE ( 'NONE', #100222, #46561, #79686, .T. ) ;
#16289 = VECTOR ( 'NONE', #22327, 1000.000000000000000 ) ;
#16290 = LINE ( 'NONE', #132261, #116611 ) ;
#16291 = VERTEX_POINT ( 'NONE', #121680 ) ;
#16292 = CARTESIAN_POINT ( 'NONE',  ( -34.92500000000001137, -11.14387692260744522, 4.000000000000000000 ) ) ;
#16293 = ADVANCED_FACE ( 'NONE', ( #76808 ), #88384, .F. ) ;
#16294 = VECTOR ( 'NONE', #27021, 1000.000000000000114 ) ;
#16295 = CARTESIAN_POINT ( 'NONE',  ( -32.99451991528749062, 28.92564299267960948, 4.000000000000000000 ) ) ;
#16296 = EDGE_CURVE ( 'NONE', #29769, #13015, #12922, .T. ) ;
#16297 = DIRECTION ( 'NONE',  ( -0.3543493200069162685, -0.000000000000000000, -0.9351131265310288487 ) ) ;
#16299 = PLANE ( 'NONE',  #126060 ) ;
#16298 = LINE ( 'NONE', #8788, #1812 ) ;
#16300 = DIRECTION ( 'NONE',  ( -0.7071067811865486830, -0.7071067811865464625, 0.000000000000000000 ) ) ;
#16301 = CARTESIAN_POINT ( 'NONE',  ( 181.0474453055293793, -48.63825160239813528, -38.47250499286692360 ) ) ;
#16302 = CARTESIAN_POINT ( 'NONE',  ( -72.48921356237309510, -27.52281430457106026, 5.000000000000000000 ) ) ;
#16303 = ORIENTED_EDGE ( 'NONE', *, *, #117790, .F. ) ;
#16304 = VECTOR ( 'NONE', #51729, 1000.000000000000000 ) ;
#16305 = CARTESIAN_POINT ( 'NONE',  ( -29.99999999999979039, 10.21212019023806583, -2.019456568337728797 ) ) ;
#16306 = CARTESIAN_POINT ( 'NONE',  ( -26.67183060077628198, -3.740707523384238176, 4.000000000000000000 ) ) ;
#16307 = EDGE_CURVE ( 'NONE', #77389, #110325, #116353, .T. ) ;
#16308 = ORIENTED_EDGE ( 'NONE', *, *, #92951, .T. ) ;
#16309 = VERTEX_POINT ( 'NONE', #67346 ) ;
#16310 = EDGE_CURVE ( 'NONE', #74842, #81201, #619, .T. ) ;
#16311 = PRESENTATION_LAYER_ASSIGNMENT (  '', '', ( #41807 ) ) ;
#16312 = ORIENTED_EDGE ( 'NONE', *, *, #67751, .T. ) ;
#16313 = CARTESIAN_POINT ( 'NONE',  ( 47.68793019189809712, 6.110000000000002984, -1.637169565754156730 ) ) ;
#16314 = EDGE_LOOP ( 'NONE', ( #24492, #9539, #52690, #71646 ) ) ;
#16315 = EDGE_CURVE ( 'NONE', #109570, #80973, #101374, .T. ) ;
#16316 = VECTOR ( 'NONE', #106059, 1000.000000000000000 ) ;
#16317 = CARTESIAN_POINT ( 'NONE',  ( 14.48330628287044064, 6.094999999999991758, 1.633150327867687102 ) ) ;
#16318 = CARTESIAN_POINT ( 'NONE',  ( -10.92112245905905610, 8.781005371807186322, -29.73817149962091477 ) ) ;
#16319 = ORIENTED_EDGE ( 'NONE', *, *, #4330, .F. ) ;
#16320 = EDGE_LOOP ( 'NONE', ( #91059, #20724, #140019, #68855 ) ) ;
#16321 = VECTOR ( 'NONE', #126106, 1000.000000000000000 ) ;
#16322 = DIRECTION ( 'NONE',  ( 1.000000000000000000, 3.115803279706882722E-16, -0.000000000000000000 ) ) ;
#16324 = ORIENTED_EDGE ( 'NONE', *, *, #109642, .T. ) ;
#16323 = CARTESIAN_POINT ( 'NONE',  ( -5.510786437626906675, -27.52281430457051314, 5.000000000000000000 ) ) ;
#16325 = ORIENTED_EDGE ( 'NONE', *, *, #36160, .T. ) ;
#16326 = CARTESIAN_POINT ( 'NONE',  ( -34.92500000000001137, -12.28150956279563566, 4.759050581649337808 ) ) ;
#16327 = DIRECTION ( 'NONE',  ( 1.055184596092948005E-16, -1.000000000000000000, 0.000000000000000000 ) ) ;
#16328 = ORIENTED_EDGE ( 'NONE', *, *, #113493, .T. ) ;
#16329 = DIRECTION ( 'NONE',  ( -0.7071067811865487940, 0.7071067811865463515, 0.000000000000000000 ) ) ;
#16330 = ORIENTED_EDGE ( 'NONE', *, *, #12967, .T. ) ;
#16331 = ORIENTED_EDGE ( 'NONE', *, *, #67741, .F. ) ;
#16332 = EDGE_LOOP ( 'NONE', ( #52948, #128127, #71049, #118794 ) ) ;
#16333 = ORIENTED_EDGE ( 'NONE', *, *, #130466, .T. ) ;
#16334 = ADVANCED_FACE ( 'NONE', ( #54344 ), #37726, .T. ) ;
#16335 = DIRECTION ( 'NONE',  ( -0.7071067811865486830, -0.7071067811865464625, 0.000000000000000000 ) ) ;
#16336 = AXIS2_PLACEMENT_3D ( 'NONE', #5803, #59538, #115266 ) ;
#16337 = CARTESIAN_POINT ( 'NONE',  ( 80.99451991528748351, 28.92564299267994699, 4.000000000000000000 ) ) ;
#16338 = CARTESIAN_POINT ( 'NONE',  ( -25.39999999999996305, 3.061616997868383141E-16, -2.500000000000000000 ) ) ;
#16339 = CARTESIAN_POINT ( 'NONE',  ( 0.000000000000000000, 0.5999999999999987566, 3.054668707061621191 ) ) ;
#16340 = DIRECTION ( 'NONE',  ( -0.7071067811865486830, -0.7071067811865464625, 0.000000000000000000 ) ) ;
#16341 = ORIENTED_EDGE ( 'NONE', *, *, #7805, .F. ) ;
#16342 = AXIS2_PLACEMENT_3D ( 'NONE', #114651, #37851, #5159 ) ;
#16343 = VECTOR ( 'NONE', #8661, 1000.000000000000000 ) ;
#16344 = DIRECTION ( 'NONE',  ( 0.7071067811865487940, 0.7071067811865463515, 0.000000000000000000 ) ) ;
#16345 = EDGE_CURVE ( 'NONE', #58222, #92260, #142745, .T. ) ;
#16346 = CARTESIAN_POINT ( 'NONE',  ( 30.89540314143522437, 2.126176841940962348, 7.934999999999989839 ) ) ;
#16347 = CARTESIAN_POINT ( 'NONE',  ( 11.99999999999993072, 14.58746187583909837, 4.000000000000000000 ) ) ;
#16348 = CARTESIAN_POINT ( 'NONE',  ( 51.18398860626899705, 28.73617430169823095, 5.000000000000000000 ) ) ;
#16349 = DIRECTION ( 'NONE',  ( 0.7071067811865487940, 0.7071067811865463515, 0.000000000000000000 ) ) ;
#16350 = EDGE_LOOP ( 'NONE', ( #70177, #64311, #116014, #69493 ) ) ;
#16351 = ORIENTED_EDGE ( 'NONE', *, *, #75961, .F. ) ;
#16352 = EDGE_CURVE ( 'NONE', #35346, #125640, #94590, .T. ) ;
#16353 = EDGE_LOOP ( 'NONE', ( #98324, #81762, #90608, #67492, #58893 ) ) ;
#16354 = DIRECTION ( 'NONE',  ( 0.7071067811865487940, -0.7071067811865463515, 0.000000000000000000 ) ) ;
#16355 = CARTESIAN_POINT ( 'NONE',  ( -39.48921356237310221, -27.52281430457082934, 5.000000000000000000 ) ) ;
#16356 = CARTESIAN_POINT ( 'NONE',  ( 29.99999999999979039, -9.033600742197645417, 5.000000000000000000 ) ) ;
#16357 = DIRECTION ( 'NONE',  ( 1.000000000000000000, 0.000000000000000000, 0.000000000000000000 ) ) ;
#16358 = AXIS2_PLACEMENT_3D ( 'NONE', #27626, #46032, #123602 ) ;
#16359 = DIRECTION ( 'NONE',  ( 0.7071067811865487940, 0.7071067811865463515, 0.000000000000000000 ) ) ;
#16360 = CARTESIAN_POINT ( 'NONE',  ( 74.57876352523145158, -7.482591942790327058E-16, 6.109999999999999432 ) ) ;
#16361 = CIRCLE ( 'NONE', #48802, 2.500000000000000444 ) ;
#16362 = VECTOR ( 'NONE', #31815, 1000.000000000000000 ) ;
#16363 = DIRECTION ( 'NONE',  ( 0.000000000000000000, 0.000000000000000000, 1.000000000000000000 ) ) ;
#16364 = DIRECTION ( 'NONE',  ( -0.7071067811865487940, 0.7071067811865463515, -0.000000000000000000 ) ) ;
#16365 = EDGE_CURVE ( 'NONE', #10400, #29217, #72193, .T. ) ;
#16366 = FACE_OUTER_BOUND ( 'NONE', #105724, .T. ) ;
#16367 = CARTESIAN_POINT ( 'NONE',  ( -17.00492477221184018, -5.240707523384225297, 12.38332538355500034 ) ) ;
#16368 = VERTEX_POINT ( 'NONE', #73579 ) ;
#16369 = VECTOR ( 'NONE', #106758, 1000.000000000000227 ) ;
#16370 = COLOUR_RGB ( '', 0.31764706, 0.68627451, 0.89019608) ;
#16371 = VECTOR ( 'NONE', #32277, 1000.000000000000000 ) ;
#16373 = CARTESIAN_POINT ( 'NONE',  ( 17.54957349249705700, -3.269999999999996909, -36.39086428169088094 ) ) ;
#16372 = VECTOR ( 'NONE', #98646, 1000.000000000000000 ) ;
#16374 = ORIENTED_EDGE ( 'NONE', *, *, #142804, .F. ) ;
#16375 = AXIS2_PLACEMENT_3D ( 'NONE', #83045, #8296, #85889 ) ;
#16376 = CARTESIAN_POINT ( 'NONE',  ( 9.208651418775088970, 0.000000000000000000, 2.500000000000000444 ) ) ;
#16378 = ORIENTED_EDGE ( 'NONE', *, *, #53551, .F. ) ;
#16377 = LINE ( 'NONE', #5507, #95035 ) ;
#16379 = EDGE_CURVE ( 'NONE', #70361, #54903, #100221, .T. ) ;
#16380 = FACE_OUTER_BOUND ( 'NONE', #27704, .T. ) ;
#16381 = DIRECTION ( 'NONE',  ( 0.000000000000000000, -1.000000000000000000, 0.000000000000000000 ) ) ;
#16382 = ORIENTED_EDGE ( 'NONE', *, *, #50180, .F. ) ;
#16383 = DIRECTION ( 'NONE',  ( -0.7071067811865487940, 0.7071067811865463515, -0.000000000000000000 ) ) ;
#16384 = ORIENTED_EDGE ( 'NONE', *, *, #113382, .F. ) ;
#16385 = PLANE ( 'NONE',  #139381 ) ;
#16386 = VECTOR ( 'NONE', #138956, 1000.000000000000000 ) ;
#16387 = ORIENTED_EDGE ( 'NONE', *, *, #133719, .F. ) ;
#16388 = FACE_OUTER_BOUND ( 'NONE', #57684, .T. ) ;
#16389 = CARTESIAN_POINT ( 'NONE',  ( 93.26669371712957002, -7.949999999999999289, 2.130196079827424427 ) ) ;
#16390 = CARTESIAN_POINT ( 'NONE',  ( 72.16666666666665719, 6.884901960086285300, 3.975000000000003642 ) ) ;
#16391 = VERTEX_POINT ( 'NONE', #84473 ) ;
#16392 = CIRCLE ( 'NONE', #100060, 2.500000000000000888 ) ;
#16393 = CARTESIAN_POINT ( 'NONE',  ( 19.49999999999986500, -8.568876922607721269, 4.000000000000000000 ) ) ;
#16394 = CARTESIAN_POINT ( 'NONE',  ( -34.92500000000001137, 3.207916084809872448, -2.206283991393058752 ) ) ;
#16395 = CARTESIAN_POINT ( 'NONE',  ( 22.31249999999999645, -4.461849672132299993, -4.461849672132299105 ) ) ;
#16397 = VECTOR ( 'NONE', #91135, 1000.000000000000000 ) ;
#16396 = DIRECTION ( 'NONE',  ( 0.000000000000000000, 1.000000000000000000, 0.000000000000000000 ) ) ;
#16398 = CARTESIAN_POINT ( 'NONE',  ( 0.000000000000000000, 0.000000000000000000, 6.350000000000004086 ) ) ;
#16399 = VERTEX_POINT ( 'NONE', #128666 ) ;
#16400 = AXIS2_PLACEMENT_3D ( 'NONE', #85654, #95828, #130636 ) ;
#16401 = CARTESIAN_POINT ( 'NONE',  ( -39.18398860626899705, 28.73617430169814568, 5.000000000000000000 ) ) ;
#16402 = VERTEX_POINT ( 'NONE', #61322 ) ;
#16403 = VECTOR ( 'NONE', #13227, 1000.000000000000000 ) ;
#16404 = EDGE_CURVE ( 'NONE', #58311, #18399, #17729, .T. ) ;
#16405 = CARTESIAN_POINT ( 'NONE',  ( 81.81293019189810423, -1.637169565754159617, -6.110000000000001208 ) ) ;
#16406 = VECTOR ( 'NONE', #142752, 1000.000000000000000 ) ;
#16407 = LINE ( 'NONE', #115703, #142629 ) ;
#16408 = CARTESIAN_POINT ( 'NONE',  ( 12.83652871126541939, 15.75929247661555976, 9.299976744542947316 ) ) ;
#16409 = DIRECTION ( 'NONE',  ( 0.7071067811865486830, -0.7071067811865464625, -0.000000000000000000 ) ) ;
#16410 = ORIENTED_EDGE ( 'NONE', *, *, #19301, .F. ) ;
#16411 = AXIS2_PLACEMENT_3D ( 'NONE', #45857, #11021, #111808 ) ;
#16412 = DIRECTION ( 'NONE',  ( 0.000000000000000000, 0.000000000000000000, 1.000000000000000000 ) ) ;
#16413 = CARTESIAN_POINT ( 'NONE',  ( 6.852250093007166143, 4.584330080086930965E-16, 0.000000000000000000 ) ) ;
#16414 = LINE ( 'NONE', #107013, #122592 ) ;
#16415 = AXIS2_PLACEMENT_3D ( 'NONE', #130721, #65468, #31385 ) ;
#16416 = EDGE_CURVE ( 'NONE', #124216, #107217, #29336, .T. ) ;
#16417 = LINE ( 'NONE', #59969, #105026 ) ;
#16419 = ORIENTED_EDGE ( 'NONE', *, *, #97526, .T. ) ;
#16418 = DIRECTION ( 'NONE',  ( 0.3543493200069162685, -0.000000000000000000, -0.9351131265310288487 ) ) ;
#16420 = DIRECTION ( 'NONE',  ( -0.7071067811865487940, 0.7071067811865463515, 0.000000000000000000 ) ) ;
#16421 = CARTESIAN_POINT ( 'NONE',  ( 11.20710678118646797, -11.24070752338417378, 5.000000000000000000 ) ) ;
#16422 =( NAMED_UNIT ( * ) PLANE_ANGLE_UNIT ( ) SI_UNIT ( $, .RADIAN. ) );
#16423 = DIRECTION ( 'NONE',  ( 0.000000000000000000, 0.000000000000000000, 1.000000000000000000 ) ) ;
#16424 = EDGE_LOOP ( 'NONE', ( #16535, #125986, #125436, #14880 ) ) ;
#16425 = ORIENTED_EDGE ( 'NONE', *, *, #54035, .T. ) ;
#16426 = VERTEX_POINT ( 'NONE', #116363 ) ;
#16427 = CARTESIAN_POINT ( 'NONE',  ( 73.20876352523143282, -7.482591942790329030E-16, 6.110000000000001208 ) ) ;
#16428 = ORIENTED_EDGE ( 'NONE', *, *, #41196, .T. ) ;
#16429 = CARTESIAN_POINT ( 'NONE',  ( -6.183988606268994381, 28.73617430169791476, 5.000000000000000000 ) ) ;
#16430 = CARTESIAN_POINT ( 'NONE',  ( -23.89661266223020419, -0.3091507863911187037, 4.000000000000000000 ) ) ;
#16431 = AXIS2_PLACEMENT_3D ( 'NONE', #107719, #77286, #19992 ) ;
#16432 = CARTESIAN_POINT ( 'NONE',  ( 15.98840764549667703, 9.139736423841732040E-16, 0.000000000000000000 ) ) ;
#16433 = CARTESIAN_POINT ( 'NONE',  ( 5.510786437626906675, -27.52281430457051314, 5.000000000000000000 ) ) ;
#16434 = ORIENTED_EDGE ( 'NONE', *, *, #18342, .T. ) ;
#16435 = VECTOR ( 'NONE', #19420, 999.9999999999998863 ) ;
#16436 = EDGE_CURVE ( 'NONE', #29394, #36181, #117749, .T. ) ;
#16437 = FACE_OUTER_BOUND ( 'NONE', #51919, .T. ) ;
#16438 = CARTESIAN_POINT ( 'NONE',  ( -10.49999999999991829, 13.56627193232213813, -10.57019076586071193 ) ) ;
#16439 = ORIENTED_EDGE ( 'NONE', *, *, #51908, .F. ) ;
#16440 = DIRECTION ( 'NONE',  ( -0.7071067811865487940, 0.7071067811865463515, 0.000000000000000000 ) ) ;
#16441 = CARTESIAN_POINT ( 'NONE',  ( -11.67183060077638146, -9.740707523384180888, 4.000000000000000000 ) ) ;
#16442 = PLANE ( 'NONE',  #5262 ) ;
#16443 = VECTOR ( 'NONE', #129410, 999.9999999999998863 ) ;
#16444 = ORIENTED_EDGE ( 'NONE', *, *, #90558, .T. ) ;
#16445 = ORIENTED_EDGE ( 'NONE', *, *, #16234, .T. ) ;
#16446 = DIRECTION ( 'NONE',  ( 0.7071067811865487940, 0.7071067811865463515, -0.000000000000000000 ) ) ;
#16447 = DIRECTION ( 'NONE',  ( 0.000000000000000000, 1.000000000000000000, 0.000000000000000000 ) ) ;
#16448 = DIRECTION ( 'NONE',  ( 0.7071067811865487940, 0.7071067811865463515, 0.000000000000000000 ) ) ;
#16449 = CARTESIAN_POINT ( 'NONE',  ( 25.40000000000000568, -6.022532542321925142, -4.245577695859290124 ) ) ;
#16450 = PRESENTATION_STYLE_ASSIGNMENT (( #83175 ) ) ;
#16451 = VECTOR ( 'NONE', #39087, 999.9999999999998863 ) ;
#16452 = CARTESIAN_POINT ( 'NONE',  ( -66.48921356237309510, -27.52281430457101763, 5.000000000000000000 ) ) ;
#16453 = CARTESIAN_POINT ( 'NONE',  ( 25.22959685856476142, -6.110000000000000320, -1.637169565754161393 ) ) ;
#16454 = SURFACE_SIDE_STYLE ('',( #60011 ) ) ;
#16455 = ORIENTED_EDGE ( 'NONE', *, *, #73788, .T. ) ;
#16456 = ADVANCED_FACE ( 'NONE', ( #60596 ), #50403, .F. ) ;
#16457 = VERTEX_POINT ( 'NONE', #96024 ) ;
#16458 = ORIENTED_EDGE ( 'NONE', *, *, #42892, .F. ) ;
#16459 = ADVANCED_FACE ( 'NONE', ( #106898 ), #104768, .F. ) ;
#16460 = ORIENTED_EDGE ( 'NONE', *, *, #120562, .T. ) ;
#16461 = EDGE_CURVE ( 'NONE', #60720, #13220, #82323, .T. ) ;
#16462 = VECTOR ( 'NONE', #68989, 1000.000000000000000 ) ;
#16463 = ADVANCED_FACE ( 'NONE', ( #138842 ), #106163, .F. ) ;
#16464 = DIRECTION ( 'NONE',  ( 0.3543493200069162685, -0.000000000000000000, -0.9351131265310288487 ) ) ;
#16465 = VECTOR ( 'NONE', #96181, 1000.000000000000000 ) ;
#16466 = VECTOR ( 'NONE', #25206, 1000.000000000000227 ) ;
#16467 = EDGE_LOOP ( 'NONE', ( #22153, #109919, #26630, #42364 ) ) ;
#16468 = DIRECTION ( 'NONE',  ( 0.000000000000000000, 0.000000000000000000, 1.000000000000000000 ) ) ;
#16469 = DIRECTION ( 'NONE',  ( -1.000000000000000000, -1.224606353822377258E-16, -0.000000000000000000 ) ) ;
#16470 = FACE_OUTER_BOUND ( 'NONE', #70218, .T. ) ;
#16471 = CARTESIAN_POINT ( 'NONE',  ( -16.49999999999988987, -5.568876922607749691, 4.000000000000000000 ) ) ;
#16472 = VECTOR ( 'NONE', #137654, 1000.000000000000000 ) ;
#16473 = VECTOR ( 'NONE', #139489, 1000.000000000000000 ) ;
#16474 = AXIS2_PLACEMENT_3D ( 'NONE', #59412, #103571, #94124 ) ;
#16475 = VECTOR ( 'NONE', #10037, 1000.000000000000000 ) ;
#16476 = LINE ( 'NONE', #50561, #21300 ) ;
#16477 = EDGE_LOOP ( 'NONE', ( #64431, #31443, #28427, #24586 ) ) ;
#16478 = TOROIDAL_SURFACE ( 'NONE', #11829, 6.000000000000000000, 3.000000000000000000 ) ;
#16479 = PLANE ( 'NONE',  #109640 ) ;
#16480 = DIRECTION ( 'NONE',  ( -1.000000000000000000, 2.840831291283848700E-14, 0.000000000000000000 ) ) ;
#16481 = ADVANCED_FACE ( 'NONE', ( #71441 ), #93886, .T. ) ;
#16482 = VERTEX_POINT ( 'NONE', #109033 ) ;
#16483 = DIRECTION ( 'NONE',  ( 0.6830127018922181881, 0.6830127018922202975, -0.2588190451025214056 ) ) ;
#16484 = ORIENTED_EDGE ( 'NONE', *, *, #140396, .T. ) ;
#16485 = EDGE_CURVE ( 'NONE', #69167, #61103, #41646, .T. ) ;
#16486 = EDGE_LOOP ( 'NONE', ( #88154, #43526, #74983, #9155 ) ) ;
#16487 = DIRECTION ( 'NONE',  ( 1.000000000000000000, 0.000000000000000000, 0.000000000000000000 ) ) ;
#16488 = VERTEX_POINT ( 'NONE', #76443 ) ;
#16489 = ORIENTED_EDGE ( 'NONE', *, *, #71975, .T. ) ;
#16490 = AXIS2_PLACEMENT_3D ( 'NONE', #46821, #1090, #132384 ) ;
#16491 = CARTESIAN_POINT ( 'NONE',  ( 69.85459685856476142, -1.637169565754161615, 6.110000000000000320 ) ) ;
#16492 = EDGE_LOOP ( 'NONE', ( #4459, #46061, #37091, #134956, #109823, #25489, #19262, #46200 ) ) ;
#16493 = ADVANCED_FACE ( 'NONE', ( #9721 ), #63213, .T. ) ;
#16494 = DIRECTION ( 'NONE',  ( -0.7071067811865486830, -0.7071067811865464625, 0.000000000000000000 ) ) ;
#16495 = CARTESIAN_POINT ( 'NONE',  ( 1.362461875839014791, 22.22500000000000142, 4.000000000000000000 ) ) ;
#16496 = PLANE ( 'NONE',  #10221 ) ;
#16497 = CARTESIAN_POINT ( 'NONE',  ( 112.7295968585647756, -6.110000000000000320, -1.637169565754161393 ) ) ;
#16498 = LINE ( 'NONE', #107090, #86559 ) ;
#16499 = AXIS2_PLACEMENT_3D ( 'NONE', #63761, #1138, #8589 ) ;
#16500 = LINE ( 'NONE', #85330, #14291 ) ;
#16501 =( NAMED_UNIT ( * ) SI_UNIT ( $, .STERADIAN. ) SOLID_ANGLE_UNIT ( ) );
#16502 = EDGE_CURVE ( 'NONE', #142939, #109568, #53991, .T. ) ;
#16503 = FACE_OUTER_BOUND ( 'NONE', #79379, .T. ) ;
#16504 = CARTESIAN_POINT ( 'NONE',  ( 0.4000000000000001887, 1.530808498934155086E-16, -1.249999999999969802 ) ) ;
#16505 = LINE ( 'NONE', #71641, #95342 ) ;
#16506 = VECTOR ( 'NONE', #128307, 1000.000000000000000 ) ;
#16507 = DIRECTION ( 'NONE',  ( 1.000000000000000000, 0.000000000000000000, 0.000000000000000000 ) ) ;
#16508 = VERTEX_POINT ( 'NONE', #130104 ) ;
#16509 = VECTOR ( 'NONE', #48384, 1000.000000000000000 ) ;
#16510 = PLANE ( 'NONE',  #124451 ) ;
#16511 = DIRECTION ( 'NONE',  ( 0.7071067811865487940, -0.7071067811865463515, 0.000000000000000000 ) ) ;
#16512 = ORIENTED_EDGE ( 'NONE', *, *, #143197, .F. ) ;
#16513 = AXIS2_PLACEMENT_3D ( 'NONE', #112798, #72022, #35283 ) ;
#16514 = ORIENTED_EDGE ( 'NONE', *, *, #97551, .T. ) ;
#16515 = EDGE_CURVE ( 'NONE', #114036, #35724, #143108, .T. ) ;
#16516 = CARTESIAN_POINT ( 'NONE',  ( 114.1208603837962414, -6.884901960086286188, 3.974999999999997424 ) ) ;
#16517 = VERTEX_POINT ( 'NONE', #119893 ) ;
#16518 = VECTOR ( 'NONE', #64386, 1000.000000000000000 ) ;
#16519 = DIRECTION ( 'NONE',  ( -0.7071067811865486830, 0.7071067811865464625, 0.000000000000000000 ) ) ;
#16520 = CARTESIAN_POINT ( 'NONE',  ( 113.1458333333333428, 2.130196079827451516, -7.949999999999988631 ) ) ;
#16521 = VECTOR ( 'NONE', #124810, 1000.000000000000000 ) ;
#16522 = CARTESIAN_POINT ( 'NONE',  ( 4.499999999999968914, -20.56887692260760048, 4.000000000000000000 ) ) ;
#16523 = LINE ( 'NONE', #4168, #94924 ) ;
#16524 = ORIENTED_EDGE ( 'NONE', *, *, #10811, .T. ) ;
#16525 = DIRECTION ( 'NONE',  ( 0.7071067811865486830, -0.7071067811865464625, -0.000000000000000000 ) ) ;
#16526 = ORIENTED_EDGE ( 'NONE', *, *, #89079, .T. ) ;
#16527 = EDGE_CURVE ( 'NONE', #86631, #27690, #8966, .T. ) ;
#16528 = CARTESIAN_POINT ( 'NONE',  ( 24.56706980810189123, 2.126176841940952134, -7.934999999999993392 ) ) ;
#16529 = CARTESIAN_POINT ( 'NONE',  ( 9.299744871391588674, -27.71228299555212971, 4.000000000000000000 ) ) ;
#16530 = CARTESIAN_POINT ( 'NONE',  ( -17.99451991528748351, 28.92564299267950645, 4.000000000000000000 ) ) ;
#16531 = CARTESIAN_POINT ( 'NONE',  ( -31.92499999999997584, -6.270000000000012896, -36.39086428169088094 ) ) ;
#16532 = VERTEX_POINT ( 'NONE', #98871 ) ;
#16533 = VERTEX_POINT ( 'NONE', #87308 ) ;
#16534 = VECTOR ( 'NONE', #33771, 1000.000000000000000 ) ;
#16535 = ORIENTED_EDGE ( 'NONE', *, *, #61205, .F. ) ;
#16536 = DIRECTION ( 'NONE',  ( -0.000000000000000000, -0.3543493200069152693, 0.9351131265310292928 ) ) ;
#16537 = CARTESIAN_POINT ( 'NONE',  ( 0.04658813629544733548, 14.25929247661557753, 18.84478104361328121 ) ) ;
#16538 = DIRECTION ( 'NONE',  ( -0.7071067811865486830, -0.7071067811865464625, 0.000000000000000000 ) ) ;
#16539 = VECTOR ( 'NONE', #43512, 1000.000000000000000 ) ;
#16540 = FILL_AREA_STYLE ('',( #138348 ) ) ;
#16541 = DIRECTION ( 'NONE',  ( 0.7071067811865487940, 0.7071067811865463515, -0.000000000000000000 ) ) ;
#16542 = FACE_OUTER_BOUND ( 'NONE', #40123, .T. ) ;
#16543 = CARTESIAN_POINT ( 'NONE',  ( -21.70701326429289324, -21.74070752338406010, 4.999753212805221558 ) ) ;
#16544 = EDGE_CURVE ( 'NONE', #35109, #118679, #32957, .T. ) ;
#16545 = DIRECTION ( 'NONE',  ( -0.6830127018922180770, -0.6830127018922204085, -0.2588190451025213501 ) ) ;
#16547 = VECTOR ( 'NONE', #126694, 999.9999999999998863 ) ;
#16546 = CARTESIAN_POINT ( 'NONE',  ( 36.18398860626899705, 28.73617430169812437, 5.000000000000000000 ) ) ;
#16548 = ORIENTED_EDGE ( 'NONE', *, *, #27767, .F. ) ;
#16549 = DIRECTION ( 'NONE',  ( -0.7071067811865487940, 0.7071067811865463515, 0.000000000000000000 ) ) ;
#16550 = AXIS2_PLACEMENT_3D ( 'NONE', #42806, #130525, #86996 ) ;
#16551 = CARTESIAN_POINT ( 'NONE',  ( 31.49999999999979039, -20.56887692260760758, 4.000000000000000000 ) ) ;
#16552 = ORIENTED_EDGE ( 'NONE', *, *, #137954, .T. ) ;
#16553 =( BOUNDED_CURVE ( )  B_SPLINE_CURVE ( 3, ( #107045, #6256, #29475, #73711 ),
 .UNSPECIFIED., .F., .T. ) 
 B_SPLINE_CURVE_WITH_KNOTS ( ( 4, 4 ),
 ( 5.390251506879594423, 5.422326034329065791 ),
 .UNSPECIFIED. ) 
 CURVE ( )  GEOMETRIC_REPRESENTATION_ITEM ( )  RATIONAL_B_SPLINE_CURVE ( ( 1.000000000000000000, 0.9999142705615216009, 0.9999142705615216009, 1.000000000000000000 ) ) 
 REPRESENTATION_ITEM ( '' )  );
#16554 = PLANE ( 'NONE',  #64572 ) ;
#16556 = ORIENTED_EDGE ( 'NONE', *, *, #127960, .F. ) ;
#16555 = CARTESIAN_POINT ( 'NONE',  ( 4.499999999999979572, 0.05218569542916884352, 5.000000000000000000 ) ) ;
#16557 = EDGE_CURVE ( 'NONE', #79734, #2427, #133993, .T. ) ;
#16558 = CARTESIAN_POINT ( 'NONE',  ( 9.299744871391588674, -27.71228299555212971, 4.000000000000000000 ) ) ;
#16559 = CARTESIAN_POINT ( 'NONE',  ( 28.98012225071434855, -17.24070752338409562, 20.23474786156475957 ) ) ;
#16561 = VERTEX_POINT ( 'NONE', #99575 ) ;
#16560 = VECTOR ( 'NONE', #18152, 1000.000000000000000 ) ;
#16562 = FACE_OUTER_BOUND ( 'NONE', #112810, .T. ) ;
#16563 = ORIENTED_EDGE ( 'NONE', *, *, #97270, .F. ) ;
#16564 = DIRECTION ( 'NONE',  ( 0.6830127018922180770, -0.6830127018922204085, -0.2588190451025213501 ) ) ;
#16565 = CARTESIAN_POINT ( 'NONE',  ( -7.968364840778035862, 2.259292476615690770, 13.77329220150635614 ) ) ;
#16566 = CARTESIAN_POINT ( 'NONE',  ( 119.6625270504628986, 7.949999999999998401, 1.460391307983218338E-15 ) ) ;
#16567 = CARTESIAN_POINT ( 'NONE',  ( -2.816011393730999401, 28.73617430169785436, 5.000000000000000000 ) ) ;
#16568 = CARTESIAN_POINT ( 'NONE',  ( -34.06996025486387936, -0.7407075233842770334, 13.87443053587618813 ) ) ;
#16570 = ADVANCED_FACE ( 'NONE', ( #77174 ), #130836, .T. ) ;
#16569 = CARTESIAN_POINT ( 'NONE',  ( 72.18398860626899705, 28.73617430169837661, 5.000000000000000000 ) ) ;
#16571 = PLANE ( 'NONE',  #142066 ) ;
#16572 = LINE ( 'NONE', #4953, #69254 ) ;
#16573 = CARTESIAN_POINT ( 'NONE',  ( 5.421010862427522170E-17, 0.000000000000000000, 6.094999999999989981 ) ) ;
#16574 = CARTESIAN_POINT ( 'NONE',  ( 5.228736474768553855, 5.808823158059031044, -5.808823158059037262 ) ) ;
#16575 = CARTESIAN_POINT ( 'NONE',  ( 42.48921356237308800, -27.52281430457085065, 5.000000000000000000 ) ) ;
#16576 = VECTOR ( 'NONE', #58523, 999.9999999999998863 ) ;
#16577 = CIRCLE ( 'NONE', #97606, 4.000000000000000000 ) ;
#16578 = FACE_OUTER_BOUND ( 'NONE', #70948, .T. ) ;
#16579 = FACE_OUTER_BOUND ( 'NONE', #140655, .T. ) ;
#16580 = ORIENTED_EDGE ( 'NONE', *, *, #29567, .F. ) ;
#16581 = VERTEX_POINT ( 'NONE', #110451 ) ;
#16582 = AXIS2_PLACEMENT_3D ( 'NONE', #87847, #45105, #119729 ) ;
#16583 = CARTESIAN_POINT ( 'NONE',  ( 79.45833333333332860, 3.974999999999997424, 6.884901960086288852 ) ) ;
#16584 = AXIS2_PLACEMENT_3D ( 'NONE', #97594, #52669, #143255 ) ;
#16586 = ORIENTED_EDGE ( 'NONE', *, *, #76601, .T. ) ;
#16585 = CARTESIAN_POINT ( 'NONE',  ( 96.03752705046289861, -9.735942053221456900E-16, 7.949999999999998401 ) ) ;
#16587 = EDGE_LOOP ( 'NONE', ( #70812, #124823, #109180, #66812 ) ) ;
#16588 = ADVANCED_FACE ( 'NONE', ( #109763 ), #11125, .F. ) ;
#16589 = CARTESIAN_POINT ( 'NONE',  ( 11.29298673570687050, -21.74070752338406365, 4.999753212805220670 ) ) ;
#16590 = CARTESIAN_POINT ( 'NONE',  ( -66.48921356237309510, -27.52281430457101763, 5.000000000000000000 ) ) ;
#16591 = AXIS2_PLACEMENT_3D ( 'NONE', #19259, #64200, #27995 ) ;
#16592 = VECTOR ( 'NONE', #97731, 1000.000000000000000 ) ;
#16593 = CONICAL_SURFACE ( 'NONE', #100030, 2.055000000000000604, 0.9599310885968764806 ) ;
#16594 = MECHANICAL_DESIGN_GEOMETRIC_PRESENTATION_REPRESENTATION (  '', ( #55964 ), #74479 ) ;
#16595 = DIRECTION ( 'NONE',  ( 0.7071067811865487940, 0.7071067811865463515, 0.000000000000000000 ) ) ;
#16596 = VERTEX_POINT ( 'NONE', #55403 ) ;
#16597 = LINE ( 'NONE', #105044, #115743 ) ;
#16598 = VECTOR ( 'NONE', #118887, 1000.000000000000000 ) ;
#16599 = CARTESIAN_POINT ( 'NONE',  ( 15.48921356237309510, -27.52281430457066236, 5.000000000000000000 ) ) ;
#16600 = CARTESIAN_POINT ( 'NONE',  ( 19.49999999999986144, 9.127013188829479873, 4.802533355213541633 ) ) ;
#16601 = PLANE ( 'NONE',  #14194 ) ;
#16602 = EDGE_CURVE ( 'NONE', #62391, #100683, #97441, .T. ) ;
#16603 = ADVANCED_FACE ( 'NONE', ( #42397 ), #98185, .F. ) ;
#16604 = DIRECTION ( 'NONE',  ( 0.6830127018922180770, -0.6830127018922204085, -0.2588190451025213501 ) ) ;
#16605 = FACE_OUTER_BOUND ( 'NONE', #23660, .T. ) ;
#16606 = AXIS2_PLACEMENT_3D ( 'NONE', #16062, #135753, #4440 ) ;
#16607 = DIRECTION ( 'NONE',  ( 1.000000000000000000, 0.000000000000000000, 0.000000000000000000 ) ) ;
#16608 = DIRECTION ( 'NONE',  ( -3.115803279706882722E-16, 1.000000000000000000, -0.000000000000000000 ) ) ;
#16609 = DIRECTION ( 'NONE',  ( 0.6830127018922180770, -0.6830127018922204085, -0.2588190451025213501 ) ) ;
#16610 = DIRECTION ( 'NONE',  ( 0.7071067811865487940, -0.7071067811865463515, 0.000000000000000000 ) ) ;
#16611 = DIRECTION ( 'NONE',  ( -0.7071067811865486830, 0.7071067811865464625, 0.000000000000000000 ) ) ;
#16612 = DIRECTION ( 'NONE',  ( -0.6830127018922180770, -0.6830127018922204085, -0.2588190451025213501 ) ) ;
#16613 = VERTEX_POINT ( 'NONE', #88751 ) ;
#16614 = EDGE_LOOP ( 'NONE', ( #26368, #107621, #60034, #13121 ) ) ;
#16615 = CARTESIAN_POINT ( 'NONE',  ( 111.1254301918981042, 5.291415217122919401, 3.055000000000002824 ) ) ;
#16616 = ORIENTED_EDGE ( 'NONE', *, *, #128025, .T. ) ;
#16617 =( LENGTH_UNIT ( ) NAMED_UNIT ( * ) SI_UNIT ( .MILLI., .METRE. ) );
#16618 = LINE ( 'NONE', #118045, #29247 ) ;
#16619 = ORIENTED_EDGE ( 'NONE', *, *, #114876, .F. ) ;
#16620 = EDGE_CURVE ( 'NONE', #33358, #61647, #142414, .T. ) ;
#16621 = DIRECTION ( 'NONE',  ( 0.7071067811865487940, 0.7071067811865463515, 0.000000000000000000 ) ) ;
#16622 = FACE_OUTER_BOUND ( 'NONE', #125276, .T. ) ;
#16623 = AXIS2_PLACEMENT_3D ( 'NONE', #28820, #74480, #15731 ) ;
#16624 = VECTOR ( 'NONE', #7545, 1000.000000000000000 ) ;
#16625 = CARTESIAN_POINT ( 'NONE',  ( 108.2662635252314374, 4.472830434245839371, -4.472830434245838482 ) ) ;
#16626 = VERTEX_POINT ( 'NONE', #118489 ) ;
#16627 = AXIS2_PLACEMENT_3D ( 'NONE', #57948, #49198, #137623 ) ;
#16628 = ORIENTED_EDGE ( 'NONE', *, *, #133031, .T. ) ;
#16629 = CARTESIAN_POINT ( 'NONE',  ( 8.218373117074998291, 21.74787736706806385, 4.999607392498049308 ) ) ;
#16630 = LINE ( 'NONE', #118054, #16777 ) ;
#16631 = AXIS2_PLACEMENT_3D ( 'NONE', #28753, #60699, #61416 ) ;
#16632 = CARTESIAN_POINT ( 'NONE',  ( -2.816011393730999401, 28.73617430169785436, 5.000000000000000000 ) ) ;
#16633 = CARTESIAN_POINT ( 'NONE',  ( 15.83159235450332147, 9.902892378096218942E-16, 0.000000000000000000 ) ) ;
#16634 = VERTEX_POINT ( 'NONE', #19189 ) ;
#16635 = ORIENTED_EDGE ( 'NONE', *, *, #14998, .T. ) ;
#16636 = ORIENTED_EDGE ( 'NONE', *, *, #103835, .T. ) ;
#16637 = LINE ( 'NONE', #5745, #90824 ) ;
#16638 = DIRECTION ( 'NONE',  ( 0.7071067811865487940, 0.7071067811865463515, 0.000000000000000000 ) ) ;
#16639 = CARTESIAN_POINT ( 'NONE',  ( 10.56706980810188767, 2.126176841940952134, -7.934999999999992504 ) ) ;
#16640 = VECTOR ( 'NONE', #127211, 1000.000000000000000 ) ;
#16641 = PLANE ( 'NONE',  #71082 ) ;
#16642 = EDGE_CURVE ( 'NONE', #140124, #100866, #19884, .T. ) ;
#16643 = DIRECTION ( 'NONE',  ( 1.000000000000000000, 0.000000000000000000, 0.000000000000000000 ) ) ;
#16644 = EDGE_CURVE ( 'NONE', #91814, #94048, #86607, .T. ) ;
#16645 = PRESENTATION_STYLE_ASSIGNMENT (( #15895 ) ) ;
#16646 = ORIENTED_EDGE ( 'NONE', *, *, #123562, .F. ) ;
#16647 = VERTEX_POINT ( 'NONE', #46715 ) ;
#16648 = EDGE_CURVE ( 'NONE', #61464, #107040, #101743, .T. ) ;
#16649 = DIRECTION ( 'NONE',  ( -0.6830127018922181881, 0.6830127018922202975, -0.2588190451025214056 ) ) ;
#16650 = VERTEX_POINT ( 'NONE', #135125 ) ;
#16651 = ORIENTED_EDGE ( 'NONE', *, *, #72838, .T. ) ;
#16652 = VECTOR ( 'NONE', #10726, 1000.000000000000227 ) ;
#16653 = VECTOR ( 'NONE', #66534, 999.9999999999998863 ) ;
#16654 = EDGE_CURVE ( 'NONE', #38177, #80628, #47423, .T. ) ;
#16655 = ADVANCED_FACE ( 'NONE', ( #111924 ), #59013, .F. ) ;
#16656 = CARTESIAN_POINT ( 'NONE',  ( 113.3704301918981230, -3.055000000000001492, 5.291415217122917625 ) ) ;
#16657 = DIRECTION ( 'NONE',  ( 4.681814790819592407E-17, 0.3543493200069153248, 0.9351131265310292928 ) ) ;
#16658 = DIRECTION ( 'NONE',  ( -0.6830127018922181881, 0.6830127018922202975, -0.2588190451025214056 ) ) ;
#16659 = ORIENTED_EDGE ( 'NONE', *, *, #65767, .F. ) ;
#16660 = FACE_OUTER_BOUND ( 'NONE', #8044, .T. ) ;
#16661 = DIRECTION ( 'NONE',  ( -0.000000000000000000, 0.3543493200069153248, 0.9351131265310292928 ) ) ;
#16662 = VECTOR ( 'NONE', #53403, 1000.000000000000000 ) ;
#16663 = CARTESIAN_POINT ( 'NONE',  ( -24.29974487139158867, -27.71228299555223273, 4.000000000000000000 ) ) ;
#16664 = CARTESIAN_POINT ( 'NONE',  ( 28.49999999999980815, 7.466399257802192935, 5.000000000000000000 ) ) ;
#16665 = ORIENTED_EDGE ( 'NONE', *, *, #99609, .F. ) ;
#16666 = CARTESIAN_POINT ( 'NONE',  ( -19.83957586139685247, 9.091547215995101183, 4.000000000000000000 ) ) ;
#16667 = FACE_BOUND ( 'NONE', #137643, .T. ) ;
#16668 = EDGE_CURVE ( 'NONE', #109897, #31681, #80730, .T. ) ;
#16669 = EDGE_LOOP ( 'NONE', ( #42187, #66573, #110058, #127474 ) ) ;
#16670 = CARTESIAN_POINT ( 'NONE',  ( 15.04658813629535707, 14.25929247661557042, 18.84478104361324213 ) ) ;
#16671 = LINE ( 'NONE', #62350, #98993 ) ;
#16672 = ADVANCED_FACE ( 'NONE', ( #114045 ), #124922, .F. ) ;
#16673 = ORIENTED_EDGE ( 'NONE', *, *, #72761, .T. ) ;
#16674 = PLANE ( 'NONE',  #52731 ) ;
#16675 = ORIENTED_EDGE ( 'NONE', *, *, #125511, .T. ) ;
#16676 = ORIENTED_EDGE ( 'NONE', *, *, #76213, .T. ) ;
#16677 = ORIENTED_EDGE ( 'NONE', *, *, #92421, .F. ) ;
#16678 = CARTESIAN_POINT ( 'NONE',  ( 33.59959685856478018, -6.109999999999997655, -1.637169565754160283 ) ) ;
#16679 = VERTEX_POINT ( 'NONE', #68445 ) ;
#16680 =( BOUNDED_CURVE ( )  B_SPLINE_CURVE ( 3, ( #70833, #125917, #114981, #126594 ),
 .UNSPECIFIED., .F., .T. ) 
 B_SPLINE_CURVE_WITH_KNOTS ( ( 4, 4 ),
 ( 5.920967161967927161, 7.341195215986594746 ),
 .UNSPECIFIED. ) 
 CURVE ( )  GEOMETRIC_REPRESENTATION_ITEM ( )  RATIONAL_B_SPLINE_CURVE ( ( 1.000000000000000000, 0.8388583629366707095, 0.8388583629366707095, 1.000000000000000000 ) ) 
 REPRESENTATION_ITEM ( '' )  );
#16681 = EDGE_CURVE ( 'NONE', #106218, #24833, #13997, .T. ) ;
#16682 = DIRECTION ( 'NONE',  ( -0.000000000000000000, -0.3543493200069152693, 0.9351131265310292928 ) ) ;
#16683 = DIRECTION ( 'NONE',  ( 1.000000000000000000, 0.000000000000000000, 0.000000000000000000 ) ) ;
#16684 = DIRECTION ( 'NONE',  ( -0.7071067811865487940, 0.7071067811865463515, -0.000000000000000000 ) ) ;
#16685 = DIRECTION ( 'NONE',  ( 1.000000000000000000, 0.000000000000000000, 0.000000000000000000 ) ) ;
#16686 = CARTESIAN_POINT ( 'NONE',  ( 12.82439460721831104, 2.055000000000001048, 0.000000000000000000 ) ) ;
#16688 = ADVANCED_FACE ( 'NONE', ( #77859 ), #90896, .F. ) ;
#16687 = AXIS2_PLACEMENT_3D ( 'NONE', #143160, #109822, #89494 ) ;
#16689 = AXIS2_PLACEMENT_3D ( 'NONE', #77212, #67781, #56192 ) ;
#16690 = AXIS2_PLACEMENT_3D ( 'NONE', #43405, #120203, #20913 ) ;
#16691 = LINE ( 'NONE', #27550, #53806 ) ;
#16692 = VECTOR ( 'NONE', #131726, 1000.000000000000227 ) ;
#16693 = VECTOR ( 'NONE', #38613, 1000.000000000000000 ) ;
#16694 = DIRECTION ( 'NONE',  ( -0.7071067811865486830, -0.7071067811865464625, 0.000000000000000000 ) ) ;
#16695 = CARTESIAN_POINT ( 'NONE',  ( 9.994118527364397764, -2.500000000000000000, 3.061616997868383634E-16 ) ) ;
#16696 = LINE ( 'NONE', #5072, #52923 ) ;
#16697 = CARTESIAN_POINT ( 'NONE',  ( -24.48921356237309510, -27.52281430457072631, 5.000000000000000000 ) ) ;
#16698 = ORIENTED_EDGE ( 'NONE', *, *, #38683, .T. ) ;
#16699 = ORIENTED_EDGE ( 'NONE', *, *, #92350, .T. ) ;
#16700 = VECTOR ( 'NONE', #24449, 1000.000000000000000 ) ;
#16702 = VERTEX_POINT ( 'NONE', #66988 ) ;
#16701 = EDGE_CURVE ( 'NONE', #52797, #33791, #133670, .T. ) ;
#16703 = CIRCLE ( 'NONE', #60842, 2.500000000000000444 ) ;
#16704 = VERTEX_POINT ( 'NONE', #91586 ) ;
#16705 = DIRECTION ( 'NONE',  ( -0.6830127018922181881, 0.6830127018922202975, -0.2588190451025214056 ) ) ;
#16706 = ORIENTED_EDGE ( 'NONE', *, *, #139666, .F. ) ;
#16707 = EDGE_LOOP ( 'NONE', ( #104002, #45864, #837, #115052 ) ) ;
#16708 = CARTESIAN_POINT ( 'NONE',  ( -34.42500000000001137, 21.72500000000000142, 5.000000000000000000 ) ) ;
#16709 = CARTESIAN_POINT ( 'NONE',  ( 25.17183060077629619, 9.759292476615618384, 4.000000000000000000 ) ) ;
#16710 = DIRECTION ( 'NONE',  ( 0.6830127018922180770, -0.6830127018922204085, -0.2588190451025213501 ) ) ;
#16711 = EDGE_CURVE ( 'NONE', #105009, #81280, #122048, .T. ) ;
#16712 = ORIENTED_EDGE ( 'NONE', *, *, #93579, .F. ) ;
#16713 = EDGE_CURVE ( 'NONE', #50240, #43657, #14735, .T. ) ;
#16714 = CARTESIAN_POINT ( 'NONE',  ( 0.000000000000000000, 0.000000000000000000, 5.000000000000000000 ) ) ;
#16715 = ORIENTED_EDGE ( 'NONE', *, *, #81037, .F. ) ;
#16716 = PLANE ( 'NONE',  #141621 ) ;
#16717 = EDGE_CURVE ( 'NONE', #71266, #102417, #124212, .T. ) ;
#16718 = CARTESIAN_POINT ( 'NONE',  ( 32.58790314143522693, 6.871911579029515771, 3.967499999999989146 ) ) ;
#16719 = ORIENTED_EDGE ( 'NONE', *, *, #134644, .T. ) ;
#16721 = CARTESIAN_POINT ( 'NONE',  ( -51.48921356237309510, -27.52281430457091460, 5.000000000000000000 ) ) ;
#16720 = CARTESIAN_POINT ( 'NONE',  ( 103.3079301918981088, -6.109999999999999432, 1.637169565754158507 ) ) ;
#16722 = SURFACE_STYLE_FILL_AREA ( #39201 ) ;
#16723 = CARTESIAN_POINT ( 'NONE',  ( -9.792893218813382816, -11.24070752338416845, 5.000000000000000000 ) ) ;
#16724 = ORIENTED_EDGE ( 'NONE', *, *, #113199, .T. ) ;
#16725 = EDGE_LOOP ( 'NONE', ( #33648, #107515, #51869, #106268 ) ) ;
#16726 = FACE_OUTER_BOUND ( 'NONE', #39668, .T. ) ;
#16727 = ORIENTED_EDGE ( 'NONE', *, *, #83958, .F. ) ;
#16728 = FILL_AREA_STYLE_COLOUR ( '', #111173 ) ;
#16729 = CARTESIAN_POINT ( 'NONE',  ( -17.99999999999987566, -10.77435723561697145, -9.972017380717186796 ) ) ;
#16730 = CARTESIAN_POINT ( 'NONE',  ( -60.18398860626900415, 28.73617430169829490, 5.000000000000000000 ) ) ;
#16731 = EDGE_CURVE ( 'NONE', #113815, #107142, #113316, .T. ) ;
#16732 = CARTESIAN_POINT ( 'NONE',  ( 20.20519093902540320, 2.500000000000000444, 0.000000000000000000 ) ) ;
#16733 = CARTESIAN_POINT ( 'NONE',  ( 183.6085471140778225, -52.10163751122234288, -40.43817685073710066 ) ) ;
#16734 = ORIENTED_EDGE ( 'NONE', *, *, #18210, .T. ) ;
#16735 = AXIS2_PLACEMENT_3D ( 'NONE', #107949, #73240, #119545 ) ;
#16736 = PLANE ( 'NONE',  #18227 ) ;
#16737 = VECTOR ( 'NONE', #30091, 1000.000000000000000 ) ;
#16738 = DIRECTION ( 'NONE',  ( -0.7071067811865486830, -0.7071067811865464625, 0.000000000000000000 ) ) ;
#16739 = DIRECTION ( 'NONE',  ( 0.3543493200069162685, -0.000000000000000000, -0.9351131265310288487 ) ) ;
#16740 = ORIENTED_EDGE ( 'NONE', *, *, #21739, .F. ) ;
#16741 = DIRECTION ( 'NONE',  ( -1.000000000000000000, -0.000000000000000000, -0.000000000000000000 ) ) ;
#16742 = AXIS2_PLACEMENT_3D ( 'NONE', #110208, #23949, #132736 ) ;
#16743 = CARTESIAN_POINT ( 'NONE',  ( 16.49999999999988987, 13.08746187583910370, 4.000000000000000000 ) ) ;
#16744 = VERTEX_POINT ( 'NONE', #89436 ) ;
#16746 = VERTEX_POINT ( 'NONE', #112623 ) ;
#16745 = PLANE ( 'NONE',  #2294 ) ;
#16747 = VERTEX_POINT ( 'NONE', #36491 ) ;
#16748 = CARTESIAN_POINT ( 'NONE',  ( -13.39050432165378446, 9.181379155046611729, -27.39219850300061765 ) ) ;
#16749 = DIRECTION ( 'NONE',  ( 0.3543493200069162685, -0.000000000000000000, -0.9351131265310288487 ) ) ;
#16750 = VECTOR ( 'NONE', #37757, 999.9999999999998863 ) ;
#16751 = VERTEX_POINT ( 'NONE', #13281 ) ;
#16752 = CARTESIAN_POINT ( 'NONE',  ( -4.499999999999968914, 7.466399257802187606, 5.000000000000000000 ) ) ;
#16753 =( BOUNDED_CURVE ( )  B_SPLINE_CURVE ( 3, ( #41531, #119792, #29942, #7473 ),
 .UNSPECIFIED., .F., .T. ) 
 B_SPLINE_CURVE_WITH_KNOTS ( ( 4, 4 ),
 ( 5.043186909253416950, 5.074607125596347856 ),
 .UNSPECIFIED. ) 
 CURVE ( )  GEOMETRIC_REPRESENTATION_ITEM ( )  RATIONAL_B_SPLINE_CURVE ( ( 1.000000000000000000, 0.9999177325257868620, 0.9999177325257868620, 1.000000000000000000 ) ) 
 REPRESENTATION_ITEM ( '' )  );
#16754 = CARTESIAN_POINT ( 'NONE',  ( 24.48921356237309510, -27.52281430457072631, 5.000000000000000000 ) ) ;
#16755 = DIRECTION ( 'NONE',  ( 0.7071067811865486830, 0.7071067811865463515, 0.000000000000000000 ) ) ;
#16756 = ORIENTED_EDGE ( 'NONE', *, *, #115986, .T. ) ;
#16757 = CARTESIAN_POINT ( 'NONE',  ( -2.999999999999971578, -4.447814304570786526, 5.000000000000000000 ) ) ;
#16758 = LINE ( 'NONE', #6544, #46621 ) ;
#16759 = EDGE_CURVE ( 'NONE', #110962, #28611, #42392, .T. ) ;
#16760 = DIRECTION ( 'NONE',  ( 0.3543493200069162685, -0.000000000000000000, -0.9351131265310288487 ) ) ;
#16761 = LINE ( 'NONE', #137123, #83759 ) ;
#16762 = AXIS2_PLACEMENT_3D ( 'NONE', #77139, #52483, #96667 ) ;
#16763 = DIRECTION ( 'NONE',  ( 0.7071067811865487940, 0.7071067811865463515, -0.000000000000000000 ) ) ;
#16764 = DIRECTION ( 'NONE',  ( -0.7071067811865486830, -0.7071067811865464625, 0.000000000000000000 ) ) ;
#16765 = CARTESIAN_POINT ( 'NONE',  ( 21.18398860626899349, 28.73617430169802134, 5.000000000000000000 ) ) ;
#16766 = LINE ( 'NONE', #115320, #106656 ) ;
#16767 = CARTESIAN_POINT ( 'NONE',  ( 32.20710678118632586, -8.240707523384191546, 5.000000000000000000 ) ) ;
#16768 = ORIENTED_EDGE ( 'NONE', *, *, #17417, .F. ) ;
#16769 = ORIENTED_EDGE ( 'NONE', *, *, #80517, .T. ) ;
#16770 = ORIENTED_EDGE ( 'NONE', *, *, #75371, .F. ) ;
#16771 = CARTESIAN_POINT ( 'NONE',  ( 115.9166666666666714, -6.884901960086287076, -3.975000000000000977 ) ) ;
#16772 = ORIENTED_EDGE ( 'NONE', *, *, #44181, .F. ) ;
#16773 = ORIENTED_EDGE ( 'NONE', *, *, #28086, .T. ) ;
#16774 = VERTEX_POINT ( 'NONE', #983 ) ;
#16775 = CARTESIAN_POINT ( 'NONE',  ( 2.700255128608413990, -27.71228299555204089, 4.000000000000000000 ) ) ;
#16776 = LINE ( 'NONE', #103759, #134316 ) ;
#16777 = VECTOR ( 'NONE', #39118, 999.9999999999998863 ) ;
#16778 = ORIENTED_EDGE ( 'NONE', *, *, #109942, .F. ) ;
#16779 = DIRECTION ( 'NONE',  ( 0.6830127018922180770, -0.6830127018922204085, -0.2588190451025213501 ) ) ;
#16780 = DIRECTION ( 'NONE',  ( 0.7071067811865487940, 0.7071067811865463515, 0.000000000000000000 ) ) ;
#16781 = DIRECTION ( 'NONE',  ( -0.3543493200069162685, -0.000000000000000000, -0.9351131265310288487 ) ) ;
#16782 = CARTESIAN_POINT ( 'NONE',  ( 72.18398860626899705, 28.73617430169837661, 5.000000000000000000 ) ) ;
#16783 = CARTESIAN_POINT ( 'NONE',  ( 115.9379301918980900, -6.110000000000001208, 1.637169565754158951 ) ) ;
#16784 = ADVANCED_FACE ( 'NONE', ( #45267 ), #34352, .T. ) ;
#16785 = VERTEX_POINT ( 'NONE', #2396 ) ;
#16786 = LINE ( 'NONE', #49459, #104265 ) ;
#16787 = LINE ( 'NONE', #96453, #86376 ) ;
#16788 = EDGE_CURVE ( 'NONE', #106463, #119988, #101019, .T. ) ;
#16790 = AXIS2_PLACEMENT_3D ( 'NONE', #139324, #61071, #40013 ) ;
#16789 = LINE ( 'NONE', #72656, #79695 ) ;
#16791 = LINE ( 'NONE', #116814, #16929 ) ;
#16792 = LINE ( 'NONE', #117505, #84524 ) ;
#16793 = CARTESIAN_POINT ( 'NONE',  ( 12.19999999999999574, -25.33999999999998920, 13.17925390838734323 ) ) ;
#16794 = PLANE ( 'NONE',  #80124 ) ;
#16795 = ADVANCED_FACE ( 'NONE', ( #136502 ), #138673, .T. ) ;
#16796 = CARTESIAN_POINT ( 'NONE',  ( 37.12086038379622011, -6.884901960086286188, 3.974999999999997424 ) ) ;
#16797 = FACE_OUTER_BOUND ( 'NONE', #128980, .T. ) ;
#16798 = ORIENTED_EDGE ( 'NONE', *, *, #45064, .F. ) ;
#16799 = ORIENTED_EDGE ( 'NONE', *, *, #135953, .F. ) ;
#16800 = CARTESIAN_POINT ( 'NONE',  ( 32.35416666666665009, -2.130196079827425315, -7.950000000000001066 ) ) ;
#16801 = VERTEX_POINT ( 'NONE', #104597 ) ;
#16802 = EDGE_CURVE ( 'NONE', #140847, #4302, #83583, .T. ) ;
#16803 = CARTESIAN_POINT ( 'NONE',  ( -12.69999999999998153, 3.061616997868383634E-16, -2.500000000000000444 ) ) ;
#16804 = CARTESIAN_POINT ( 'NONE',  ( 23.89661266223020419, -0.3091507863911187037, 4.000000000000000000 ) ) ;
#16805 = EDGE_LOOP ( 'NONE', ( #66834, #102036, #92760, #19762 ) ) ;
#16806 = CIRCLE ( 'NONE', #53874, 2.500000000000000444 ) ;
#16807 = VECTOR ( 'NONE', #43665, 1000.000000000000000 ) ;
#16808 = VECTOR ( 'NONE', #107586, 1000.000000000000227 ) ;
#16809 = CARTESIAN_POINT ( 'NONE',  ( 21.15294044719737698, -2.499999999999996447, 0.000000000000000000 ) ) ;
#16810 = DIRECTION ( 'NONE',  ( 1.000000000000000000, 0.000000000000000000, 0.000000000000000000 ) ) ;
#16811 = AXIS2_PLACEMENT_3D ( 'NONE', #142441, #106190, #109063 ) ;
#16812 = EDGE_CURVE ( 'NONE', #127177, #133750, #18263, .T. ) ;
#16813 = DIRECTION ( 'NONE',  ( 0.6830127018922180770, -0.6830127018922204085, -0.2588190451025213501 ) ) ;
#16815 = VECTOR ( 'NONE', #112270, 1000.000000000000227 ) ;
#16814 = CARTESIAN_POINT ( 'NONE',  ( 53.99451991528749062, 28.92564299267975869, 4.000000000000000000 ) ) ;
#16816 = CARTESIAN_POINT ( 'NONE',  ( 28.72959685856476497, -6.110000000000000320, -1.637169565754161393 ) ) ;
#16817 = ORIENTED_EDGE ( 'NONE', *, *, #13676, .T. ) ;
#16818 = CARTESIAN_POINT ( 'NONE',  ( 60.29974487139158867, -27.71228299555248142, 4.000000000000000000 ) ) ;
#16819 = ORIENTED_EDGE ( 'NONE', *, *, #96974, .F. ) ;
#16820 = AXIS2_PLACEMENT_3D ( 'NONE', #125595, #128442, #37876 ) ;
#16821 =( GEOMETRIC_REPRESENTATION_CONTEXT ( 3 ) GLOBAL_UNCERTAINTY_ASSIGNED_CONTEXT ( ( #73823 ) ) GLOBAL_UNIT_ASSIGNED_CONTEXT ( ( #40008, #50148, #52269 ) ) REPRESENTATION_CONTEXT ( 'NONE', 'WORKASPACE' ) );
#16822 = PLANE ( 'NONE',  #95892 ) ;
#16823 = ADVANCED_FACE ( 'NONE', ( #17569 ), #81454, .T. ) ;
#16824 = CARTESIAN_POINT ( 'NONE',  ( 5.994519915287488843, 28.92564299267942118, 4.000000000000000000 ) ) ;
#16825 = FACE_OUTER_BOUND ( 'NONE', #128059, .T. ) ;
#16826 = PLANE ( 'NONE',  #90423 ) ;
#16827 = ORIENTED_EDGE ( 'NONE', *, *, #49078, .T. ) ;
#16828 = CARTESIAN_POINT ( 'NONE',  ( 51.77126352523143993, 4.472830434245839371, 4.472830434245842035 ) ) ;
#16829 = ORIENTED_EDGE ( 'NONE', *, *, #88004, .T. ) ;
#16830 = DIRECTION ( 'NONE',  ( -0.7071067811865486830, -0.7071067811865464625, 0.000000000000000000 ) ) ;
#16831 = DIRECTION ( 'NONE',  ( 0.3543493200069163240, 0.000000000000000000, 0.9351131265310288487 ) ) ;
#16832 = DIRECTION ( 'NONE',  ( -0.000000000000000000, 0.3543493200069153248, 0.9351131265310292928 ) ) ;
#16833 = EDGE_CURVE ( 'NONE', #108472, #104144, #137812, .T. ) ;
#16834 = PLANE ( 'NONE',  #60312 ) ;
#16835 = EDGE_CURVE ( 'NONE', #54369, #84048, #117577, .T. ) ;
#16836 = VECTOR ( 'NONE', #33021, 1000.000000000000000 ) ;
#16837 = CARTESIAN_POINT ( 'NONE',  ( 50.22459685856477307, -1.637169565754160949, 6.109999999999997655 ) ) ;
#16838 = ORIENTED_EDGE ( 'NONE', *, *, #90982, .F. ) ;
#16839 = CARTESIAN_POINT ( 'NONE',  ( 124.2291666666666714, 7.950000000000001954, -2.130196079827421762 ) ) ;
#16840 = EDGE_CURVE ( 'NONE', #84066, #50105, #72008, .T. ) ;
#16841 = CARTESIAN_POINT ( 'NONE',  ( 23.99999999999984013, 16.55218569542900298, 5.000000000000000000 ) ) ;
#16842 = ORIENTED_EDGE ( 'NONE', *, *, #97483, .F. ) ;
#16843 = ORIENTED_EDGE ( 'NONE', *, *, #64343, .F. ) ;
#16844 = DIRECTION ( 'NONE',  ( -0.000000000000000000, 0.3543493200069153248, 0.9351131265310291818 ) ) ;
#16845 = ORIENTED_EDGE ( 'NONE', *, *, #58621, .F. ) ;
#16846 = VECTOR ( 'NONE', #96362, 999.9999999999998863 ) ;
#16847 = EDGE_CURVE ( 'NONE', #123433, #91250, #28486, .T. ) ;
#16848 = EDGE_CURVE ( 'NONE', #112433, #89628, #62540, .T. ) ;
#16849 = PRODUCT_DEFINITION_SHAPE ( 'NONE', 'NONE',  #143570 ) ;
#16850 = DIRECTION ( 'NONE',  ( -0.3543493200069163240, -0.000000000000000000, -0.9351131265310288487 ) ) ;
#16851 = ORIENTED_EDGE ( 'NONE', *, *, #68849, .T. ) ;
#16852 = AXIS2_PLACEMENT_3D ( 'NONE', #72056, #128544, #138716 ) ;
#16853 = CARTESIAN_POINT ( 'NONE',  ( 44.70419371712955581, -6.884901960086285300, -3.975000000000000089 ) ) ;
#16854 = DIRECTION ( 'NONE',  ( -0.000000000000000000, -0.3543493200069152693, 0.9351131265310292928 ) ) ;
#16855 = VECTOR ( 'NONE', #46268, 1000.000000000000000 ) ;
#16856 = EDGE_CURVE ( 'NONE', #122361, #34748, #106710, .T. ) ;
#16857 = CARTESIAN_POINT ( 'NONE',  ( -12.70612307739187052, 22.22500000000000142, 4.000000000000000000 ) ) ;
#16858 = FACE_BOUND ( 'NONE', #89617, .T. ) ;
#16859 = EDGE_CURVE ( 'NONE', #142079, #10908, #16883, .T. ) ;
#16860 = LINE ( 'NONE', #26310, #105879 ) ;
#16861 = CARTESIAN_POINT ( 'NONE',  ( 2.000000000000256239, -6.019044215166783118, 0.9592349742722835471 ) ) ;
#16862 = DIRECTION ( 'NONE',  ( -0.000000000000000000, 0.3543493200069153248, 0.9351131265310292928 ) ) ;
#16863 = VERTEX_POINT ( 'NONE', #16123 ) ;
#16864 = PRESENTATION_STYLE_ASSIGNMENT (( #103147 ) ) ;
#16866 = VERTEX_POINT ( 'NONE', #61833 ) ;
#16865 = CARTESIAN_POINT ( 'NONE',  ( 54.29974487139159578, -27.71228299555243879, 4.000000000000000000 ) ) ;
#16867 = VERTEX_POINT ( 'NONE', #93013 ) ;
#16868 = ORIENTED_EDGE ( 'NONE', *, *, #137292, .T. ) ;
#16869 = ORIENTED_EDGE ( 'NONE', *, *, #20291, .F. ) ;
#16870 = CARTESIAN_POINT ( 'NONE',  ( 69.47459685856476597, 1.637169565754164280, -6.109999999999996767 ) ) ;
#16871 = ORIENTED_EDGE ( 'NONE', *, *, #63698, .F. ) ;
#16872 = EDGE_CURVE ( 'NONE', #26872, #123892, #7403, .T. ) ;
#16873 = DIRECTION ( 'NONE',  ( -0.7071067811865486830, 0.7071067811865464625, 0.000000000000000000 ) ) ;
#16874 = CARTESIAN_POINT ( 'NONE',  ( 0.1839886062690032631, 28.73617430169787568, 5.000000000000000000 ) ) ;
#16875 = VECTOR ( 'NONE', #113478, 1000.000000000000000 ) ;
#16876 = ORIENTED_EDGE ( 'NONE', *, *, #46481, .F. ) ;
#16877 = CARTESIAN_POINT ( 'NONE',  ( 20.67183060077633172, -9.740707523384180888, 4.000000000000000000 ) ) ;
#16878 = VECTOR ( 'NONE', #123972, 1000.000000000000000 ) ;
#16879 = ADVANCED_FACE ( 'NONE', ( #5260 ), #105993, .F. ) ;
#16880 = CARTESIAN_POINT ( 'NONE',  ( -21.11237052021067129, 8.776708805967446736, 4.202873650309270737 ) ) ;
#16881 = DIRECTION ( 'NONE',  ( 0.6830127018922181881, 0.6830127018922202975, -0.2588190451025214056 ) ) ;
#16882 = LINE ( 'NONE', #38634, #38889 ) ;
#16883 = LINE ( 'NONE', #103850, #67873 ) ;
#16884 = LINE ( 'NONE', #27032, #18440 ) ;
#16885 = EDGE_LOOP ( 'NONE', ( #76114, #5983, #142149, #12451, #121240 ) ) ;
#16886 = VECTOR ( 'NONE', #74446, 1000.000000000000000 ) ;
#16887 = EDGE_LOOP ( 'NONE', ( #141916, #134552, #19702, #62075 ) ) ;
#16888 = CARTESIAN_POINT ( 'NONE',  ( -39.18398860626899705, 28.73617430169814568, 5.000000000000000000 ) ) ;
#16889 = CARTESIAN_POINT ( 'NONE',  ( -3.005480084712505828, 28.92564299267936079, 4.000000000000000000 ) ) ;
#16890 = ORIENTED_EDGE ( 'NONE', *, *, #80680, .T. ) ;
#16891 = ORIENTED_EDGE ( 'NONE', *, *, #13550, .T. ) ;
#16892 = EDGE_LOOP ( 'NONE', ( #130109, #111616, #108534 ) ) ;
#16893 = CARTESIAN_POINT ( 'NONE',  ( 2.999999999999999112, -7.600000000000061817, 34.92499999999998295 ) ) ;
#16894 = CARTESIAN_POINT ( 'NONE',  ( 29.43749999999998934, 5.819803920172574863, -5.819803920172573086 ) ) ;
#16895 = VECTOR ( 'NONE', #35390, 1000.000000000000000 ) ;
#16896 = VERTEX_POINT ( 'NONE', #6660 ) ;
#16897 = CARTESIAN_POINT ( 'NONE',  ( 13.78501580275802141, -3.740707523384238176, 15.76143240460127082 ) ) ;
#16898 = EDGE_CURVE ( 'NONE', #122922, #66605, #139407, .T. ) ;
#16899 = CARTESIAN_POINT ( 'NONE',  ( 8.000000000000007105, 0.000000000000000000, 0.000000000000000000 ) ) ;
#16900 = CARTESIAN_POINT ( 'NONE',  ( 11.29623647476855375, 7.934999999999990727, -1.457635852685135314E-15 ) ) ;
#16901 = LINE ( 'NONE', #105323, #70445 ) ;
#16902 = EDGE_LOOP ( 'NONE', ( #82366, #87529, #11725, #112782 ) ) ;
#16903 = DIRECTION ( 'NONE',  ( 0.6830127018922180770, 0.6830127018922202975, -0.2588190451025213501 ) ) ;
#16904 = DIRECTION ( 'NONE',  ( 1.000000000000000000, 0.000000000000000000, 0.000000000000000000 ) ) ;
#16905 = AXIS2_PLACEMENT_3D ( 'NONE', #10144, #100033, #103558 ) ;
#16907 = ORIENTED_EDGE ( 'NONE', *, *, #19396, .T. ) ;
#16906 = DIRECTION ( 'NONE',  ( -0.7071067811865486830, -0.7071067811865464625, -0.000000000000000000 ) ) ;
#16908 = CARTESIAN_POINT ( 'NONE',  ( -26.99999999999980815, 11.96639925780214675, 5.000000000000000000 ) ) ;
#16909 = ORIENTED_EDGE ( 'NONE', *, *, #83294, .T. ) ;
#16910 = LINE ( 'NONE', #16151, #35743 ) ;
#16911 = DIRECTION ( 'NONE',  ( 0.7071067811865487940, 0.7071067811865463515, 0.000000000000000000 ) ) ;
#16912 = VECTOR ( 'NONE', #126217, 1000.000000000000000 ) ;
#16913 = DIRECTION ( 'NONE',  ( -0.000000000000000000, 0.000000000000000000, 1.000000000000000000 ) ) ;
#16915 = EDGE_LOOP ( 'NONE', ( #27482, #113616, #102670, #51257 ) ) ;
#16914 = AXIS2_PLACEMENT_3D ( 'NONE', #138119, #38807, #85866 ) ;
#16916 = LINE ( 'NONE', #125693, #28698 ) ;
#16917 = DIRECTION ( 'NONE',  ( -0.7071067811865486830, 0.7071067811865464625, 0.000000000000000000 ) ) ;
#16918 = CARTESIAN_POINT ( 'NONE',  ( -21.48921356237309155, -27.52281430457070499, 5.000000000000000000 ) ) ;
#16919 = VECTOR ( 'NONE', #28149, 1000.000000000000000 ) ;
#16920 = VERTEX_POINT ( 'NONE', #40784 ) ;
#16921 = AXIS2_PLACEMENT_3D ( 'NONE', #135950, #103302, #35246 ) ;
#16922 = DIRECTION ( 'NONE',  ( 0.3543493200069162685, -0.000000000000000000, -0.9351131265310288487 ) ) ;
#16923 = FACE_OUTER_BOUND ( 'NONE', #63620, .T. ) ;
#16924 = DIRECTION ( 'NONE',  ( 0.3543493200069162685, -0.000000000000000000, -0.9351131265310288487 ) ) ;
#16925 = CARTESIAN_POINT ( 'NONE',  ( -22.37177410554622980, -1.784312229707115893, 4.000000000000000000 ) ) ;
#16926 = CARTESIAN_POINT ( 'NONE',  ( -35.18650864602339112, -15.74070752338412049, 8.904080028139022218 ) ) ;
#16927 = ORIENTED_EDGE ( 'NONE', *, *, #70877, .F. ) ;
#16928 = VERTEX_POINT ( 'NONE', #42933 ) ;
#16929 = VECTOR ( 'NONE', #44283, 1000.000000000000000 ) ;
#16930 = PLANE ( 'NONE',  #93526 ) ;
#16931 = DIRECTION ( 'NONE',  ( 0.6830127018922180770, -0.6830127018922204085, -0.2588190451025213501 ) ) ;
#16932 = CARTESIAN_POINT ( 'NONE',  ( 5.666236474768552966, 7.934999999999990727, -1.457635852685135314E-15 ) ) ;
#16933 = CARTESIAN_POINT ( 'NONE',  ( 23.99451991528749062, 28.92564299267954908, 4.000000000000000000 ) ) ;
#16934 = COLOUR_RGB ( '', 0.66274510, 0.83137255, 0.94901961) ;
#16935 = DIRECTION ( 'NONE',  ( 0.5735764363510453823, -0.8191520442889923537, 1.003171929053525486E-16 ) ) ;
#16936 = CARTESIAN_POINT ( 'NONE',  ( -28.78678096696623356, 12.75929247661558996, 10.29404684609028742 ) ) ;
#16937 = CARTESIAN_POINT ( 'NONE',  ( -36.18398860626899705, 28.73617430169812437, 5.000000000000000000 ) ) ;
#16938 = VERTEX_POINT ( 'NONE', #42220 ) ;
#16939 = CARTESIAN_POINT ( 'NONE',  ( -63.48921356237309510, -27.52281430457099631, 5.000000000000000000 ) ) ;
#16940 = ADVANCED_FACE ( 'NONE', ( #43615 ), #87840, .F. ) ;
#16941 = FACE_OUTER_BOUND ( 'NONE', #77364, .T. ) ;
#16942 = FACE_OUTER_BOUND ( 'NONE', #47157, .T. ) ;
#16943 = DIRECTION ( 'NONE',  ( 0.5735764363510453823, -0.8191520442889923537, 1.003171929053525486E-16 ) ) ;
#16944 = CARTESIAN_POINT ( 'NONE',  ( 49.34959685856478728, 6.109999999999997655, 1.637169565754163836 ) ) ;
#16945 = VECTOR ( 'NONE', #130132, 999.9999999999998863 ) ;
#16946 = CARTESIAN_POINT ( 'NONE',  ( 183.6042742895559172, -52.10338527932237440, -40.45859298138255156 ) ) ;
#16948 = EDGE_CURVE ( 'NONE', #34094, #105119, #19718, .T. ) ;
#16947 = ORIENTED_EDGE ( 'NONE', *, *, #91461, .F. ) ;
#16949 = FACE_OUTER_BOUND ( 'NONE', #85502, .T. ) ;
#16950 = CIRCLE ( 'NONE', #35511, 3.999999999999996447 ) ;
#16951 = ORIENTED_EDGE ( 'NONE', *, *, #32919, .T. ) ;
#16952 = VERTEX_POINT ( 'NONE', #21865 ) ;
#16953 = LINE ( 'NONE', #140167, #29312 ) ;
#16954 = DIRECTION ( 'NONE',  ( 0.000000000000000000, -0.000000000000000000, -1.000000000000000000 ) ) ;
#16956 = VECTOR ( 'NONE', #49749, 1000.000000000000227 ) ;
#16955 = CARTESIAN_POINT ( 'NONE',  ( 7.139999999999985469, -39.93000000000000682, -7.899272885403731514 ) ) ;
#16957 = EDGE_CURVE ( 'NONE', #13692, #111562, #30629, .T. ) ;
#16958 = CARTESIAN_POINT ( 'NONE',  ( -42.18398860626899705, 28.73617430169816700, 5.000000000000000000 ) ) ;
#16959 = PLANE ( 'NONE',  #67313 ) ;
#16960 = EDGE_CURVE ( 'NONE', #132555, #74043, #21475, .T. ) ;
#16961 = ADVANCED_FACE ( 'NONE', ( #32033 ), #77001, .F. ) ;
#16962 = ORIENTED_EDGE ( 'NONE', *, *, #42728, .F. ) ;
#16963 = DIRECTION ( 'NONE',  ( 0.7071067811865487940, 0.7071067811865463515, 0.000000000000000000 ) ) ;
#16964 = CARTESIAN_POINT ( 'NONE',  ( 7.499999999999947597, -16.53360074219757081, 5.000000000000000000 ) ) ;
#16965 = UNCERTAINTY_MEASURE_WITH_UNIT (LENGTH_MEASURE( 1.000000000000000082E-05 ), #43590, 'distance_accuracy_value', 'NONE');
#16966 = DIRECTION ( 'NONE',  ( 0.6830127018922181881, 0.6830127018922202975, -0.2588190451025214056 ) ) ;
#16967 = DIRECTION ( 'NONE',  ( -1.000000000000000000, -0.000000000000000000, -0.000000000000000000 ) ) ;
#16968 = CARTESIAN_POINT ( 'NONE',  ( -3.328169399223508851, 17.25929247661553489, 4.000000000000000000 ) ) ;
#16970 = EDGE_CURVE ( 'NONE', #72338, #31169, #85682, .T. ) ;
#16969 = VECTOR ( 'NONE', #131225, 1000.000000000000000 ) ;
#16972 = ADVANCED_FACE ( 'NONE', ( #130659 ), #75549, .F. ) ;
#16971 = CARTESIAN_POINT ( 'NONE',  ( 65.41252705046289861, -7.949999999999998401, -4.867971026610728450E-16 ) ) ;
#16973 = DIRECTION ( 'NONE',  ( -0.000000000000000000, 0.000000000000000000, 1.000000000000000000 ) ) ;
#16974 = ORIENTED_EDGE ( 'NONE', *, *, #24336, .T. ) ;
#16975 = ORIENTED_EDGE ( 'NONE', *, *, #31824, .F. ) ;
#16976 = CARTESIAN_POINT ( 'NONE',  ( 67.64583333333330017, 2.130196079827431976, -7.949999999999999289 ) ) ;
#16977 = CARTESIAN_POINT ( 'NONE',  ( -24.70710678118637560, 11.25929247661560417, 5.000000000000000000 ) ) ;
#16978 = EDGE_CURVE ( 'NONE', #115946, #46130, #109588, .T. ) ;
#16979 = LINE ( 'NONE', #136598, #57886 ) ;
#16980 = VECTOR ( 'NONE', #80476, 1000.000000000000000 ) ;
#16981 = EDGE_LOOP ( 'NONE', ( #135597, #82932, #9443, #29082, #75042, #127690 ) ) ;
#16982 =( BOUNDED_CURVE ( )  B_SPLINE_CURVE ( 3, ( #53419, #8440, #7752, #56143 ),
 .UNSPECIFIED., .F., .F. ) 
 B_SPLINE_CURVE_WITH_KNOTS ( ( 4, 4 ),
 ( 2.779374508378134045, 4.199602562396851368 ),
 .UNSPECIFIED. ) 
 CURVE ( )  GEOMETRIC_REPRESENTATION_ITEM ( )  RATIONAL_B_SPLINE_CURVE ( ( 1.000000000000000000, 0.8388583629366599403, 0.8388583629366599403, 1.000000000000000000 ) ) 
 REPRESENTATION_ITEM ( '' )  );
#16983 = CARTESIAN_POINT ( 'NONE',  ( 33.52083333333333570, 7.949999999999998401, 2.130196079827431532 ) ) ;
#16984 = EDGE_CURVE ( 'NONE', #16056, #110777, #52352, .T. ) ;
#16985 = LINE ( 'NONE', #38039, #125353 ) ;
#16986 = CARTESIAN_POINT ( 'NONE',  ( 52.93793019189809002, -6.110000000000001208, 1.637169565754158951 ) ) ;
#16987 = DIRECTION ( 'NONE',  ( 0.7071067811865486830, -0.7071067811865464625, -0.000000000000000000 ) ) ;
#16988 = ORIENTED_EDGE ( 'NONE', *, *, #6146, .T. ) ;
#16989 = ORIENTED_EDGE ( 'NONE', *, *, #52192, .T. ) ;
#16990 = PRESENTATION_LAYER_ASSIGNMENT (  '', '', ( #88724 ) ) ;
#16991 = DIRECTION ( 'NONE',  ( -0.7071067811865486830, -0.7071067811865464625, 0.000000000000000000 ) ) ;
#16992 = DIRECTION ( 'NONE',  ( 0.7071067811865487940, 0.7071067811865463515, 0.000000000000000000 ) ) ;
#16993 = CARTESIAN_POINT ( 'NONE',  ( 18.79333936457835108, 21.75929247661549937, 4.998822639870708073 ) ) ;
#16994 = LINE ( 'NONE', #39476, #83395 ) ;
#16995 = LINE ( 'NONE', #72132, #62711 ) ;
#16997 = ORIENTED_EDGE ( 'NONE', *, *, #87866, .F. ) ;
#16996 = DIRECTION ( 'NONE',  ( -1.000000000000000000, -1.224606353822377258E-16, -0.000000000000000000 ) ) ;
#16998 = DIRECTION ( 'NONE',  ( -0.7071067811865487940, 0.7071067811865463515, -0.000000000000000000 ) ) ;
#16999 = PLANE ( 'NONE',  #54639 ) ;
#17000 = AXIS2_PLACEMENT_3D ( 'NONE', #14844, #102599, #34471 ) ;
#17001 = LINE ( 'NONE', #103974, #118813 ) ;
#17002 = EDGE_CURVE ( 'NONE', #124237, #98685, #98704, .T. ) ;
#17003 = CARTESIAN_POINT ( 'NONE',  ( 15.29974487139158867, -27.71228299555216879, 4.000000000000000000 ) ) ;
#17004 = ORIENTED_EDGE ( 'NONE', *, *, #177, .F. ) ;
#17005 = ORIENTED_EDGE ( 'NONE', *, *, #93848, .T. ) ;
#17006 = AXIS2_PLACEMENT_3D ( 'NONE', #18632, #72382, #117231 ) ;
#17007 = CARTESIAN_POINT ( 'NONE',  ( 55.56056557994604361, -57.14999999999999147, -39.86617647058817937 ) ) ;
#17008 = LINE ( 'NONE', #38062, #87259 ) ;
#17009 = EDGE_CURVE ( 'NONE', #131899, #48968, #102616, .T. ) ;
#17010 = CARTESIAN_POINT ( 'NONE',  ( 33.29974487139158867, -27.71228299555229313, 4.000000000000000000 ) ) ;
#17011 = DIRECTION ( 'NONE',  ( -0.000000000000000000, 0.3543493200069153248, 0.9351131265310292928 ) ) ;
#17012 = VERTEX_POINT ( 'NONE', #32771 ) ;
#17013 = ORIENTED_EDGE ( 'NONE', *, *, #117489, .F. ) ;
#17014 = DIRECTION ( 'NONE',  ( 0.6830127018922181881, 0.6830127018922202975, -0.2588190451025214056 ) ) ;
#17015 = CARTESIAN_POINT ( 'NONE',  ( 63.29974487139158867, -27.71228299555250274, 4.000000000000000000 ) ) ;
#17016 = ORIENTED_EDGE ( 'NONE', *, *, #143326, .T. ) ;
#17017 = AXIS2_PLACEMENT_3D ( 'NONE', #105136, #26162, #38461 ) ;
#17018 = ADVANCED_FACE ( 'NONE', ( #10264 ), #53052, .F. ) ;
#17019 = ORIENTED_EDGE ( 'NONE', *, *, #12573, .F. ) ;
#17020 = DIRECTION ( 'NONE',  ( 0.7071067811865487940, -0.7071067811865463515, 0.000000000000000000 ) ) ;
#17022 = EDGE_CURVE ( 'NONE', #31340, #26097, #65410, .T. ) ;
#17021 = VERTEX_POINT ( 'NONE', #64668 ) ;
#17023 = DIRECTION ( 'NONE',  ( 0.7071067811865486830, -0.7071067811865464625, -0.000000000000000000 ) ) ;
#17024 = DIRECTION ( 'NONE',  ( -0.7071067811865487940, 0.7071067811865463515, 0.000000000000000000 ) ) ;
#17025 = AXIS2_PLACEMENT_3D ( 'NONE', #116130, #18213, #105260 ) ;
#17026 = CARTESIAN_POINT ( 'NONE',  ( 123.3754301918981184, -5.291415217122920289, -3.055000000000001492 ) ) ;
#17027 = EDGE_CURVE ( 'NONE', #28105, #137698, #74118, .T. ) ;
#17028 = FACE_BOUND ( 'NONE', #2951, .T. ) ;
#17029 = DIRECTION ( 'NONE',  ( 1.000000000000000000, 0.000000000000000000, 0.000000000000000000 ) ) ;
#17030 = CARTESIAN_POINT ( 'NONE',  ( -26.99999999999980815, -9.033600742197648970, 5.000000000000000000 ) ) ;
#17032 = EDGE_LOOP ( 'NONE', ( #60600, #104935, #128876 ) ) ;
#17031 = CYLINDRICAL_SURFACE ( 'NONE', #66721, 6.349999999999999645 ) ;
#17034 = EDGE_CURVE ( 'NONE', #745, #47403, #66113, .T. ) ;
#17033 = VECTOR ( 'NONE', #26317, 1000.000000000000000 ) ;
#17035 = PRESENTATION_STYLE_ASSIGNMENT (( #14162 ) ) ;
#17036 = SHAPE_DEFINITION_REPRESENTATION ( #10005, #9754 ) ;
#17037 = VERTEX_POINT ( 'NONE', #84985 ) ;
#17038 = VECTOR ( 'NONE', #138375, 999.9999999999998863 ) ;
#17039 = ORIENTED_EDGE ( 'NONE', *, *, #38073, .T. ) ;
#17040 = CARTESIAN_POINT ( 'NONE',  ( 93.53709685856479439, -3.054999999999998828, -5.291415217122919401 ) ) ;
#17041 = EDGE_LOOP ( 'NONE', ( #50439, #47263, #95344, #29623, #135931 ) ) ;
#17042 = EDGE_CURVE ( 'NONE', #82553, #27734, #132081, .T. ) ;
#17043 = CARTESIAN_POINT ( 'NONE',  ( 45.18398860626900415, 28.73617430169818832, 5.000000000000000000 ) ) ;
#17044 = LINE ( 'NONE', #61313, #7632 ) ;
#17045 = VECTOR ( 'NONE', #125680, 1000.000000000000000 ) ;
#17046 = CARTESIAN_POINT ( 'NONE',  ( 0.000000000000000000, 0.000000000000000000, 10.00000000000000000 ) ) ;
#17047 = ORIENTED_EDGE ( 'NONE', *, *, #58860, .T. ) ;
#17048 = DIRECTION ( 'NONE',  ( -0.7071067811865486830, 0.7071067811865464625, 0.000000000000000000 ) ) ;
#17049 = ADVANCED_FACE ( 'NONE', ( #19016 ), #100855, .F. ) ;
#17050 = DIRECTION ( 'NONE',  ( 0.000000000000000000, 0.000000000000000000, -1.000000000000000000 ) ) ;
#17051 = CONICAL_SURFACE ( 'NONE', #30938, 2.500000000000000888, 0.9599310885968822538 ) ;
#17052 = CARTESIAN_POINT ( 'NONE',  ( 102.5000000000000142, 0.000000000000000000, -7.950000000000000178 ) ) ;
#17054 = CARTESIAN_POINT ( 'NONE',  ( 13.29826936130429260, 3.821174125832445049E-16, 0.000000000000000000 ) ) ;
#17053 = DIRECTION ( 'NONE',  ( -1.000000000000000000, -1.224606353822377258E-16, -0.000000000000000000 ) ) ;
#17055 = DIRECTION ( 'NONE',  ( 0.000000000000000000, 0.000000000000000000, 1.000000000000000000 ) ) ;
#17056 = DIRECTION ( 'NONE',  ( -1.000000000000000000, -0.000000000000000000, -0.000000000000000000 ) ) ;
#17057 = VERTEX_POINT ( 'NONE', #124748 ) ;
#17058 = FACE_OUTER_BOUND ( 'NONE', #13517, .T. ) ;
#17059 = CARTESIAN_POINT ( 'NONE',  ( -32.99999999999977263, -21.41253812416053037, 4.000000000000000000 ) ) ;
#17060 = VECTOR ( 'NONE', #105784, 1000.000000000000000 ) ;
#17061 = VERTEX_POINT ( 'NONE', #90719 ) ;
#17062 = EDGE_CURVE ( 'NONE', #123049, #90489, #78400, .T. ) ;
#17063 = ORIENTED_EDGE ( 'NONE', *, *, #79029, .F. ) ;
#17064 = EDGE_LOOP ( 'NONE', ( #46098, #31323, #25421, #89404 ) ) ;
#17065 = CARTESIAN_POINT ( 'NONE',  ( 44.04209685856477563, 5.291415217122923842, -3.054999999999996163 ) ) ;
#17066 = VERTEX_POINT ( 'NONE', #22547 ) ;
#17067 = VECTOR ( 'NONE', #30796, 1000.000000000000000 ) ;
#17068 = EDGE_CURVE ( 'NONE', #45188, #10027, #69, .T. ) ;
#17069 = VECTOR ( 'NONE', #37029, 1000.000000000000000 ) ;
#17070 = CARTESIAN_POINT ( 'NONE',  ( 15.79580628287043709, -5.278424836066144543, 3.047499999999995879 ) ) ;
#17071 = CARTESIAN_POINT ( 'NONE',  ( -16.11017474120846060, 1.958518950653415303, -30.40717620614491068 ) ) ;
#17072 = ORIENTED_EDGE ( 'NONE', *, *, #38798, .F. ) ;
#17073 = DIRECTION ( 'NONE',  ( -0.000000000000000000, 0.000000000000000000, 1.000000000000000000 ) ) ;
#17074 = ORIENTED_EDGE ( 'NONE', *, *, #38299, .F. ) ;
#17075 = CARTESIAN_POINT ( 'NONE',  ( 11.99451991528749417, 28.92564299267946382, 4.000000000000000000 ) ) ;
#17076 = CIRCLE ( 'NONE', #139735, 5.968999999999998529 ) ;
#17077 = DIRECTION ( 'NONE',  ( 0.000000000000000000, -1.000000000000000000, 0.000000000000000000 ) ) ;
#17079 = ORIENTED_EDGE ( 'NONE', *, *, #99781, .F. ) ;
#17078 = DIRECTION ( 'NONE',  ( -0.6830127018922180770, -0.6830127018922204085, -0.2588190451025213501 ) ) ;
#17080 = VERTEX_POINT ( 'NONE', #11668 ) ;
#17081 = LINE ( 'NONE', #36672, #79363 ) ;
#17082 = CARTESIAN_POINT ( 'NONE',  ( -3.469446951953614189E-15, -9.412538124160651165, 4.000000000000000000 ) ) ;
#17083 = EDGE_LOOP ( 'NONE', ( #17310, #68930, #117046, #94123 ) ) ;
#17084 = EDGE_CURVE ( 'NONE', #62679, #138950, #12408, .T. ) ;
#17085 = FACE_OUTER_BOUND ( 'NONE', #109905, .T. ) ;
#17086 = VERTEX_POINT ( 'NONE', #133498 ) ;
#17087 = ORIENTED_EDGE ( 'NONE', *, *, #55588, .T. ) ;
#17088 = ORIENTED_EDGE ( 'NONE', *, *, #12082, .F. ) ;
#17089 = VERTEX_POINT ( 'NONE', #99398 ) ;
#17090 = DIRECTION ( 'NONE',  ( 0.000000000000000000, 1.000000000000000000, -3.469446951953614189E-15 ) ) ;
#17091 = AXIS2_PLACEMENT_3D ( 'NONE', #62043, #93923, #72942 ) ;
#17092 = LINE ( 'NONE', #40300, #81769 ) ;
#17093 = LINE ( 'NONE', #16338, #111970 ) ;
#17094 = CARTESIAN_POINT ( 'NONE',  ( 3.250000000000000000, -5.000000000000000000, -6.123233995736766282E-16 ) ) ;
#17095 = EDGE_CURVE ( 'NONE', #41252, #127203, #122597, .T. ) ;
#17096 = ORIENTED_EDGE ( 'NONE', *, *, #67932, .T. ) ;
#17097 = FACE_OUTER_BOUND ( 'NONE', #19744, .T. ) ;
#17098 = AXIS2_PLACEMENT_3D ( 'NONE', #81214, #111113, #137003 ) ;
#17099 = ORIENTED_EDGE ( 'NONE', *, *, #115643, .F. ) ;
#17100 = DIRECTION ( 'NONE',  ( -0.000000000000000000, 0.3543493200069153248, 0.9351131265310292928 ) ) ;
#17101 = CARTESIAN_POINT ( 'NONE',  ( 30.60373647476856007, 5.808823158059036373, 5.808823158059032821 ) ) ;
#17102 = LINE ( 'NONE', #92494, #104128 ) ;
#17103 = VECTOR ( 'NONE', #4517, 999.9999999999998863 ) ;
#17104 = DIRECTION ( 'NONE',  ( -0.7071067811865486830, -0.7071067811865464625, -0.000000000000000000 ) ) ;
#17105 = PLANE ( 'NONE',  #97605 ) ;
#17106 = ORIENTED_EDGE ( 'NONE', *, *, #68943, .T. ) ;
#17107 = ORIENTED_EDGE ( 'NONE', *, *, #80434, .T. ) ;
#17108 = ORIENTED_EDGE ( 'NONE', *, *, #99160, .T. ) ;
#17109 = CARTESIAN_POINT ( 'NONE',  ( 20.16170612452607358, -6.740707523384209310, 16.75550250614871928 ) ) ;
#17110 = CARTESIAN_POINT ( 'NONE',  ( 94.87086038379621300, 6.884901960086289741, -3.974999999999993427 ) ) ;
#17111 = CYLINDRICAL_SURFACE ( 'NONE', #15227, 1.898649999999994842 ) ;
#17112 = CARTESIAN_POINT ( 'NONE',  ( 11.70025512860841133, -27.71228299555198049, 4.000000000000000000 ) ) ;
#17113 = CARTESIAN_POINT ( 'NONE',  ( 0.2099742459738602463, -51.66308182546714534, -38.35990878063566356 ) ) ;
#17114 = CARTESIAN_POINT ( 'NONE',  ( 73.84959685856480860, 6.109999999999997655, 1.637169565754163836 ) ) ;
#17115 = VECTOR ( 'NONE', #98358, 999.9999999999998863 ) ;
#17116 = DIRECTION ( 'NONE',  ( -0.000000000000000000, 1.301042606982605074E-16, -1.000000000000000000 ) ) ;
#17117 = CARTESIAN_POINT ( 'NONE',  ( 41.99451991528749062, 28.92564299267967343, 4.000000000000000000 ) ) ;
#17118 = LINE ( 'NONE', #127294, #13101 ) ;
#17119 = DIRECTION ( 'NONE',  ( -0.7071067811865487940, 0.7071067811865463515, -0.000000000000000000 ) ) ;
#17120 = LINE ( 'NONE', #95386, #109023 ) ;
#17121 = EDGE_LOOP ( 'NONE', ( #28099, #53632, #63589, #27610, #79779, #46093 ) ) ;
#17122 = CARTESIAN_POINT ( 'NONE',  ( -27.48921356237309155, -27.52281430457074762, 5.000000000000000000 ) ) ;
#17123 = VERTEX_POINT ( 'NONE', #1509 ) ;
#17124 = ADVANCED_FACE ( 'NONE', ( #13111 ), #5396, .T. ) ;
#17125 = DIRECTION ( 'NONE',  ( -0.3543493200069162685, -0.000000000000000000, -0.9351131265310288487 ) ) ;
#17127 = ORIENTED_EDGE ( 'NONE', *, *, #58693, .F. ) ;
#17126 = LINE ( 'NONE', #49058, #18650 ) ;
#17128 = SPHERICAL_SURFACE ( 'NONE', #67980, 0.5000000000000000000 ) ;
#17129 = CARTESIAN_POINT ( 'NONE',  ( -27.48921356237309155, -27.52281430457074762, 5.000000000000000000 ) ) ;
#17130 = EDGE_CURVE ( 'NONE', #107938, #64706, #124045, .T. ) ;
#17131 = EDGE_LOOP ( 'NONE', ( #75288, #43806, #73065 ) ) ;
#17132 = ORIENTED_EDGE ( 'NONE', *, *, #112990, .F. ) ;
#17133 = DIRECTION ( 'NONE',  ( -0.6830127018922181881, 0.6830127018922202975, -0.2588190451025214056 ) ) ;
#17134 = CARTESIAN_POINT ( 'NONE',  ( 120.9750270504628986, -5.819803920172573086, 5.819803920172573086 ) ) ;
#17135 = VECTOR ( 'NONE', #75202, 1000.000000000000000 ) ;
#17136 = DIRECTION ( 'NONE',  ( 0.7071067811865487940, 0.7071067811865463515, -0.000000000000000000 ) ) ;
#17137 = EDGE_CURVE ( 'NONE', #67449, #1511, #36326, .T. ) ;
#17139 = ADVANCED_FACE ( 'NONE', ( #101555 ), #56381, .T. ) ;
#17138 = CARTESIAN_POINT ( 'NONE',  ( 89.76669371712954160, -7.949999999999999289, 2.130196079827424427 ) ) ;
#17140 = CARTESIAN_POINT ( 'NONE',  ( 71.14583333333332860, 2.130196079827356037, -7.950000000000043698 ) ) ;
#17141 = VECTOR ( 'NONE', #39274, 1000.000000000000227 ) ;
#17142 = FACE_OUTER_BOUND ( 'NONE', #21288, .T. ) ;
#17144 = ADVANCED_FACE ( 'NONE', ( #34909 ), #100158, .T. ) ;
#17143 = ORIENTED_EDGE ( 'NONE', *, *, #67503, .F. ) ;
#17145 = CARTESIAN_POINT ( 'NONE',  ( 0.000000000000000000, 0.000000000000000000, 7.950000000000000178 ) ) ;
#17146 = ADVANCED_FACE ( 'NONE', ( #123351 ), #91421, .F. ) ;
#17147 = LINE ( 'NONE', #17827, #41487 ) ;
#17148 = CARTESIAN_POINT ( 'NONE',  ( 21.58333333333333570, -5.278424836066144543, 3.047499999999995879 ) ) ;
#17149 = CARTESIAN_POINT ( 'NONE',  ( -15.68879807097514956, -1.757674993583058898, 4.000000000000000000 ) ) ;
#17150 = PLANE ( 'NONE',  #16631 ) ;
#17151 = ADVANCED_FACE ( 'NONE', ( #113140 ), #25419, .F. ) ;
#17152 = VERTEX_POINT ( 'NONE', #24019 ) ;
#17153 = CARTESIAN_POINT ( 'NONE',  ( -25.49999999999982236, -11.94781430457071103, 5.000000000000000000 ) ) ;
#17155 = ORIENTED_EDGE ( 'NONE', *, *, #132793, .T. ) ;
#17154 = ADVANCED_FACE ( 'NONE', ( #44369 ), #34185, .F. ) ;
#17156 = AXIS2_PLACEMENT_3D ( 'NONE', #109621, #96568, #107480 ) ;
#17157 = CARTESIAN_POINT ( 'NONE',  ( 84.72959685856476142, -6.110000000000000320, -1.637169565754161393 ) ) ;
#17158 = CARTESIAN_POINT ( 'NONE',  ( 21.44840764549667611, -2.500000000000000888, 0.000000000000000000 ) ) ;
#17159 = DIRECTION ( 'NONE',  ( -0.000000000000000000, -1.000000000000000000, -0.000000000000000000 ) ) ;
#17160 = DIRECTION ( 'NONE',  ( -1.000000000000000000, 0.000000000000000000, -0.000000000000000000 ) ) ;
#17161 = VERTEX_POINT ( 'NONE', #46532 ) ;
#17162 = CARTESIAN_POINT ( 'NONE',  ( -25.49999999999981171, 22.08746187583901843, 4.000000000000000000 ) ) ;
#17163 = AXIS2_PLACEMENT_3D ( 'NONE', #54572, #118362, #140150 ) ;
#17164 = ADVANCED_FACE ( 'NONE', ( #45098 ), #23271, .F. ) ;
#17165 = CARTESIAN_POINT ( 'NONE',  ( 0.000000000000000000, 0.000000000000000000, 6.750000000000000888 ) ) ;
#17166 = VECTOR ( 'NONE', #118891, 999.9999999999998863 ) ;
#17167 = PLANE ( 'NONE',  #143509 ) ;
#17169 = ORIENTED_EDGE ( 'NONE', *, *, #26330, .F. ) ;
#17168 = DIRECTION ( 'NONE',  ( -0.7071067811865486830, -0.7071067811865464625, -0.000000000000000000 ) ) ;
#17170 = CARTESIAN_POINT ( 'NONE',  ( 51.18398860626899705, 28.73617430169823095, 5.000000000000000000 ) ) ;
#17171 = CARTESIAN_POINT ( 'NONE',  ( -23.03315071937583980, 7.620612595215163765, 4.000000000000000000 ) ) ;
#17172 = CARTESIAN_POINT ( 'NONE',  ( 1.394470636259349527, -0.3801107925066945503, 6.692409305308472334 ) ) ;
#17173 = EDGE_CURVE ( 'NONE', #15103, #99152, #82004, .T. ) ;
#17174 = CARTESIAN_POINT ( 'NONE',  ( -54.48921356237310221, -27.52281430457093236, 5.000000000000000000 ) ) ;
#17175 = AXIS2_PLACEMENT_3D ( 'NONE', #90525, #136870, #135470 ) ;
#17176 = VERTEX_POINT ( 'NONE', #115250 ) ;
#17177 = EDGE_LOOP ( 'NONE', ( #124029, #69148, #22987, #53212 ) ) ;
#17178 = CARTESIAN_POINT ( 'NONE',  ( 74.37543019189810423, -5.291415217122920289, -3.055000000000001492 ) ) ;
#17179 = CONICAL_SURFACE ( 'NONE', #51959, 2.055000000000001048, 0.9599310885968758145 ) ;
#17180 = VERTEX_POINT ( 'NONE', #28307 ) ;
#17181 = FACE_OUTER_BOUND ( 'NONE', #107031, .T. ) ;
#17182 = CARTESIAN_POINT ( 'NONE',  ( 184.1500000000000057, -14.29000000000013593, 12.69999999999954632 ) ) ;
#17183 = DIRECTION ( 'NONE',  ( -0.000000000000000000, 0.000000000000000000, 1.000000000000000000 ) ) ;
#17184 = ORIENTED_EDGE ( 'NONE', *, *, #139362, .F. ) ;
#17185 = LINE ( 'NONE', #74439, #32947 ) ;
#17186 = LINE ( 'NONE', #49123, #83809 ) ;
#17187 =( GEOMETRIC_REPRESENTATION_CONTEXT ( 3 ) GLOBAL_UNCERTAINTY_ASSIGNED_CONTEXT ( ( #108726 ) ) GLOBAL_UNIT_ASSIGNED_CONTEXT ( ( #90147, #122777, #2395 ) ) REPRESENTATION_CONTEXT ( 'NONE', 'WORKASPACE' ) );
#17188 = ORIENTED_EDGE ( 'NONE', *, *, #24340, .T. ) ;
#17189 = CARTESIAN_POINT ( 'NONE',  ( 25.49999999999981526, -11.94781430457070215, 5.000000000000000000 ) ) ;
#17190 = EDGE_CURVE ( 'NONE', #129678, #50577, #115991, .T. ) ;
#17191 = CARTESIAN_POINT ( 'NONE',  ( 10.46799328145038821, 2.055000000000001048, 2.516649172247811554E-16 ) ) ;
#17192 = CIRCLE ( 'NONE', #91309, 5.968999999999998529 ) ;
#17193 = CARTESIAN_POINT ( 'NONE',  ( 12.19999999999999574, -59.76999999999998892, -39.50000000000000000 ) ) ;
#17194 = EDGE_CURVE ( 'NONE', #75175, #123070, #82687, .T. ) ;
#17195 = ORIENTED_EDGE ( 'NONE', *, *, #33873, .F. ) ;
#17196 = ORIENTED_EDGE ( 'NONE', *, *, #140874, .T. ) ;
#17197 = CARTESIAN_POINT ( 'NONE',  ( 1.499999999999990896, 3.653845994658389884, -4.504631822206375702 ) ) ;
#17198 = CARTESIAN_POINT ( 'NONE',  ( 1.171830600776463838, -14.24070752338414358, 4.000000000000000000 ) ) ;
#17199 = LINE ( 'NONE', #26644, #102089 ) ;
#17200 = SURFACE_STYLE_USAGE ( .BOTH. , #93331 ) ;
#17201 = ADVANCED_FACE ( 'NONE', ( #92105 ), #4321, .F. ) ;
#17202 = LINE ( 'NONE', #38955, #21102 ) ;
#17203 =( NAMED_UNIT ( * ) PLANE_ANGLE_UNIT ( ) SI_UNIT ( $, .RADIAN. ) );
#17204 = ORIENTED_EDGE ( 'NONE', *, *, #128984, .F. ) ;
#17205 = VERTEX_POINT ( 'NONE', #60977 ) ;
#17206 = ORIENTED_EDGE ( 'NONE', *, *, #30383, .T. ) ;
#17207 = ADVANCED_FACE ( 'NONE', ( #113871 ), #71825, .T. ) ;
#17208 = VERTEX_POINT ( 'NONE', #126868 ) ;
#17209 = AXIS2_PLACEMENT_3D ( 'NONE', #26326, #132446, #45427 ) ;
#17210 = PLANE ( 'NONE',  #59395 ) ;
#17211 = SURFACE_STYLE_FILL_AREA ( #18607 ) ;
#17212 = ORIENTED_EDGE ( 'NONE', *, *, #76926, .F. ) ;
#17213 = SURFACE_STYLE_FILL_AREA ( #61475 ) ;
#17214 = CYLINDRICAL_SURFACE ( 'NONE', #116660, 7.950000000000000178 ) ;
#17215 = CARTESIAN_POINT ( 'NONE',  ( 2.510786437626908008, -27.52281430457053446, 5.000000000000000000 ) ) ;
#17216 = LINE ( 'NONE', #74476, #4441 ) ;
#17217 = CARTESIAN_POINT ( 'NONE',  ( 27.00000000000000000, -6.630908077684978252, -3.107243673821709962 ) ) ;
#17218 = EDGE_LOOP ( 'NONE', ( #6845, #26789, #61714, #30068, #135587, #74553 ) ) ;
#17219 = DIRECTION ( 'NONE',  ( -0.7071067811865486830, -0.7071067811865464625, 0.000000000000000000 ) ) ;
#17220 = CARTESIAN_POINT ( 'NONE',  ( 31.49999999999978684, 0.05218569542916537407, 5.000000000000000000 ) ) ;
#17221 = ORIENTED_EDGE ( 'NONE', *, *, #119476, .T. ) ;
#17222 = CARTESIAN_POINT ( 'NONE',  ( -4.000000000000000000, -8.616843969807042924, -4.898587196589412829E-16 ) ) ;
#17223 = ORIENTED_EDGE ( 'NONE', *, *, #265, .T. ) ;
#17224 = EDGE_CURVE ( 'NONE', #78506, #76045, #103678, .T. ) ;
#17225 = CARTESIAN_POINT ( 'NONE',  ( 12.19999999999999574, -40.43000000000000682, -40.00000000000000000 ) ) ;
#17226 = ORIENTED_EDGE ( 'NONE', *, *, #76840, .T. ) ;
#17227 = ORIENTED_EDGE ( 'NONE', *, *, #17842, .F. ) ;
#17228 = CARTESIAN_POINT ( 'NONE',  ( 70.29209685856477563, -5.291415217122921177, 3.054999999999999272 ) ) ;
#17229 = VECTOR ( 'NONE', #77007, 1000.000000000000000 ) ;
#17230 = ORIENTED_EDGE ( 'NONE', *, *, #29375, .T. ) ;
#17231 = DIRECTION ( 'NONE',  ( -0.7071067811865487940, 0.7071067811865463515, 0.000000000000000000 ) ) ;
#17232 = AXIS2_PLACEMENT_3D ( 'NONE', #92735, #49980, #94163 ) ;
#17233 = CARTESIAN_POINT ( 'NONE',  ( 5.999999999999970690, 5.587461875839184522, 4.000000000000000000 ) ) ;
#17234 = CARTESIAN_POINT ( 'NONE',  ( 107.7712635252314328, 4.472830434245838482, 4.472830434245842035 ) ) ;
#17235 = DIRECTION ( 'NONE',  ( 0.7071067811865486830, -0.7071067811865464625, -0.000000000000000000 ) ) ;
#17236 = VECTOR ( 'NONE', #58386, 1000.000000000000000 ) ;
#17237 = CARTESIAN_POINT ( 'NONE',  ( -48.29974487139158867, -27.71228299555239971, 4.000000000000000000 ) ) ;
#17238 = DIRECTION ( 'NONE',  ( -0.6830127018922180770, -0.6830127018922204085, -0.2588190451025213501 ) ) ;
#17239 = DIRECTION ( 'NONE',  ( 0.7071067811865487940, -0.7071067811865463515, 0.000000000000000000 ) ) ;
#17240 = ADVANCED_FACE ( 'NONE', ( #126184 ), #26859, .F. ) ;
#17241 = LINE ( 'NONE', #48445, #90713 ) ;
#17242 = LINE ( 'NONE', #61505, #70703 ) ;
#17243 = EDGE_LOOP ( 'NONE', ( #36555, #2940, #78777 ) ) ;
#17244 = ADVANCED_FACE ( 'NONE', ( #83398 ), #29010, .F. ) ;
#17245 = PLANE ( 'NONE',  #50373 ) ;
#17247 = DIRECTION ( 'NONE',  ( 0.7071067811865487940, -0.7071067811865463515, 0.000000000000000000 ) ) ;
#17246 = VECTOR ( 'NONE', #89145, 999.9999999999998863 ) ;
#17248 = ORIENTED_EDGE ( 'NONE', *, *, #63682, .F. ) ;
#17249 = ORIENTED_EDGE ( 'NONE', *, *, #127836, .F. ) ;
#17250 = CARTESIAN_POINT ( 'NONE',  ( 113.6833603837962272, -2.130196079827426203, 7.949999999999996625 ) ) ;
#17251 = EDGE_LOOP ( 'NONE', ( #38518, #38764, #131382, #124818 ) ) ;
#17252 = LINE ( 'NONE', #20087, #97659 ) ;
#17253 = PLANE ( 'NONE',  #80241 ) ;
#17254 = LINE ( 'NONE', #83979, #120359 ) ;
#17255 = EDGE_CURVE ( 'NONE', #91102, #73050, #93556, .T. ) ;
#17256 = CARTESIAN_POINT ( 'NONE',  ( 17.35681257248251086, -20.24070752338407431, 21.22881796311217073 ) ) ;
#17257 = VERTEX_POINT ( 'NONE', #5791 ) ;
#17258 = CARTESIAN_POINT ( 'NONE',  ( 0.1121846519738732423, -51.37040454773215714, 37.49526731631105037 ) ) ;
#17259 = ORIENTED_EDGE ( 'NONE', *, *, #100147, .F. ) ;
#17260 = CARTESIAN_POINT ( 'NONE',  ( 6.541236474768552966, 0.000000000000000000, 7.934999999999990727 ) ) ;
#17261 = DIRECTION ( 'NONE',  ( -1.000000000000000000, -1.224606353822377258E-16, -0.000000000000000000 ) ) ;
#17262 = VECTOR ( 'NONE', #98922, 1000.000000000000000 ) ;
#17263 = CARTESIAN_POINT ( 'NONE',  ( 15.18398860626900237, 28.73617430169797871, 5.000000000000000000 ) ) ;
#17264 = VECTOR ( 'NONE', #134745, 1000.000000000000000 ) ;
#17265 = CARTESIAN_POINT ( 'NONE',  ( 11.47373016279025748, -8.505883529166709422, 4.231315693744567064 ) ) ;
#17266 = VERTEX_POINT ( 'NONE', #94954 ) ;
#17267 = ORIENTED_EDGE ( 'NONE', *, *, #21550, .T. ) ;
#17268 = ORIENTED_EDGE ( 'NONE', *, *, #54279, .F. ) ;
#17269 = DIRECTION ( 'NONE',  ( 0.000000000000000000, -1.000000000000000000, 0.000000000000000000 ) ) ;
#17270 = CARTESIAN_POINT ( 'NONE',  ( 18.29974487139159223, -27.71228299555219010, 4.000000000000000000 ) ) ;
#17271 = PLANE ( 'NONE',  #107502 ) ;
#17272 =( NAMED_UNIT ( * ) PLANE_ANGLE_UNIT ( ) SI_UNIT ( $, .RADIAN. ) );
#17273 = CARTESIAN_POINT ( 'NONE',  ( 12.18398860626900060, 28.73617430169795739, 5.000000000000000000 ) ) ;
#17274 = DIRECTION ( 'NONE',  ( 0.000000000000000000, -1.000000000000000000, 0.000000000000000000 ) ) ;
#17275 = VECTOR ( 'NONE', #48247, 1000.000000000000227 ) ;
#17276 = LINE ( 'NONE', #138352, #90228 ) ;
#17277 = CARTESIAN_POINT ( 'NONE',  ( 7.939999999999994174, -60.26999999999998892, -10.00000000000000178 ) ) ;
#17278 = CARTESIAN_POINT ( 'NONE',  ( 32.99451991528749062, 28.92564299267960948, 4.000000000000000000 ) ) ;
#17279 = EDGE_LOOP ( 'NONE', ( #114771, #115357, #61360, #52851 ) ) ;
#17280 = CARTESIAN_POINT ( 'NONE',  ( -12.64318742751729907, -20.24070752338407075, 21.22881796311209612 ) ) ;
#17281 = CARTESIAN_POINT ( 'NONE',  ( 0.000000000000000000, 12.25461709320620507, -10.07315571508697261 ) ) ;
#17282 = ORIENTED_EDGE ( 'NONE', *, *, #124140, .F. ) ;
#17283 = DIRECTION ( 'NONE',  ( 0.6830127018922181881, 0.6830127018922202975, -0.2588190451025214056 ) ) ;
#17285 = ORIENTED_EDGE ( 'NONE', *, *, #91486, .T. ) ;
#17284 = DIRECTION ( 'NONE',  ( 0.7071067811865486830, -0.7071067811865464625, -0.000000000000000000 ) ) ;
#17286 = LINE ( 'NONE', #138362, #102418 ) ;
#17287 = CARTESIAN_POINT ( 'NONE',  ( 104.8333333333333286, -6.884901960086287964, 3.974999999999998312 ) ) ;
#17288 = ORIENTED_EDGE ( 'NONE', *, *, #84605, .F. ) ;
#17289 = PLANE ( 'NONE',  #60523 ) ;
#17290 = UNCERTAINTY_MEASURE_WITH_UNIT (LENGTH_MEASURE( 1.000000000000000082E-05 ), #128184, 'distance_accuracy_value', 'NONE');
#17291 = ORIENTED_EDGE ( 'NONE', *, *, #26796, .T. ) ;
#17292 = CARTESIAN_POINT ( 'NONE',  ( 35.99451991528749772, 28.92564299267963079, 4.000000000000000000 ) ) ;
#17294 = EDGE_CURVE ( 'NONE', #139679, #92329, #14563, .T. ) ;
#17293 = CARTESIAN_POINT ( 'NONE',  ( 122.4333603837962130, 2.130196079827431532, -7.949999999999997513 ) ) ;
#17295 = CARTESIAN_POINT ( 'NONE',  ( 20.29289321881332242, -15.74070752338412049, 5.000000000000000000 ) ) ;
#17296 = DIRECTION ( 'NONE',  ( 0.7071067811865487940, 0.7071067811865463515, 0.000000000000000000 ) ) ;
#17297 = ADVANCED_FACE ( 'NONE', ( #61662 ), #27555, .F. ) ;
#17298 = EDGE_CURVE ( 'NONE', #140272, #29472, #139222, .T. ) ;
#17299 = DIRECTION ( 'NONE',  ( -0.7071067811865486830, -0.7071067811865464625, 0.000000000000000000 ) ) ;
#17300 = PLANE ( 'NONE',  #61075 ) ;
#17301 = EDGE_CURVE ( 'NONE', #86059, #34296, #92827, .T. ) ;
#17302 = CARTESIAN_POINT ( 'NONE',  ( 39.48921356237310221, -27.52281430457082934, 5.000000000000000000 ) ) ;
#17303 = CARTESIAN_POINT ( 'NONE',  ( 0.1458333333333333981, -1.633150327867689988, 6.094999999999989981 ) ) ;
#17304 = CARTESIAN_POINT ( 'NONE',  ( 9.312069808101886892, 7.934999999999992504, 2.126176841940951689 ) ) ;
#17305 = LINE ( 'NONE', #26057, #66755 ) ;
#17307 = ADVANCED_FACE ( 'NONE', ( #39918 ), #128338, .F. ) ;
#17306 = LINE ( 'NONE', #17985, #112679 ) ;
#17308 = VERTEX_POINT ( 'NONE', #47941 ) ;
#17309 = VECTOR ( 'NONE', #47081, 1000.000000000000000 ) ;
#17310 = ORIENTED_EDGE ( 'NONE', *, *, #8258, .T. ) ;
#17311 = CARTESIAN_POINT ( 'NONE',  ( 83.83333333333332860, -6.884901960086287964, 3.974999999999998312 ) ) ;
#17312 = LINE ( 'NONE', #118761, #111501 ) ;
#17313 = ORIENTED_EDGE ( 'NONE', *, *, #1762, .T. ) ;
#17314 = EDGE_CURVE ( 'NONE', #43657, #70215, #37024, .T. ) ;
#17315 = FACE_OUTER_BOUND ( 'NONE', #92051, .T. ) ;
#17316 = CARTESIAN_POINT ( 'NONE',  ( -12.20000000000000284, -35.14999999999999147, -39.50000000000000000 ) ) ;
#17317 = DIRECTION ( 'NONE',  ( 0.6830127018922181881, 0.6830127018922202975, -0.2588190451025214056 ) ) ;
#17318 = ORIENTED_EDGE ( 'NONE', *, *, #137828, .F. ) ;
#17319 = CARTESIAN_POINT ( 'NONE',  ( 8.293207492759204769, 20.25929247661551358, 20.83292124670812839 ) ) ;
#17320 = CARTESIAN_POINT ( 'NONE',  ( -21.33010218547252279, 17.25929247661553845, 19.83885114516075987 ) ) ;
#17321 = EDGE_CURVE ( 'NONE', #123762, #13717, #53629, .T. ) ;
#17322 = CARTESIAN_POINT ( 'NONE',  ( 34.49999999999975842, 15.43112307739203004, 4.000000000000000000 ) ) ;
#17323 = DIRECTION ( 'NONE',  ( 0.7071067811865486830, -0.7071067811865464625, -0.000000000000000000 ) ) ;
#17324 = EDGE_CURVE ( 'NONE', #28047, #108474, #62367, .T. ) ;
#17325 = LINE ( 'NONE', #71026, #74854 ) ;
#17326 = FACE_OUTER_BOUND ( 'NONE', #125456, .T. ) ;
#17327 = SURFACE_STYLE_FILL_AREA ( #60890 ) ;
#17328 = CARTESIAN_POINT ( 'NONE',  ( -2.510786437626908008, -27.52281430457053446, 5.000000000000000000 ) ) ;
#17329 = CARTESIAN_POINT ( 'NONE',  ( 2.483345613589531542, 22.22500000000000142, 4.500000000000000888 ) ) ;
#17330 = DIRECTION ( 'NONE',  ( 0.7071067811865486830, -0.7071067811865464625, -0.000000000000000000 ) ) ;
#17331 = LINE ( 'NONE', #3574, #123981 ) ;
#17332 = EDGE_CURVE ( 'NONE', #1839, #55182, #31167, .T. ) ;
#17333 = DIRECTION ( 'NONE',  ( -0.000000000000000000, -0.3543493200069152693, 0.9351131265310292928 ) ) ;
#17334 = VECTOR ( 'NONE', #26612, 1000.000000000000000 ) ;
#17335 = VERTEX_POINT ( 'NONE', #8627 ) ;
#17336 = VERTEX_POINT ( 'NONE', #131898 ) ;
#17337 = CARTESIAN_POINT ( 'NONE',  ( 98.72959685856478984, -6.110000000000000320, -1.637169565754161393 ) ) ;
#17338 = ORIENTED_EDGE ( 'NONE', *, *, #55299, .F. ) ;
#17339 = AXIS2_PLACEMENT_3D ( 'NONE', #78147, #89033, #99883 ) ;
#17340 = DIRECTION ( 'NONE',  ( 0.3543493200069162685, -0.000000000000000000, -0.9351131265310288487 ) ) ;
#17341 = CARTESIAN_POINT ( 'NONE',  ( -17.70025512860841488, -27.71228299555193786, 4.000000000000000000 ) ) ;
#17342 = EDGE_LOOP ( 'NONE', ( #29275, #2980, #20814, #27365 ) ) ;
#17343 = CARTESIAN_POINT ( 'NONE',  ( 75.52083333333332860, 7.949999999999998401, 2.130196079827431532 ) ) ;
#17344 = DIRECTION ( 'NONE',  ( 0.7071067811865487940, 0.7071067811865463515, 0.000000000000000000 ) ) ;
#17345 = CARTESIAN_POINT ( 'NONE',  ( 91.64126352523143737, 4.472830434245836706, 4.472830434245840259 ) ) ;
#17346 = VECTOR ( 'NONE', #135691, 1000.000000000000000 ) ;
#17347 = ORIENTED_EDGE ( 'NONE', *, *, #84683, .F. ) ;
#17348 = FACE_OUTER_BOUND ( 'NONE', #48317, .T. ) ;
#17349 = ORIENTED_EDGE ( 'NONE', *, *, #23989, .T. ) ;
#17351 = EDGE_CURVE ( 'NONE', #119366, #83686, #119549, .T. ) ;
#17350 = CARTESIAN_POINT ( 'NONE',  ( 22.04515773336653695, -21.74070752338405654, 21.72585301388589585 ) ) ;
#17352 = DIRECTION ( 'NONE',  ( 0.7071067811865486830, -0.7071067811865464625, -0.000000000000000000 ) ) ;
#17353 = FACE_OUTER_BOUND ( 'NONE', #142231, .T. ) ;
#17354 = DIRECTION ( 'NONE',  ( -0.6830127018922180770, -0.6830127018922204085, -0.2588190451025213501 ) ) ;
#17355 = ORIENTED_EDGE ( 'NONE', *, *, #25732, .T. ) ;
#17356 = ORIENTED_EDGE ( 'NONE', *, *, #51219, .F. ) ;
#17357 = EDGE_LOOP ( 'NONE', ( #72681, #129649, #25397, #91221 ) ) ;
#17358 = DIRECTION ( 'NONE',  ( -0.3543493200069162685, -0.000000000000000000, -0.9351131265310288487 ) ) ;
#17359 = DIRECTION ( 'NONE',  ( 0.7071067811865487940, 0.7071067811865463515, 0.000000000000000000 ) ) ;
#17360 = CARTESIAN_POINT ( 'NONE',  ( 11.44206980810188767, 7.934999999999992504, 2.126176841940951689 ) ) ;
#17361 = DIRECTION ( 'NONE',  ( 0.7071067811865487940, 0.7071067811865463515, -0.000000000000000000 ) ) ;
#17362 = VECTOR ( 'NONE', #43199, 1000.000000000000000 ) ;
#17364 = AXIS2_PLACEMENT_3D ( 'NONE', #93752, #6688, #72768 ) ;
#17363 = FILL_AREA_STYLE_COLOUR ( '', #23755 ) ;
#17365 = PRESENTATION_LAYER_ASSIGNMENT (  '', '', ( #89104 ) ) ;
#17366 = VERTEX_POINT ( 'NONE', #109419 ) ;
#17368 = EDGE_LOOP ( 'NONE', ( #45009, #388, #78434, #128650 ) ) ;
#17367 = MECHANICAL_DESIGN_GEOMETRIC_PRESENTATION_REPRESENTATION (  '', ( #105422 ), #84560 ) ;
#17369 = CARTESIAN_POINT ( 'NONE',  ( 50.99451991528749062, 28.92564299267973738, 4.000000000000000000 ) ) ;
#17371 = ORIENTED_EDGE ( 'NONE', *, *, #98286, .F. ) ;
#17370 = EDGE_CURVE ( 'NONE', #36339, #88739, #73244, .T. ) ;
#17372 = EDGE_LOOP ( 'NONE', ( #63428, #64168, #113003, #82662 ) ) ;
#17373 = CARTESIAN_POINT ( 'NONE',  ( 115.9954301918981230, 5.291415217122916737, 3.055000000000001936 ) ) ;
#17374 = DIRECTION ( 'NONE',  ( -1.000000000000000000, -0.000000000000000000, -0.000000000000000000 ) ) ;
#17375 = DIRECTION ( 'NONE',  ( 0.7071067811865487940, -0.7071067811865463515, 0.000000000000000000 ) ) ;
#17376 = ORIENTED_EDGE ( 'NONE', *, *, #48645, .T. ) ;
#17377 = CARTESIAN_POINT ( 'NONE',  ( -2.207106781186530586, 6.759292476615651246, 5.000000000000000000 ) ) ;
#17378 = EDGE_CURVE ( 'NONE', #55777, #137620, #52870, .T. ) ;
#17379 = DIRECTION ( 'NONE',  ( -1.000000000000000000, -1.224606353822377258E-16, -0.000000000000000000 ) ) ;
#17380 = DIRECTION ( 'NONE',  ( 1.000000000000000000, 0.000000000000000000, 0.000000000000000000 ) ) ;
#17381 = DIRECTION ( 'NONE',  ( 0.3543493200069162685, -0.000000000000000000, -0.9351131265310288487 ) ) ;
#17382 = ORIENTED_EDGE ( 'NONE', *, *, #104405, .T. ) ;
#17383 = DIRECTION ( 'NONE',  ( 0.7071067811865487940, 0.7071067811865463515, 0.000000000000000000 ) ) ;
#17384 = FACE_BOUND ( 'NONE', #6648, .T. ) ;
#17385 = EDGE_LOOP ( 'NONE', ( #85166, #3643, #66790, #43738 ) ) ;
#17386 = CARTESIAN_POINT ( 'NONE',  ( 25.40000000000000568, -0.2953647482591277851, -7.939948287776192437 ) ) ;
#17388 = EDGE_CURVE ( 'NONE', #34870, #22742, #10101, .T. ) ;
#17387 = DIRECTION ( 'NONE',  ( 0.3543493200069162685, -0.000000000000000000, -0.9351131265310288487 ) ) ;
#17389 = EDGE_LOOP ( 'NONE', ( #85050, #128031, #82158, #142943 ) ) ;
#17390 = DIRECTION ( 'NONE',  ( -0.000000000000000000, 0.3543493200069153248, 0.9351131265310292928 ) ) ;
#17391 = EDGE_LOOP ( 'NONE', ( #7499, #141154, #55044, #10523, #2557, #95487 ) ) ;
#17392 = ORIENTED_EDGE ( 'NONE', *, *, #26645, .F. ) ;
#17393 = ORIENTED_EDGE ( 'NONE', *, *, #88418, .F. ) ;
#17394 = CARTESIAN_POINT ( 'NONE',  ( 32.28709685856477307, 3.054999999999997495, 5.291415217122919401 ) ) ;
#17395 = EDGE_LOOP ( 'NONE', ( #32486, #41347, #130300, #99301 ) ) ;
#17396 = CARTESIAN_POINT ( 'NONE',  ( 2.292893218813435219, 14.25929247661557753, 5.000000000000000000 ) ) ;
#17397 = CARTESIAN_POINT ( 'NONE',  ( 6.639999999999984581, -40.42999999999999972, -40.00000000000000000 ) ) ;
#17398 = DIRECTION ( 'NONE',  ( -0.000000000000000000, -0.3543493200069152693, 0.9351131265310292928 ) ) ;
#17399 = CARTESIAN_POINT ( 'NONE',  ( 20.66840764549667497, 9.139736423841732040E-16, 0.000000000000000000 ) ) ;
#17400 = CARTESIAN_POINT ( 'NONE',  ( 5.538396446294259867, -9.740707523384180888, 17.74957260769611977 ) ) ;
#17401 = LINE ( 'NONE', #96360, #12514 ) ;
#17402 = CARTESIAN_POINT ( 'NONE',  ( -11.99999999999991296, 4.384688058510558761, -7.090945410444713382 ) ) ;
#17403 = LINE ( 'NONE', #126865, #143221 ) ;
#17404 = EDGE_CURVE ( 'NONE', #119665, #68775, #141330, .T. ) ;
#17405 = CARTESIAN_POINT ( 'NONE',  ( -34.42499999999997584, -22.26999999999999247, -40.00000000000000000 ) ) ;
#17406 = EDGE_CURVE ( 'NONE', #69796, #35696, #96365, .T. ) ;
#17407 = EDGE_LOOP ( 'NONE', ( #91509, #91597, #87698, #34911 ) ) ;
#17408 = ORIENTED_EDGE ( 'NONE', *, *, #59702, .F. ) ;
#17409 = ORIENTED_EDGE ( 'NONE', *, *, #112715, .F. ) ;
#17410 = EDGE_LOOP ( 'NONE', ( #57733, #38206, #79653, #2870, #40043 ) ) ;
#17411 = DIRECTION ( 'NONE',  ( -0.3543493200069162685, -0.000000000000000000, -0.9351131265310288487 ) ) ;
#17412 = ORIENTED_EDGE ( 'NONE', *, *, #31217, .F. ) ;
#17413 =( BOUNDED_CURVE ( )  B_SPLINE_CURVE ( 3, ( #36351, #46557, #79174, #13131 ),
 .UNSPECIFIED., .F., .F. ) 
 B_SPLINE_CURVE_WITH_KNOTS ( ( 4, 4 ),
 ( 2.001653308786169649, 3.503810798801450854 ),
 .UNSPECIFIED. ) 
 CURVE ( )  GEOMETRIC_REPRESENTATION_ITEM ( )  RATIONAL_B_SPLINE_CURVE ( ( 1.000000000000000000, 0.8206354192515240564, 0.8206354192515240564, 1.000000000000000000 ) ) 
 REPRESENTATION_ITEM ( '' )  );
#17414 = VERTEX_POINT ( 'NONE', #42766 ) ;
#17415 = CARTESIAN_POINT ( 'NONE',  ( -27.18398860626900060, 28.73617430169806042, 5.000000000000000000 ) ) ;
#17416 = CARTESIAN_POINT ( 'NONE',  ( 11.51078643762690490, -27.52281430457047406, 5.000000000000000000 ) ) ;
#17417 = EDGE_CURVE ( 'NONE', #4524, #75885, #95681, .T. ) ;
#17418 = EDGE_CURVE ( 'NONE', #71117, #49830, #73940, .T. ) ;
#17419 = DIRECTION ( 'NONE',  ( 1.000000000000000000, 0.000000000000000000, 0.000000000000000000 ) ) ;
#17420 = ORIENTED_EDGE ( 'NONE', *, *, #45777, .T. ) ;
#17421 = DIRECTION ( 'NONE',  ( 1.000000000000000000, 0.000000000000000000, 0.000000000000000000 ) ) ;
#17422 = ORIENTED_EDGE ( 'NONE', *, *, #105538, .F. ) ;
#17423 = CARTESIAN_POINT ( 'NONE',  ( 5.207106781186515931, 6.759292476615653023, 5.000000000000000000 ) ) ;
#17424 = VECTOR ( 'NONE', #103271, 1000.000000000000000 ) ;
#17425 = PLANE ( 'NONE',  #91386 ) ;
#17426 = CARTESIAN_POINT ( 'NONE',  ( 7.358736474768553748, 5.808823158059031044, -5.808823158059038150 ) ) ;
#17427 = ORIENTED_EDGE ( 'NONE', *, *, #41221, .T. ) ;
#17429 = CARTESIAN_POINT ( 'NONE',  ( 55.18164086290604331, -52.14999999999999147, 41.64499999999997470 ) ) ;
#17428 = CARTESIAN_POINT ( 'NONE',  ( 101.1204301918981230, 3.055000000000002380, -5.291415217122917625 ) ) ;
#17430 = VECTOR ( 'NONE', #83724, 1000.000000000000000 ) ;
#17431 = LINE ( 'NONE', #82710, #62896 ) ;
#17432 = CARTESIAN_POINT ( 'NONE',  ( 13.29826936130429260, 0.000000000000000000, 2.500000000000000444 ) ) ;
#17433 = ORIENTED_EDGE ( 'NONE', *, *, #21110, .F. ) ;
#17434 = ORIENTED_EDGE ( 'NONE', *, *, #139883, .F. ) ;
#17435 = LINE ( 'NONE', #61692, #12593 ) ;
#17436 = VERTEX_POINT ( 'NONE', #98540 ) ;
#17437 = CARTESIAN_POINT ( 'NONE',  ( -2.282422613574296655, -21.73023691814492153, 5.000000000000000888 ) ) ;
#17438 = LINE ( 'NONE', #82034, #29165 ) ;
#17439 = FACE_OUTER_BOUND ( 'NONE', #60965, .T. ) ;
#17440 = DIRECTION ( 'NONE',  ( -0.7071067811865486830, -0.7071067811865464625, 0.000000000000000000 ) ) ;
#17441 = EDGE_CURVE ( 'NONE', #67004, #102793, #28626, .T. ) ;
#17442 = ORIENTED_EDGE ( 'NONE', *, *, #86746, .T. ) ;
#17443 = LINE ( 'NONE', #126221, #8889 ) ;
#17444 = AXIS2_PLACEMENT_3D ( 'NONE', #123235, #112341, #134835 ) ;
#17445 = CARTESIAN_POINT ( 'NONE',  ( 34.92499999999998295, -19.48753812416032716, 4.000000000000000000 ) ) ;
#17446 = LINE ( 'NONE', #5111, #19054 ) ;
#17447 = VERTEX_POINT ( 'NONE', #142078 ) ;
#17448 = DIRECTION ( 'NONE',  ( 0.6830127018922181881, 0.6830127018922202975, -0.2588190451025214056 ) ) ;
#17449 = DIRECTION ( 'NONE',  ( 0.5735764363510444941, 0.8191520442889929088, 0.000000000000000000 ) ) ;
#17450 = ORIENTED_EDGE ( 'NONE', *, *, #39835, .F. ) ;
#17452 = ORIENTED_EDGE ( 'NONE', *, *, #18592, .F. ) ;
#17451 = CARTESIAN_POINT ( 'NONE',  ( 0.2153679725188837879, -51.67626207039724306, -38.40320453011149482 ) ) ;
#17453 = VERTEX_POINT ( 'NONE', #140607 ) ;
#17454 = PRESENTATION_STYLE_ASSIGNMENT (( #50821 ) ) ;
#17455 = EDGE_LOOP ( 'NONE', ( #100788, #121878, #89319, #128322, #92643 ) ) ;
#17456 = CARTESIAN_POINT ( 'NONE',  ( 25.39999999999999858, -57.15000000000008384, -34.92499999999998295 ) ) ;
#17457 = UNCERTAINTY_MEASURE_WITH_UNIT (LENGTH_MEASURE( 1.000000000000000082E-05 ), #68939, 'distance_accuracy_value', 'NONE');
#17458 = EDGE_CURVE ( 'NONE', #72549, #14195, #29698, .T. ) ;
#17459 = CARTESIAN_POINT ( 'NONE',  ( 20.65000000000000213, 0.000000000000000000, 0.000000000000000000 ) ) ;
#17461 = ADVANCED_FACE ( 'NONE', ( #19551 ), #129023, .F. ) ;
#17460 = VECTOR ( 'NONE', #66042, 1000.000000000000227 ) ;
#17462 = FACE_OUTER_BOUND ( 'NONE', #23496, .T. ) ;
#17463 = CIRCLE ( 'NONE', #68529, 4.607329295533711289 ) ;
#17464 = DIRECTION ( 'NONE',  ( -1.000000000000000000, -1.224606353822377258E-16, -0.000000000000000000 ) ) ;
#17465 = EDGE_CURVE ( 'NONE', #108894, #31809, #20970, .T. ) ;
#17466 = CARTESIAN_POINT ( 'NONE',  ( 0.000000000000000000, 0.000000000000000000, 5.000000000000000000 ) ) ;
#17467 = FACE_OUTER_BOUND ( 'NONE', #74599, .T. ) ;
#17468 = LINE ( 'NONE', #61039, #141583 ) ;
#17469 = DIRECTION ( 'NONE',  ( -0.7071067811865486830, 0.7071067811865464625, 0.000000000000000000 ) ) ;
#17470 = LINE ( 'NONE', #105885, #118398 ) ;
#17471 = PLANE ( 'NONE',  #78445 ) ;
#17472 = VECTOR ( 'NONE', #43883, 1000.000000000000000 ) ;
#17473 = FACE_OUTER_BOUND ( 'NONE', #134269, .T. ) ;
#17475 = EDGE_CURVE ( 'NONE', #107725, #104096, #121110, .T. ) ;
#17474 = LINE ( 'NONE', #61729, #140317 ) ;
#17477 = ADVANCED_FACE ( 'NONE', ( #107268 ), #31865, .F. ) ;
#17476 = VERTEX_POINT ( 'NONE', #18085 ) ;
#17478 = ORIENTED_EDGE ( 'NONE', *, *, #128627, .T. ) ;
#17479 = VERTEX_POINT ( 'NONE', #85501 ) ;
#17480 = CARTESIAN_POINT ( 'NONE',  ( 111.1041666666666714, 2.130196079827422206, 7.950000000000001954 ) ) ;
#17481 = ORIENTED_EDGE ( 'NONE', *, *, #69953, .T. ) ;
#17482 = ORIENTED_EDGE ( 'NONE', *, *, #20259, .F. ) ;
#17483 = ORIENTED_EDGE ( 'NONE', *, *, #106004, .T. ) ;
#17484 = DIRECTION ( 'NONE',  ( 1.000000000000000000, 0.000000000000000000, 0.000000000000000000 ) ) ;
#17485 = VERTEX_POINT ( 'NONE', #23087 ) ;
#17486 = CARTESIAN_POINT ( 'NONE',  ( 16.61159235450331906, 9.902892378096218942E-16, 0.000000000000000000 ) ) ;
#17487 = FACE_OUTER_BOUND ( 'NONE', #50689, .T. ) ;
#17488 = EDGE_CURVE ( 'NONE', #38637, #72848, #134782, .T. ) ;
#17489 = CARTESIAN_POINT ( 'NONE',  ( -36.18398860626899705, 28.73617430169812437, 5.000000000000000000 ) ) ;
#17490 = DIRECTION ( 'NONE',  ( -1.000000000000000000, -1.224606353822377258E-16, -0.000000000000000000 ) ) ;
#17491 = CARTESIAN_POINT ( 'NONE',  ( 106.8962635252314328, 4.472830434245840259, -4.472830434245839371 ) ) ;
#17492 = ORIENTED_EDGE ( 'NONE', *, *, #128472, .F. ) ;
#17493 = ADVANCED_FACE ( 'NONE', ( #122424 ), #12943, .T. ) ;
#17494 = CARTESIAN_POINT ( 'NONE',  ( -8.396172048266301147, 10.44511258719185953, -28.53519072974560800 ) ) ;
#17495 = CARTESIAN_POINT ( 'NONE',  ( 3.489213562373097322, -27.52281430457057709, 5.000000000000000000 ) ) ;
#17496 = DIRECTION ( 'NONE',  ( 1.000000000000000000, 0.000000000000000000, 0.000000000000000000 ) ) ;
#17497 = FACE_BOUND ( 'NONE', #111787, .T. ) ;
#17498 = DIRECTION ( 'NONE',  ( -0.6830127018922181881, 0.6830127018922202975, -0.2588190451025214056 ) ) ;
#17499 = SURFACE_SIDE_STYLE ('',( #84905 ) ) ;
#17500 = CARTESIAN_POINT ( 'NONE',  ( 40.32919371712954870, -3.975000000000001865, 6.884901960086284411 ) ) ;
#17501 = EDGE_CURVE ( 'NONE', #81904, #63910, #33337, .T. ) ;
#17502 = CARTESIAN_POINT ( 'NONE',  ( 45.48921356237309510, -27.52281430457087197, 5.000000000000000000 ) ) ;
#17503 = CARTESIAN_POINT ( 'NONE',  ( 25.49999999999982947, 10.46639925780215208, 5.000000000000000000 ) ) ;
#17504 = ORIENTED_EDGE ( 'NONE', *, *, #140821, .F. ) ;
#17505 = EDGE_LOOP ( 'NONE', ( #267, #15186, #114321, #87575 ) ) ;
#17506 = CARTESIAN_POINT ( 'NONE',  ( 127.4587635252314470, 0.000000000000000000, -6.110000000000001208 ) ) ;
#17507 = EDGE_LOOP ( 'NONE', ( #29832, #13112, #140233, #40422 ) ) ;
#17508 = PLANE ( 'NONE',  #140924 ) ;
#17509 = CARTESIAN_POINT ( 'NONE',  ( 34.42499999999998295, 0.000000000000000000, 4.500000000000000888 ) ) ;
#17510 = ADVANCED_FACE ( 'NONE', ( #643 ), #11494, .F. ) ;
#17511 = CARTESIAN_POINT ( 'NONE',  ( 18.70710678118641113, -6.740707523384205757, 5.000000000000000000 ) ) ;
#17512 = DIRECTION ( 'NONE',  ( -0.000000000000000000, -0.000000000000000000, 1.000000000000000000 ) ) ;
#17513 = CARTESIAN_POINT ( 'NONE',  ( 27.85459685856477208, -1.637169565754161615, 6.110000000000000320 ) ) ;
#17514 = ORIENTED_EDGE ( 'NONE', *, *, #95909, .T. ) ;
#17515 = CARTESIAN_POINT ( 'NONE',  ( 35.99451991528749772, 28.92564299267963079, 4.000000000000000000 ) ) ;
#17516 = ORIENTED_EDGE ( 'NONE', *, *, #100401, .F. ) ;
#17517 = EDGE_CURVE ( 'NONE', #114247, #75689, #34730, .T. ) ;
#17518 = DIRECTION ( 'NONE',  ( 0.000000000000000000, 1.000000000000000000, 0.000000000000000000 ) ) ;
#17519 = CARTESIAN_POINT ( 'NONE',  ( 4.499999999999966249, -19.53360074219753884, 5.000000000000000000 ) ) ;
#17520 = CARTESIAN_POINT ( 'NONE',  ( -11.70025512860841133, -27.71228299555198049, 4.000000000000000000 ) ) ;
#17521 = FACE_OUTER_BOUND ( 'NONE', #21105, .T. ) ;
#17522 = ORIENTED_EDGE ( 'NONE', *, *, #82608, .T. ) ;
#17523 = CARTESIAN_POINT ( 'NONE',  ( 57.31293019189811133, -1.637169565754159617, -6.110000000000001208 ) ) ;
#17524 = EDGE_LOOP ( 'NONE', ( #93835, #26509, #77809, #133429 ) ) ;
#17525 = PLANE ( 'NONE',  #95647 ) ;
#17526 = CARTESIAN_POINT ( 'NONE',  ( -18.48921356237309510, -27.52281430457068367, 5.000000000000000000 ) ) ;
#17527 = DIRECTION ( 'NONE',  ( -0.000000000000000000, -0.000000000000000000, 1.000000000000000000 ) ) ;
#17528 = ADVANCED_FACE ( 'NONE', ( #57219 ), #101396, .F. ) ;
#17529 = EDGE_CURVE ( 'NONE', #80972, #133165, #123176, .T. ) ;
#17530 = LINE ( 'NONE', #52303, #34521 ) ;
#17531 = EDGE_CURVE ( 'NONE', #50205, #75083, #112295, .T. ) ;
#17532 = VECTOR ( 'NONE', #107050, 999.9999999999998863 ) ;
#17533 = CARTESIAN_POINT ( 'NONE',  ( 45.70376352523145158, 6.109999999999998543, 1.122388791418548911E-15 ) ) ;
#17534 = ORIENTED_EDGE ( 'NONE', *, *, #71106, .T. ) ;
#17535 = AXIS2_PLACEMENT_3D ( 'NONE', #2351, #79992, #111120 ) ;
#17536 = CARTESIAN_POINT ( 'NONE',  ( -34.49999999999975131, 13.56627193232212392, -10.57019076586076700 ) ) ;
#17537 = ORIENTED_EDGE ( 'NONE', *, *, #2032, .F. ) ;
#17538 = ORIENTED_EDGE ( 'NONE', *, *, #126161, .F. ) ;
#17539 = CARTESIAN_POINT ( 'NONE',  ( -19.28515664589289003, 1.196650378695325090, -30.59010235425025215 ) ) ;
#17540 = VERTEX_POINT ( 'NONE', #44186 ) ;
#17541 = DIRECTION ( 'NONE',  ( 0.6830127018922180770, -0.6830127018922204085, -0.2588190451025214056 ) ) ;
#17542 = VERTEX_POINT ( 'NONE', #111561 ) ;
#17543 = CARTESIAN_POINT ( 'NONE',  ( 17.72082203615853047, 8.995094813919580545, 4.338987337627234098 ) ) ;
#17544 = FACE_OUTER_BOUND ( 'NONE', #97678, .T. ) ;
#17545 = FACE_BOUND ( 'NONE', #67227, .T. ) ;
#17546 = LINE ( 'NONE', #94399, #103505 ) ;
#17547 =( NAMED_UNIT ( * ) PLANE_ANGLE_UNIT ( ) SI_UNIT ( $, .RADIAN. ) );
#17548 = FACE_OUTER_BOUND ( 'NONE', #35933, .T. ) ;
#17549 = VERTEX_POINT ( 'NONE', #99981 ) ;
#17551 = ORIENTED_EDGE ( 'NONE', *, *, #87257, .T. ) ;
#17550 = DIRECTION ( 'NONE',  ( 0.7071067811865487940, 0.7071067811865463515, 0.000000000000000000 ) ) ;
#17552 = ORIENTED_EDGE ( 'NONE', *, *, #60039, .T. ) ;
#17553 = CARTESIAN_POINT ( 'NONE',  ( -29.99999999999979039, 11.96639925780214320, 5.000000000000000000 ) ) ;
#17554 = AXIS2_PLACEMENT_3D ( 'NONE', #7697, #141821, #131651 ) ;
#17555 = ORIENTED_EDGE ( 'NONE', *, *, #42680, .F. ) ;
#17556 = COLOUR_RGB ( '', 0.72549020, 0.75294118, 0.79215686) ;
#17557 = CARTESIAN_POINT ( 'NONE',  ( 53.57876352523144448, -7.482591942790325086E-16, 6.109999999999998543 ) ) ;
#17558 = ORIENTED_EDGE ( 'NONE', *, *, #70265, .F. ) ;
#17559 = AXIS2_PLACEMENT_3D ( 'NONE', #27596, #59556, #103712 ) ;
#17560 = DIRECTION ( 'NONE',  ( 0.6830127018922181881, 0.6830127018922202975, -0.2588190451025214056 ) ) ;
#17561 = VECTOR ( 'NONE', #77624, 1000.000000000000000 ) ;
#17562 = CARTESIAN_POINT ( 'NONE',  ( 63.18398860626900415, 28.73617430169831621, 5.000000000000000000 ) ) ;
#17563 = ORIENTED_EDGE ( 'NONE', *, *, #56667, .F. ) ;
#17564 = PLANE ( 'NONE',  #39868 ) ;
#17565 = PRESENTATION_LAYER_ASSIGNMENT (  '', '', ( #121772 ) ) ;
#17566 = PLANE ( 'NONE',  #29322 ) ;
#17567 = CARTESIAN_POINT ( 'NONE',  ( 14.85700540165866634, 7.427722529079420433, 4.951096321256156507 ) ) ;
#17568 = CARTESIAN_POINT ( 'NONE',  ( 12.48921356237309155, -27.52281430457064104, 5.000000000000000000 ) ) ;
#17569 = FACE_OUTER_BOUND ( 'NONE', #72878, .T. ) ;
#17570 = CARTESIAN_POINT ( 'NONE',  ( -11.81601139373100651, 28.73617430169779041, 5.000000000000000000 ) ) ;
#17571 = ORIENTED_EDGE ( 'NONE', *, *, #48167, .T. ) ;
#17572 = ORIENTED_EDGE ( 'NONE', *, *, #96871, .T. ) ;
#17573 = DIRECTION ( 'NONE',  ( -0.7071067811865486830, -0.7071067811865464625, 0.000000000000000000 ) ) ;
#17574 = CARTESIAN_POINT ( 'NONE',  ( 15.18079593298623564, 2.055000000000001048, 0.000000000000000000 ) ) ;
#17575 = ORIENTED_EDGE ( 'NONE', *, *, #63992, .F. ) ;
#17576 = EDGE_LOOP ( 'NONE', ( #8261, #73218, #33340, #26233 ) ) ;
#17577 = ORIENTED_EDGE ( 'NONE', *, *, #3843, .T. ) ;
#17578 = CARTESIAN_POINT ( 'NONE',  ( 18.48921356237309510, -27.52281430457068367, 5.000000000000000000 ) ) ;
#17579 = EDGE_CURVE ( 'NONE', #114619, #18858, #66645, .T. ) ;
#17580 = EDGE_CURVE ( 'NONE', #14634, #123707, #44936, .T. ) ;
#17581 = CARTESIAN_POINT ( 'NONE',  ( -22.49999999999984368, 12.43112307739206024, 4.000000000000000000 ) ) ;
#17582 = ORIENTED_EDGE ( 'NONE', *, *, #71832, .F. ) ;
#17583 = CARTESIAN_POINT ( 'NONE',  ( 32.99999999999977973, 17.96639925780207747, 5.000000000000000000 ) ) ;
#17584 = CARTESIAN_POINT ( 'NONE',  ( 5.462903141435219823, -3.967499999999994476, 6.871911579029513106 ) ) ;
#17585 = LINE ( 'NONE', #137975, #142134 ) ;
#17586 = ORIENTED_EDGE ( 'NONE', *, *, #112507, .T. ) ;
#17587 = DIRECTION ( 'NONE',  ( 0.000000000000000000, 0.000000000000000000, 1.000000000000000000 ) ) ;
#17588 = ADVANCED_FACE ( 'NONE', ( #21701 ), #110114, .T. ) ;
#17589 = CARTESIAN_POINT ( 'NONE',  ( -44.99451991528749772, 28.92564299267969474, 4.000000000000000000 ) ) ;
#17590 = CARTESIAN_POINT ( 'NONE',  ( 25.40000000000000568, -6.088644610809077484, -0.2782657062331916342 ) ) ;
#17592 = EDGE_LOOP ( 'NONE', ( #108958, #127486, #13314, #26622 ) ) ;
#17591 = DIRECTION ( 'NONE',  ( 0.6830127018922180770, -0.6830127018922204085, -0.2588190451025213501 ) ) ;
#17593 = AXIS2_PLACEMENT_3D ( 'NONE', #20707, #19295, #119302 ) ;
#17594 = PLANE ( 'NONE',  #3035 ) ;
#17595 = ORIENTED_EDGE ( 'NONE', *, *, #116380, .T. ) ;
#17596 = CARTESIAN_POINT ( 'NONE',  ( 0.000000000000000000, 0.000000000000000000, 5.000000000000000000 ) ) ;
#17597 = CARTESIAN_POINT ( 'NONE',  ( 15.83159235450332147, -2.500000000000000000, 3.061616997868384127E-16 ) ) ;
#17598 = CARTESIAN_POINT ( 'NONE',  ( 108.9166666666666572, -6.884901960086287076, -3.975000000000000977 ) ) ;
#17599 = EDGE_CURVE ( 'NONE', #28471, #116082, #55059, .T. ) ;
#17600 = EDGE_LOOP ( 'NONE', ( #92171, #33463, #48996, #124004 ) ) ;
#17601 = DIRECTION ( 'NONE',  ( -0.7071067811865486830, 0.7071067811865464625, 0.000000000000000000 ) ) ;
#17602 = CYLINDRICAL_SURFACE ( 'NONE', #44150, 9.500000000000001776 ) ;
#17603 = DIRECTION ( 'NONE',  ( 0.7071067811865486830, -0.7071067811865464625, -0.000000000000000000 ) ) ;
#17604 = ORIENTED_EDGE ( 'NONE', *, *, #12866, .T. ) ;
#17605 = EDGE_CURVE ( 'NONE', #49860, #64348, #34024, .T. ) ;
#17606 = DIRECTION ( 'NONE',  ( -1.000000000000000000, -1.224606353822377258E-16, -0.000000000000000000 ) ) ;
#17607 = LINE ( 'NONE', #140144, #123470 ) ;
#17608 = CARTESIAN_POINT ( 'NONE',  ( 6.836528711265448699, 15.75929247661555976, 9.299976744542933105 ) ) ;
#17609 = CARTESIAN_POINT ( 'NONE',  ( 1.301042606982605321E-15, -21.41253812416053748, 4.000000000000000000 ) ) ;
#17610 = CARTESIAN_POINT ( 'NONE',  ( 21.48921356237309155, -27.52281430457070499, 5.000000000000000000 ) ) ;
#17611 = ORIENTED_EDGE ( 'NONE', *, *, #16644, .F. ) ;
#17612 = EDGE_LOOP ( 'NONE', ( #7610, #45907, #52844, #70920 ) ) ;
#17613 = FACE_OUTER_BOUND ( 'NONE', #14616, .T. ) ;
#17614 = DIRECTION ( 'NONE',  ( -1.000000000000000000, -0.000000000000000000, -0.000000000000000000 ) ) ;
#17615 = CARTESIAN_POINT ( 'NONE',  ( 2.895403141435219485, 2.126176841940962348, 7.934999999999989839 ) ) ;
#17616 = VECTOR ( 'NONE', #75024, 999.9999999999998863 ) ;
#17617 = LINE ( 'NONE', #127102, #83003 ) ;
#17618 = CARTESIAN_POINT ( 'NONE',  ( 24.00548008471250938, 28.92564299267921513, 4.000000000000000000 ) ) ;
#17619 = DIRECTION ( 'NONE',  ( 0.7071067811865487940, 0.7071067811865463515, 0.000000000000000000 ) ) ;
#17620 = AXIS2_PLACEMENT_3D ( 'NONE', #20915, #97021, #41991 ) ;
#17621 = ORIENTED_EDGE ( 'NONE', *, *, #52558, .F. ) ;
#17622 = EDGE_CURVE ( 'NONE', #81439, #80081, #143465, .T. ) ;
#17623 = FACE_OUTER_BOUND ( 'NONE', #58483, .T. ) ;
#17624 = CARTESIAN_POINT ( 'NONE',  ( -11.67183060077638856, 5.259292476615662792, 4.000000000000000000 ) ) ;
#17625 = DIRECTION ( 'NONE',  ( 0.7071067811865486830, -0.7071067811865464625, -0.000000000000000000 ) ) ;
#17626 = DIRECTION ( 'NONE',  ( -0.000000000000000000, 0.000000000000000000, 1.000000000000000000 ) ) ;
#17627 = CARTESIAN_POINT ( 'NONE',  ( 44.53709685856478728, -3.054999999999999272, -5.291415217122919401 ) ) ;
#17628 = LINE ( 'NONE', #139476, #60352 ) ;
#17629 = EDGE_CURVE ( 'NONE', #127668, #903, #56493, .T. ) ;
#17630 = EDGE_CURVE ( 'NONE', #131124, #140410, #23815, .T. ) ;
#17631 = ORIENTED_EDGE ( 'NONE', *, *, #38250, .T. ) ;
#17632 = LINE ( 'NONE', #95926, #48862 ) ;
#17633 = ORIENTED_EDGE ( 'NONE', *, *, #115124, .T. ) ;
#17634 = AXIS2_PLACEMENT_3D ( 'NONE', #26815, #27515, #92062 ) ;
#17635 = ORIENTED_EDGE ( 'NONE', *, *, #140237, .F. ) ;
#17636 = CARTESIAN_POINT ( 'NONE',  ( -34.49999999999975131, 4.087461875839202285, 4.000000000000000000 ) ) ;
#17637 = EDGE_CURVE ( 'NONE', #24661, #24394, #113662, .T. ) ;
#17638 = CARTESIAN_POINT ( 'NONE',  ( -30.87485380690746695, -14.24070752338413826, 9.401115078912727796 ) ) ;
#17639 = DIRECTION ( 'NONE',  ( -0.7071067811865486830, -0.7071067811865464625, 0.000000000000000000 ) ) ;
#17640 = VECTOR ( 'NONE', #94709, 1000.000000000000000 ) ;
#17641 = ADVANCED_FACE ( 'NONE', ( #79677 ), #12444, .T. ) ;
#17642 = DIRECTION ( 'NONE',  ( 0.000000000000000000, 0.000000000000000000, 1.000000000000000000 ) ) ;
#17643 = LINE ( 'NONE', #72095, #77798 ) ;
#17644 = ORIENTED_EDGE ( 'NONE', *, *, #22169, .F. ) ;
#17645 = EDGE_CURVE ( 'NONE', #26178, #82150, #68081, .T. ) ;
#17646 = DIRECTION ( 'NONE',  ( -0.7071067811865486830, 0.7071067811865464625, 0.000000000000000000 ) ) ;
#17647 = CARTESIAN_POINT ( 'NONE',  ( 54.18398860626899705, 28.73617430169825226, 5.000000000000000000 ) ) ;
#17648 = CARTESIAN_POINT ( 'NONE',  ( 13.69176145124043131, 22.22500000000000142, -13.42270830385341363 ) ) ;
#17649 = DIRECTION ( 'NONE',  ( 0.7071067811865486830, -0.7071067811865464625, -0.000000000000000000 ) ) ;
#17650 = CIRCLE ( 'NONE', #110264, 9.524999999999998579 ) ;
#17651 = CONICAL_SURFACE ( 'NONE', #38588, 2.500000000000000888, 0.9599310885968822538 ) ;
#17652 = CARTESIAN_POINT ( 'NONE',  ( 62.93336038379622721, 2.130196079827431532, -7.949999999999997513 ) ) ;
#17653 = AXIS2_PLACEMENT_3D ( 'NONE', #68915, #110929, #68223 ) ;
#17654 = CARTESIAN_POINT ( 'NONE',  ( -11.99999999999990941, 19.55218569542897100, 5.000000000000000000 ) ) ;
#17655 = EDGE_LOOP ( 'NONE', ( #21265, #100236, #2172, #90403 ) ) ;
#17656 = ORIENTED_EDGE ( 'NONE', *, *, #106500, .F. ) ;
#17657 = CARTESIAN_POINT ( 'NONE',  ( 60.06249999999998579, -5.819803920172572198, -5.819803920172573086 ) ) ;
#17658 = EDGE_CURVE ( 'NONE', #88912, #29169, #33984, .T. ) ;
#17659 = CARTESIAN_POINT ( 'NONE',  ( -9.316579611327837185, -6.740707523384216415, 11.88629033278126279 ) ) ;
#17660 = DIRECTION ( 'NONE',  ( 0.7071067811865487940, 0.7071067811865463515, 0.000000000000000000 ) ) ;
#17662 = CARTESIAN_POINT ( 'NONE',  ( 25.39999999999999858, 0.000000000000000000, 0.000000000000000000 ) ) ;
#17661 = AXIS2_PLACEMENT_3D ( 'NONE', #111453, #52774, #86866 ) ;
#17663 = ORIENTED_EDGE ( 'NONE', *, *, #7341, .T. ) ;
#17664 = ADVANCED_FACE ( 'NONE', ( #101364 ), #3455, .F. ) ;
#17665 = FACE_OUTER_BOUND ( 'NONE', #14766, .T. ) ;
#17666 = CARTESIAN_POINT ( 'NONE',  ( 15.48921356237309510, -27.52281430457066236, 5.000000000000000000 ) ) ;
#17667 = CARTESIAN_POINT ( 'NONE',  ( 56.72959685856476142, -6.110000000000000320, -1.637169565754161393 ) ) ;
#17668 = ORIENTED_EDGE ( 'NONE', *, *, #796, .F. ) ;
#17669 = CARTESIAN_POINT ( 'NONE',  ( -15.29974487139158867, -27.71228299555216879, 4.000000000000000000 ) ) ;
#17670 = VERTEX_POINT ( 'NONE', #91911 ) ;
#17671 = ORIENTED_EDGE ( 'NONE', *, *, #116508, .T. ) ;
#17672 = PLANE ( 'NONE',  #47030 ) ;
#17673 = CARTESIAN_POINT ( 'NONE',  ( 7.499999999999940492, -1.912538124160725106, 4.000000000000000000 ) ) ;
#17674 = CARTESIAN_POINT ( 'NONE',  ( -11.81601139373100651, 28.73617430169779041, 5.000000000000000000 ) ) ;
#17675 = CARTESIAN_POINT ( 'NONE',  ( 27.48921356237309155, -27.52281430457074762, 5.000000000000000000 ) ) ;
#17676 = CARTESIAN_POINT ( 'NONE',  ( -15.48921356237309510, -27.52281430457066236, 5.000000000000000000 ) ) ;
#17678 = ORIENTED_EDGE ( 'NONE', *, *, #71755, .F. ) ;
#17677 = CARTESIAN_POINT ( 'NONE',  ( -16.45742106731621845, 0.9613713492673547911, -33.49048331797055766 ) ) ;
#17679 = LINE ( 'NONE', #116304, #129442 ) ;
#17680 = LINE ( 'NONE', #128614, #3766 ) ;
#17681 = LINE ( 'NONE', #82278, #26313 ) ;
#17682 = EDGE_CURVE ( 'NONE', #9454, #66309, #11469, .T. ) ;
#17683 = LINE ( 'NONE', #6785, #43843 ) ;
#17684 = ADVANCED_FACE ( 'NONE', ( #134748 ), #111527, .F. ) ;
#17685 = VERTEX_POINT ( 'NONE', #68768 ) ;
#17686 = EDGE_CURVE ( 'NONE', #116862, #536, #110784, .T. ) ;
#17687 = ORIENTED_EDGE ( 'NONE', *, *, #48645, .F. ) ;
#17688 = VECTOR ( 'NONE', #127441, 1000.000000000000000 ) ;
#17689 = PRESENTATION_STYLE_ASSIGNMENT (( #80853 ) ) ;
#17690 = FACE_OUTER_BOUND ( 'NONE', #29308, .T. ) ;
#17691 = CARTESIAN_POINT ( 'NONE',  ( 29.29298673570674438, -21.74070752338405654, 4.999753212805219782 ) ) ;
#17692 = CARTESIAN_POINT ( 'NONE',  ( 29.27718569542920335, -21.72500000000000142, 5.000000000000000000 ) ) ;
#17693 = DIRECTION ( 'NONE',  ( -0.000000000000000000, -0.3543493200069152693, 0.9351131265310292928 ) ) ;
#17694 = EDGE_LOOP ( 'NONE', ( #83042, #100580, #89247, #6553 ) ) ;
#17695 = ORIENTED_EDGE ( 'NONE', *, *, #63152, .F. ) ;
#17696 = STYLED_ITEM ( 'NONE', ( #50691 ), #13350 ) ;
#17697 = PLANE ( 'NONE',  #132603 ) ;
#17698 = CARTESIAN_POINT ( 'NONE',  ( 13.49999999999990408, 15.43112307739202294, 4.000000000000000000 ) ) ;
#17699 = EDGE_LOOP ( 'NONE', ( #126975, #106689, #48299, #86374 ) ) ;
#17700 = ORIENTED_EDGE ( 'NONE', *, *, #137466, .T. ) ;
#17701 = CARTESIAN_POINT ( 'NONE',  ( -30.48921356237309510, -27.52281430457076894, 5.000000000000000000 ) ) ;
#17702 = ORIENTED_EDGE ( 'NONE', *, *, #134833, .F. ) ;
#17703 = CARTESIAN_POINT ( 'NONE',  ( 13.92145407031093818, 4.584330080086930965E-16, 0.000000000000000000 ) ) ;
#17705 = CONICAL_SURFACE ( 'NONE', #73321, 2.500000000000000444, 0.9599310885968830309 ) ;
#17704 = CARTESIAN_POINT ( 'NONE',  ( 34.49999999999976552, 4.464255608400454101, 4.994342998332159667 ) ) ;
#17706 = FACE_BOUND ( 'NONE', #33151, .T. ) ;
#17707 = DIRECTION ( 'NONE',  ( -1.000000000000000000, -1.224606353822377258E-16, -0.000000000000000000 ) ) ;
#17708 = CARTESIAN_POINT ( 'NONE',  ( -2.994519915287485734, 28.92564299267940342, 4.000000000000000000 ) ) ;
#17709 = CARTESIAN_POINT ( 'NONE',  ( 9.187500000000001776, 4.461849672132297329, -4.461849672132302658 ) ) ;
#17711 = ORIENTED_EDGE ( 'NONE', *, *, #40487, .F. ) ;
#17710 = CARTESIAN_POINT ( 'NONE',  ( 23.00840764549667483, -2.500000000000000888, 0.000000000000000000 ) ) ;
#17712 = FILL_AREA_STYLE_COLOUR ( '', #23152 ) ;
#17713 = PRODUCT_CONTEXT ( 'NONE', #80048, 'mechanical' ) ;
#17715 = ORIENTED_EDGE ( 'NONE', *, *, #26330, .T. ) ;
#17714 = VECTOR ( 'NONE', #103165, 1000.000000000000227 ) ;
#17716 = ORIENTED_EDGE ( 'NONE', *, *, #123364, .F. ) ;
#17717 = CARTESIAN_POINT ( 'NONE',  ( 95.14126352523143737, 4.472830434245835818, 4.472830434245840259 ) ) ;
#17718 = VERTEX_POINT ( 'NONE', #112260 ) ;
#17719 = VECTOR ( 'NONE', #135267, 1000.000000000000000 ) ;
#17720 = DIRECTION ( 'NONE',  ( 1.000000000000000000, -0.000000000000000000, -0.000000000000000000 ) ) ;
#17721 = VECTOR ( 'NONE', #72827, 1000.000000000000000 ) ;
#17722 = DIRECTION ( 'NONE',  ( -1.000000000000000000, 0.000000000000000000, -0.000000000000000000 ) ) ;
#17723 = LINE ( 'NONE', #138834, #114229 ) ;
#17724 = ORIENTED_EDGE ( 'NONE', *, *, #100296, .F. ) ;
#17725 = CARTESIAN_POINT ( 'NONE',  ( -29.99999999999979039, 13.93112307739203892, 4.000000000000000000 ) ) ;
#17726 = CARTESIAN_POINT ( 'NONE',  ( 15.79289321881335084, -11.24070752338416845, 5.000000000000000000 ) ) ;
#17727 = AXIS2_PLACEMENT_3D ( 'NONE', #83932, #137571, #94743 ) ;
#17728 = DIRECTION ( 'NONE',  ( 0.7071067811865487940, -0.7071067811865463515, 0.000000000000000000 ) ) ;
#17729 = LINE ( 'NONE', #139578, #7569 ) ;
#17730 = CARTESIAN_POINT ( 'NONE',  ( 180.9243601523648692, -48.88932940808381034, -39.16623080367945420 ) ) ;
#17731 = CARTESIAN_POINT ( 'NONE',  ( -21.48921356237309155, -27.52281430457070499, 5.000000000000000000 ) ) ;
#17732 = EDGE_LOOP ( 'NONE', ( #76289, #14200, #90520, #117297 ) ) ;
#17733 = DIRECTION ( 'NONE',  ( -0.000000000000000000, -0.3543493200069152693, 0.9351131265310292928 ) ) ;
#17734 = DIRECTION ( 'NONE',  ( 0.7071067811865487940, 0.7071067811865463515, 0.000000000000000000 ) ) ;
#17735 = EDGE_CURVE ( 'NONE', #79314, #83079, #128270, .T. ) ;
#17736 = ORIENTED_EDGE ( 'NONE', *, *, #122820, .F. ) ;
#17738 = ORIENTED_EDGE ( 'NONE', *, *, #19486, .T. ) ;
#17737 = VECTOR ( 'NONE', #96837, 1000.000000000000000 ) ;
#17739 = EDGE_CURVE ( 'NONE', #33310, #61158, #46319, .T. ) ;
#17740 = EDGE_LOOP ( 'NONE', ( #34336, #14267, #122950, #59371 ) ) ;
#17741 = CARTESIAN_POINT ( 'NONE',  ( 47.83376352523143993, 6.110000000000001208, 1.122388791418549305E-15 ) ) ;
#17742 = VERTEX_POINT ( 'NONE', #25224 ) ;
#17743 = AXIS2_PLACEMENT_3D ( 'NONE', #91886, #66069, #88525 ) ;
#17744 = EDGE_CURVE ( 'NONE', #45590, #13451, #57900, .T. ) ;
#17745 = EDGE_CURVE ( 'NONE', #74597, #118741, #35442, .T. ) ;
#17746 = VECTOR ( 'NONE', #75653, 1000.000000000000000 ) ;
#17747 = CARTESIAN_POINT ( 'NONE',  ( 15.21247294953710671, 0.000000000000000000, 6.094999999999989981 ) ) ;
#17748 = CARTESIAN_POINT ( 'NONE',  ( -18.92851995498817530, 2.123550300856637207, -30.34508942967045186 ) ) ;
#17749 = ORIENTED_EDGE ( 'NONE', *, *, #6728, .T. ) ;
#17750 = EDGE_CURVE ( 'NONE', #13173, #77699, #73869, .T. ) ;
#17751 = CARTESIAN_POINT ( 'NONE',  ( 18.28838880452753202, -2.745211937670052560, 5.000000000000000000 ) ) ;
#17752 = ORIENTED_EDGE ( 'NONE', *, *, #1300, .T. ) ;
#17753 = CARTESIAN_POINT ( 'NONE',  ( -28.49999999999979750, 0.4311230773921762571, 4.000000000000000000 ) ) ;
#17754 = VECTOR ( 'NONE', #3753, 1000.000000000000000 ) ;
#17755 = LINE ( 'NONE', #103342, #77629 ) ;
#17757 = EDGE_LOOP ( 'NONE', ( #11864, #80979, #71115, #42183 ) ) ;
#17756 = LINE ( 'NONE', #139603, #100359 ) ;
#17758 = VERTEX_POINT ( 'NONE', #47058 ) ;
#17759 = CARTESIAN_POINT ( 'NONE',  ( -34.92500000000001137, -12.18334561358944335, 4.500000000000000888 ) ) ;
#17760 = CARTESIAN_POINT ( 'NONE',  ( 0.000000000000000000, 0.000000000000000000, 0.000000000000000000 ) ) ;
#17761 = EDGE_CURVE ( 'NONE', #65062, #117371, #99946, .T. ) ;
#17762 = ORIENTED_EDGE ( 'NONE', *, *, #124705, .F. ) ;
#17763 = DIRECTION ( 'NONE',  ( 0.7071067811865486830, -0.7071067811865464625, -0.000000000000000000 ) ) ;
#17764 = EDGE_LOOP ( 'NONE', ( #82983, #90171, #70123, #22895, #49790 ) ) ;
#17765 = ORIENTED_EDGE ( 'NONE', *, *, #38528, .T. ) ;
#17766 = VERTEX_POINT ( 'NONE', #58645 ) ;
#17767 = ORIENTED_EDGE ( 'NONE', *, *, #112539, .T. ) ;
#17768 = CARTESIAN_POINT ( 'NONE',  ( 10.19018167574442124, -18.74070752338409207, 7.910009926591483165 ) ) ;
#17769 = ADVANCED_FACE ( 'NONE', ( #36817 ), #22345, .F. ) ;
#17770 = CARTESIAN_POINT ( 'NONE',  ( 0.000000000000000000, 21.72500000000000142, 4.500000000000000888 ) ) ;
#17771 = PLANE ( 'NONE',  #70297 ) ;
#17772 = CARTESIAN_POINT ( 'NONE',  ( 9.792893218813388145, 18.75929247661553489, 5.000000000000000000 ) ) ;
#17773 = VERTEX_POINT ( 'NONE', #28092 ) ;
#17774 = CARTESIAN_POINT ( 'NONE',  ( -8.671830600776409881, -12.74070752338415424, 4.000000000000000000 ) ) ;
#17775 = ORIENTED_EDGE ( 'NONE', *, *, #22179, .T. ) ;
#17776 = VECTOR ( 'NONE', #116003, 1000.000000000000000 ) ;
#17777 = EDGE_CURVE ( 'NONE', #96318, #103184, #72358, .T. ) ;
#17778 = CARTESIAN_POINT ( 'NONE',  ( -26.99451991528749417, 28.92564299267956685, 4.000000000000000000 ) ) ;
#17779 = CARTESIAN_POINT ( 'NONE',  ( 32.79123647476855297, -9.717572351234235426E-16, -7.934999999999990727 ) ) ;
#17780 = DIRECTION ( 'NONE',  ( -0.7071067811865487940, 0.7071067811865463515, -0.000000000000000000 ) ) ;
#17781 = AXIS2_PLACEMENT_3D ( 'NONE', #46096, #1796, #101868 ) ;
#17782 = VERTEX_POINT ( 'NONE', #103484 ) ;
#17783 = CARTESIAN_POINT ( 'NONE',  ( 23.20666063542136115, 21.75929247661548871, 4.998822639870701856 ) ) ;
#17784 = DIRECTION ( 'NONE',  ( -1.000000000000000000, -1.224606353822377258E-16, -0.000000000000000000 ) ) ;
#17785 = EDGE_LOOP ( 'NONE', ( #32631, #62652, #73622, #36329 ) ) ;
#17786 = ORIENTED_EDGE ( 'NONE', *, *, #101685, .T. ) ;
#17788 = ORIENTED_EDGE ( 'NONE', *, *, #53348, .T. ) ;
#17787 = EDGE_CURVE ( 'NONE', #103460, #80827, #112025, .T. ) ;
#17789 = LINE ( 'NONE', #63503, #57986 ) ;
#17790 = DIRECTION ( 'NONE',  ( 0.000000000000000000, 1.000000000000000000, -2.556434596176436916E-15 ) ) ;
#17791 = CARTESIAN_POINT ( 'NONE',  ( 1.199999999999999956, 0.5999999999999987566, -4.750000000000000888 ) ) ;
#17792 = AXIS2_PLACEMENT_3D ( 'NONE', #133722, #113366, #67788 ) ;
#17793 = CARTESIAN_POINT ( 'NONE',  ( -34.47516574401892342, -17.97193265888399694, 4.998110765256835286 ) ) ;
#17794 = CARTESIAN_POINT ( 'NONE',  ( 0.2242312616510835910, -48.73293412427781846, -38.67339632249748149 ) ) ;
#17795 = CARTESIAN_POINT ( 'NONE',  ( 75.30793019189809456, -6.109999999999999432, 1.637169565754158507 ) ) ;
#17796 =( BOUNDED_CURVE ( )  B_SPLINE_CURVE ( 2, ( #124499, #80312, #102762, #12159, #47004, #79631, #35389, #25173, #34645, #67279, #24468, #90447, #23768 ),
 .UNSPECIFIED., .F., .F. ) 
 B_SPLINE_CURVE_WITH_KNOTS ( ( 3, 2, 2, 2, 2, 2, 3 ),
 ( 0.2500000000000000000, 0.2527777777777777679, 0.2555555555555555358, 0.2583333333333333592, 0.2611111111111111271, 0.2638888888888888951, 0.2666666666666666630 ),
 .UNSPECIFIED. ) 
 CURVE ( )  GEOMETRIC_REPRESENTATION_ITEM ( )  RATIONAL_B_SPLINE_CURVE ( ( 1.000000000000000000, 0.9659258262890683122, 1.000000000000000000, 0.9659258262890683122, 1.000000000000000000, 0.9659258262890683122, 1.000000000000000000, 0.9659258262890683122, 1.000000000000000000, 0.9659258262890683122, 1.000000000000000000, 0.9659258262890683122, 1.000000000000000000 ) ) 
 REPRESENTATION_ITEM ( '' )  );
#17797 = DIRECTION ( 'NONE',  ( -0.6830127018922180770, -0.6830127018922204085, -0.2588190451025213501 ) ) ;
#17798 = EDGE_CURVE ( 'NONE', #132198, #36664, #60768, .T. ) ;
#17799 = DIRECTION ( 'NONE',  ( -1.000000000000000000, -1.224606353822377258E-16, -0.000000000000000000 ) ) ;
#17800 = LINE ( 'NONE', #108359, #71962 ) ;
#17801 = DIRECTION ( 'NONE',  ( 0.5735764363510448272, -0.8191520442889927978, 1.003171929053526103E-16 ) ) ;
#17802 = EDGE_CURVE ( 'NONE', #1490, #104227, #82482, .T. ) ;
#17803 = CARTESIAN_POINT ( 'NONE',  ( 34.36246187583877543, 22.22500000000000142, 4.000000000000000000 ) ) ;
#17804 = PRESENTATION_LAYER_ASSIGNMENT (  '', '', ( #101126 ) ) ;
#17805 = ORIENTED_EDGE ( 'NONE', *, *, #1235, .F. ) ;
#17806 = PLANE ( 'NONE',  #40676 ) ;
#17807 = EDGE_LOOP ( 'NONE', ( #120913, #41421, #27639, #115257 ) ) ;
#17808 =( BOUNDED_CURVE ( )  B_SPLINE_CURVE ( 2, ( #140885, #87244, #32147, #119142, #44488, #64066, #66924, #19825, #41583, #108965, #108232, #53167, #87953 ),
 .UNSPECIFIED., .F., .F. ) 
 B_SPLINE_CURVE_WITH_KNOTS ( ( 3, 2, 2, 2, 2, 2, 3 ),
 ( 0.4500000000000000111, 0.4527777777777777790, 0.4555555555555555469, 0.4583333333333333148, 0.4611111111111111382, 0.4638888888888889062, 0.4666666666666666741 ),
 .UNSPECIFIED. ) 
 CURVE ( )  GEOMETRIC_REPRESENTATION_ITEM ( )  RATIONAL_B_SPLINE_CURVE ( ( 1.000000000000000000, 0.9659258262890683122, 1.000000000000000000, 0.9659258262890683122, 1.000000000000000000, 0.9659258262890683122, 1.000000000000000000, 0.9659258262890683122, 1.000000000000000000, 0.9659258262890683122, 1.000000000000000000, 0.9659258262890683122, 1.000000000000000000 ) ) 
 REPRESENTATION_ITEM ( '' )  );
#17809 = ADVANCED_FACE ( 'NONE', ( #39704 ), #73058, .F. ) ;
#17810 = LINE ( 'NONE', #62079, #34564 ) ;
#17812 = ORIENTED_EDGE ( 'NONE', *, *, #36306, .F. ) ;
#17811 = DIRECTION ( 'NONE',  ( 0.7071067811865486830, -0.7071067811865464625, -0.000000000000000000 ) ) ;
#17813 = DIRECTION ( 'NONE',  ( -1.000000000000000000, -1.224606353822377258E-16, -0.000000000000000000 ) ) ;
#17814 = CARTESIAN_POINT ( 'NONE',  ( -24.47512612785031294, 14.25929247661557753, 9.797011795316580063 ) ) ;
#17815 = ORIENTED_EDGE ( 'NONE', *, *, #25789, .F. ) ;
#17816 = VERTEX_POINT ( 'NONE', #115767 ) ;
#17817 = CARTESIAN_POINT ( 'NONE',  ( 22.49999999999984723, -16.91253812416058011, 4.000000000000000000 ) ) ;
#17818 = DIRECTION ( 'NONE',  ( 0.7071067811865487940, 0.7071067811865463515, -0.000000000000000000 ) ) ;
#17819 = CARTESIAN_POINT ( 'NONE',  ( 60.48921356237309510, -27.52281430457097500, 5.000000000000000000 ) ) ;
#17820 = CARTESIAN_POINT ( 'NONE',  ( 93.99586038379622721, -3.974999999999998312, -6.884901960086286188 ) ) ;
#17821 = FACE_OUTER_BOUND ( 'NONE', #116099, .T. ) ;
#17822 = LINE ( 'NONE', #114978, #55259 ) ;
#17823 = ORIENTED_EDGE ( 'NONE', *, *, #20831, .F. ) ;
#17824 = VECTOR ( 'NONE', #55380, 1000.000000000000000 ) ;
#17825 = EDGE_CURVE ( 'NONE', #75708, #12022, #117211, .T. ) ;
#17826 = DIRECTION ( 'NONE',  ( 0.000000000000000000, 0.000000000000000000, 1.000000000000000000 ) ) ;
#17827 = CARTESIAN_POINT ( 'NONE',  ( 14.81601139373099585, 28.73617430169776910, 5.000000000000000000 ) ) ;
#17828 = CARTESIAN_POINT ( 'NONE',  ( 29.60416666666666430, -1.633150327867691987, -6.094999999999989093 ) ) ;
#17829 = DIRECTION ( 'NONE',  ( -0.6830127018922180770, -0.6830127018922204085, -0.2588190451025213501 ) ) ;
#17830 = ORIENTED_EDGE ( 'NONE', *, *, #69011, .T. ) ;
#17831 = ADVANCED_FACE ( 'NONE', ( #104930 ), #17214, .T. ) ;
#17832 = ORIENTED_EDGE ( 'NONE', *, *, #11576, .F. ) ;
#17833 = CARTESIAN_POINT ( 'NONE',  ( 86.33376352523144703, 6.110000000000001208, 1.122388791418549305E-15 ) ) ;
#17834 = DIRECTION ( 'NONE',  ( 0.7071067811865487940, -0.7071067811865463515, 0.000000000000000000 ) ) ;
#17835 = LINE ( 'NONE', #16408, #109424 ) ;
#17836 = DIRECTION ( 'NONE',  ( 0.3543493200069162685, -0.000000000000000000, -0.9351131265310288487 ) ) ;
#17837 = ORIENTED_EDGE ( 'NONE', *, *, #72526, .F. ) ;
#17838 = DIRECTION ( 'NONE',  ( 0.3543493200069162685, -0.000000000000000000, -0.9351131265310288487 ) ) ;
#17839 = CARTESIAN_POINT ( 'NONE',  ( -9.328169399223465774, -0.7407075233842718154, 4.000000000000000000 ) ) ;
#17840 = AXIS2_PLACEMENT_3D ( 'NONE', #1639, #71061, #124175 ) ;
#17841 = CARTESIAN_POINT ( 'NONE',  ( 30.18398860626900060, 28.73617430169808173, 5.000000000000000000 ) ) ;
#17842 = EDGE_CURVE ( 'NONE', #15864, #9322, #114382, .T. ) ;
#17844 = ORIENTED_EDGE ( 'NONE', *, *, #110763, .T. ) ;
#17843 = CARTESIAN_POINT ( 'NONE',  ( 28.49999999999979750, -8.947814304570737676, 5.000000000000000000 ) ) ;
#17845 = CARTESIAN_POINT ( 'NONE',  ( 13.70833333333333393, 3.047499999999997655, 5.278424836066143655 ) ) ;
#17846 = CARTESIAN_POINT ( 'NONE',  ( -42.48921356237308800, -27.52281430457085065, 5.000000000000000000 ) ) ;
#17847 = DIRECTION ( 'NONE',  ( -1.000000000000000000, -1.224606353822377258E-16, -0.000000000000000000 ) ) ;
#17848 = AXIS2_PLACEMENT_3D ( 'NONE', #93858, #106132, #14866 ) ;
#17849 = VECTOR ( 'NONE', #43082, 1000.000000000000227 ) ;
#17850 = EDGE_LOOP ( 'NONE', ( #101128, #9708, #76905, #64073 ) ) ;
#17851 = EDGE_CURVE ( 'NONE', #60360, #61548, #91237, .T. ) ;
#17852 = ORIENTED_EDGE ( 'NONE', *, *, #38412, .T. ) ;
#17853 = AXIS2_PLACEMENT_3D ( 'NONE', #54464, #120356, #34124 ) ;
#17854 = CARTESIAN_POINT ( 'NONE',  ( 76.56293019189810423, 1.637169565754157174, 6.110000000000002984 ) ) ;
#17855 = ORIENTED_EDGE ( 'NONE', *, *, #56587, .T. ) ;
#17856 = DIRECTION ( 'NONE',  ( -0.7071067811865486830, 0.7071067811865464625, 0.000000000000000000 ) ) ;
#17857 = CARTESIAN_POINT ( 'NONE',  ( 20.88987624306225754, 8.854559187742358617, 4.414246686754478510 ) ) ;
#17858 = CARTESIAN_POINT ( 'NONE',  ( 14.99999999999990230, 7.007997736742463957, -8.085015511992081017 ) ) ;
#17859 = ORIENTED_EDGE ( 'NONE', *, *, #104038, .T. ) ;
#17860 = LINE ( 'NONE', #28062, #21325 ) ;
#17861 = DIRECTION ( 'NONE',  ( -0.7071067811865486830, -0.7071067811865464625, -0.000000000000000000 ) ) ;
#17862 = ADVANCED_FACE ( 'NONE', ( #61476 ), #128137, .F. ) ;
#17863 = ORIENTED_EDGE ( 'NONE', *, *, #123371, .T. ) ;
#17864 = LINE ( 'NONE', #51970, #32810 ) ;
#17865 = DIRECTION ( 'NONE',  ( -0.7071067811865487940, 0.7071067811865463515, -0.000000000000000000 ) ) ;
#17866 = CARTESIAN_POINT ( 'NONE',  ( 11.99999999999992006, 12.25461709320621928, -10.07315571508694418 ) ) ;
#17867 = ORIENTED_EDGE ( 'NONE', *, *, #33167, .F. ) ;
#17868 = ORIENTED_EDGE ( 'NONE', *, *, #91884, .F. ) ;
#17869 = EDGE_CURVE ( 'NONE', #112404, #50577, #6280, .T. ) ;
#17870 = CARTESIAN_POINT ( 'NONE',  ( -0.7071067811865398012, 8.259292476615641476, 5.000000000000000000 ) ) ;
#17871 = DIRECTION ( 'NONE',  ( 0.000000000000000000, 0.000000000000000000, 1.000000000000000000 ) ) ;
#17872 = LINE ( 'NONE', #106306, #108994 ) ;
#17873 = DIRECTION ( 'NONE',  ( -0.000000000000000000, 0.3543493200069153248, 0.9351131265310292928 ) ) ;
#17874 = AXIS2_PLACEMENT_3D ( 'NONE', #90914, #135145, #16143 ) ;
#17875 = CARTESIAN_POINT ( 'NONE',  ( 17.70025512860841488, -27.71228299555193786, 4.000000000000000000 ) ) ;
#17876 = CARTESIAN_POINT ( 'NONE',  ( 42.48921356237308800, -27.52281430457085065, 5.000000000000000000 ) ) ;
#17877 = ORIENTED_EDGE ( 'NONE', *, *, #89697, .T. ) ;
#17878 = VECTOR ( 'NONE', #119416, 1000.000000000000000 ) ;
#17879 = ORIENTED_EDGE ( 'NONE', *, *, #118971, .F. ) ;
#17880 = ORIENTED_EDGE ( 'NONE', *, *, #122261, .T. ) ;
#17881 = EDGE_LOOP ( 'NONE', ( #41173, #113679, #90274, #94479 ) ) ;
#17882 = VECTOR ( 'NONE', #57689, 1000.000000000000000 ) ;
#17883 = DIRECTION ( 'NONE',  ( -0.7071067811865486830, -0.7071067811865464625, 0.000000000000000000 ) ) ;
#17884 =( NAMED_UNIT ( * ) SI_UNIT ( $, .STERADIAN. ) SOLID_ANGLE_UNIT ( ) );
#17885 = ORIENTED_EDGE ( 'NONE', *, *, #3415, .F. ) ;
#17886 = LINE ( 'NONE', #71605, #101561 ) ;
#17887 = DIRECTION ( 'NONE',  ( 0.000000000000000000, -1.000000000000000000, 0.000000000000000000 ) ) ;
#17889 = ADVANCED_FACE ( 'NONE', ( #126669 ), #26663, .T. ) ;
#17888 = DIRECTION ( 'NONE',  ( 0.7071067811865486830, -0.7071067811865464625, -0.000000000000000000 ) ) ;
#17890 = CARTESIAN_POINT ( 'NONE',  ( 151.4000000000000057, -16.48000000000005016, -12.70000000000045404 ) ) ;
#17891 = CARTESIAN_POINT ( 'NONE',  ( 27.00000000000001066, -7.055460226182286299, -2.590656038797956029 ) ) ;
#17892 = ORIENTED_EDGE ( 'NONE', *, *, #47128, .T. ) ;
#17893 = CARTESIAN_POINT ( 'NONE',  ( 29.99999999999999645, -2.375000000000000000, -4.320000000000002061 ) ) ;
#17894 = PLANE ( 'NONE',  #41972 ) ;
#17895 = ORIENTED_EDGE ( 'NONE', *, *, #18633, .F. ) ;
#17896 = ORIENTED_EDGE ( 'NONE', *, *, #4547, .F. ) ;
#17897 = EDGE_CURVE ( 'NONE', #142173, #101006, #38262, .T. ) ;
#17898 = EDGE_CURVE ( 'NONE', #142746, #129157, #7001, .T. ) ;
#17899 = DIRECTION ( 'NONE',  ( -0.7071067811865486830, 0.7071067811865464625, 0.000000000000000000 ) ) ;
#17900 = EDGE_LOOP ( 'NONE', ( #114158, #111690, #4831, #143309, #130354, #67370, #13975, #59741, #61371, #27387, #37932, #61730, #47743, #124177, #64216, #119409, #122662, #46592 ) ) ;
#17901 = CARTESIAN_POINT ( 'NONE',  ( 76.85459685856477563, -1.637169565754161615, 6.110000000000000320 ) ) ;
#17902 = ORIENTED_EDGE ( 'NONE', *, *, #137261, .T. ) ;
#17903 = EDGE_CURVE ( 'NONE', #35767, #104436, #38965, .T. ) ;
#17904 = ADVANCED_FACE ( 'NONE', ( #40418 ), #15054, .F. ) ;
#17906 = ADVANCED_FACE ( 'NONE', ( #115058 ), #75197, .F. ) ;
#17905 = FACE_OUTER_BOUND ( 'NONE', #123016, .T. ) ;
#17907 = VECTOR ( 'NONE', #781, 1000.000000000000227 ) ;
#17908 = CARTESIAN_POINT ( 'NONE',  ( 109.2295968585647614, -6.110000000000000320, -1.637169565754161393 ) ) ;
#17909 = DIRECTION ( 'NONE',  ( -0.000000000000000000, 0.000000000000000000, 1.000000000000000000 ) ) ;
#17910 = EDGE_CURVE ( 'NONE', #25446, #13935, #108457, .T. ) ;
#17911 = CARTESIAN_POINT ( 'NONE',  ( -78.48921356237309510, -27.52281430457109934, 5.000000000000000000 ) ) ;
#17912 = CARTESIAN_POINT ( 'NONE',  ( -42.48921356237308800, -27.52281430457085065, 5.000000000000000000 ) ) ;
#17913 = PLANE ( 'NONE',  #128623 ) ;
#17914 = EDGE_CURVE ( 'NONE', #60360, #98372, #65764, .T. ) ;
#17915 = DIRECTION ( 'NONE',  ( -0.3543493200069162685, -0.000000000000000000, -0.9351131265310288487 ) ) ;
#17916 = DIRECTION ( 'NONE',  ( 0.000000000000000000, 0.000000000000000000, 1.000000000000000000 ) ) ;
#17917 = FACE_OUTER_BOUND ( 'NONE', #452, .T. ) ;
#17918 = EDGE_CURVE ( 'NONE', #15815, #2157, #9138, .T. ) ;
#17919 = ORIENTED_EDGE ( 'NONE', *, *, #92572, .T. ) ;
#17920 = AXIS2_PLACEMENT_3D ( 'NONE', #88839, #20694, #77265 ) ;
#17921 = SURFACE_SIDE_STYLE ('',( #35472 ) ) ;
#17922 = DIRECTION ( 'NONE',  ( 0.000000000000000000, 0.000000000000000000, 1.000000000000000000 ) ) ;
#17923 = ORIENTED_EDGE ( 'NONE', *, *, #47686, .T. ) ;
#17924 = ORIENTED_EDGE ( 'NONE', *, *, #66583, .T. ) ;
#17925 = LINE ( 'NONE', #45992, #100590 ) ;
#17926 = ORIENTED_EDGE ( 'NONE', *, *, #53196, .T. ) ;
#17927 = DIRECTION ( 'NONE',  ( 0.3543493200069162685, -0.000000000000000000, -0.9351131265310288487 ) ) ;
#17928 = LINE ( 'NONE', #86092, #68647 ) ;
#17929 = EDGE_CURVE ( 'NONE', #5604, #91707, #63609, .T. ) ;
#17930 = VECTOR ( 'NONE', #102630, 1000.000000000000000 ) ;
#17931 = DIRECTION ( 'NONE',  ( -0.7071067811865486830, -0.7071067811865464625, -0.000000000000000000 ) ) ;
#17932 = LINE ( 'NONE', #109802, #78820 ) ;
#17933 =( REPRESENTATION_RELATIONSHIP ('NONE','NONE', #69070, #428 ) REPRESENTATION_RELATIONSHIP_WITH_TRANSFORMATION ( #130084 )SHAPE_REPRESENTATION_RELATIONSHIP( ) );
#17934 = VERTEX_POINT ( 'NONE', #96869 ) ;
#17935 = SURFACE_SIDE_STYLE ('',( #31013 ) ) ;
#17936 = EDGE_LOOP ( 'NONE', ( #81907, #105161, #79468 ) ) ;
#17937 = EDGE_CURVE ( 'NONE', #104733, #2653, #141875, .T. ) ;
#17938 = VECTOR ( 'NONE', #133315, 1000.000000000000227 ) ;
#17939 = VECTOR ( 'NONE', #80328, 999.9999999999998863 ) ;
#17940 = CARTESIAN_POINT ( 'NONE',  ( 3.770403141435219041, -7.934999999999989839, 2.126176841940957907 ) ) ;
#17941 = CARTESIAN_POINT ( 'NONE',  ( 11.72733514412567857, 3.821174125832445049E-16, 0.000000000000000000 ) ) ;
#17942 = LINE ( 'NONE', #16530, #48282 ) ;
#17943 = CARTESIAN_POINT ( 'NONE',  ( 12.99975870850580861, -8.843799839164724119, 3.473668526774862819 ) ) ;
#17944 = ORIENTED_EDGE ( 'NONE', *, *, #137694, .F. ) ;
#17945 = ORIENTED_EDGE ( 'NONE', *, *, #130159, .F. ) ;
#17946 = VERTEX_POINT ( 'NONE', #107770 ) ;
#17947 = CARTESIAN_POINT ( 'NONE',  ( 68.99451991528748351, 28.92564299267986172, 4.000000000000000000 ) ) ;
#17948 = VECTOR ( 'NONE', #22306, 999.9999999999998863 ) ;
#17949 = FACE_OUTER_BOUND ( 'NONE', #35751, .T. ) ;
#17950 = CARTESIAN_POINT ( 'NONE',  ( -60.29974487139158867, -27.71228299555248142, 4.000000000000000000 ) ) ;
#17951 = CARTESIAN_POINT ( 'NONE',  ( 42.48921356237308800, -27.52281430457085065, 5.000000000000000000 ) ) ;
#17952 = PLANE ( 'NONE',  #131335 ) ;
#17953 = PLANE ( 'NONE',  #136743 ) ;
#17954 = EDGE_CURVE ( 'NONE', #19275, #59344, #14730, .T. ) ;
#17955 = FACE_OUTER_BOUND ( 'NONE', #3459, .T. ) ;
#17956 = SURFACE_SIDE_STYLE ('',( #130344 ) ) ;
#17957 = EDGE_CURVE ( 'NONE', #125874, #139670, #141118, .T. ) ;
#17958 = ORIENTED_EDGE ( 'NONE', *, *, #16960, .F. ) ;
#17959 = DIRECTION ( 'NONE',  ( 0.6830127018922180770, -0.6830127018922204085, -0.2588190451025213501 ) ) ;
#17960 = PLANE ( 'NONE',  #140227 ) ;
#17961 = ORIENTED_EDGE ( 'NONE', *, *, #65610, .F. ) ;
#17962 = ADVANCED_FACE ( 'NONE', ( #8431 ), #99035, .F. ) ;
#17963 = CARTESIAN_POINT ( 'NONE',  ( 34.11017322888187664, -22.22500000000000142, 4.785647885939352975 ) ) ;
#17965 = ORIENTED_EDGE ( 'NONE', *, *, #120106, .F. ) ;
#17964 = CARTESIAN_POINT ( 'NONE',  ( 12.48921356237309155, -27.52281430457064104, 5.000000000000000000 ) ) ;
#17966 = CARTESIAN_POINT ( 'NONE',  ( -34.92500000000001137, -8.028593703617126209, -6.464217593021346353 ) ) ;
#17968 = AXIS2_PLACEMENT_3D ( 'NONE', #27920, #115590, #6123 ) ;
#17967 = CARTESIAN_POINT ( 'NONE',  ( 15.29974487139158867, -27.71228299555216879, 4.000000000000000000 ) ) ;
#17969 = ORIENTED_EDGE ( 'NONE', *, *, #48082, .T. ) ;
#17970 = CARTESIAN_POINT ( 'NONE',  ( -75.29974487139158157, -27.71228299555258445, 4.000000000000000000 ) ) ;
#17971 = ORIENTED_EDGE ( 'NONE', *, *, #53875, .T. ) ;
#17972 = DIRECTION ( 'NONE',  ( -0.3543493200069162685, -0.000000000000000000, -0.9351131265310288487 ) ) ;
#17973 = CARTESIAN_POINT ( 'NONE',  ( 120.8291937171295700, -3.975000000000001865, 6.884901960086284411 ) ) ;
#17974 = AXIS2_PLACEMENT_3D ( 'NONE', #64500, #40622, #7954 ) ;
#17975 = DIRECTION ( 'NONE',  ( 0.7071067811865486830, -0.7071067811865464625, -0.000000000000000000 ) ) ;
#17976 = DIRECTION ( 'NONE',  ( 0.6830127018922180770, -0.6830127018922204085, -0.2588190451025213501 ) ) ;
#17977 = EDGE_CURVE ( 'NONE', #110210, #138157, #42570, .T. ) ;
#17978 = DIRECTION ( 'NONE',  ( 0.7071067811865487940, -0.7071067811865463515, 0.000000000000000000 ) ) ;
#17979 = CARTESIAN_POINT ( 'NONE',  ( -14.99451991528749595, 28.92564299267948513, 4.000000000000000000 ) ) ;
#17980 = FACE_OUTER_BOUND ( 'NONE', #85243, .T. ) ;
#17981 = CARTESIAN_POINT ( 'NONE',  ( 27.68706980810188867, -2.126176841940956130, 7.934999999999991616 ) ) ;
#17982 = CARTESIAN_POINT ( 'NONE',  ( 7.853736474768552966, -5.808823158059035485, -5.808823158059033709 ) ) ;
#17983 = CARTESIAN_POINT ( 'NONE',  ( -29.14994871458958414, -8.240707523384193323, 17.25253755692232360 ) ) ;
#17984 = FACE_OUTER_BOUND ( 'NONE', #71363, .T. ) ;
#17985 = CARTESIAN_POINT ( 'NONE',  ( 6.299744871391586898, -27.71228299555210484, 4.000000000000000000 ) ) ;
#17986 = VERTEX_POINT ( 'NONE', #75887 ) ;
#17987 = ORIENTED_EDGE ( 'NONE', *, *, #120981, .F. ) ;
#17988 = CARTESIAN_POINT ( 'NONE',  ( 86.75000000000000000, -9.735942053221458872E-16, 7.950000000000000178 ) ) ;
#17989 = FACE_OUTER_BOUND ( 'NONE', #95732, .T. ) ;
#17990 = EDGE_LOOP ( 'NONE', ( #136684, #104395, #142497, #52816 ) ) ;
#17991 = DIRECTION ( 'NONE',  ( 0.6830127018922180770, -0.6830127018922204085, -0.2588190451025213501 ) ) ;
#17992 = PRESENTATION_STYLE_ASSIGNMENT (( #41944 ) ) ;
#17993 = CARTESIAN_POINT ( 'NONE',  ( 2.994519915287485734, 28.92564299267940342, 4.000000000000000000 ) ) ;
#17994 = ORIENTED_EDGE ( 'NONE', *, *, #138838, .T. ) ;
#17995 = DIRECTION ( 'NONE',  ( 0.6830127018922180770, -0.6830127018922204085, -0.2588190451025213501 ) ) ;
#17996 = DIRECTION ( 'NONE',  ( 0.5735764363510451602, 0.8191520442889924647, 0.000000000000000000 ) ) ;
#17997 = DIRECTION ( 'NONE',  ( -0.7071067811865486830, 0.7071067811865464625, 0.000000000000000000 ) ) ;
#17998 = CARTESIAN_POINT ( 'NONE',  ( 11.99999999999993072, -16.44781430457065952, 5.000000000000000000 ) ) ;
#17999 = EDGE_CURVE ( 'NONE', #68842, #925, #96175, .T. ) ;
#18001 = ADVANCED_FACE ( 'NONE', ( #120052 ), #54861, .F. ) ;
#18000 = CARTESIAN_POINT ( 'NONE',  ( 25.39999999999999858, 0.000000000000000000, 0.000000000000000000 ) ) ;
#18002 = CARTESIAN_POINT ( 'NONE',  ( 0.000000000000000000, 1.761378380278681099, -6.096875308897254264 ) ) ;
#18003 = DIRECTION ( 'NONE',  ( 0.7071067811865486830, -0.7071067811865464625, -0.000000000000000000 ) ) ;
#18004 = LINE ( 'NONE', #126112, #123977 ) ;
#18005 = PLANE ( 'NONE',  #102598 ) ;
#18006 = CARTESIAN_POINT ( 'NONE',  ( 29.99999999999979750, 4.384688058510596953, -7.090945410444616570 ) ) ;
#18007 = DIRECTION ( 'NONE',  ( 0.7071067811865486830, -0.7071067811865464625, -0.000000000000000000 ) ) ;
#18008 = CARTESIAN_POINT ( 'NONE',  ( 61.46640106136304382, -43.15000000000001279, 34.92499999999998295 ) ) ;
#18009 = EDGE_CURVE ( 'NONE', #27663, #125881, #143269, .T. ) ;
#18010 = ORIENTED_EDGE ( 'NONE', *, *, #41523, .F. ) ;
#18011 = ORIENTED_EDGE ( 'NONE', *, *, #44136, .F. ) ;
#18012 = CARTESIAN_POINT ( 'NONE',  ( 98.00043019189810423, -3.055000000000002380, 5.291415217122920289 ) ) ;
#18013 = VECTOR ( 'NONE', #49347, 1000.000000000000227 ) ;
#18014 = ORIENTED_EDGE ( 'NONE', *, *, #58532, .T. ) ;
#18015 = EDGE_CURVE ( 'NONE', #23807, #3366, #119354, .T. ) ;
#18016 = CARTESIAN_POINT ( 'NONE',  ( -1.499999999999987566, -10.53360074219763121, 5.000000000000000000 ) ) ;
#18017 = CARTESIAN_POINT ( 'NONE',  ( -18.79289321881332242, -14.24070752338413648, 5.000000000000000000 ) ) ;
#18018 = ORIENTED_EDGE ( 'NONE', *, *, #108113, .F. ) ;
#18019 = CARTESIAN_POINT ( 'NONE',  ( 75.08333333333332860, 6.884901960086290629, -3.974999999999994316 ) ) ;
#18021 = EDGE_CURVE ( 'NONE', #116046, #72349, #21507, .T. ) ;
#18020 = DIRECTION ( 'NONE',  ( -0.000000000000000000, 0.000000000000000000, 1.000000000000000000 ) ) ;
#18022 = CARTESIAN_POINT ( 'NONE',  ( 95.14126352523143737, 4.472830434245836706, 4.472830434245840259 ) ) ;
#18023 = EDGE_CURVE ( 'NONE', #7112, #55621, #32386, .T. ) ;
#18024 = ORIENTED_EDGE ( 'NONE', *, *, #131323, .T. ) ;
#18025 = CARTESIAN_POINT ( 'NONE',  ( 17.29298673570682254, -21.74070752338406720, 4.999753212805220670 ) ) ;
#18026 = ORIENTED_EDGE ( 'NONE', *, *, #60411, .F. ) ;
#18027 = LINE ( 'NONE', #52812, #1362 ) ;
#18028 = DIRECTION ( 'NONE',  ( -0.000000000000000000, -0.000000000000000000, 1.000000000000000000 ) ) ;
#18029 = AXIS2_PLACEMENT_3D ( 'NONE', #141734, #140979, #30836 ) ;
#18030 = LINE ( 'NONE', #62311, #90185 ) ;
#18031 = EDGE_LOOP ( 'NONE', ( #65134, #77199, #60960, #71114 ) ) ;
#18032 = VERTEX_POINT ( 'NONE', #64294 ) ;
#18033 = VECTOR ( 'NONE', #116338, 1000.000000000000000 ) ;
#18034 = ORIENTED_EDGE ( 'NONE', *, *, #91827, .F. ) ;
#18035 = DIRECTION ( 'NONE',  ( 0.7071067811865486830, -0.7071067811865464625, -0.000000000000000000 ) ) ;
#18036 = EDGE_CURVE ( 'NONE', #37816, #67034, #7741, .T. ) ;
#18037 = LINE ( 'NONE', #138441, #12965 ) ;
#18038 = CARTESIAN_POINT ( 'NONE',  ( 7.650403141435218934, 7.934999999999988951, -2.126176841940961904 ) ) ;
#18039 = VECTOR ( 'NONE', #76263, 1000.000000000000227 ) ;
#18040 = VECTOR ( 'NONE', #2941, 1000.000000000000000 ) ;
#18041 = LINE ( 'NONE', #41250, #115001 ) ;
#18042 = EDGE_LOOP ( 'NONE', ( #75263, #61863, #81232, #2864 ) ) ;
#18043 = ORIENTED_EDGE ( 'NONE', *, *, #138932, .F. ) ;
#18044 = DIRECTION ( 'NONE',  ( -0.7071067811865486830, -0.7071067811865464625, 0.000000000000000000 ) ) ;
#18045 = VERTEX_POINT ( 'NONE', #84622 ) ;
#18046 = ORIENTED_EDGE ( 'NONE', *, *, #13906, .T. ) ;
#18047 = CARTESIAN_POINT ( 'NONE',  ( 17.50000000000000000, 0.000000000000000000, 6.094999999999989981 ) ) ;
#18048 = CARTESIAN_POINT ( 'NONE',  ( -28.49999999999979750, 3.073033219394599058, -6.593910359671034449 ) ) ;
#18049 = VERTEX_POINT ( 'NONE', #41106 ) ;
#18050 = DIRECTION ( 'NONE',  ( -0.7071067811865486830, 0.7071067811865464625, 0.000000000000000000 ) ) ;
#18051 = EDGE_CURVE ( 'NONE', #43580, #104227, #128823, .T. ) ;
#18052 = LINE ( 'NONE', #62341, #77980 ) ;
#18053 = DIRECTION ( 'NONE',  ( 0.000000000000000000, -1.000000000000000000, 0.000000000000000000 ) ) ;
#18054 = LINE ( 'NONE', #41267, #55994 ) ;
#18055 = ORIENTED_EDGE ( 'NONE', *, *, #97627, .T. ) ;
#18056 = AXIS2_PLACEMENT_3D ( 'NONE', #50288, #40829, #29929 ) ;
#18057 = LINE ( 'NONE', #93527, #4639 ) ;
#18058 = FACE_BOUND ( 'NONE', #12050, .T. ) ;
#18059 = ORIENTED_EDGE ( 'NONE', *, *, #47667, .F. ) ;
#18060 = CARTESIAN_POINT ( 'NONE',  ( 25.39999999999999503, 2.515948873491120175, -7.536568151888201506 ) ) ;
#18061 = CARTESIAN_POINT ( 'NONE',  ( 1.042387978378689573, -0.4000000000000003553, 2.015694669338588429 ) ) ;
#18062 = LINE ( 'NONE', #53609, #123316 ) ;
#18064 = EDGE_LOOP ( 'NONE', ( #113373, #102825, #55394, #5309 ) ) ;
#18063 = EDGE_CURVE ( 'NONE', #127570, #45162, #67907, .T. ) ;
#18065 = CARTESIAN_POINT ( 'NONE',  ( 4.499999999999974243, 21.05218569542895679, 5.000000000000000000 ) ) ;
#18066 = EDGE_LOOP ( 'NONE', ( #48211, #85871, #131204, #105891 ) ) ;
#18067 = AXIS2_PLACEMENT_3D ( 'NONE', #44177, #65953, #78232 ) ;
#18068 = VERTEX_POINT ( 'NONE', #126339 ) ;
#18069 = EDGE_LOOP ( 'NONE', ( #80922, #85875, #82470, #19630 ) ) ;
#18070 = ADVANCED_FACE ( 'NONE', ( #22187 ), #46132, .F. ) ;
#18071 = CARTESIAN_POINT ( 'NONE',  ( 26.45376352523144803, -6.109999999999998543, -3.741295971395162543E-16 ) ) ;
#18072 = LINE ( 'NONE', #126175, #52972 ) ;
#18074 = ADVANCED_FACE ( 'NONE', ( #114728 ), #103840, .F. ) ;
#18073 = LINE ( 'NONE', #52861, #31051 ) ;
#18075 = LINE ( 'NONE', #61656, #46250 ) ;
#18076 = CARTESIAN_POINT ( 'NONE',  ( 14.67183060077636725, 14.25929247661557042, 4.000000000000000000 ) ) ;
#18077 = EDGE_CURVE ( 'NONE', #67478, #143446, #1829, .T. ) ;
#18078 = DIRECTION ( 'NONE',  ( -0.000000000000000000, 0.3543493200069153248, 0.9351131265310292928 ) ) ;
#18079 = DIRECTION ( 'NONE',  ( -0.000000000000000000, 0.000000000000000000, 1.000000000000000000 ) ) ;
#18080 = VECTOR ( 'NONE', #24541, 1000.000000000000000 ) ;
#18081 = ADVANCED_FACE ( 'NONE', ( #112093 ), #48797, .T. ) ;
#18082 = DIRECTION ( 'NONE',  ( 0.7071067811865486830, -0.7071067811865464625, -0.000000000000000000 ) ) ;
#18083 = CARTESIAN_POINT ( 'NONE',  ( -39.48921356237310221, -27.52281430457082934, 5.000000000000000000 ) ) ;
#18084 = DIRECTION ( 'NONE',  ( -1.000000000000000000, -0.000000000000000000, -0.000000000000000000 ) ) ;
#18085 = CARTESIAN_POINT ( 'NONE',  ( 13.84116387061258457, 6.089959206779446355, 4.000000000000000000 ) ) ;
#18086 = EDGE_CURVE ( 'NONE', #22993, #21534, #16113, .T. ) ;
#18087 = ORIENTED_EDGE ( 'NONE', *, *, #9508, .F. ) ;
#18088 = VERTEX_POINT ( 'NONE', #82162 ) ;
#18089 = EDGE_LOOP ( 'NONE', ( #77156, #46075, #75331, #4352 ) ) ;
#18090 = ORIENTED_EDGE ( 'NONE', *, *, #86206, .T. ) ;
#18091 = DIRECTION ( 'NONE',  ( 1.000000000000000000, 0.000000000000000000, 0.000000000000000000 ) ) ;
#18092 = ORIENTED_EDGE ( 'NONE', *, *, #22680, .F. ) ;
#18093 = ORIENTED_EDGE ( 'NONE', *, *, #49086, .F. ) ;
#18094 = CARTESIAN_POINT ( 'NONE',  ( -51.18398860626899705, 28.73617430169823095, 5.000000000000000000 ) ) ;
#18095 = CARTESIAN_POINT ( 'NONE',  ( 0.000000000000000000, 0.000000000000000000, 5.000000000000000000 ) ) ;
#18097 = EDGE_CURVE ( 'NONE', #81966, #87517, #84065, .T. ) ;
#18096 = DIRECTION ( 'NONE',  ( -0.3543493200069162685, -0.000000000000000000, -0.9351131265310288487 ) ) ;
#18098 = ADVANCED_FACE ( 'NONE', ( #122217 ), #57014, .F. ) ;
#18099 = DIRECTION ( 'NONE',  ( -0.6830127018922180770, -0.6830127018922204085, -0.2588190451025213501 ) ) ;
#18100 = ORIENTED_EDGE ( 'NONE', *, *, #11391, .F. ) ;
#18101 = CARTESIAN_POINT ( 'NONE',  ( 24.21271579574130683, 0.1791150535437372460, 5.000000000000000000 ) ) ;
#18102 = ORIENTED_EDGE ( 'NONE', *, *, #35864, .F. ) ;
#18103 = EDGE_CURVE ( 'NONE', #84862, #129515, #67153, .T. ) ;
#18104 = LINE ( 'NONE', #93572, #76861 ) ;
#18105 = PLANE ( 'NONE',  #40379 ) ;
#18106 = CARTESIAN_POINT ( 'NONE',  ( 6.921236474768553748, -9.717572351234235426E-16, -7.934999999999990727 ) ) ;
#18107 = VERTEX_POINT ( 'NONE', #59682 ) ;
#18108 = CARTESIAN_POINT ( 'NONE',  ( 93.82876352523145158, 0.000000000000000000, -6.109999999999999432 ) ) ;
#18109 = VECTOR ( 'NONE', #112453, 1000.000000000000227 ) ;
#18110 = SURFACE_SIDE_STYLE ('',( #59043 ) ) ;
#18111 = DIRECTION ( 'NONE',  ( 1.000000000000000000, 0.000000000000000000, 0.000000000000000000 ) ) ;
#18112 = ORIENTED_EDGE ( 'NONE', *, *, #108895, .T. ) ;
#18113 = ORIENTED_EDGE ( 'NONE', *, *, #39306, .F. ) ;
#18114 = DIRECTION ( 'NONE',  ( 0.000000000000000000, 0.000000000000000000, -1.000000000000000000 ) ) ;
#18115 = VERTEX_POINT ( 'NONE', #37191 ) ;
#18116 = CARTESIAN_POINT ( 'NONE',  ( -21.18398860626899349, 28.73617430169802134, 5.000000000000000000 ) ) ;
#18117 = CARTESIAN_POINT ( 'NONE',  ( -23.99451991528749062, 28.92564299267954908, 4.000000000000000000 ) ) ;
#18118 = DIRECTION ( 'NONE',  ( -0.7071067811865486830, -0.7071067811865463515, 0.000000000000000000 ) ) ;
#18119 = CARTESIAN_POINT ( 'NONE',  ( -23.99999999999982592, -22.22500000000000853, 4.412002311790067743 ) ) ;
#18120 = CARTESIAN_POINT ( 'NONE',  ( 181.1395720402182974, -48.08977582060997946, -37.49964900842754645 ) ) ;
#18121 = VERTEX_POINT ( 'NONE', #4491 ) ;
#18122 = DIRECTION ( 'NONE',  ( 0.7071067811865486830, -0.7071067811865464625, -0.000000000000000000 ) ) ;
#18123 = AXIS2_PLACEMENT_3D ( 'NONE', #22580, #68314, #92139 ) ;
#18124 = CARTESIAN_POINT ( 'NONE',  ( -8.994519915287490619, 28.92564299267944250, 4.000000000000000000 ) ) ;
#18125 = LINE ( 'NONE', #117454, #86225 ) ;
#18126 = ADVANCED_FACE ( 'NONE', ( #122958 ), #88925, .T. ) ;
#18127 = ORIENTED_EDGE ( 'NONE', *, *, #34084, .F. ) ;
#18128 = CARTESIAN_POINT ( 'NONE',  ( 34.49999999999975131, -5.945670655168991736, 4.994342998332164996 ) ) ;
#18129 = VECTOR ( 'NONE', #55027, 1000.000000000000000 ) ;
#18130 = AXIS2_PLACEMENT_3D ( 'NONE', #23872, #59379, #12964 ) ;
#18131 = LINE ( 'NONE', #106575, #67967 ) ;
#18132 = ORIENTED_EDGE ( 'NONE', *, *, #49739, .T. ) ;
#18133 = VECTOR ( 'NONE', #10236, 1000.000000000000000 ) ;
#18135 = ORIENTED_EDGE ( 'NONE', *, *, #67174, .T. ) ;
#18134 = DIRECTION ( 'NONE',  ( -0.6830127018922180770, -0.6830127018922204085, -0.2588190451025213501 ) ) ;
#18136 = AXIS2_PLACEMENT_3D ( 'NONE', #17951, #19413, #94805 ) ;
#18137 = CARTESIAN_POINT ( 'NONE',  ( -34.92500000000001137, 12.95788372223792528, 1.488343219358023939 ) ) ;
#18138 = LINE ( 'NONE', #106581, #62295 ) ;
#18139 = VECTOR ( 'NONE', #50761, 1000.000000000000000 ) ;
#18140 = ORIENTED_EDGE ( 'NONE', *, *, #110779, .F. ) ;
#18141 = FACE_OUTER_BOUND ( 'NONE', #94402, .T. ) ;
#18142 = VECTOR ( 'NONE', #29226, 999.9999999999998863 ) ;
#18143 = EDGE_CURVE ( 'NONE', #75982, #108304, #111343, .T. ) ;
#18144 = LINE ( 'NONE', #105877, #70683 ) ;
#18145 = SURFACE_STYLE_FILL_AREA ( #26917 ) ;
#18146 = DIRECTION ( 'NONE',  ( 0.7071067811865487940, -0.7071067811865463515, 0.000000000000000000 ) ) ;
#18147 = CARTESIAN_POINT ( 'NONE',  ( -36.48921356237310221, -27.52281430457080802, 5.000000000000000000 ) ) ;
#18148 = EDGE_CURVE ( 'NONE', #9583, #133905, #77349, .T. ) ;
#18149 = DIRECTION ( 'NONE',  ( 0.3543493200069162685, -0.000000000000000000, -0.9351131265310288487 ) ) ;
#18150 = DIRECTION ( 'NONE',  ( 0.7071067811865487940, 0.7071067811865463515, -0.000000000000000000 ) ) ;
#18151 = DIRECTION ( 'NONE',  ( 0.6830127018922180770, -0.6830127018922204085, -0.2588190451025213501 ) ) ;
#18152 = DIRECTION ( 'NONE',  ( -0.7071067811865487940, 0.7071067811865463515, 0.000000000000000000 ) ) ;
#18153 = CARTESIAN_POINT ( 'NONE',  ( -17.99451991528748351, 28.92564299267950645, 4.000000000000000000 ) ) ;
#18154 = CARTESIAN_POINT ( 'NONE',  ( 8.999999999999944933, 4.384688058510572972, -7.090945410444662755 ) ) ;
#18155 = CARTESIAN_POINT ( 'NONE',  ( 23.20710678118638626, -14.24070752338414536, 5.000000000000000000 ) ) ;
#18156 = VERTEX_POINT ( 'NONE', #71269 ) ;
#18157 = ORIENTED_EDGE ( 'NONE', *, *, #50372, .F. ) ;
#18158 = ORIENTED_EDGE ( 'NONE', *, *, #76231, .T. ) ;
#18159 = CARTESIAN_POINT ( 'NONE',  ( 108.3333333333333428, -6.884901960086287964, 3.974999999999998312 ) ) ;
#18160 = VECTOR ( 'NONE', #36219, 1000.000000000000000 ) ;
#18161 = EDGE_LOOP ( 'NONE', ( #8393, #125638, #63101, #142791 ) ) ;
#18162 = EDGE_LOOP ( 'NONE', ( #12291, #124677, #5086, #62056 ) ) ;
#18163 = ADVANCED_FACE ( 'NONE', ( #104588 ), #56319, .F. ) ;
#18164 = ORIENTED_EDGE ( 'NONE', *, *, #98814, .T. ) ;
#18165 = CARTESIAN_POINT ( 'NONE',  ( 47.99451991528749062, 28.92564299267971251, 4.000000000000000000 ) ) ;
#18166 = VECTOR ( 'NONE', #127500, 1000.000000000000000 ) ;
#18167 = LINE ( 'NONE', #5152, #141216 ) ;
#18168 = VERTEX_POINT ( 'NONE', #100499 ) ;
#18169 = DIRECTION ( 'NONE',  ( 0.7071067811865487940, 0.7071067811865463515, 0.000000000000000000 ) ) ;
#18170 = AXIS2_PLACEMENT_3D ( 'NONE', #73816, #105694, #140483 ) ;
#18171 = DIRECTION ( 'NONE',  ( -1.000000000000000000, -0.000000000000000000, -0.000000000000000000 ) ) ;
#18172 = DIRECTION ( 'NONE',  ( -0.6830127018922181881, 0.6830127018922202975, -0.2588190451025214056 ) ) ;
#18173 = DIRECTION ( 'NONE',  ( 0.6830127018922180770, -0.6830127018922204085, -0.2588190451025213501 ) ) ;
#18174 = CARTESIAN_POINT ( 'NONE',  ( 99.45876352523144703, 0.000000000000000000, -6.110000000000001208 ) ) ;
#18175 = EDGE_CURVE ( 'NONE', #19828, #13154, #23636, .T. ) ;
#18176 = EDGE_LOOP ( 'NONE', ( #132395, #53154, #114863, #72607 ) ) ;
#18177 = DIRECTION ( 'NONE',  ( -0.7071067811865486830, 0.7071067811865464625, 0.000000000000000000 ) ) ;
#18178 = CARTESIAN_POINT ( 'NONE',  ( 0.000000000000000000, -49.85820393249936444, -34.92499999999998295 ) ) ;
#18179 = CARTESIAN_POINT ( 'NONE',  ( 83.05836038379621300, -7.949999999999996625, -2.130196079827426203 ) ) ;
#18180 = CYLINDRICAL_SURFACE ( 'NONE', #140094, 2.500000000000000444 ) ;
#18181 = VECTOR ( 'NONE', #73832, 1000.000000000000000 ) ;
#18182 = DIRECTION ( 'NONE',  ( -0.7071067811865486830, -0.7071067811865464625, 0.000000000000000000 ) ) ;
#18183 = FACE_OUTER_BOUND ( 'NONE', #38565, .T. ) ;
#18184 = CARTESIAN_POINT ( 'NONE',  ( 40.91252705046288440, -7.949999999999998401, -4.867971026610728450E-16 ) ) ;
#18185 = LINE ( 'NONE', #8721, #104600 ) ;
#18186 = CARTESIAN_POINT ( 'NONE',  ( -34.92500000000001137, 22.22500000000000142, 4.000000000000000000 ) ) ;
#18187 = EDGE_LOOP ( 'NONE', ( #136546, #105778, #124315, #83485 ) ) ;
#18188 = ORIENTED_EDGE ( 'NONE', *, *, #108773, .T. ) ;
#18189 = CARTESIAN_POINT ( 'NONE',  ( 125.5629301918981042, 1.637169565754157174, 6.110000000000002984 ) ) ;
#18190 = ORIENTED_EDGE ( 'NONE', *, *, #120509, .F. ) ;
#18191 = DIRECTION ( 'NONE',  ( -0.7071067811865486830, -0.7071067811865464625, -0.000000000000000000 ) ) ;
#18192 = LINE ( 'NONE', #105928, #57074 ) ;
#18193 = VECTOR ( 'NONE', #109810, 1000.000000000000000 ) ;
#18194 = DIRECTION ( 'NONE',  ( -0.000000000000000000, 0.000000000000000000, 1.000000000000000000 ) ) ;
#18195 = EDGE_CURVE ( 'NONE', #121192, #69181, #40085, .T. ) ;
#18197 = VECTOR ( 'NONE', #119787, 1000.000000000000000 ) ;
#18196 = PLANE ( 'NONE',  #16820 ) ;
#18198 = LINE ( 'NONE', #129854, #7330 ) ;
#18199 = FILL_AREA_STYLE ('',( #29116 ) ) ;
#18200 = CARTESIAN_POINT ( 'NONE',  ( 122.5579301918981088, 6.110000000000000320, -1.637169565754156064 ) ) ;
#18201 = ADVANCED_FACE ( 'NONE', ( #83575 ), #95848, .F. ) ;
#18202 = EDGE_LOOP ( 'NONE', ( #24361, #32154, #113453, #103706 ) ) ;
#18203 = DIRECTION ( 'NONE',  ( -0.5735764363510503783, -0.8191520442889886899, 0.000000000000000000 ) ) ;
#18204 = ORIENTED_EDGE ( 'NONE', *, *, #61364, .T. ) ;
#18205 = DIRECTION ( 'NONE',  ( -0.7071067811865486830, -0.7071067811865464625, -0.000000000000000000 ) ) ;
#18206 = CYLINDRICAL_SURFACE ( 'NONE', #8417, 2.552699999999994418 ) ;
#18207 = DIRECTION ( 'NONE',  ( 0.7071067811865487940, 0.7071067811865463515, -0.000000000000000000 ) ) ;
#18208 = LINE ( 'NONE', #63909, #85754 ) ;
#18210 = EDGE_CURVE ( 'NONE', #139467, #115804, #61148, .T. ) ;
#18209 = EDGE_LOOP ( 'NONE', ( #56222, #52445, #107958, #69287 ) ) ;
#18211 = CARTESIAN_POINT ( 'NONE',  ( 49.87543019189810423, -5.291415217122920289, -3.055000000000001492 ) ) ;
#18212 = ORIENTED_EDGE ( 'NONE', *, *, #131358, .F. ) ;
#18213 = DIRECTION ( 'NONE',  ( -0.000000000000000000, 0.000000000000000000, 1.000000000000000000 ) ) ;
#18214 = EDGE_CURVE ( 'NONE', #51507, #121969, #7392, .T. ) ;
#18215 = PLANE ( 'NONE',  #11442 ) ;
#18216 = CARTESIAN_POINT ( 'NONE',  ( -34.92500000000001137, 10.51246187583939395, 4.000000000000000000 ) ) ;
#18217 = CARTESIAN_POINT ( 'NONE',  ( 31.36246187583879674, 22.22500000000000142, 4.000000000000000000 ) ) ;
#18218 = PRODUCT_RELATED_PRODUCT_CATEGORY ( 'part', '', ( #72462 ) ) ;
#18219 = CARTESIAN_POINT ( 'NONE',  ( 47.30793019189811588, -6.109999999999998543, 1.637169565754158063 ) ) ;
#18220 = ORIENTED_EDGE ( 'NONE', *, *, #121798, .F. ) ;
#18221 = CARTESIAN_POINT ( 'NONE',  ( 1.171830600776465392, 9.759292476615627265, 4.000000000000000000 ) ) ;
#18222 = PLANE ( 'NONE',  #110371 ) ;
#18223 = ORIENTED_EDGE ( 'NONE', *, *, #6618, .T. ) ;
#18224 = ORIENTED_EDGE ( 'NONE', *, *, #119546, .T. ) ;
#18225 = ORIENTED_EDGE ( 'NONE', *, *, #114224, .T. ) ;
#18226 = EDGE_CURVE ( 'NONE', #118457, #38058, #113651, .T. ) ;
#18227 = AXIS2_PLACEMENT_3D ( 'NONE', #61013, #94290, #131213 ) ;
#18228 = LINE ( 'NONE', #115394, #56104 ) ;
#18229 = ORIENTED_EDGE ( 'NONE', *, *, #4194, .T. ) ;
#18230 = CARTESIAN_POINT ( 'NONE',  ( 44.55836038379621300, -7.949999999999996625, -2.130196079827426203 ) ) ;
#18231 = VECTOR ( 'NONE', #114209, 999.9999999999998863 ) ;
#18232 = AXIS2_PLACEMENT_3D ( 'NONE', #19242, #109091, #64186 ) ;
#18233 = CONICAL_SURFACE ( 'NONE', #8896, 2.055000000000000604, 0.9599310885968764806 ) ;
#18234 = DIRECTION ( 'NONE',  ( -0.7071067811865487940, 0.7071067811865463515, -0.000000000000000000 ) ) ;
#18235 = AXIS2_PLACEMENT_3D ( 'NONE', #131148, #23061, #142737 ) ;
#18236 = FACE_BOUND ( 'NONE', #26236, .T. ) ;
#18237 = LINE ( 'NONE', #62519, #82742 ) ;
#18238 = CARTESIAN_POINT ( 'NONE',  ( 23.99999999999983302, -9.412538124160661823, 4.000000000000000000 ) ) ;
#18239 = CARTESIAN_POINT ( 'NONE',  ( -8.816011393731004731, 28.73617430169781173, 5.000000000000000000 ) ) ;
#18240 = ORIENTED_EDGE ( 'NONE', *, *, #74596, .F. ) ;
#18241 = PLANE ( 'NONE',  #22600 ) ;
#18242 = ORIENTED_EDGE ( 'NONE', *, *, #27836, .F. ) ;
#18243 = ORIENTED_EDGE ( 'NONE', *, *, #59968, .F. ) ;
#18244 = AXIS2_PLACEMENT_3D ( 'NONE', #74510, #118695, #120088 ) ;
#18245 = COLOUR_RGB ( '', 0.40784314, 0.44705882, 0.49803922) ;
#18246 = DIRECTION ( 'NONE',  ( 0.000000000000000000, 0.000000000000000000, 1.000000000000000000 ) ) ;
#18247 = EDGE_LOOP ( 'NONE', ( #16706, #21337, #88581, #70164 ) ) ;
#18248 = EDGE_CURVE ( 'NONE', #69267, #103049, #45004, .T. ) ;
#18249 = CARTESIAN_POINT ( 'NONE',  ( 57.37043019189810877, -3.055000000000001492, 5.291415217122917625 ) ) ;
#18250 = ORIENTED_EDGE ( 'NONE', *, *, #135892, .T. ) ;
#18251 = CARTESIAN_POINT ( 'NONE',  ( -69.48921356237309510, -27.52281430457103895, 5.000000000000000000 ) ) ;
#18252 = ADVANCED_FACE ( 'NONE', ( #85674 ), #28475, .F. ) ;
#18253 = CARTESIAN_POINT ( 'NONE',  ( -14.99999999999988987, -12.41253812416063163, 4.000000000000000000 ) ) ;
#18254 = ORIENTED_EDGE ( 'NONE', *, *, #59434, .T. ) ;
#18255 = CARTESIAN_POINT ( 'NONE',  ( 15.18398860626900237, 28.73617430169797871, 5.000000000000000000 ) ) ;
#18256 = AXIS2_PLACEMENT_3D ( 'NONE', #42814, #74733, #142816 ) ;
#18257 = EDGE_CURVE ( 'NONE', #88566, #52144, #30619, .T. ) ;
#18258 = EDGE_CURVE ( 'NONE', #136293, #131560, #63269, .T. ) ;
#18259 = VECTOR ( 'NONE', #32313, 1000.000000000000000 ) ;
#18260 = DIRECTION ( 'NONE',  ( -0.7071067811865487940, 0.7071067811865463515, 0.000000000000000000 ) ) ;
#18261 = PLANE ( 'NONE',  #94510 ) ;
#18262 = LINE ( 'NONE', #106709, #18039 ) ;
#18263 = LINE ( 'NONE', #48807, #90926 ) ;
#18264 = CARTESIAN_POINT ( 'NONE',  ( 23.70025512860841133, -27.71228299555189523, 4.000000000000000000 ) ) ;
#18265 = ORIENTED_EDGE ( 'NONE', *, *, #106262, .F. ) ;
#18266 = VERTEX_POINT ( 'NONE', #18253 ) ;
#18267 = VECTOR ( 'NONE', #82276, 1000.000000000000000 ) ;
#18268 = DIRECTION ( 'NONE',  ( 2.496005001405478586E-15, 1.000000000000000000, -0.000000000000000000 ) ) ;
#18269 = DIRECTION ( 'NONE',  ( 0.6830127018922180770, -0.6830127018922204085, -0.2588190451025213501 ) ) ;
#18270 = VERTEX_POINT ( 'NONE', #96530 ) ;
#18271 = AXIS2_PLACEMENT_3D ( 'NONE', #131605, #76526, #120701 ) ;
#18272 = ORIENTED_EDGE ( 'NONE', *, *, #126773, .F. ) ;
#18273 = AXIS2_PLACEMENT_3D ( 'NONE', #101259, #77408, #22948 ) ;
#18274 = ORIENTED_EDGE ( 'NONE', *, *, #13215, .T. ) ;
#18275 = CARTESIAN_POINT ( 'NONE',  ( -30.48921356237309510, -27.52281430457076894, 5.000000000000000000 ) ) ;
#18276 = EDGE_CURVE ( 'NONE', #16863, #129679, #119025, .T. ) ;
#18277 = EDGE_CURVE ( 'NONE', #129125, #25409, #116889, .T. ) ;
#18278 = FACE_OUTER_BOUND ( 'NONE', #63053, .T. ) ;
#18279 = VERTEX_POINT ( 'NONE', #62533 ) ;
#18280 = VECTOR ( 'NONE', #79602, 1000.000000000000000 ) ;
#18281 = CARTESIAN_POINT ( 'NONE',  ( 41.99451991528749062, 28.92564299267967343, 4.000000000000000000 ) ) ;
#18282 = VECTOR ( 'NONE', #35458, 1000.000000000000000 ) ;
#18283 = ADVANCED_FACE ( 'NONE', ( #140095 ), #49535, .F. ) ;
#18284 = CARTESIAN_POINT ( 'NONE',  ( 6.337903141435219823, -6.871911579029513106, -3.967499999999993587 ) ) ;
#18285 = LINE ( 'NONE', #51681, #28710 ) ;
#18286 = ORIENTED_EDGE ( 'NONE', *, *, #62092, .T. ) ;
#18287 = CARTESIAN_POINT ( 'NONE',  ( 127.6620968585647802, -5.291415217122919401, 3.054999999999998384 ) ) ;
#18288 = DIRECTION ( 'NONE',  ( 0.000000000000000000, -1.000000000000000000, 0.000000000000000000 ) ) ;
#18289 = DIRECTION ( 'NONE',  ( -0.7071067811865486830, -0.7071067811865464625, 0.000000000000000000 ) ) ;
#18290 = ADVANCED_FACE ( 'NONE', ( #39356 ), #129180, .F. ) ;
#18291 = VECTOR ( 'NONE', #34228, 1000.000000000000000 ) ;
#18293 = VERTEX_POINT ( 'NONE', #72737 ) ;
#18292 = DIRECTION ( 'NONE',  ( 0.000000000000000000, -1.000000000000000000, 0.000000000000000000 ) ) ;
#18294 = CARTESIAN_POINT ( 'NONE',  ( 11.12913961620377101, 5.278424836066147208, 3.047499999999990550 ) ) ;
#18295 = EDGE_LOOP ( 'NONE', ( #88554, #101503, #21158 ) ) ;
#18296 = CARTESIAN_POINT ( 'NONE',  ( 75.76669371712954160, -7.949999999999998401, 2.130196079827423983 ) ) ;
#18297 = LINE ( 'NONE', #42254, #135016 ) ;
#18298 = CARTESIAN_POINT ( 'NONE',  ( 108.0416666666666714, -3.975000000000002753, 6.884901960086286188 ) ) ;
#18299 = ORIENTED_EDGE ( 'NONE', *, *, #115303, .T. ) ;
#18300 = DIRECTION ( 'NONE',  ( -0.6830127018922181881, 0.6830127018922202975, -0.2588190451025214056 ) ) ;
#18301 = CARTESIAN_POINT ( 'NONE',  ( 10.40832548098994614, -0.7407075233842770334, 14.76736230305383124 ) ) ;
#18302 = FACE_OUTER_BOUND ( 'NONE', #27934, .T. ) ;
#18303 = EDGE_CURVE ( 'NONE', #121955, #110155, #118300, .T. ) ;
#18304 = ORIENTED_EDGE ( 'NONE', *, *, #53359, .T. ) ;
#18305 = CARTESIAN_POINT ( 'NONE',  ( 7.499999999999944045, -1.592773361805365662, -6.492772025301245087 ) ) ;
#18306 = CARTESIAN_POINT ( 'NONE',  ( 29.99999999999979750, 7.007997736742478168, -8.085015511992047266 ) ) ;
#18307 = DIRECTION ( 'NONE',  ( -0.7071067811865486830, -0.7071067811865464625, 0.000000000000000000 ) ) ;
#18308 = LINE ( 'NONE', #108891, #70397 ) ;
#18309 = DIRECTION ( 'NONE',  ( 1.000000000000000000, 0.000000000000000000, 0.000000000000000000 ) ) ;
#18310 = ORIENTED_EDGE ( 'NONE', *, *, #91077, .T. ) ;
#18311 = ORIENTED_EDGE ( 'NONE', *, *, #74417, .T. ) ;
#18312 = DIRECTION ( 'NONE',  ( -0.3543493200069162685, -0.000000000000000000, -0.9351131265310288487 ) ) ;
#18313 = CARTESIAN_POINT ( 'NONE',  ( 0.000000000000000000, 0.000000000000000000, 5.000000000000000000 ) ) ;
#18314 = EDGE_CURVE ( 'NONE', #22706, #83800, #52342, .T. ) ;
#18315 = CARTESIAN_POINT ( 'NONE',  ( 15.43706980810188512, 2.126176841940952134, -7.934999999999993392 ) ) ;
#18316 = DIRECTION ( 'NONE',  ( 1.000000000000000000, 0.000000000000000000, 0.000000000000000000 ) ) ;
#18317 = LINE ( 'NONE', #118367, #41349 ) ;
#18318 = FACE_OUTER_BOUND ( 'NONE', #126621, .T. ) ;
#18319 = VERTEX_POINT ( 'NONE', #61825 ) ;
#18320 = CARTESIAN_POINT ( 'NONE',  ( 12.19999999999999574, -40.43000000000000682, -39.50000000000000000 ) ) ;
#18321 = CARTESIAN_POINT ( 'NONE',  ( 128.5894344200537489, -52.00875322212550600, 39.86617647058822911 ) ) ;
#18322 = CARTESIAN_POINT ( 'NONE',  ( 4.858306282870439752, -1.633150327867700202, 6.094999999999985540 ) ) ;
#18323 = CARTESIAN_POINT ( 'NONE',  ( 0.4892135623730947680, -27.52281430457055578, 5.000000000000000000 ) ) ;
#18324 = CARTESIAN_POINT ( 'NONE',  ( 36.95376352523144448, -6.109999999999999432, -3.741295971395163529E-16 ) ) ;
#18325 = DIRECTION ( 'NONE',  ( 0.7071067811865486830, -0.7071067811865464625, -0.000000000000000000 ) ) ;
#18326 = ORIENTED_EDGE ( 'NONE', *, *, #138877, .T. ) ;
#18327 = DIRECTION ( 'NONE',  ( -0.000000000000000000, 0.3543493200069153248, 0.9351131265310292928 ) ) ;
#18328 = VECTOR ( 'NONE', #129059, 999.9999999999998863 ) ;
#18329 = EDGE_LOOP ( 'NONE', ( #112922, #130805, #85876, #7050 ) ) ;
#18330 = ADVANCED_FACE ( 'NONE', ( #137950 ), #38627, .F. ) ;
#18331 = ORIENTED_EDGE ( 'NONE', *, *, #74463, .T. ) ;
#18332 = FACE_OUTER_BOUND ( 'NONE', #65457, .T. ) ;
#18333 = VECTOR ( 'NONE', #71099, 1000.000000000000000 ) ;
#18334 = VECTOR ( 'NONE', #3188, 1000.000000000000000 ) ;
#18335 = AXIS2_PLACEMENT_3D ( 'NONE', #65721, #86724, #43221 ) ;
#18336 = LINE ( 'NONE', #39440, #99408 ) ;
#18337 = LINE ( 'NONE', #61910, #2506 ) ;
#18338 = VECTOR ( 'NONE', #39707, 1000.000000000000000 ) ;
#18339 = CARTESIAN_POINT ( 'NONE',  ( 27.79333936457828358, 21.75929247661549226, 4.998822639870708073 ) ) ;
#18340 = CARTESIAN_POINT ( 'NONE',  ( 81.93750000000000000, 5.819803920172574863, -5.819803920172573086 ) ) ;
#18341 = CARTESIAN_POINT ( 'NONE',  ( 30.18398860626900060, 28.73617430169808173, 5.000000000000000000 ) ) ;
#18342 = EDGE_CURVE ( 'NONE', #28284, #56879, #132069, .T. ) ;
#18343 = ORIENTED_EDGE ( 'NONE', *, *, #118922, .T. ) ;
#18344 = CARTESIAN_POINT ( 'NONE',  ( -31.49999999999977973, 16.18958161055400069, -11.56426086740818704 ) ) ;
#18345 = DIRECTION ( 'NONE',  ( -0.6830127018922181881, 0.6830127018922202975, -0.2588190451025214056 ) ) ;
#18346 = CARTESIAN_POINT ( 'NONE',  ( 7.689442160698723328, -22.22500000000000142, 21.14820514618944713 ) ) ;
#18347 = VECTOR ( 'NONE', #3536, 1000.000000000000000 ) ;
#18348 = DIRECTION ( 'NONE',  ( 1.000000000000000000, 0.000000000000000000, 0.000000000000000000 ) ) ;
#18349 = DIRECTION ( 'NONE',  ( -0.6830127018922181881, 0.6830127018922202975, -0.2588190451025214056 ) ) ;
#18350 = DIRECTION ( 'NONE',  ( -0.6830127018922181881, 0.6830127018922202975, -0.2588190451025214056 ) ) ;
#18351 = CARTESIAN_POINT ( 'NONE',  ( 70.22502705046287019, 5.819803920172573086, -5.819803920172572198 ) ) ;
#18352 = PLANE ( 'NONE',  #94744 ) ;
#18353 = EDGE_LOOP ( 'NONE', ( #5985, #68071, #143528, #6752 ) ) ;
#18354 = EDGE_LOOP ( 'NONE', ( #49112, #69125, #113431, #111599 ) ) ;
#18355 =( BOUNDED_CURVE ( )  B_SPLINE_CURVE ( 3, ( #13439, #125082, #122210, #78036 ),
 .UNSPECIFIED., .F., .T. ) 
 B_SPLINE_CURVE_WITH_KNOTS ( ( 4, 4 ),
 ( 1.864375635226952044, 1.933014472006561624 ),
 .UNSPECIFIED. ) 
 CURVE ( )  GEOMETRIC_REPRESENTATION_ITEM ( )  RATIONAL_B_SPLINE_CURVE ( ( 1.000000000000000000, 0.9996074310407765395, 0.9996074310407765395, 1.000000000000000000 ) ) 
 REPRESENTATION_ITEM ( '' )  );
#18356 = CARTESIAN_POINT ( 'NONE',  ( 53.06250000000000000, -5.819803920172572198, -5.819803920172573086 ) ) ;
#18357 = CARTESIAN_POINT ( 'NONE',  ( -32.20710678118632586, 9.759292476615627265, 5.000000000000000000 ) ) ;
#18358 = CARTESIAN_POINT ( 'NONE',  ( -23.99999999999982592, 19.55218569542896390, 5.000000000000000000 ) ) ;
#18359 = VECTOR ( 'NONE', #73129, 1000.000000000000000 ) ;
#18360 = CIRCLE ( 'NONE', #4462, 2.500000000000000888 ) ;
#18361 = CARTESIAN_POINT ( 'NONE',  ( 24.39999999999999858, -2.600000000000060929, 28.92500000000001492 ) ) ;
#18362 = ORIENTED_EDGE ( 'NONE', *, *, #21080, .T. ) ;
#18363 = CARTESIAN_POINT ( 'NONE',  ( 33.81249999999999289, 5.819803920172571310, 5.819803920172576639 ) ) ;
#18364 = AXIS2_PLACEMENT_3D ( 'NONE', #126971, #115353, #39282 ) ;
#18365 = CARTESIAN_POINT ( 'NONE',  ( 44.91709685856476142, 3.054999999999998828, 5.291415217122922066 ) ) ;
#18366 = ADVANCED_FACE ( 'NONE', ( #110271 ), #33485, .F. ) ;
#18367 = VERTEX_POINT ( 'NONE', #131339 ) ;
#18368 = ADVANCED_FACE ( 'NONE', ( #122585 ), #45089, .F. ) ;
#18369 = CARTESIAN_POINT ( 'NONE',  ( 11.99999999999991651, 4.931123077392129517, 4.000000000000000000 ) ) ;
#18370 = ORIENTED_EDGE ( 'NONE', *, *, #134582, .T. ) ;
#18371 = ORIENTED_EDGE ( 'NONE', *, *, #99965, .T. ) ;
#18372 = DIRECTION ( 'NONE',  ( -0.6830127018922180770, -0.6830127018922204085, -0.2588190451025213501 ) ) ;
#18373 = VECTOR ( 'NONE', #13946, 1000.000000000000000 ) ;
#18374 = VECTOR ( 'NONE', #70506, 1000.000000000000000 ) ;
#18375 = LINE ( 'NONE', #82268, #121760 ) ;
#18376 = LINE ( 'NONE', #19127, #14232 ) ;
#18377 = AXIS2_PLACEMENT_3D ( 'NONE', #139286, #39978, #128390 ) ;
#18378 = FACE_OUTER_BOUND ( 'NONE', #107432, .T. ) ;
#18379 = EDGE_CURVE ( 'NONE', #143241, #36066, #8785, .T. ) ;
#18380 = CARTESIAN_POINT ( 'NONE',  ( -3.758600742197928835, 21.72499999999999432, 5.000000000000000000 ) ) ;
#18382 = ORIENTED_EDGE ( 'NONE', *, *, #19594, .T. ) ;
#18381 = CARTESIAN_POINT ( 'NONE',  ( 100.1208603837962272, -6.884901960086286188, 3.974999999999997424 ) ) ;
#18383 = ADVANCED_FACE ( 'NONE', ( #64657 ), #139873, .T. ) ;
#18384 = DIRECTION ( 'NONE',  ( -0.7071067811865487940, 0.7071067811865463515, 0.000000000000000000 ) ) ;
#18385 = DIRECTION ( 'NONE',  ( 0.7071067811865487940, 0.7071067811865463515, 0.000000000000000000 ) ) ;
#18386 =( LENGTH_UNIT ( ) NAMED_UNIT ( * ) SI_UNIT ( .MILLI., .METRE. ) );
#18387 = AXIS2_PLACEMENT_3D ( 'NONE', #54615, #32131, #98798 ) ;
#18388 = CARTESIAN_POINT ( 'NONE',  ( 6.299744871391586898, -27.71228299555210484, 4.000000000000000000 ) ) ;
#18389 = DIRECTION ( 'NONE',  ( -4.681814790819591790E-17, -0.3543493200069152693, 0.9351131265310292928 ) ) ;
#18390 = VERTEX_POINT ( 'NONE', #66798 ) ;
#18391 = VERTEX_POINT ( 'NONE', #110978 ) ;
#18392 = EDGE_CURVE ( 'NONE', #72085, #14802, #86425, .T. ) ;
#18393 = CARTESIAN_POINT ( 'NONE',  ( 0.000000000000000000, 0.000000000000000000, 5.000000000000000000 ) ) ;
#18394 = CARTESIAN_POINT ( 'NONE',  ( 81.14126352523143737, 4.472830434245836706, 4.472830434245840259 ) ) ;
#18395 = DIRECTION ( 'NONE',  ( 0.7071067811865487940, 0.7071067811865463515, 0.000000000000000000 ) ) ;
#18396 = LINE ( 'NONE', #119163, #1496 ) ;
#18397 = DIRECTION ( 'NONE',  ( 0.7071067811865487940, 0.7071067811865463515, -0.000000000000000000 ) ) ;
#18398 = VERTEX_POINT ( 'NONE', #97241 ) ;
#18399 = VERTEX_POINT ( 'NONE', #130651 ) ;
#18400 = STYLED_ITEM ( 'NONE', ( #98950 ), #21720 ) ;
#18401 = CARTESIAN_POINT ( 'NONE',  ( 29.67183060077626067, -15.74070752338412760, 4.000000000000000000 ) ) ;
#18402 = FILL_AREA_STYLE ('',( #86569 ) ) ;
#18403 = ORIENTED_EDGE ( 'NONE', *, *, #103890, .T. ) ;
#18404 = ADVANCED_FACE ( 'NONE', ( #66101 ), #121160, .T. ) ;
#18405 = VERTEX_POINT ( 'NONE', #75541 ) ;
#18406 = DIRECTION ( 'NONE',  ( -0.7071067811865487940, 0.7071067811865463515, -0.000000000000000000 ) ) ;
#18407 = ORIENTED_EDGE ( 'NONE', *, *, #46115, .T. ) ;
#18408 = CARTESIAN_POINT ( 'NONE',  ( 25.49999999999982236, 19.39370406404969316, 1.459788787078142303 ) ) ;
#18409 = DIRECTION ( 'NONE',  ( 0.7071067811865486830, -0.7071067811865464625, -0.000000000000000000 ) ) ;
#18410 = FACE_BOUND ( 'NONE', #67679, .T. ) ;
#18411 = CARTESIAN_POINT ( 'NONE',  ( 32.99999999999977973, -9.412538124160656494, 4.000000000000000000 ) ) ;
#18412 = DIRECTION ( 'NONE',  ( 1.201410254241279878E-16, -1.000000000000000000, 0.000000000000000000 ) ) ;
#18413 = CARTESIAN_POINT ( 'NONE',  ( 8.510786437626906675, -27.52281430457049183, 5.000000000000000000 ) ) ;
#18415 = VERTEX_POINT ( 'NONE', #55211 ) ;
#18414 = LINE ( 'NONE', #62694, #117586 ) ;
#18416 =( BOUNDED_CURVE ( )  B_SPLINE_CURVE ( 3, ( #99650, #64195, #10497, #53295 ),
 .UNSPECIFIED., .F., .T. ) 
 B_SPLINE_CURVE_WITH_KNOTS ( ( 4, 4 ),
 ( 4.767201131347619025, 4.812229608965456151 ),
 .UNSPECIFIED. ) 
 CURVE ( )  GEOMETRIC_REPRESENTATION_ITEM ( )  RATIONAL_B_SPLINE_CURVE ( ( 1.000000000000000000, 0.9998310434873430852, 0.9998310434873430852, 1.000000000000000000 ) ) 
 REPRESENTATION_ITEM ( '' )  );
#18417 = EDGE_LOOP ( 'NONE', ( #103564, #51985, #42721, #1579 ) ) ;
#18419 = VERTEX_POINT ( 'NONE', #120415 ) ;
#18418 = EDGE_CURVE ( 'NONE', #38637, #70950, #119712, .T. ) ;
#18420 = CARTESIAN_POINT ( 'NONE',  ( 84.49543019189812298, 5.291415217122916737, 3.055000000000001936 ) ) ;
#18421 = ORIENTED_EDGE ( 'NONE', *, *, #120728, .T. ) ;
#18422 = DIRECTION ( 'NONE',  ( -0.000000000000000000, 0.000000000000000000, 1.000000000000000000 ) ) ;
#18423 = PLANE ( 'NONE',  #132254 ) ;
#18424 = EDGE_CURVE ( 'NONE', #46586, #46174, #98001, .T. ) ;
#18425 = CARTESIAN_POINT ( 'NONE',  ( 13.03163515922184423, 2.259292476615701428, 13.77329220150640054 ) ) ;
#18426 = EDGE_CURVE ( 'NONE', #38919, #104775, #65400, .T. ) ;
#18427 = EDGE_CURVE ( 'NONE', #49695, #373, #125466, .T. ) ;
#18428 = DIRECTION ( 'NONE',  ( 1.000000000000000000, 0.000000000000000000, 0.000000000000000000 ) ) ;
#18429 = DIRECTION ( 'NONE',  ( 0.3543493200069162685, -0.000000000000000000, -0.9351131265310288487 ) ) ;
#18430 = CARTESIAN_POINT ( 'NONE',  ( 12.86840764549667604, 9.139736423841732040E-16, 0.000000000000000000 ) ) ;
#18431 = DIRECTION ( 'NONE',  ( -0.000000000000000000, -0.3543493200069152693, 0.9351131265310292928 ) ) ;
#18432 = VECTOR ( 'NONE', #94028, 1000.000000000000000 ) ;
#18433 = VECTOR ( 'NONE', #86273, 1000.000000000000000 ) ;
#18434 = CARTESIAN_POINT ( 'NONE',  ( 24.48921356237309510, -27.52281430457072631, 5.000000000000000000 ) ) ;
#18435 = AXIS2_PLACEMENT_3D ( 'NONE', #40807, #32803, #98730 ) ;
#18436 = EDGE_LOOP ( 'NONE', ( #68390, #99532, #56884, #141834 ) ) ;
#18437 = EDGE_CURVE ( 'NONE', #30706, #36198, #3632, .T. ) ;
#18438 = PLANE ( 'NONE',  #105085 ) ;
#18439 = PLANE ( 'NONE',  #132225 ) ;
#18440 = VECTOR ( 'NONE', #73414, 1000.000000000000000 ) ;
#18441 = ORIENTED_EDGE ( 'NONE', *, *, #8726, .F. ) ;
#18442 = VERTEX_POINT ( 'NONE', #68964 ) ;
#18443 = EDGE_CURVE ( 'NONE', #113567, #942, #134204, .T. ) ;
#18445 = VERTEX_POINT ( 'NONE', #15234 ) ;
#18444 = EDGE_CURVE ( 'NONE', #109300, #99727, #2949, .T. ) ;
#18446 = CARTESIAN_POINT ( 'NONE',  ( 32.66709685856476852, -3.055000000000000160, -5.291415217122921177 ) ) ;
#18447 = ORIENTED_EDGE ( 'NONE', *, *, #97526, .F. ) ;
#18448 = AXIS2_PLACEMENT_3D ( 'NONE', #140344, #64944, #130922 ) ;
#18449 = LINE ( 'NONE', #42414, #115770 ) ;
#18450 = EDGE_CURVE ( 'NONE', #76165, #15535, #58834, .T. ) ;
#18451 = AXIS2_PLACEMENT_3D ( 'NONE', #51706, #60456, #138715 ) ;
#18452 = CARTESIAN_POINT ( 'NONE',  ( 11.12913961620377101, 5.278424836066147208, 3.047499999999990550 ) ) ;
#18453 = CARTESIAN_POINT ( 'NONE',  ( 12.77438429321126812, 9.652835684742514744, -27.12452711299875574 ) ) ;
#18454 = EDGE_CURVE ( 'NONE', #121024, #85852, #38130, .T. ) ;
#18455 = VERTEX_POINT ( 'NONE', #47931 ) ;
#18456 = CARTESIAN_POINT ( 'NONE',  ( -45.18398860626900415, 28.73617430169818832, 5.000000000000000000 ) ) ;
#18457 = VERTEX_POINT ( 'NONE', #92095 ) ;
#18458 = LINE ( 'NONE', #138144, #7045 ) ;
#18459 = VECTOR ( 'NONE', #93637, 1000.000000000000000 ) ;
#18460 = DIRECTION ( 'NONE',  ( -0.000000000000000000, 0.000000000000000000, -1.000000000000000000 ) ) ;
#18461 = ADVANCED_FACE ( 'NONE', ( #12398 ), #2204, .F. ) ;
#18463 = ORIENTED_EDGE ( 'NONE', *, *, #126914, .T. ) ;
#18462 = CARTESIAN_POINT ( 'NONE',  ( -5.510786437626906675, -27.52281430457051314, 5.000000000000000000 ) ) ;
#18464 = ORIENTED_EDGE ( 'NONE', *, *, #78698, .F. ) ;
#18465 = LINE ( 'NONE', #86639, #9866 ) ;
#18466 = EDGE_LOOP ( 'NONE', ( #63622, #45031, #122439, #117856 ) ) ;
#18467 = VECTOR ( 'NONE', #64972, 999.9999999999998863 ) ;
#18468 = CARTESIAN_POINT ( 'NONE',  ( -0.1839886062690032631, 28.73617430169787568, 5.000000000000000000 ) ) ;
#18469 = ORIENTED_EDGE ( 'NONE', *, *, #76575, .F. ) ;
#18470 = EDGE_LOOP ( 'NONE', ( #57873, #76751, #93519 ) ) ;
#18471 = ORIENTED_EDGE ( 'NONE', *, *, #47808, .F. ) ;
#18472 = ORIENTED_EDGE ( 'NONE', *, *, #119317, .T. ) ;
#18473 = DIRECTION ( 'NONE',  ( 0.7071067811865486830, -0.7071067811865464625, -0.000000000000000000 ) ) ;
#18474 = EDGE_CURVE ( 'NONE', #140592, #80880, #69682, .T. ) ;
#18475 = CIRCLE ( 'NONE', #87951, 2.500000000000000444 ) ;
#18476 = VECTOR ( 'NONE', #19634, 1000.000000000000000 ) ;
#18477 = CARTESIAN_POINT ( 'NONE',  ( -12.18398860626900060, 28.73617430169795739, 5.000000000000000000 ) ) ;
#18478 = DIRECTION ( 'NONE',  ( 0.7071067811865487940, 0.7071067811865463515, 0.000000000000000000 ) ) ;
#18479 = DIRECTION ( 'NONE',  ( -1.000000000000000000, 2.496005001405478586E-15, -6.809571051365719919E-16 ) ) ;
#18480 = CARTESIAN_POINT ( 'NONE',  ( -7.122370700763609008, -39.92999999999999261, 19.06900128115122328 ) ) ;
#18481 = ORIENTED_EDGE ( 'NONE', *, *, #9387, .T. ) ;
#18482 = LINE ( 'NONE', #106947, #48982 ) ;
#18483 = ORIENTED_EDGE ( 'NONE', *, *, #77848, .F. ) ;
#18484 = AXIS2_PLACEMENT_3D ( 'NONE', #125940, #132006, #32700 ) ;
#18485 = EDGE_CURVE ( 'NONE', #59881, #61485, #91415, .T. ) ;
#18486 = DIRECTION ( 'NONE',  ( -0.3543493200069162685, -0.000000000000000000, -0.9351131265310288487 ) ) ;
#18487 = EDGE_CURVE ( 'NONE', #11133, #77537, #135629, .T. ) ;
#18488 = CARTESIAN_POINT ( 'NONE',  ( 29.43706980810189222, 2.126176841940952134, -7.934999999999993392 ) ) ;
#18489 = CARTESIAN_POINT ( 'NONE',  ( -41.99451991528749062, 28.92564299267967343, 4.000000000000000000 ) ) ;
#18490 = ORIENTED_EDGE ( 'NONE', *, *, #42802, .F. ) ;
#18491 = VECTOR ( 'NONE', #130083, 1000.000000000000000 ) ;
#18492 = CARTESIAN_POINT ( 'NONE',  ( 0.000000000000000000, 0.000000000000000000, 5.000000000000000000 ) ) ;
#18493 = CARTESIAN_POINT ( 'NONE',  ( 3.299744871391591339, -27.71228299555208352, 4.000000000000000000 ) ) ;
#18494 = VERTEX_POINT ( 'NONE', #123342 ) ;
#18495 = ORIENTED_EDGE ( 'NONE', *, *, #110960, .F. ) ;
#18496 = EDGE_LOOP ( 'NONE', ( #21483, #82731, #107887, #88474 ) ) ;
#18497 = DIRECTION ( 'NONE',  ( 0.7071067811865487940, 0.7071067811865463515, -0.000000000000000000 ) ) ;
#18498 = CARTESIAN_POINT ( 'NONE',  ( -50.99451991528749062, 28.92564299267973738, 4.000000000000000000 ) ) ;
#18499 = VECTOR ( 'NONE', #103237, 1000.000000000000000 ) ;
#18500 = LINE ( 'NONE', #106959, #97857 ) ;
#18501 = FACE_OUTER_BOUND ( 'NONE', #121149, .T. ) ;
#18502 = EDGE_CURVE ( 'NONE', #28383, #59940, #59512, .T. ) ;
#18503 = CARTESIAN_POINT ( 'NONE',  ( 21.98911971346036154, -22.02621442084248216, 4.990779571109222879 ) ) ;
#18504 = CARTESIAN_POINT ( 'NONE',  ( 76.62043019189812298, 3.055000000000002380, -5.291415217122917625 ) ) ;
#18505 = LINE ( 'NONE', #85934, #88060 ) ;
#18506 = DIRECTION ( 'NONE',  ( 1.000000000000000000, 0.000000000000000000, 0.000000000000000000 ) ) ;
#18507 = CARTESIAN_POINT ( 'NONE',  ( 12.32816939922345334, 14.25929247661557753, 4.000000000000000000 ) ) ;
#18508 = LINE ( 'NONE', #138188, #86047 ) ;
#18509 = ORIENTED_EDGE ( 'NONE', *, *, #139934, .T. ) ;
#18510 = CARTESIAN_POINT ( 'NONE',  ( 19.25000000000000355, -7.464222240803106570E-16, -6.094999999999989981 ) ) ;
#18511 = EDGE_LOOP ( 'NONE', ( #136556, #58545, #66967, #141346 ) ) ;
#18512 = VECTOR ( 'NONE', #115445, 1000.000000000000000 ) ;
#18513 = LINE ( 'NONE', #51910, #50135 ) ;
#18514 = CARTESIAN_POINT ( 'NONE',  ( -24.48921356237309510, -27.52281430457072631, 5.000000000000000000 ) ) ;
#18515 = ORIENTED_EDGE ( 'NONE', *, *, #122013, .T. ) ;
#18516 = FACE_OUTER_BOUND ( 'NONE', #54593, .T. ) ;
#18518 = ORIENTED_EDGE ( 'NONE', *, *, #42064, .F. ) ;
#18517 = LINE ( 'NONE', #114962, #106609 ) ;
#18519 = CARTESIAN_POINT ( 'NONE',  ( -1.499999999999989120, -13.53360074219760278, 5.000000000000000000 ) ) ;
#18520 = FACE_OUTER_BOUND ( 'NONE', #113894, .T. ) ;
#18521 = VERTEX_POINT ( 'NONE', #68267 ) ;
#18522 = ORIENTED_EDGE ( 'NONE', *, *, #97338, .T. ) ;
#18523 = DIRECTION ( 'NONE',  ( -0.6830127018922180770, -0.6830127018922204085, -0.2588190451025213501 ) ) ;
#18524 = DIRECTION ( 'NONE',  ( 0.000000000000000000, 1.000000000000000000, -0.000000000000000000 ) ) ;
#18525 = VECTOR ( 'NONE', #108373, 1000.000000000000000 ) ;
#18526 = CARTESIAN_POINT ( 'NONE',  ( 9.707106781186473299, -15.74070752338412049, 5.000000000000000000 ) ) ;
#18527 = CARTESIAN_POINT ( 'NONE',  ( 94.43336038379622721, 2.130196079827431532, -7.949999999999997513 ) ) ;
#18528 = DIRECTION ( 'NONE',  ( -1.000000000000000000, -1.224606353822377258E-16, -0.000000000000000000 ) ) ;
#18529 = DIRECTION ( 'NONE',  ( -0.6830127018922180770, -0.6830127018922204085, -0.2588190451025213501 ) ) ;
#18530 = VERTEX_POINT ( 'NONE', #81263 ) ;
#18531 = DIRECTION ( 'NONE',  ( 0.6830127018922181881, 0.6830127018922202975, -0.2588190451025214056 ) ) ;
#18532 = ADVANCED_FACE ( 'NONE', ( #103669 ), #36315, .F. ) ;
#18533 = CARTESIAN_POINT ( 'NONE',  ( 26.99999999999982592, -16.44781430457065952, 5.000000000000000000 ) ) ;
#18534 = CARTESIAN_POINT ( 'NONE',  ( 31.93750000000000355, -4.461849672132299105, 4.461849672132299993 ) ) ;
#18535 = DIRECTION ( 'NONE',  ( 0.7071067811865486830, -0.7071067811865464625, -0.000000000000000000 ) ) ;
#18536 = ORIENTED_EDGE ( 'NONE', *, *, #35952, .F. ) ;
#18537 = CARTESIAN_POINT ( 'NONE',  ( 46.74586038379622011, 3.974999999999996980, 6.884901960086287964 ) ) ;
#18538 = ORIENTED_EDGE ( 'NONE', *, *, #95965, .T. ) ;
#18539 = VECTOR ( 'NONE', #53456, 999.9999999999998863 ) ;
#18540 = CARTESIAN_POINT ( 'NONE',  ( 84.29209685856477563, -5.291415217122921177, 3.054999999999999272 ) ) ;
#18541 = LINE ( 'NONE', #9080, #63985 ) ;
#18542 = DIRECTION ( 'NONE',  ( 0.7071067811865486830, -0.7071067811865464625, -0.000000000000000000 ) ) ;
#18543 = ORIENTED_EDGE ( 'NONE', *, *, #131093, .F. ) ;
#18544 = AXIS2_PLACEMENT_3D ( 'NONE', #14038, #24232, #135160 ) ;
#18545 = AXIS2_PLACEMENT_3D ( 'NONE', #49417, #91469, #47982 ) ;
#18546 = AXIS2_PLACEMENT_3D ( 'NONE', #34214, #112482, #79179 ) ;
#18547 = FACE_OUTER_BOUND ( 'NONE', #112725, .T. ) ;
#18548 = VECTOR ( 'NONE', #50586, 1000.000000000000000 ) ;
#18549 = DIRECTION ( 'NONE',  ( -0.6830127018922181881, 0.6830127018922202975, -0.2588190451025214056 ) ) ;
#18550 = DIRECTION ( 'NONE',  ( 0.000000000000000000, -1.000000000000000000, 0.000000000000000000 ) ) ;
#18551 = EDGE_CURVE ( 'NONE', #132258, #63562, #137047, .T. ) ;
#18553 = ORIENTED_EDGE ( 'NONE', *, *, #26211, .T. ) ;
#18552 = DIRECTION ( 'NONE',  ( 0.6830127018922181881, 0.6830127018922202975, -0.2588190451025214056 ) ) ;
#18554 = ADVANCED_FACE ( 'NONE', ( #124740 ), #46524, .T. ) ;
#18555 = FACE_OUTER_BOUND ( 'NONE', #135254, .T. ) ;
#18556 = DIRECTION ( 'NONE',  ( -0.7071067811865487940, 0.7071067811865463515, -0.000000000000000000 ) ) ;
#18557 = CARTESIAN_POINT ( 'NONE',  ( -27.87485380690749182, -14.24070752338412937, 9.401115078912724243 ) ) ;
#18558 = AXIS2_PLACEMENT_3D ( 'NONE', #89193, #92026, #24631 ) ;
#18559 = DIRECTION ( 'NONE',  ( -0.7071067811865487940, 0.7071067811865463515, -0.000000000000000000 ) ) ;
#18560 = EDGE_CURVE ( 'NONE', #20671, #47204, #126177, .T. ) ;
#18561 = ORIENTED_EDGE ( 'NONE', *, *, #6803, .F. ) ;
#18562 = ORIENTED_EDGE ( 'NONE', *, *, #124531, .F. ) ;
#18563 = CARTESIAN_POINT ( 'NONE',  ( 69.41709685856477563, 3.054999999999998828, 5.291415217122922066 ) ) ;
#18564 = ORIENTED_EDGE ( 'NONE', *, *, #128832, .F. ) ;
#18565 = EDGE_CURVE ( 'NONE', #57582, #95196, #124036, .T. ) ;
#18566 = CARTESIAN_POINT ( 'NONE',  ( 21.79289321881331176, -8.240707523384200428, 5.000000000000000000 ) ) ;
#18567 = FACE_OUTER_BOUND ( 'NONE', #141903, .T. ) ;
#18568 = VECTOR ( 'NONE', #58015, 1000.000000000000000 ) ;
#18569 = CARTESIAN_POINT ( 'NONE',  ( -75.29974487139158157, -27.71228299555258445, 4.000000000000000000 ) ) ;
#18570 = DIRECTION ( 'NONE',  ( -0.7071067811865487940, 0.7071067811865463515, -0.000000000000000000 ) ) ;
#18571 = ORIENTED_EDGE ( 'NONE', *, *, #18800, .T. ) ;
#18572 = DIRECTION ( 'NONE',  ( -0.000000000000000000, 0.3543493200069153248, 0.9351131265310292928 ) ) ;
#18573 = FACE_OUTER_BOUND ( 'NONE', #91036, .T. ) ;
#18574 = EDGE_CURVE ( 'NONE', #79366, #21205, #13805, .T. ) ;
#18575 = AXIS2_PLACEMENT_3D ( 'NONE', #1620, #135072, #11796 ) ;
#18576 = VERTEX_POINT ( 'NONE', #94945 ) ;
#18577 = AXIS2_PLACEMENT_3D ( 'NONE', #83574, #94414, #138662 ) ;
#18578 = LINE ( 'NONE', #61451, #14251 ) ;
#18579 = AXIS2_PLACEMENT_3D ( 'NONE', #116272, #129271, #16963 ) ;
#18580 = CARTESIAN_POINT ( 'NONE',  ( 34.92499999999998295, 19.70193056682078137, 4.500000000000000888 ) ) ;
#18581 = LINE ( 'NONE', #62860, #132614 ) ;
#18582 = ADVANCED_FACE ( 'NONE', ( #15929 ), #3426, .T. ) ;
#18583 = VECTOR ( 'NONE', #22774, 1000.000000000000000 ) ;
#18584 = VERTEX_POINT ( 'NONE', #71814 ) ;
#18585 = ORIENTED_EDGE ( 'NONE', *, *, #55046, .T. ) ;
#18586 = AXIS2_PLACEMENT_3D ( 'NONE', #123019, #4022, #49038 ) ;
#18587 = DIRECTION ( 'NONE',  ( -2.781805975412905890E-17, 0.3543493200069152693, 0.9351131265310292928 ) ) ;
#18588 = CARTESIAN_POINT ( 'NONE',  ( 6.299744871391586898, -27.71228299555210484, 4.000000000000000000 ) ) ;
#18589 = CARTESIAN_POINT ( 'NONE',  ( 25.40000000000000568, -6.374262171851336589, -2.013297974899656229 ) ) ;
#18590 = DIRECTION ( 'NONE',  ( -0.000000000000000000, 1.000000000000000000, -0.000000000000000000 ) ) ;
#18591 = EDGE_CURVE ( 'NONE', #29382, #87099, #40604, .T. ) ;
#18592 = EDGE_CURVE ( 'NONE', #129881, #124632, #28294, .T. ) ;
#18593 = DIRECTION ( 'NONE',  ( -0.000000000000000000, -0.000000000000000000, 1.000000000000000000 ) ) ;
#18594 = CARTESIAN_POINT ( 'NONE',  ( 0.8678420939694353464, -0.6000000000000000888, 4.443813723662917603 ) ) ;
#18595 = FILL_AREA_STYLE ('',( #129511 ) ) ;
#18596 = ORIENTED_EDGE ( 'NONE', *, *, #78062, .T. ) ;
#18597 = VECTOR ( 'NONE', #75618, 1000.000000000000000 ) ;
#18598 = ORIENTED_EDGE ( 'NONE', *, *, #87740, .F. ) ;
#18599 = ORIENTED_EDGE ( 'NONE', *, *, #15752, .F. ) ;
#18600 = ORIENTED_EDGE ( 'NONE', *, *, #97500, .F. ) ;
#18601 = EDGE_CURVE ( 'NONE', #28286, #12547, #98351, .T. ) ;
#18602 = MECHANICAL_DESIGN_GEOMETRIC_PRESENTATION_REPRESENTATION (  '', ( #14065 ), #113624 ) ;
#18603 = CARTESIAN_POINT ( 'NONE',  ( -16.11017322888198677, -22.22500000000000142, 4.785647885939350310 ) ) ;
#18604 = LINE ( 'NONE', #60017, #135840 ) ;
#18605 = EDGE_CURVE ( 'NONE', #9454, #69693, #127606, .T. ) ;
#18606 = EDGE_CURVE ( 'NONE', #35602, #123337, #137778, .T. ) ;
#18607 = FILL_AREA_STYLE ('',( #105616 ) ) ;
#18608 = ORIENTED_EDGE ( 'NONE', *, *, #17002, .T. ) ;
#18609 = DIRECTION ( 'NONE',  ( -0.000000000000000000, 0.000000000000000000, 1.000000000000000000 ) ) ;
#18610 = DIRECTION ( 'NONE',  ( -0.7071067811865486830, 0.7071067811865464625, -0.000000000000000000 ) ) ;
#18611 = CARTESIAN_POINT ( 'NONE',  ( 3.707013264293012256, -21.74070752338405654, 4.999753212805217117 ) ) ;
#18612 = FACE_OUTER_BOUND ( 'NONE', #108687, .T. ) ;
#18613 = VECTOR ( 'NONE', #136348, 1000.000000000000000 ) ;
#18614 = DIRECTION ( 'NONE',  ( 1.000000000000000000, 0.000000000000000000, 0.000000000000000000 ) ) ;
#18615 = VERTEX_POINT ( 'NONE', #138483 ) ;
#18616 = EDGE_CURVE ( 'NONE', #81350, #110059, #137689, .T. ) ;
#18617 = LINE ( 'NONE', #10603, #54215 ) ;
#18618 = CARTESIAN_POINT ( 'NONE',  ( 50.58333333333332860, 6.884901960086290629, -3.974999999999994316 ) ) ;
#18619 = ORIENTED_EDGE ( 'NONE', *, *, #70626, .F. ) ;
#18620 = DIRECTION ( 'NONE',  ( 0.3543493200069162685, -0.000000000000000000, -0.9351131265310288487 ) ) ;
#18621 = ORIENTED_EDGE ( 'NONE', *, *, #117888, .T. ) ;
#18622 = EDGE_CURVE ( 'NONE', #126064, #92829, #50755, .T. ) ;
#18623 = CARTESIAN_POINT ( 'NONE',  ( 12.58747294953710671, -6.094999999999989981, 3.732111120401553285E-16 ) ) ;
#18624 = ORIENTED_EDGE ( 'NONE', *, *, #126008, .T. ) ;
#18625 = CARTESIAN_POINT ( 'NONE',  ( 67.37543019189810423, -5.291415217122920289, -3.055000000000001492 ) ) ;
#18627 = EDGE_LOOP ( 'NONE', ( #94387, #125540, #27209, #47913, #24086 ) ) ;
#18626 = CONICAL_SURFACE ( 'NONE', #9402, 2.500000000000000444, 0.9599310885968830309 ) ;
#18628 = ORIENTED_EDGE ( 'NONE', *, *, #83180, .T. ) ;
#18629 = CARTESIAN_POINT ( 'NONE',  ( 5.443598275411213550, 3.821174125832445049E-16, 0.000000000000000000 ) ) ;
#18630 = DIRECTION ( 'NONE',  ( 0.6830127018922181881, 0.6830127018922202975, -0.2588190451025214056 ) ) ;
#18631 = CARTESIAN_POINT ( 'NONE',  ( 112.4379301918981184, -6.110000000000001208, 1.637169565754158951 ) ) ;
#18632 = CARTESIAN_POINT ( 'NONE',  ( 12.35051985313232237, 4.584330080086930965E-16, 0.000000000000000000 ) ) ;
#18633 = EDGE_CURVE ( 'NONE', #80457, #140709, #102911, .T. ) ;
#18634 = CARTESIAN_POINT ( 'NONE',  ( 5.999999999999960032, -8.731860332648835765, -2.120594902707523932 ) ) ;
#18636 = ADVANCED_FACE ( 'NONE', ( #7206 ), #139214, .T. ) ;
#18635 = VECTOR ( 'NONE', #71890, 999.9999999999998863 ) ;
#18637 = DIRECTION ( 'NONE',  ( -1.000000000000000000, -1.224606353822377258E-16, -0.000000000000000000 ) ) ;
#18638 =( BOUNDED_CURVE ( )  B_SPLINE_CURVE ( 2, ( #73739, #63616, #42578, #95483, #30233, #74485, #130999, #20780, #18618, #65033, #139746, #40424, #86056 ),
 .UNSPECIFIED., .F., .F. ) 
 B_SPLINE_CURVE_WITH_KNOTS ( ( 3, 2, 2, 2, 2, 2, 3 ),
 ( 0.7166666666666667851, 0.7194444444444445530, 0.7222222222222223209, 0.7250000000000000888, 0.7277777777777778567, 0.7305555555555556246, 0.7333333333333333925 ),
 .UNSPECIFIED. ) 
 CURVE ( )  GEOMETRIC_REPRESENTATION_ITEM ( )  RATIONAL_B_SPLINE_CURVE ( ( 0.9999999999999986677, 0.9659258262890696445, 1.000000000000000000, 0.9659258262890683122, 1.000000000000000000, 0.9659258262890683122, 1.000000000000000000, 0.9659258262890683122, 1.000000000000000000, 0.9659258262890683122, 1.000000000000000000, 0.9659258262890669799, 1.000000000000001332 ) ) 
 REPRESENTATION_ITEM ( '' )  );
#18639 = CARTESIAN_POINT ( 'NONE',  ( 28.82816939922332367, -11.24070752338416490, 4.000000000000000000 ) ) ;
#18641 = CARTESIAN_POINT ( 'NONE',  ( 77.95419371712955581, 6.884901960086283523, 3.975000000000002753 ) ) ;
#18640 = AXIS2_PLACEMENT_3D ( 'NONE', #88379, #79681, #13628 ) ;
#18643 = ORIENTED_EDGE ( 'NONE', *, *, #102150, .F. ) ;
#18642 = CIRCLE ( 'NONE', #16256, 2.552699999999997971 ) ;
#18644 = LINE ( 'NONE', #51318, #127032 ) ;
#18645 = CARTESIAN_POINT ( 'NONE',  ( 0.9387689034200082938, 0.4000000000000001332, -2.166563668000045517 ) ) ;
#18646 = EDGE_LOOP ( 'NONE', ( #72572, #2021, #8299, #142152 ) ) ;
#18647 = ORIENTED_EDGE ( 'NONE', *, *, #111149, .F. ) ;
#18648 = ORIENTED_EDGE ( 'NONE', *, *, #28436, .F. ) ;
#18649 = VECTOR ( 'NONE', #49410, 999.9999999999998863 ) ;
#18650 = VECTOR ( 'NONE', #93254, 1000.000000000000227 ) ;
#18651 = ORIENTED_EDGE ( 'NONE', *, *, #3909, .T. ) ;
#18652 = VECTOR ( 'NONE', #5488, 999.9999999999998863 ) ;
#18653 = VECTOR ( 'NONE', #14324, 1000.000000000000000 ) ;
#18654 =( BOUNDED_CURVE ( )  B_SPLINE_CURVE ( 3, ( #134662, #125918, #2672, #114982 ),
 .UNSPECIFIED., .F., .T. ) 
 B_SPLINE_CURVE_WITH_KNOTS ( ( 4, 4 ),
 ( 1.864375635226932282, 1.933014472006533868 ),
 .UNSPECIFIED. ) 
 CURVE ( )  GEOMETRIC_REPRESENTATION_ITEM ( )  RATIONAL_B_SPLINE_CURVE ( ( 1.000000000000000000, 0.9996074310407765395, 0.9996074310407765395, 1.000000000000000000 ) ) 
 REPRESENTATION_ITEM ( '' )  );
#18655 = AXIS2_PLACEMENT_3D ( 'NONE', #65793, #122982, #44757 ) ;
#18656 = LINE ( 'NONE', #83976, #30734 ) ;
#18657 = FACE_OUTER_BOUND ( 'NONE', #70088, .T. ) ;
#18658 = CARTESIAN_POINT ( 'NONE',  ( -2.999999999999975131, -16.06887692260765377, 4.000000000000000000 ) ) ;
#18659 = ORIENTED_EDGE ( 'NONE', *, *, #91601, .T. ) ;
#18661 = VERTEX_POINT ( 'NONE', #51478 ) ;
#18660 = CIRCLE ( 'NONE', #25725, 5.968999999999998529 ) ;
#18662 = ADVANCED_FACE ( 'NONE', ( #39906 ), #38455, .T. ) ;
#18663 = CARTESIAN_POINT ( 'NONE',  ( 5.957903141435219929, 6.871911579029515771, 3.967499999999989146 ) ) ;
#18664 = CARTESIAN_POINT ( 'NONE',  ( 90.49586038379622721, -3.974999999999998312, -6.884901960086286188 ) ) ;
#18665 = DIRECTION ( 'NONE',  ( -0.6830127018922181881, 0.6830127018922202975, -0.2588190451025214056 ) ) ;
#18666 = VECTOR ( 'NONE', #100120, 999.9999999999998863 ) ;
#18667 = CARTESIAN_POINT ( 'NONE',  ( 38.18749999999999289, -5.819803920172573974, 5.819803920172573086 ) ) ;
#18668 = ORIENTED_EDGE ( 'NONE', *, *, #117666, .T. ) ;
#18669 = VERTEX_POINT ( 'NONE', #96357 ) ;
#18670 = ORIENTED_EDGE ( 'NONE', *, *, #19483, .F. ) ;
#18672 = VECTOR ( 'NONE', #6905, 1000.000000000000227 ) ;
#18671 = LINE ( 'NONE', #107122, #28795 ) ;
#18673 = CARTESIAN_POINT ( 'NONE',  ( 33.18398860626899705, 28.73617430169810305, 5.000000000000000000 ) ) ;
#18674 = CARTESIAN_POINT ( 'NONE',  ( 16.17183060077635659, 12.75929247661558641, 4.000000000000000000 ) ) ;
#18675 = DIRECTION ( 'NONE',  ( 0.6830127018922180770, 0.6830127018922202975, -0.2588190451025213501 ) ) ;
#18676 = DIRECTION ( 'NONE',  ( 0.000000000000000000, 0.000000000000000000, 1.000000000000000000 ) ) ;
#18677 = LINE ( 'NONE', #29564, #17878 ) ;
#18678 = FACE_OUTER_BOUND ( 'NONE', #8464, .T. ) ;
#18679 = AXIS2_PLACEMENT_3D ( 'NONE', #25211, #123845, #90486 ) ;
#18680 = VECTOR ( 'NONE', #94530, 1000.000000000000000 ) ;
#18681 = PLANE ( 'NONE',  #6671 ) ;
#18682 = CARTESIAN_POINT ( 'NONE',  ( 28.14626352523143638, -4.472830434245840259, 4.472830434245839371 ) ) ;
#18683 = DIRECTION ( 'NONE',  ( -0.7071067811865486830, -0.7071067811865464625, 0.000000000000000000 ) ) ;
#18684 = VECTOR ( 'NONE', #31952, 1000.000000000000227 ) ;
#18685 = VERTEX_POINT ( 'NONE', #29004 ) ;
#18686 = DIRECTION ( 'NONE',  ( -0.6830127018922180770, -0.6830127018922204085, -0.2588190451025213501 ) ) ;
#18688 = AXIS2_PLACEMENT_3D ( 'NONE', #25484, #69762, #14628 ) ;
#18687 = LINE ( 'NONE', #105691, #77168 ) ;
#18689 = ORIENTED_EDGE ( 'NONE', *, *, #29371, .F. ) ;
#18690 = CARTESIAN_POINT ( 'NONE',  ( 32.99999999999976552, -5.527737879153157508, -7.983877177622447974 ) ) ;
#18692 = VERTEX_POINT ( 'NONE', #18076 ) ;
#18691 = CARTESIAN_POINT ( 'NONE',  ( 52.83697049268915436, -48.90295371244931033, -39.18578444878554734 ) ) ;
#18693 = VECTOR ( 'NONE', #104649, 1000.000000000000227 ) ;
#18694 = FACE_OUTER_BOUND ( 'NONE', #113829, .T. ) ;
#18695 = DIRECTION ( 'NONE',  ( 3.115803279706882722E-16, -1.000000000000000000, 0.000000000000000000 ) ) ;
#18696 = VERTEX_POINT ( 'NONE', #93546 ) ;
#18697 = FACE_OUTER_BOUND ( 'NONE', #7817, .T. ) ;
#18698 = ORIENTED_EDGE ( 'NONE', *, *, #80182, .F. ) ;
#18699 = CARTESIAN_POINT ( 'NONE',  ( 94.14169371712955581, -2.130196079827424871, -7.949999999999998401 ) ) ;
#18700 = CARTESIAN_POINT ( 'NONE',  ( 124.3291937171295700, -3.975000000000001865, 6.884901960086284411 ) ) ;
#18701 = DIRECTION ( 'NONE',  ( -0.6830127018922180770, -0.6830127018922204085, -0.2588190451025213501 ) ) ;
#18702 = VECTOR ( 'NONE', #73481, 1000.000000000000000 ) ;
#18703 = DIRECTION ( 'NONE',  ( -0.7071067811865487940, 0.7071067811865463515, -0.000000000000000000 ) ) ;
#18704 = FACE_OUTER_BOUND ( 'NONE', #10307, .T. ) ;
#18705 = LINE ( 'NONE', #39061, #135141 ) ;
#18706 = DIRECTION ( 'NONE',  ( -0.7071067811865487940, 0.7071067811865463515, -0.000000000000000000 ) ) ;
#18708 = AXIS2_PLACEMENT_3D ( 'NONE', #59274, #68024, #2693 ) ;
#18707 = CARTESIAN_POINT ( 'NONE',  ( 2.333333333333333481, 5.278424836066143655, -3.047499999999997655 ) ) ;
#18709 = CARTESIAN_POINT ( 'NONE',  ( 4.207903141435219929, -6.871911579029513106, -3.967499999999993587 ) ) ;
#18711 = VECTOR ( 'NONE', #104264, 999.9999999999998863 ) ;
#18710 = CARTESIAN_POINT ( 'NONE',  ( 0.000000000000000000, 2.375000000000000000, 4.319999999999998508 ) ) ;
#18712 = CARTESIAN_POINT ( 'NONE',  ( -26.99999999999981526, -16.60178936734450872, 0.8616154019346856652 ) ) ;
#18713 = VERTEX_POINT ( 'NONE', #140599 ) ;
#18714 = ORIENTED_EDGE ( 'NONE', *, *, #90844, .T. ) ;
#18715 = CARTESIAN_POINT ( 'NONE',  ( 85.29166666666667140, 3.975000000000003642, -6.884901960086285300 ) ) ;
#18717 = EDGE_CURVE ( 'NONE', #122313, #61905, #62362, .T. ) ;
#18716 = DIRECTION ( 'NONE',  ( -0.000000000000000000, 0.000000000000000000, 1.000000000000000000 ) ) ;
#18718 = ORIENTED_EDGE ( 'NONE', *, *, #103953, .T. ) ;
#18719 = EDGE_CURVE ( 'NONE', #111562, #119104, #26849, .T. ) ;
#18720 = EDGE_CURVE ( 'NONE', #86478, #6439, #130764, .T. ) ;
#18721 = LINE ( 'NONE', #42671, #10959 ) ;
#18722 = EDGE_CURVE ( 'NONE', #116519, #20421, #63086, .T. ) ;
#18723 = PLANE ( 'NONE',  #129730 ) ;
#18724 = AXIS2_PLACEMENT_3D ( 'NONE', #104067, #1873, #112827 ) ;
#18725 = CARTESIAN_POINT ( 'NONE',  ( 29.97502705046288440, -5.819803920172573086, 5.819803920172573086 ) ) ;
#18726 = ORIENTED_EDGE ( 'NONE', *, *, #129035, .T. ) ;
#18727 = CARTESIAN_POINT ( 'NONE',  ( -14.99999999999989342, -18.03360074219755660, 5.000000000000000000 ) ) ;
#18728 = EDGE_CURVE ( 'NONE', #57216, #15048, #71100, .T. ) ;
#18729 = CARTESIAN_POINT ( 'NONE',  ( 29.48334561358934991, 22.22500000000000142, 4.500000000000000888 ) ) ;
#18730 = LINE ( 'NONE', #63712, #18737 ) ;
#18731 = ADVANCED_FACE ( 'NONE', ( #126859 ), #32583, .F. ) ;
#18732 = ADVANCED_FACE ( 'NONE', ( #64482 ), #76819, .F. ) ;
#18734 = VERTEX_POINT ( 'NONE', #31161 ) ;
#18733 = CARTESIAN_POINT ( 'NONE',  ( 0.2569208697893813342, -0.4000000000000003553, 2.015694669338588429 ) ) ;
#18735 = CARTESIAN_POINT ( 'NONE',  ( 40.66666666666665719, 6.884901960086285300, 3.975000000000003642 ) ) ;
#18736 = DIRECTION ( 'NONE',  ( 1.000000000000000000, 0.000000000000000000, 0.000000000000000000 ) ) ;
#18737 = VECTOR ( 'NONE', #33072, 1000.000000000000000 ) ;
#18738 = DIRECTION ( 'NONE',  ( 0.7071067811865487940, 0.7071067811865463515, 0.000000000000000000 ) ) ;
#18739 = CARTESIAN_POINT ( 'NONE',  ( 8.510786437626906675, -27.52281430457049183, 5.000000000000000000 ) ) ;
#18740 = DIRECTION ( 'NONE',  ( 0.6830127018922181881, 0.6830127018922202975, -0.2588190451025214056 ) ) ;
#18741 = CARTESIAN_POINT ( 'NONE',  ( 55.29044309249616163, -47.26730531257655343, 36.54674188582600181 ) ) ;
#18742 = EDGE_CURVE ( 'NONE', #40894, #69819, #112230, .T. ) ;
#18743 = ADVANCED_FACE ( 'NONE', ( #31857 ), #86248, .F. ) ;
#18744 = ORIENTED_EDGE ( 'NONE', *, *, #86824, .F. ) ;
#18745 = ORIENTED_EDGE ( 'NONE', *, *, #118465, .T. ) ;
#18746 = CARTESIAN_POINT ( 'NONE',  ( 97.70876352523144703, -7.482591942790329030E-16, 6.110000000000001208 ) ) ;
#18747 = ORIENTED_EDGE ( 'NONE', *, *, #82507, .F. ) ;
#18748 = EDGE_CURVE ( 'NONE', #6450, #80414, #120243, .T. ) ;
#18749 = CARTESIAN_POINT ( 'NONE',  ( 125.3761450143286993, -47.18881911353552994, 35.55177538329112963 ) ) ;
#18750 = LINE ( 'NONE', #62297, #138026 ) ;
#18751 = EDGE_LOOP ( 'NONE', ( #117571, #73751, #79502, #10268 ) ) ;
#18752 = AXIS2_PLACEMENT_3D ( 'NONE', #57961, #34048, #124603 ) ;
#18753 = DIRECTION ( 'NONE',  ( -0.7071067811865486830, -0.7071067811865464625, -0.000000000000000000 ) ) ;
#18754 = LINE ( 'NONE', #95618, #2619 ) ;
#18755 = VECTOR ( 'NONE', #43277, 1000.000000000000000 ) ;
#18756 = ADVANCED_FACE ( 'NONE', ( #119541 ), #143457, .F. ) ;
#18757 = VECTOR ( 'NONE', #78915, 999.9999999999998863 ) ;
#18758 = CARTESIAN_POINT ( 'NONE',  ( 97.91209685856478018, 5.291415217122921177, -3.054999999999994831 ) ) ;
#18759 = ORIENTED_EDGE ( 'NONE', *, *, #141272, .T. ) ;
#18760 = CYLINDRICAL_SURFACE ( 'NONE', #35085, 0.5000000000000004441 ) ;
#18761 = VERTEX_POINT ( 'NONE', #129726 ) ;
#18762 = CARTESIAN_POINT ( 'NONE',  ( -27.48921356237309155, -27.52281430457074762, 5.000000000000000000 ) ) ;
#18763 = VECTOR ( 'NONE', #60091, 1000.000000000000000 ) ;
#18764 = VECTOR ( 'NONE', #23545, 1000.000000000000227 ) ;
#18765 = DIRECTION ( 'NONE',  ( 0.3543493200069162685, -0.000000000000000000, -0.9351131265310288487 ) ) ;
#18766 = VECTOR ( 'NONE', #63849, 1000.000000000000000 ) ;
#18767 = AXIS2_PLACEMENT_3D ( 'NONE', #28947, #60165, #73876 ) ;
#18768 = PLANE ( 'NONE',  #67023 ) ;
#18769 = VECTOR ( 'NONE', #23294, 1000.000000000000000 ) ;
#18770 = ORIENTED_EDGE ( 'NONE', *, *, #17301, .T. ) ;
#18771 = EDGE_LOOP ( 'NONE', ( #74023, #38665, #1816, #108309 ) ) ;
#18772 = ORIENTED_EDGE ( 'NONE', *, *, #26796, .F. ) ;
#18773 = DIRECTION ( 'NONE',  ( 0.7071067811865486830, -0.7071067811865464625, -0.000000000000000000 ) ) ;
#18774 = DIRECTION ( 'NONE',  ( 0.7071067811865487940, 0.7071067811865463515, 0.000000000000000000 ) ) ;
#18775 = CARTESIAN_POINT ( 'NONE',  ( 12.46290314143521982, -3.967499999999994476, 6.871911579029513106 ) ) ;
#18776 = VECTOR ( 'NONE', #104879, 1000.000000000000000 ) ;
#18777 = ADVANCED_FACE ( 'NONE', ( #44174 ), #8618, .F. ) ;
#18778 = CARTESIAN_POINT ( 'NONE',  ( 21.72916666666666785, -6.094999999999989093, 1.633150327867691542 ) ) ;
#18779 = ORIENTED_EDGE ( 'NONE', *, *, #107356, .T. ) ;
#18780 = ORIENTED_EDGE ( 'NONE', *, *, #129605, .T. ) ;
#18781 = AXIS2_PLACEMENT_3D ( 'NONE', #105449, #8264, #82311 ) ;
#18782 = CARTESIAN_POINT ( 'NONE',  ( 27.99999999999999645, 9.521314400968980422E-16, 0.000000000000000000 ) ) ;
#18783 = VERTEX_POINT ( 'NONE', #20238 ) ;
#18784 = VERTEX_POINT ( 'NONE', #110806 ) ;
#18785 = EDGE_CURVE ( 'NONE', #95585, #101043, #97821, .T. ) ;
#18786 = AXIS2_PLACEMENT_3D ( 'NONE', #127768, #111712, #88551 ) ;
#18787 = EDGE_CURVE ( 'NONE', #2746, #100224, #109409, .T. ) ;
#18788 = VECTOR ( 'NONE', #105073, 1000.000000000000000 ) ;
#18789 = CARTESIAN_POINT ( 'NONE',  ( -8.773457579940252170E-14, -35.14999999999997726, -40.00000000000000000 ) ) ;
#18790 = CARTESIAN_POINT ( 'NONE',  ( 12.69999999999999574, -40.43000000000000682, -40.00000000000000000 ) ) ;
#18791 = ORIENTED_EDGE ( 'NONE', *, *, #129229, .T. ) ;
#18792 = CARTESIAN_POINT ( 'NONE',  ( -14.09068777029287567, 6.496774105546209377, 4.000000000000000000 ) ) ;
#18793 = EDGE_CURVE ( 'NONE', #62749, #109346, #131165, .T. ) ;
#18794 = VECTOR ( 'NONE', #115786, 1000.000000000000000 ) ;
#18795 = CARTESIAN_POINT ( 'NONE',  ( -32.20666063542130075, 21.75929247661549226, 4.998822639870715179 ) ) ;
#18796 = FACE_OUTER_BOUND ( 'NONE', #96396, .T. ) ;
#18797 = VECTOR ( 'NONE', #55668, 1000.000000000000227 ) ;
#18798 = DIRECTION ( 'NONE',  ( -0.7071067811865486830, 0.7071067811865464625, 0.000000000000000000 ) ) ;
#18799 = ORIENTED_EDGE ( 'NONE', *, *, #29230, .F. ) ;
#18800 = EDGE_CURVE ( 'NONE', #50175, #100764, #121409, .T. ) ;
#18801 = LINE ( 'NONE', #63070, #139033 ) ;
#18802 = CARTESIAN_POINT ( 'NONE',  ( -8.241399257801971245, 21.72500000000000142, 5.000000000000000000 ) ) ;
#18803 = EDGE_LOOP ( 'NONE', ( #72570, #98156, #96062, #7959 ) ) ;
#18804 = DIRECTION ( 'NONE',  ( -0.7071067811865487940, 0.7071067811865463515, -0.000000000000000000 ) ) ;
#18805 = CARTESIAN_POINT ( 'NONE',  ( 19.83042955554208220, -2.395858916147067585, -33.25513085038058136 ) ) ;
#18806 = VECTOR ( 'NONE', #126245, 1000.000000000000000 ) ;
#18807 = LINE ( 'NONE', #94934, #26026 ) ;
#18808 = ORIENTED_EDGE ( 'NONE', *, *, #48578, .T. ) ;
#18809 = CARTESIAN_POINT ( 'NONE',  ( 22.49999999999985434, 19.46639925780206326, 5.000000000000000000 ) ) ;
#18810 = ORIENTED_EDGE ( 'NONE', *, *, #92308, .T. ) ;
#18811 = VERTEX_POINT ( 'NONE', #87662 ) ;
#18812 = EDGE_CURVE ( 'NONE', #129071, #83273, #44926, .T. ) ;
#18813 = EDGE_LOOP ( 'NONE', ( #139549, #62137, #113217, #15765 ) ) ;
#18814 = DIRECTION ( 'NONE',  ( 0.7071067811865487940, 0.7071067811865463515, 0.000000000000000000 ) ) ;
#18815 = MECHANICAL_DESIGN_GEOMETRIC_PRESENTATION_REPRESENTATION (  '', ( #134551 ), #2558 ) ;
#18816 = CARTESIAN_POINT ( 'NONE',  ( -31.92499999999997584, -21.76999999999999247, -40.00000000000000000 ) ) ;
#18817 = DIRECTION ( 'NONE',  ( 0.7071067811865486830, -0.7071067811865464625, -0.000000000000000000 ) ) ;
#18818 = CARTESIAN_POINT ( 'NONE',  ( 5.068407645496677105, -2.499999999999998224, 0.000000000000000000 ) ) ;
#18819 = DIRECTION ( 'NONE',  ( 0.000000000000000000, -1.000000000000000000, 0.000000000000000000 ) ) ;
#18820 = ADVANCED_FACE ( 'NONE', ( #10091 ), #20961, .F. ) ;
#18821 = CARTESIAN_POINT ( 'NONE',  ( -17.67183060077634593, -6.740707523384212863, 4.000000000000000000 ) ) ;
#18823 = DIRECTION ( 'NONE',  ( -0.000000000000000000, -0.3543493200069152693, 0.9351131265310292928 ) ) ;
#18822 = CIRCLE ( 'NONE', #35112, 2.500000000000000444 ) ;
#18824 = VECTOR ( 'NONE', #134636, 1000.000000000000000 ) ;
#18825 = DIRECTION ( 'NONE',  ( -0.6830127018922181881, 0.6830127018922202975, -0.2588190451025214056 ) ) ;
#18826 = CARTESIAN_POINT ( 'NONE',  ( -17.51078643762690845, -27.52281430457043143, 5.000000000000000000 ) ) ;
#18827 = CARTESIAN_POINT ( 'NONE',  ( -25.17183060077629619, -5.240707523384230626, 4.000000000000000000 ) ) ;
#18828 = CARTESIAN_POINT ( 'NONE',  ( 15.18398860626900237, 28.73617430169797871, 5.000000000000000000 ) ) ;
#18829 = ORIENTED_EDGE ( 'NONE', *, *, #15465, .F. ) ;
#18830 = VERTEX_POINT ( 'NONE', #43448 ) ;
#18831 = ORIENTED_EDGE ( 'NONE', *, *, #109264, .T. ) ;
#18832 = AXIS2_PLACEMENT_3D ( 'NONE', #29051, #141375, #50808 ) ;
#18833 = VERTEX_POINT ( 'NONE', #33329 ) ;
#18834 = DIRECTION ( 'NONE',  ( -1.000000000000000000, 0.000000000000000000, 0.000000000000000000 ) ) ;
#18835 = VERTEX_POINT ( 'NONE', #141320 ) ;
#18836 = VERTEX_POINT ( 'NONE', #77531 ) ;
#18837 = CARTESIAN_POINT ( 'NONE',  ( -29.99999999999978328, -1.447814304570818500, 5.000000000000000000 ) ) ;
#18838 = CARTESIAN_POINT ( 'NONE',  ( -12.69999999999998153, -0.4000000000000004108, 2.467792535850613866 ) ) ;
#18839 = EDGE_CURVE ( 'NONE', #117948, #143110, #95954, .T. ) ;
#18840 = LINE ( 'NONE', #129753, #9210 ) ;
#18841 = EDGE_CURVE ( 'NONE', #75908, #106956, #118856, .T. ) ;
#18842 = ORIENTED_EDGE ( 'NONE', *, *, #112077, .T. ) ;
#18843 = LINE ( 'NONE', #63112, #2365 ) ;
#18844 = VECTOR ( 'NONE', #71173, 1000.000000000000227 ) ;
#18845 = ORIENTED_EDGE ( 'NONE', *, *, #26958, .T. ) ;
#18846 =( BOUNDED_CURVE ( )  B_SPLINE_CURVE ( 2, ( #136212, #28177, #36208, #94122, #36896, #72439, #81145, #116607, #17287, #3526, #2840, #92700, #47135 ),
 .UNSPECIFIED., .F., .T. ) 
 B_SPLINE_CURVE_WITH_KNOTS ( ( 3, 2, 2, 2, 2, 2, 3 ),
 ( 0.2000000000000000389, 0.2027777777777778068, 0.2055555555555555747, 0.2083333333333333703, 0.2111111111111111660, 0.2138888888888889339, 0.2166666666666667296 ),
 .UNSPECIFIED. ) 
 CURVE ( )  GEOMETRIC_REPRESENTATION_ITEM ( )  RATIONAL_B_SPLINE_CURVE ( ( 0.9999999999999996669, 0.9659258262890686453, 1.000000000000000000, 0.9659258262890683122, 1.000000000000000000, 0.9659258262890683122, 1.000000000000000000, 0.9659258262890683122, 1.000000000000000000, 0.9659258262890683122, 1.000000000000000000, 0.9659258262890676461, 1.000000000000000666 ) ) 
 REPRESENTATION_ITEM ( '' )  );
#18847 = CARTESIAN_POINT ( 'NONE',  ( 28.93003974513574050, -0.7407075233842770334, 13.87443053587604069 ) ) ;
#18848 = DIRECTION ( 'NONE',  ( -0.000000000000000000, -0.3543493200069152693, 0.9351131265310292928 ) ) ;
#18849 = CARTESIAN_POINT ( 'NONE',  ( 9.837903141435219823, -6.871911579029513106, -3.967499999999993587 ) ) ;
#18850 = ORIENTED_EDGE ( 'NONE', *, *, #94042, .F. ) ;
#18851 = CARTESIAN_POINT ( 'NONE',  ( 87.99543019189812298, 5.291415217122917625, 3.055000000000002380 ) ) ;
#18852 = CARTESIAN_POINT ( 'NONE',  ( -13.49999999999989697, 0.05218569542916363935, 5.000000000000000000 ) ) ;
#18853 = DIRECTION ( 'NONE',  ( -1.000000000000000000, -0.000000000000000000, -0.000000000000000000 ) ) ;
#18854 = CARTESIAN_POINT ( 'NONE',  ( 27.99999999999996803, -49.14999999999999147, 49.92499999999997584 ) ) ;
#18855 = ORIENTED_EDGE ( 'NONE', *, *, #57855, .T. ) ;
#18856 = ORIENTED_EDGE ( 'NONE', *, *, #109458, .F. ) ;
#18857 = FACE_OUTER_BOUND ( 'NONE', #45005, .T. ) ;
#18858 = VERTEX_POINT ( 'NONE', #56516 ) ;
#18859 = DIRECTION ( 'NONE',  ( 0.7071067811865487940, -0.7071067811865463515, 0.000000000000000000 ) ) ;
#18860 = DIRECTION ( 'NONE',  ( -0.7071067811865486830, 0.7071067811865464625, 0.000000000000000000 ) ) ;
#18861 = VECTOR ( 'NONE', #89657, 1000.000000000000000 ) ;
#18862 = DIRECTION ( 'NONE',  ( 0.7071067811865487940, 0.7071067811865463515, 0.000000000000000000 ) ) ;
#18863 = CARTESIAN_POINT ( 'NONE',  ( 0.000000000000000000, 0.000000000000000000, 5.000000000000000000 ) ) ;
#18865 = ADVANCED_FACE ( 'NONE', ( #134034 ), #34011, .F. ) ;
#18864 = ORIENTED_EDGE ( 'NONE', *, *, #108336, .T. ) ;
#18866 = AXIS2_PLACEMENT_3D ( 'NONE', #88025, #11862, #55408 ) ;
#18867 = CARTESIAN_POINT ( 'NONE',  ( 27.18398860626900060, 28.73617430169806042, 5.000000000000000000 ) ) ;
#18868 = VECTOR ( 'NONE', #93158, 999.9999999999998863 ) ;
#18869 = EDGE_CURVE ( 'NONE', #16019, #10551, #82139, .T. ) ;
#18870 = CARTESIAN_POINT ( 'NONE',  ( 0.000000000000000000, 0.000000000000000000, 0.000000000000000000 ) ) ;
#18871 = DIRECTION ( 'NONE',  ( -0.000000000000000000, 0.3543493200069153248, 0.9351131265310292928 ) ) ;
#18872 = ORIENTED_EDGE ( 'NONE', *, *, #100107, .F. ) ;
#18873 = CARTESIAN_POINT ( 'NONE',  ( 8.700255128608413102, -27.71228299555199825, 4.000000000000000000 ) ) ;
#18874 = VECTOR ( 'NONE', #140325, 999.9999999999998863 ) ;
#18875 = AXIS2_PLACEMENT_3D ( 'NONE', #57118, #14288, #4064 ) ;
#18876 = AXIS2_PLACEMENT_3D ( 'NONE', #43506, #76885, #121054 ) ;
#18877 = VECTOR ( 'NONE', #51256, 1000.000000000000000 ) ;
#18878 = DIRECTION ( 'NONE',  ( 0.000000000000000000, -1.000000000000000000, 0.000000000000000000 ) ) ;
#18880 = VERTEX_POINT ( 'NONE', #78959 ) ;
#18879 = VECTOR ( 'NONE', #73271, 1000.000000000000000 ) ;
#18882 = ORIENTED_EDGE ( 'NONE', *, *, #78011, .F. ) ;
#18881 = DIRECTION ( 'NONE',  ( -1.000000000000000000, -0.000000000000000000, -0.000000000000000000 ) ) ;
#18883 = ORIENTED_EDGE ( 'NONE', *, *, #17903, .T. ) ;
#18884 = EDGE_CURVE ( 'NONE', #27936, #115169, #14383, .T. ) ;
#18885 = DIRECTION ( 'NONE',  ( -0.7071067811865487940, 0.7071067811865463515, 0.000000000000000000 ) ) ;
#18886 = VECTOR ( 'NONE', #56803, 1000.000000000000000 ) ;
#18887 = CARTESIAN_POINT ( 'NONE',  ( -30.29974487139158867, -27.71228299555227537, 4.000000000000000000 ) ) ;
#18888 = ORIENTED_EDGE ( 'NONE', *, *, #29080, .F. ) ;
#18889 = CARTESIAN_POINT ( 'NONE',  ( -34.92500000000001137, 22.22500000000000142, 4.000000000000000000 ) ) ;
#18890 = LINE ( 'NONE', #10154, #12776 ) ;
#18891 =( NAMED_UNIT ( * ) PLANE_ANGLE_UNIT ( ) SI_UNIT ( $, .RADIAN. ) );
#18892 = VECTOR ( 'NONE', #88742, 999.9999999999998863 ) ;
#18893 = DIRECTION ( 'NONE',  ( -0.3543493200069162685, -0.000000000000000000, -0.9351131265310288487 ) ) ;
#18894 = CARTESIAN_POINT ( 'NONE',  ( 31.77083333333333215, -7.949999999999998401, -2.130196079827426203 ) ) ;
#18895 = FACE_OUTER_BOUND ( 'NONE', #108155, .T. ) ;
#18896 = CARTESIAN_POINT ( 'NONE',  ( 9.299744871391588674, -27.71228299555212971, 4.000000000000000000 ) ) ;
#18897 = PLANE ( 'NONE',  #76680 ) ;
#18898 = CARTESIAN_POINT ( 'NONE',  ( 19.49999999999986855, 12.05218569542904206, 5.000000000000000000 ) ) ;
#18899 = LINE ( 'NONE', #52248, #72206 ) ;
#18900 = LINE ( 'NONE', #92894, #48318 ) ;
#18901 = CARTESIAN_POINT ( 'NONE',  ( 36.18398860626899705, 28.73617430169812437, 5.000000000000000000 ) ) ;
#18902 = PLANE ( 'NONE',  #107890 ) ;
#18903 = EDGE_LOOP ( 'NONE', ( #75529, #101583, #32914 ) ) ;
#18904 = VECTOR ( 'NONE', #110249, 999.9999999999998863 ) ;
#18905 = ORIENTED_EDGE ( 'NONE', *, *, #115834, .F. ) ;
#18906 = ORIENTED_EDGE ( 'NONE', *, *, #19200, .T. ) ;
#18907 = CARTESIAN_POINT ( 'NONE',  ( 106.4374999999999858, 5.819803920172573974, -5.819803920172572198 ) ) ;
#18908 = VECTOR ( 'NONE', #83738, 1000.000000000000227 ) ;
#18909 = ORIENTED_EDGE ( 'NONE', *, *, #48732, .T. ) ;
#18910 = ORIENTED_EDGE ( 'NONE', *, *, #64111, .F. ) ;
#18911 = ADVANCED_BREP_SHAPE_REPRESENTATION ( '', ( #90242, #127880 ), #141741 ) ;
#18912 = AXIS2_PLACEMENT_3D ( 'NONE', #15417, #127811, #116202 ) ;
#18913 = ORIENTED_EDGE ( 'NONE', *, *, #12121, .T. ) ;
#18914 = DIRECTION ( 'NONE',  ( 0.7071067811865486830, -0.7071067811865464625, -0.000000000000000000 ) ) ;
#18915 = CARTESIAN_POINT ( 'NONE',  ( 15.05159235450332034, 2.500000000000001776, 0.000000000000000000 ) ) ;
#18916 = AXIS2_PLACEMENT_3D ( 'NONE', #81373, #59620, #103776 ) ;
#18917 = ORIENTED_EDGE ( 'NONE', *, *, #82014, .F. ) ;
#18918 = FACE_OUTER_BOUND ( 'NONE', #21196, .T. ) ;
#18919 = FACE_OUTER_BOUND ( 'NONE', #82715, .T. ) ;
#18920 = PLANE ( 'NONE',  #50995 ) ;
#18921 = FACE_OUTER_BOUND ( 'NONE', #30314, .T. ) ;
#18922 = CARTESIAN_POINT ( 'NONE',  ( 107.9170968585647756, 3.054999999999998828, 5.291415217122922066 ) ) ;
#18923 = ORIENTED_EDGE ( 'NONE', *, *, #97764, .T. ) ;
#18924 = ADVANCED_FACE ( 'NONE', ( #2781 ), #79699, .F. ) ;
#18925 = CARTESIAN_POINT ( 'NONE',  ( -9.535978227293808729, 9.762579867702294578, -29.04603976045208569 ) ) ;
#18926 = SURFACE_SIDE_STYLE ('',( #94345 ) ) ;
#18927 = CARTESIAN_POINT ( 'NONE',  ( -24.71230993966011269, -21.73547319004781286, 4.999917730833664642 ) ) ;
#18929 = VECTOR ( 'NONE', #31492, 1000.000000000000000 ) ;
#18928 = DIRECTION ( 'NONE',  ( -0.7071067811865486830, -0.7071067811865464625, 0.000000000000000000 ) ) ;
#18930 = FACE_OUTER_BOUND ( 'NONE', #143370, .T. ) ;
#18931 = CARTESIAN_POINT ( 'NONE',  ( 152.4000000000000057, -18.48000000000005372, -33.92499999999998295 ) ) ;
#18932 = CARTESIAN_POINT ( 'NONE',  ( 30.12086038379621655, -6.884901960086286188, 3.974999999999997424 ) ) ;
#18933 = LINE ( 'NONE', #6584, #67706 ) ;
#18934 = ADVANCED_FACE ( 'NONE', ( #122413 ), #90527, .F. ) ;
#18935 = ADVANCED_FACE ( 'NONE', ( #25980 ), #2034, .F. ) ;
#18936 = ORIENTED_EDGE ( 'NONE', *, *, #42361, .F. ) ;
#18937 = ORIENTED_EDGE ( 'NONE', *, *, #18841, .F. ) ;
#18938 = CARTESIAN_POINT ( 'NONE',  ( 29.87500000000000000, 7.950000000000000178, 1.460391307983218535E-15 ) ) ;
#18939 = ADVANCED_FACE ( 'NONE', ( #3477 ), #123882, .T. ) ;
#18940 = ORIENTED_EDGE ( 'NONE', *, *, #20016, .T. ) ;
#18941 = CARTESIAN_POINT ( 'NONE',  ( 2.000000000000008882, 7.464222240803104598E-16, -6.094999999999989093 ) ) ;
#18942 = EDGE_CURVE ( 'NONE', #82308, #70075, #112285, .T. ) ;
#18943 = VECTOR ( 'NONE', #113082, 1000.000000000000000 ) ;
#18944 = DIRECTION ( 'NONE',  ( 0.7071067811865486830, -0.7071067811865464625, -0.000000000000000000 ) ) ;
#18945 = VECTOR ( 'NONE', #66873, 1000.000000000000000 ) ;
#18946 = ADVANCED_FACE ( 'NONE', ( #23079 ), #24540, .F. ) ;
#18947 = DIRECTION ( 'NONE',  ( -1.000000000000000000, -0.000000000000000000, -0.000000000000000000 ) ) ;
#18948 = DIRECTION ( 'NONE',  ( 0.7071067811865487940, 0.7071067811865463515, 0.000000000000000000 ) ) ;
#18949 = CARTESIAN_POINT ( 'NONE',  ( -29.99999999999978328, -0.4125381241607550820, 4.000000000000000000 ) ) ;
#18950 = CARTESIAN_POINT ( 'NONE',  ( 50.99451991528749062, 28.92564299267973738, 4.000000000000000000 ) ) ;
#18951 = EDGE_CURVE ( 'NONE', #5194, #141895, #63402, .T. ) ;
#18952 = CARTESIAN_POINT ( 'NONE',  ( 124.7454301918981230, -5.291415217122918513, -3.055000000000000160 ) ) ;
#18953 = VERTEX_POINT ( 'NONE', #67357 ) ;
#18954 = DIRECTION ( 'NONE',  ( 0.7071067811865487940, 0.7071067811865463515, 0.000000000000000000 ) ) ;
#18955 = ORIENTED_EDGE ( 'NONE', *, *, #47925, .T. ) ;
#18956 = STYLED_ITEM ( 'NONE', ( #130273 ), #28818 ) ;
#18957 = CARTESIAN_POINT ( 'NONE',  ( 11.81601139373100651, 28.73617430169779041, 5.000000000000000000 ) ) ;
#18958 = CARTESIAN_POINT ( 'NONE',  ( 1.827855086967997922, -2.055000000000000160, 0.000000000000000000 ) ) ;
#18959 = DIRECTION ( 'NONE',  ( -1.000000000000000000, -1.224606353822377258E-16, -0.000000000000000000 ) ) ;
#18960 = ADVANCED_FACE ( 'NONE', ( #101388 ), #57928, .F. ) ;
#18961 = LINE ( 'NONE', #131292, #67256 ) ;
#18962 = ORIENTED_EDGE ( 'NONE', *, *, #42342, .T. ) ;
#18963 = CARTESIAN_POINT ( 'NONE',  ( 50.02126352523143282, -4.472830434245839371, -4.472830434245840259 ) ) ;
#18964 = ORIENTED_EDGE ( 'NONE', *, *, #69220, .T. ) ;
#18965 = DIRECTION ( 'NONE',  ( 0.6830127018922181881, 0.6830127018922202975, -0.2588190451025214056 ) ) ;
#18966 = CARTESIAN_POINT ( 'NONE',  ( -5.485869665262789852, 22.22500000000000142, -6.155586976313258241 ) ) ;
#18967 = CARTESIAN_POINT ( 'NONE',  ( 51.29974487139158867, -27.71228299555242103, 4.000000000000000000 ) ) ;
#18968 = DIRECTION ( 'NONE',  ( -0.6830127018922181881, 0.6830127018922202975, -0.2588190451025214056 ) ) ;
#18969 = AXIS2_PLACEMENT_3D ( 'NONE', #56591, #100756, #46420 ) ;
#18970 = EDGE_CURVE ( 'NONE', #33459, #124649, #102121, .T. ) ;
#18971 = CARTESIAN_POINT ( 'NONE',  ( 43.22459685856478728, -1.637169565754160949, 6.109999999999997655 ) ) ;
#18972 = ORIENTED_EDGE ( 'NONE', *, *, #6168, .T. ) ;
#18973 = DIRECTION ( 'NONE',  ( 1.000000000000000000, 0.000000000000000000, 0.000000000000000000 ) ) ;
#18974 = ORIENTED_EDGE ( 'NONE', *, *, #140869, .F. ) ;
#18975 = ORIENTED_EDGE ( 'NONE', *, *, #27618, .T. ) ;
#18976 = AXIS2_PLACEMENT_3D ( 'NONE', #16181, #14062, #127106 ) ;
#18977 = AXIS2_PLACEMENT_3D ( 'NONE', #69707, #113891, #3657 ) ;
#18978 = ORIENTED_EDGE ( 'NONE', *, *, #65496, .F. ) ;
#18979 = VECTOR ( 'NONE', #130640, 1000.000000000000227 ) ;
#18980 = CARTESIAN_POINT ( 'NONE',  ( -34.47516574401892342, 1.490517612115595636, 4.998110765256835286 ) ) ;
#18981 = CARTESIAN_POINT ( 'NONE',  ( 80.14169371712957002, -2.130196079827424871, -7.949999999999998401 ) ) ;
#18982 = ORIENTED_EDGE ( 'NONE', *, *, #84272, .F. ) ;
#18983 = CARTESIAN_POINT ( 'NONE',  ( 17.61782366839360847, 8.969638207445433054, 4.000000000000000000 ) ) ;
#18984 = ADVANCED_FACE ( 'NONE', ( #114404 ), #136158, .F. ) ;
#18985 = VECTOR ( 'NONE', #12678, 1000.000000000000000 ) ;
#18986 = AXIS2_PLACEMENT_3D ( 'NONE', #112702, #99672, #111256 ) ;
#18987 =( GEOMETRIC_REPRESENTATION_CONTEXT ( 3 ) GLOBAL_UNCERTAINTY_ASSIGNED_CONTEXT ( ( #56376 ) ) GLOBAL_UNIT_ASSIGNED_CONTEXT ( ( #37717, #132948, #81957 ) ) REPRESENTATION_CONTEXT ( 'NONE', 'WORKASPACE' ) );
#18988 = CARTESIAN_POINT ( 'NONE',  ( -34.92500000000001137, -22.22500000000000142, 4.000000000000000000 ) ) ;
#18989 = LINE ( 'NONE', #140078, #58186 ) ;
#18990 = FACE_BOUND ( 'NONE', #137366, .T. ) ;
#18991 = ORIENTED_EDGE ( 'NONE', *, *, #43045, .T. ) ;
#18992 = CARTESIAN_POINT ( 'NONE',  ( -57.18398860626899705, 28.73617430169827358, 5.000000000000000000 ) ) ;
#18993 = LINE ( 'NONE', #131325, #100023 ) ;
#18994 = LINE ( 'NONE', #54503, #122701 ) ;
#18995 = ORIENTED_EDGE ( 'NONE', *, *, #74960, .T. ) ;
#18996 = LINE ( 'NONE', #141496, #140701 ) ;
#18997 = ORIENTED_EDGE ( 'NONE', *, *, #55818, .F. ) ;
#18998 = ORIENTED_EDGE ( 'NONE', *, *, #34836, .T. ) ;
#18999 = DIRECTION ( 'NONE',  ( -0.7071067811865487940, 0.7071067811865463515, 0.000000000000000000 ) ) ;
#19000 = ADVANCED_FACE ( 'NONE', ( #70245 ), #15077, .T. ) ;
#19001 = EDGE_LOOP ( 'NONE', ( #98953, #142794, #14574, #41431 ) ) ;
#19002 = CARTESIAN_POINT ( 'NONE',  ( 58.82876352523144448, 0.000000000000000000, -6.109999999999998543 ) ) ;
#19003 = ORIENTED_EDGE ( 'NONE', *, *, #82912, .T. ) ;
#19004 = CARTESIAN_POINT ( 'NONE',  ( 23.67183060077630685, -0.7407075233842701500, 4.000000000000000000 ) ) ;
#19005 = CARTESIAN_POINT ( 'NONE',  ( -6.932893218813454439, -34.94289321881344534, -40.00000000000000000 ) ) ;
#19006 = ADVANCED_FACE ( 'NONE', ( #28837 ), #126692, .T. ) ;
#19007 = ORIENTED_EDGE ( 'NONE', *, *, #122434, .F. ) ;
#19008 = CARTESIAN_POINT ( 'NONE',  ( -17.51078643762690845, -27.52281430457043143, 5.000000000000000000 ) ) ;
#19009 = AXIS2_PLACEMENT_3D ( 'NONE', #89771, #123863, #112955 ) ;
#19010 = VECTOR ( 'NONE', #99362, 1000.000000000000000 ) ;
#19011 = CARTESIAN_POINT ( 'NONE',  ( -21.48921356237309155, -27.52281430457070499, 5.000000000000000000 ) ) ;
#19012 = ADVANCED_FACE ( 'NONE', ( #105645 ), #114265, .T. ) ;
#19013 = DIRECTION ( 'NONE',  ( -0.7071067811865487940, 0.7071067811865463515, 0.000000000000000000 ) ) ;
#19014 = DIRECTION ( 'NONE',  ( 0.7071067811865486830, -0.7071067811865464625, -0.000000000000000000 ) ) ;
#19015 = VECTOR ( 'NONE', #68121, 999.9999999999998863 ) ;
#19016 = FACE_OUTER_BOUND ( 'NONE', #103556, .T. ) ;
#19017 = CARTESIAN_POINT ( 'NONE',  ( -15.29974487139158867, -27.71228299555216879, 4.000000000000000000 ) ) ;
#19018 = EDGE_LOOP ( 'NONE', ( #89313, #117492, #113179, #28628 ) ) ;
#19019 = ORIENTED_EDGE ( 'NONE', *, *, #120542, .F. ) ;
#19020 = AXIS2_PLACEMENT_3D ( 'NONE', #108762, #41398, #119645 ) ;
#19021 = LINE ( 'NONE', #112460, #75116 ) ;
#19022 = CARTESIAN_POINT ( 'NONE',  ( -3.183988606268992161, 28.73617430169789699, 5.000000000000000000 ) ) ;
#19023 = ORIENTED_EDGE ( 'NONE', *, *, #26465, .T. ) ;
#19024 = ORIENTED_EDGE ( 'NONE', *, *, #121757, .T. ) ;
#19025 = VERTEX_POINT ( 'NONE', #27373 ) ;
#19026 = CARTESIAN_POINT ( 'NONE',  ( 4.889826771117856019, -22.22500000000000142, 4.785647885939352086 ) ) ;
#19027 = EDGE_CURVE ( 'NONE', #39158, #99753, #827, .T. ) ;
#19028 = CARTESIAN_POINT ( 'NONE',  ( -30.48921356237309510, -27.52281430457076894, 5.000000000000000000 ) ) ;
#19029 = VERTEX_POINT ( 'NONE', #48439 ) ;
#19030 = DIRECTION ( 'NONE',  ( 0.7071067811865487940, 0.7071067811865463515, 0.000000000000000000 ) ) ;
#19031 = FACE_OUTER_BOUND ( 'NONE', #29277, .T. ) ;
#19032 = ADVANCED_FACE ( 'NONE', ( #95496 ), #6301, .F. ) ;
#19033 = CARTESIAN_POINT ( 'NONE',  ( 22.08790314143522338, 6.871911579029515771, 3.967499999999989146 ) ) ;
#19034 = CARTESIAN_POINT ( 'NONE',  ( -15.18398860626900237, 28.73617430169797871, 5.000000000000000000 ) ) ;
#19035 = ORIENTED_EDGE ( 'NONE', *, *, #70877, .T. ) ;
#19036 = CARTESIAN_POINT ( 'NONE',  ( 117.5995968585647944, -6.109999999999998543, -1.637169565754160727 ) ) ;
#19037 = DIRECTION ( 'NONE',  ( -1.000000000000000000, -0.000000000000000000, -0.000000000000000000 ) ) ;
#19038 = VECTOR ( 'NONE', #106124, 1000.000000000000000 ) ;
#19039 = DIRECTION ( 'NONE',  ( -0.6830127018922180770, -0.6830127018922204085, -0.2588190451025213501 ) ) ;
#19041 = ORIENTED_EDGE ( 'NONE', *, *, #76749, .T. ) ;
#19040 = CARTESIAN_POINT ( 'NONE',  ( -25.49999999999982592, 14.14708470758588987, -0.5283514160165968532 ) ) ;
#19043 = AXIS2_PLACEMENT_3D ( 'NONE', #115150, #137680, #14455 ) ;
#19042 = CARTESIAN_POINT ( 'NONE',  ( -13.49999999999990230, 21.05218569542895679, 5.000000000000000000 ) ) ;
#19044 = ORIENTED_EDGE ( 'NONE', *, *, #97157, .T. ) ;
#19045 = DIRECTION ( 'NONE',  ( -0.000000000000000000, 0.3543493200069153248, 0.9351131265310292928 ) ) ;
#19046 = DIRECTION ( 'NONE',  ( -0.5735764363510499342, -0.8191520442889891340, 0.000000000000000000 ) ) ;
#19047 = CARTESIAN_POINT ( 'NONE',  ( 35.35681257248241138, -20.24070752338406720, 21.22881796311220981 ) ) ;
#19049 = EDGE_CURVE ( 'NONE', #16920, #17718, #71632, .T. ) ;
#19048 = ORIENTED_EDGE ( 'NONE', *, *, #118170, .F. ) ;
#19050 = ADVANCED_FACE ( 'NONE', ( #50583 ), #92634, .F. ) ;
#19051 = CARTESIAN_POINT ( 'NONE',  ( 24.48921356237309510, -27.52281430457072631, 5.000000000000000000 ) ) ;
#19052 = DIRECTION ( 'NONE',  ( -1.000000000000000000, -1.224606353822377258E-16, -0.000000000000000000 ) ) ;
#19053 = CARTESIAN_POINT ( 'NONE',  ( -23.20666063542136470, 21.75929247661548516, 4.998822639870711626 ) ) ;
#19054 = VECTOR ( 'NONE', #14603, 1000.000000000000000 ) ;
#19055 = ORIENTED_EDGE ( 'NONE', *, *, #48422, .F. ) ;
#19056 = CARTESIAN_POINT ( 'NONE',  ( -14.99999999999989164, -11.35517001088073208, -1.126524801160144529 ) ) ;
#19057 = CARTESIAN_POINT ( 'NONE',  ( -19.49999999999985079, -20.94781430457061333, 5.000000000000000000 ) ) ;
#19058 = DIRECTION ( 'NONE',  ( 0.000000000000000000, -1.000000000000000000, 0.000000000000000000 ) ) ;
#19059 = ORIENTED_EDGE ( 'NONE', *, *, #736, .T. ) ;
#19060 = ADVANCED_FACE ( 'NONE', ( #138309 ), #115790, .F. ) ;
#19061 = ORIENTED_EDGE ( 'NONE', *, *, #104505, .F. ) ;
#19062 = VECTOR ( 'NONE', #31257, 1000.000000000000000 ) ;
#19063 = CARTESIAN_POINT ( 'NONE',  ( -24.48921356237309510, -27.52281430457072631, 5.000000000000000000 ) ) ;
#19064 = LINE ( 'NONE', #63326, #20449 ) ;
#19065 = CARTESIAN_POINT ( 'NONE',  ( 12.81206980810188512, 7.934999999999993392, 2.126176841940951689 ) ) ;
#19066 = PLANE ( 'NONE',  #78345 ) ;
#19067 = CARTESIAN_POINT ( 'NONE',  ( 35.99451991528749772, 28.92564299267963079, 4.000000000000000000 ) ) ;
#19068 = CARTESIAN_POINT ( 'NONE',  ( 2.671830600776451181, -0.7407075233842770334, 4.000000000000000000 ) ) ;
#19069 = VERTEX_POINT ( 'NONE', #137603 ) ;
#19070 = CARTESIAN_POINT ( 'NONE',  ( 57.18398860626899705, 28.73617430169827358, 5.000000000000000000 ) ) ;
#19071 = CARTESIAN_POINT ( 'NONE',  ( 1.040834085586084257E-14, 14.58746187583908771, 4.000000000000000000 ) ) ;
#19072 = CARTESIAN_POINT ( 'NONE',  ( 31.49999999999978684, 7.466399257802189382, 5.000000000000000000 ) ) ;
#19073 = VECTOR ( 'NONE', #52069, 1000.000000000000000 ) ;
#19074 = VECTOR ( 'NONE', #18478, 999.9999999999998863 ) ;
#19075 = VECTOR ( 'NONE', #30381, 999.9999999999998863 ) ;
#19076 = PLANE ( 'NONE',  #64487 ) ;
#19077 = CARTESIAN_POINT ( 'NONE',  ( 35.20376352523143737, 6.109999999999999432, 1.122388791418549108E-15 ) ) ;
#19078 = CARTESIAN_POINT ( 'NONE',  ( -26.99451991528749417, 28.92564299267956685, 4.000000000000000000 ) ) ;
#19079 = VECTOR ( 'NONE', #16911, 999.9999999999998863 ) ;
#19080 = VERTEX_POINT ( 'NONE', #126016 ) ;
#19081 = DIRECTION ( 'NONE',  ( -0.000000000000000000, 0.000000000000000000, 1.000000000000000000 ) ) ;
#19082 = ORIENTED_EDGE ( 'NONE', *, *, #5365, .T. ) ;
#19083 = ORIENTED_EDGE ( 'NONE', *, *, #116649, .T. ) ;
#19084 = AXIS2_PLACEMENT_3D ( 'NONE', #23388, #35023, #3749 ) ;
#19085 = DIRECTION ( 'NONE',  ( 0.7071067811865487940, 0.7071067811865463515, 0.000000000000000000 ) ) ;
#19086 = MECHANICAL_DESIGN_GEOMETRIC_PRESENTATION_REPRESENTATION (  '', ( #74686 ), #30704 ) ;
#19087 = PLANE ( 'NONE',  #48618 ) ;
#19088 = ORIENTED_EDGE ( 'NONE', *, *, #59925, .T. ) ;
#19090 = EDGE_CURVE ( 'NONE', #131612, #54251, #26686, .T. ) ;
#19089 = CARTESIAN_POINT ( 'NONE',  ( -34.80981832425529632, -18.74070752338408852, 7.910009926591588858 ) ) ;
#19091 = CARTESIAN_POINT ( 'NONE',  ( -1.954842266633324943, -21.74070752338406010, 21.72585301388583900 ) ) ;
#19092 = CARTESIAN_POINT ( 'NONE',  ( -54.29974487139159578, -27.71228299555243879, 4.000000000000000000 ) ) ;
#19093 = PLANE ( 'NONE',  #68596 ) ;
#19094 = ORIENTED_EDGE ( 'NONE', *, *, #81999, .T. ) ;
#19095 = FACE_OUTER_BOUND ( 'NONE', #67625, .T. ) ;
#19096 = DIRECTION ( 'NONE',  ( -1.000000000000000000, -1.224606353822377258E-16, -0.000000000000000000 ) ) ;
#19097 = CARTESIAN_POINT ( 'NONE',  ( 34.82816939922328459, 6.759292476615649470, 4.000000000000000000 ) ) ;
#19098 = DIRECTION ( 'NONE',  ( 1.000000000000000000, 0.000000000000000000, 0.000000000000000000 ) ) ;
#19099 = LINE ( 'NONE', #116979, #42723 ) ;
#19100 = CARTESIAN_POINT ( 'NONE',  ( 104.7875270504628986, 0.000000000000000000, -7.949999999999998401 ) ) ;
#19101 = CARTESIAN_POINT ( 'NONE',  ( 54.03752705046288440, -9.735942053221456900E-16, 7.949999999999998401 ) ) ;
#19102 = EDGE_CURVE ( 'NONE', #16920, #89076, #84642, .T. ) ;
#19104 = DIRECTION ( 'NONE',  ( 0.6830127018922180770, -0.6830127018922204085, -0.2588190451025213501 ) ) ;
#19103 = VECTOR ( 'NONE', #103880, 1000.000000000000000 ) ;
#19105 = ORIENTED_EDGE ( 'NONE', *, *, #82466, .F. ) ;
#19106 = ORIENTED_EDGE ( 'NONE', *, *, #120231, .F. ) ;
#19107 = CARTESIAN_POINT ( 'NONE',  ( 51.60416666666665009, 2.130196079827422206, 7.950000000000001954 ) ) ;
#19108 = DIRECTION ( 'NONE',  ( -1.000000000000000000, -1.224606353822377258E-16, -0.000000000000000000 ) ) ;
#19109 = EDGE_CURVE ( 'NONE', #35471, #14309, #16498, .T. ) ;
#19110 = DIRECTION ( 'NONE',  ( -8.817971600062199903E-18, 0.3543493200069153248, 0.9351131265310292928 ) ) ;
#19111 = ADVANCED_FACE ( 'NONE', ( #37579 ), #51308, .F. ) ;
#19112 = PLANE ( 'NONE',  #32171 ) ;
#19113 = ORIENTED_EDGE ( 'NONE', *, *, #92054, .T. ) ;
#19114 = EDGE_CURVE ( 'NONE', #89949, #33791, #5619, .T. ) ;
#19115 = VECTOR ( 'NONE', #87311, 1000.000000000000000 ) ;
#19116 = CARTESIAN_POINT ( 'NONE',  ( 31.49999999999977973, 3.653845994658420970, -4.504631822206443204 ) ) ;
#19117 = CARTESIAN_POINT ( 'NONE',  ( 49.43793019189809002, -6.110000000000001208, 1.637169565754158951 ) ) ;
#19118 = AXIS2_PLACEMENT_3D ( 'NONE', #81665, #126544, #47618 ) ;
#19119 = ORIENTED_EDGE ( 'NONE', *, *, #38630, .F. ) ;
#19120 = CARTESIAN_POINT ( 'NONE',  ( 37.74999999999999289, -9.735942053221458872E-16, 7.950000000000000178 ) ) ;
#19121 = VERTEX_POINT ( 'NONE', #15751 ) ;
#19122 = ORIENTED_EDGE ( 'NONE', *, *, #115611, .F. ) ;
#19123 = STYLED_ITEM ( 'NONE', ( #136610 ), #2933 ) ;
#19124 = AXIS2_PLACEMENT_3D ( 'NONE', #84232, #40705, #95057 ) ;
#19125 = LINE ( 'NONE', #72126, #583 ) ;
#19126 = CARTESIAN_POINT ( 'NONE',  ( 47.99451991528749062, 28.92564299267971251, 4.000000000000000000 ) ) ;
#19127 = CARTESIAN_POINT ( 'NONE',  ( -45.18398860626900415, 28.73617430169818832, 5.000000000000000000 ) ) ;
#19128 = EDGE_CURVE ( 'NONE', #22127, #137445, #73079, .T. ) ;
#19129 = EDGE_LOOP ( 'NONE', ( #100706, #36273, #44236, #72377 ) ) ;
#19130 = EDGE_CURVE ( 'NONE', #56540, #4701, #139026, .T. ) ;
#19131 = DIRECTION ( 'NONE',  ( 0.7071067811865486830, -0.7071067811865464625, -0.000000000000000000 ) ) ;
#19133 = ORIENTED_EDGE ( 'NONE', *, *, #8639, .T. ) ;
#19132 = DIRECTION ( 'NONE',  ( -0.000000000000000000, 0.3543493200069153248, 0.9351131265310292928 ) ) ;
#19134 = LINE ( 'NONE', #120551, #87845 ) ;
#19135 = CARTESIAN_POINT ( 'NONE',  ( -0.8382938754737979670, -6.740707523384212863, 16.75550250614867309 ) ) ;
#19136 = CARTESIAN_POINT ( 'NONE',  ( 19.49999999999987210, -10.91253812416064228, 4.000000000000000000 ) ) ;
#19137 = CARTESIAN_POINT ( 'NONE',  ( -10.49999999999991651, -14.94781430457067195, 5.000000000000000000 ) ) ;
#19138 = EDGE_CURVE ( 'NONE', #131955, #114421, #128161, .T. ) ;
#19139 = VERTEX_POINT ( 'NONE', #128845 ) ;
#19140 = ORIENTED_EDGE ( 'NONE', *, *, #7099, .F. ) ;
#19141 = B_SPLINE_CURVE_WITH_KNOTS ( 'NONE', 3,
 ( #52692, #53417, #84628, #19364 ),
 .UNSPECIFIED., .F., .F.,
 ( 4, 4 ),
 ( 0.003785693138453205195, 0.004021000868919195545 ),
 .UNSPECIFIED. ) ;
#19142 = DIRECTION ( 'NONE',  ( 0.7071067811865486830, -0.7071067811865463515, 0.000000000000000000 ) ) ;
#19143 = CARTESIAN_POINT ( 'NONE',  ( 69.03709685856478018, -3.054999999999998828, -5.291415217122919401 ) ) ;
#19144 = DIRECTION ( 'NONE',  ( -0.6830127018922181881, 0.6830127018922202975, -0.2588190451025214056 ) ) ;
#19145 = VECTOR ( 'NONE', #93877, 1000.000000000000114 ) ;
#19146 = CARTESIAN_POINT ( 'NONE',  ( -27.98911971346032601, -22.02621442084248216, 4.990779571109220214 ) ) ;
#19147 = CARTESIAN_POINT ( 'NONE',  ( 4.499999999999970690, 6.431123077392120635, 4.000000000000000000 ) ) ;
#19148 = ORIENTED_EDGE ( 'NONE', *, *, #4059, .F. ) ;
#19150 = EDGE_CURVE ( 'NONE', #27298, #23510, #49177, .T. ) ;
#19149 = ORIENTED_EDGE ( 'NONE', *, *, #127993, .T. ) ;
#19151 = VECTOR ( 'NONE', #14278, 1000.000000000000000 ) ;
#19152 = CARTESIAN_POINT ( 'NONE',  ( 42.18398860626899705, 28.73617430169816700, 5.000000000000000000 ) ) ;
#19153 = CARTESIAN_POINT ( 'NONE',  ( 27.29974487139158512, -27.71228299555225405, 4.000000000000000000 ) ) ;
#19154 = ORIENTED_EDGE ( 'NONE', *, *, #36349, .F. ) ;
#19155 = ORIENTED_EDGE ( 'NONE', *, *, #84240, .T. ) ;
#19156 = DIRECTION ( 'NONE',  ( 0.6830127018922181881, 0.6830127018922202975, -0.2588190451025214056 ) ) ;
#19157 = ORIENTED_EDGE ( 'NONE', *, *, #107223, .F. ) ;
#19158 = CARTESIAN_POINT ( 'NONE',  ( 122.6835989386367771, -43.14999999999999147, -34.92499999999998295 ) ) ;
#19159 = CARTESIAN_POINT ( 'NONE',  ( 1.199999999999999956, 0.5999999999999987566, 4.543283425070392845 ) ) ;
#19160 = EDGE_CURVE ( 'NONE', #64078, #26808, #88218, .T. ) ;
#19161 = VECTOR ( 'NONE', #36791, 1000.000000000000227 ) ;
#19162 = DIRECTION ( 'NONE',  ( -0.7071067811865486830, -0.7071067811865464625, 0.000000000000000000 ) ) ;
#19163 = FACE_BOUND ( 'NONE', #50569, .T. ) ;
#19164 = DIRECTION ( 'NONE',  ( 0.000000000000000000, -1.000000000000000000, 0.000000000000000000 ) ) ;
#19165 = CARTESIAN_POINT ( 'NONE',  ( 0.000000000000000000, -57.15000000000003411, -15.92500000000064730 ) ) ;
#19166 = CARTESIAN_POINT ( 'NONE',  ( -78.18398860626899705, 28.73617430169841924, 5.000000000000000000 ) ) ;
#19167 = AXIS2_PLACEMENT_3D ( 'NONE', #59285, #103439, #91861 ) ;
#19168 = CARTESIAN_POINT ( 'NONE',  ( 7.171830600776422315, -11.24070752338416845, 4.000000000000000000 ) ) ;
#19170 = EDGE_LOOP ( 'NONE', ( #118011, #119347, #142983, #46148 ) ) ;
#19169 = LINE ( 'NONE', #44531, #96780 ) ;
#19171 = CARTESIAN_POINT ( 'NONE',  ( -60.48921356237309510, -27.52281430457097500, 5.000000000000000000 ) ) ;
#19172 = ITEM_DEFINED_TRANSFORMATION ( 'NONE', 'NONE', #58680,  #127880 ) ;
#19173 = ORIENTED_EDGE ( 'NONE', *, *, #31991, .F. ) ;
#19174 = EDGE_LOOP ( 'NONE', ( #22701, #68483, #49166, #38239, #116343 ) ) ;
#19175 = CARTESIAN_POINT ( 'NONE',  ( 86.97459685856479439, 1.637169565754164280, -6.109999999999996767 ) ) ;
#19176 = ORIENTED_EDGE ( 'NONE', *, *, #54945, .T. ) ;
#19177 = CARTESIAN_POINT ( 'NONE',  ( -51.18398860626899705, 28.73617430169823095, 5.000000000000000000 ) ) ;
#19178 = DIRECTION ( 'NONE',  ( 0.7071067811865487940, -0.7071067811865463515, 0.000000000000000000 ) ) ;
#19179 = EDGE_CURVE ( 'NONE', #140087, #41095, #22209, .T. ) ;
#19180 = LINE ( 'NONE', #51111, #5020 ) ;
#19181 = AXIS2_PLACEMENT_3D ( 'NONE', #29212, #85022, #97294 ) ;
#19182 = VECTOR ( 'NONE', #137093, 1000.000000000000000 ) ;
#19183 = CARTESIAN_POINT ( 'NONE',  ( -19.05000000000000071, 3.174999999999997158, 4.000000000000000000 ) ) ;
#19184 = CARTESIAN_POINT ( 'NONE',  ( -18.18398860626898994, 28.73617430169800002, 5.000000000000000000 ) ) ;
#19185 = FACE_OUTER_BOUND ( 'NONE', #30615, .T. ) ;
#19186 = EDGE_CURVE ( 'NONE', #55371, #92458, #29392, .T. ) ;
#19187 = DIRECTION ( 'NONE',  ( 0.7071067811865486830, -0.7071067811865464625, -0.000000000000000000 ) ) ;
#19188 = LINE ( 'NONE', #64846, #88921 ) ;
#19189 = CARTESIAN_POINT ( 'NONE',  ( -14.99999999999990230, -22.22500000000000142, 4.412002311790018894 ) ) ;
#19190 = DIRECTION ( 'NONE',  ( -0.6830127018922180770, -0.6830127018922204085, -0.2588190451025213501 ) ) ;
#19191 = ORIENTED_EDGE ( 'NONE', *, *, #37322, .T. ) ;
#19192 = VECTOR ( 'NONE', #67001, 999.9999999999998863 ) ;
#19193 = PRESENTATION_LAYER_ASSIGNMENT (  '', '', ( #21481 ) ) ;
#19194 = CARTESIAN_POINT ( 'NONE',  ( -38.99451991528749062, 28.92564299267965211, 4.000000000000000000 ) ) ;
#19195 = ORIENTED_EDGE ( 'NONE', *, *, #15785, .F. ) ;
#19196 = CARTESIAN_POINT ( 'NONE',  ( 122.5791937171295700, 3.975000000000002753, -6.884901960086283523 ) ) ;
#19197 = FACE_OUTER_BOUND ( 'NONE', #33097, .T. ) ;
#19198 = VERTEX_POINT ( 'NONE', #87497 ) ;
#19199 = VERTEX_POINT ( 'NONE', #19377 ) ;
#19200 = EDGE_CURVE ( 'NONE', #14243, #20682, #8453, .T. ) ;
#19201 = EDGE_LOOP ( 'NONE', ( #82844, #134131, #29178, #81857 ) ) ;
#19202 = CARTESIAN_POINT ( 'NONE',  ( 38.93793019189809002, -6.110000000000001208, 1.637169565754158951 ) ) ;
#19203 = ORIENTED_EDGE ( 'NONE', *, *, #96338, .F. ) ;
#19204 = FACE_OUTER_BOUND ( 'NONE', #122374, .T. ) ;
#19205 = AXIS2_PLACEMENT_3D ( 'NONE', #95373, #65662, #62775 ) ;
#19206 = CARTESIAN_POINT ( 'NONE',  ( 24.25413961620377279, 3.047499999999993214, -5.278424836066146320 ) ) ;
#19207 = CARTESIAN_POINT ( 'NONE',  ( 15.02190751083870524, 7.730481892681857481, -28.15093226488858491 ) ) ;
#19208 = EDGE_LOOP ( 'NONE', ( #89462, #57798, #59589, #138131 ) ) ;
#19209 = FACE_OUTER_BOUND ( 'NONE', #67168, .T. ) ;
#19210 = ORIENTED_EDGE ( 'NONE', *, *, #85208, .T. ) ;
#19211 = DIRECTION ( 'NONE',  ( 0.3543493200069162685, -0.000000000000000000, -0.9351131265310288487 ) ) ;
#19212 = DIRECTION ( 'NONE',  ( -0.6830127018922181881, 0.6830127018922202975, -0.2588190451025214056 ) ) ;
#19214 = VERTEX_POINT ( 'NONE', #129553 ) ;
#19213 = PLANE ( 'NONE',  #125817 ) ;
#19215 = ORIENTED_EDGE ( 'NONE', *, *, #134026, .F. ) ;
#19216 = DIRECTION ( 'NONE',  ( -0.6830127018922180770, -0.6830127018922204085, -0.2588190451025213501 ) ) ;
#19217 = VECTOR ( 'NONE', #56349, 1000.000000000000000 ) ;
#19218 = EDGE_CURVE ( 'NONE', #73986, #102653, #93339, .T. ) ;
#19219 = DIRECTION ( 'NONE',  ( 0.7071067811865487940, -0.7071067811865463515, 0.000000000000000000 ) ) ;
#19220 = VERTEX_POINT ( 'NONE', #141899 ) ;
#19221 = CARTESIAN_POINT ( 'NONE',  ( 109.6000270504628844, 5.819803920172570422, 5.819803920172575751 ) ) ;
#19222 = ORIENTED_EDGE ( 'NONE', *, *, #43191, .F. ) ;
#19223 = PRODUCT_DEFINITION_SHAPE ( 'NONE', 'NONE',  #143569 ) ;
#19225 = ORIENTED_EDGE ( 'NONE', *, *, #13663, .F. ) ;
#19224 = EDGE_CURVE ( 'NONE', #120628, #92397, #33157, .T. ) ;
#19226 = AXIS2_PLACEMENT_3D ( 'NONE', #11162, #43139, #55439 ) ;
#19227 = EDGE_LOOP ( 'NONE', ( #14612, #132302, #134639, #31300 ) ) ;
#19228 = FACE_OUTER_BOUND ( 'NONE', #34167, .T. ) ;
#19229 = LINE ( 'NONE', #28699, #74721 ) ;
#19230 = DIRECTION ( 'NONE',  ( 0.7071067811865486830, -0.7071067811865464625, -0.000000000000000000 ) ) ;
#19232 = EDGE_CURVE ( 'NONE', #89674, #129739, #75905, .T. ) ;
#19231 = DIRECTION ( 'NONE',  ( 0.7071067811865486830, -0.7071067811865464625, -0.000000000000000000 ) ) ;
#19233 = CARTESIAN_POINT ( 'NONE',  ( 4.495848767239241539, 4.584330080086930965E-16, 0.000000000000000000 ) ) ;
#19234 = ORIENTED_EDGE ( 'NONE', *, *, #114902, .F. ) ;
#19235 = EDGE_CURVE ( 'NONE', #140787, #135668, #58252, .T. ) ;
#19236 = CARTESIAN_POINT ( 'NONE',  ( 16.96659967656967893, 6.759292476615653023, 12.28218704918526072 ) ) ;
#19237 = ORIENTED_EDGE ( 'NONE', *, *, #38013, .T. ) ;
#19238 = CARTESIAN_POINT ( 'NONE',  ( -5.999999999999960032, 5.966399257802207146, 5.000000000000000000 ) ) ;
#19239 = CARTESIAN_POINT ( 'NONE',  ( 31.62456980810188867, -6.871911579029512218, 3.967499999999996252 ) ) ;
#19241 = ORIENTED_EDGE ( 'NONE', *, *, #134164, .T. ) ;
#19240 = VECTOR ( 'NONE', #35868, 1000.000000000000114 ) ;
#19242 = CARTESIAN_POINT ( 'NONE',  ( 16.61159235450331906, 9.902892378096218942E-16, 0.000000000000000000 ) ) ;
#19243 =( BOUNDED_CURVE ( )  B_SPLINE_CURVE ( 3, ( #114751, #14753, #103183, #26354 ),
 .UNSPECIFIED., .F., .T. ) 
 B_SPLINE_CURVE_WITH_KNOTS ( ( 4, 4 ),
 ( 5.920967161967926273, 7.341195215986584977 ),
 .UNSPECIFIED. ) 
 CURVE ( )  GEOMETRIC_REPRESENTATION_ITEM ( )  RATIONAL_B_SPLINE_CURVE ( ( 1.000000000000000000, 0.8388583629366725969, 0.8388583629366725969, 1.000000000000000000 ) ) 
 REPRESENTATION_ITEM ( '' )  );
#19244 = LINE ( 'NONE', #9783, #127758 ) ;
#19245 = ORIENTED_EDGE ( 'NONE', *, *, #104548, .T. ) ;
#19246 = ORIENTED_EDGE ( 'NONE', *, *, #80131, .T. ) ;
#19247 = AXIS2_PLACEMENT_3D ( 'NONE', #111914, #12575, #56856 ) ;
#19248 = CARTESIAN_POINT ( 'NONE',  ( -11.99999999999990585, -13.44781430457068794, 5.000000000000000000 ) ) ;
#19249 = CARTESIAN_POINT ( 'NONE',  ( -12.69999999999998153, 0.000000000000000000, 2.500000000000000444 ) ) ;
#19250 = CARTESIAN_POINT ( 'NONE',  ( -25.17183060077629619, -8.240707523384200428, 4.000000000000000000 ) ) ;
#19251 = VECTOR ( 'NONE', #136976, 1000.000000000000227 ) ;
#19252 = LINE ( 'NONE', #128725, #93725 ) ;
#19253 = LINE ( 'NONE', #6899, #108323 ) ;
#19254 = CARTESIAN_POINT ( 'NONE',  ( 64.80793019189812298, -6.109999999999999432, 1.637169565754158507 ) ) ;
#19255 = EDGE_CURVE ( 'NONE', #23291, #43567, #43997, .T. ) ;
#19256 = DIRECTION ( 'NONE',  ( -0.000000000000000000, 0.000000000000000000, 1.000000000000000000 ) ) ;
#19257 = DIRECTION ( 'NONE',  ( 0.7071067811865487940, 0.7071067811865463515, 0.000000000000000000 ) ) ;
#19258 = DIRECTION ( 'NONE',  ( 0.000000000000000000, -1.000000000000000000, 0.000000000000000000 ) ) ;
#19259 = CARTESIAN_POINT ( 'NONE',  ( 7.326124847093153925, 4.202752102959690472E-16, 0.000000000000000000 ) ) ;
#19260 = VERTEX_POINT ( 'NONE', #54190 ) ;
#19261 = CARTESIAN_POINT ( 'NONE',  ( -17.92867102513379862, 9.037728232668255757, 5.000000000000000000 ) ) ;
#19262 = ORIENTED_EDGE ( 'NONE', *, *, #97463, .T. ) ;
#19263 = VECTOR ( 'NONE', #13168, 1000.000000000000000 ) ;
#19264 = LINE ( 'NONE', #15126, #693 ) ;
#19265 = LINE ( 'NONE', #120698, #137952 ) ;
#19266 = ORIENTED_EDGE ( 'NONE', *, *, #75462, .T. ) ;
#19267 = DIRECTION ( 'NONE',  ( 0.7071067811865487940, -0.7071067811865463515, 0.000000000000000000 ) ) ;
#19269 = EDGE_LOOP ( 'NONE', ( #96117, #12731, #136659, #57032 ) ) ;
#19268 = LINE ( 'NONE', #76527, #39612 ) ;
#19270 = PLANE ( 'NONE',  #129557 ) ;
#19271 = CARTESIAN_POINT ( 'NONE',  ( -42.29974487139158157, -27.71228299555235708, 4.000000000000000000 ) ) ;
#19272 = CARTESIAN_POINT ( 'NONE',  ( -37.64175702458837236, 15.75929247661555088, 19.34181609438708449 ) ) ;
#19273 = ORIENTED_EDGE ( 'NONE', *, *, #42598, .F. ) ;
#19275 = VERTEX_POINT ( 'NONE', #86792 ) ;
#19274 = AXIS2_PLACEMENT_3D ( 'NONE', #92390, #93133, #27150 ) ;
#19276 = CARTESIAN_POINT ( 'NONE',  ( -34.92500000000001137, 22.22500000000000142, 4.000000000000000000 ) ) ;
#19277 = CARTESIAN_POINT ( 'NONE',  ( 10.94186803553636977, 3.821174125832445049E-16, 0.000000000000000000 ) ) ;
#19278 = CARTESIAN_POINT ( 'NONE',  ( -12.13499573751615124, 3.759292476615685441, 15.36553568819729065 ) ) ;
#19279 = CARTESIAN_POINT ( 'NONE',  ( 92.24586038379622721, 3.974999999999996980, 6.884901960086287964 ) ) ;
#19280 = DIRECTION ( 'NONE',  ( 0.6830127018922181881, 0.6830127018922202975, -0.2588190451025214056 ) ) ;
#19281 = EDGE_CURVE ( 'NONE', #114028, #128067, #131009, .T. ) ;
#19282 = CARTESIAN_POINT ( 'NONE',  ( -25.49999999999982236, -5.568876922607755908, 4.000000000000000000 ) ) ;
#19283 = ORIENTED_EDGE ( 'NONE', *, *, #28617, .F. ) ;
#19284 = LINE ( 'NONE', #75124, #77027 ) ;
#19285 = ADVANCED_FACE ( 'NONE', ( #30248 ), #85329, .F. ) ;
#19286 = DIRECTION ( 'NONE',  ( -0.000000000000000000, 0.000000000000000000, 1.000000000000000000 ) ) ;
#19287 = CARTESIAN_POINT ( 'NONE',  ( 32.22916666666666430, -6.094999999999989093, 1.633150327867691765 ) ) ;
#19288 = ORIENTED_EDGE ( 'NONE', *, *, #64644, .F. ) ;
#19289 = EDGE_CURVE ( 'NONE', #120806, #14374, #141142, .T. ) ;
#19290 = EDGE_CURVE ( 'NONE', #5092, #63283, #30993, .T. ) ;
#19291 = VECTOR ( 'NONE', #7215, 1000.000000000000000 ) ;
#19292 = CARTESIAN_POINT ( 'NONE',  ( 41.99451991528749062, 28.92564299267967343, 4.000000000000000000 ) ) ;
#19293 = EDGE_LOOP ( 'NONE', ( #59158, #50522, #133619, #55623, #26521, #138751, #3201, #142303 ) ) ;
#19294 = CARTESIAN_POINT ( 'NONE',  ( 78.02126352523146124, -4.472830434245839371, -4.472830434245840259 ) ) ;
#19295 = DIRECTION ( 'NONE',  ( 1.000000000000000000, 0.000000000000000000, -0.000000000000000000 ) ) ;
#19297 = CARTESIAN_POINT ( 'NONE',  ( 42.48921356237308800, -27.52281430457085065, 5.000000000000000000 ) ) ;
#19296 = VECTOR ( 'NONE', #86384, 1000.000000000000000 ) ;
#19298 = EDGE_LOOP ( 'NONE', ( #83849, #128857, #30648, #94914 ) ) ;
#19299 = FACE_OUTER_BOUND ( 'NONE', #30987, .T. ) ;
#19300 = DIRECTION ( 'NONE',  ( 0.7071067811865486830, -0.7071067811865464625, -0.000000000000000000 ) ) ;
#19301 = EDGE_CURVE ( 'NONE', #114199, #135973, #65790, .T. ) ;
#19302 = CARTESIAN_POINT ( 'NONE',  ( 1.042387978378689573, 0.3999999999999995781, 2.015694669338588429 ) ) ;
#19303 = EDGE_CURVE ( 'NONE', #1414, #97534, #42593, .T. ) ;
#19304 = LINE ( 'NONE', #120005, #106429 ) ;
#19306 = ORIENTED_EDGE ( 'NONE', *, *, #22569, .F. ) ;
#19305 = CARTESIAN_POINT ( 'NONE',  ( 24.56840764549667355, 9.139736423841732040E-16, 0.000000000000000000 ) ) ;
#19307 = CARTESIAN_POINT ( 'NONE',  ( 0.1839886062690032631, 28.73617430169787568, 5.000000000000000000 ) ) ;
#19308 = LINE ( 'NONE', #63564, #61590 ) ;
#19309 = LINE ( 'NONE', #9091, #61027 ) ;
#19310 = CARTESIAN_POINT ( 'NONE',  ( 181.1500000000000057, -3.180000000000061444, -34.92499999999998295 ) ) ;
#19311 = EDGE_LOOP ( 'NONE', ( #63256, #85091, #4322, #88523 ) ) ;
#19312 = EDGE_CURVE ( 'NONE', #102663, #106069, #10617, .T. ) ;
#19313 = VERTEX_POINT ( 'NONE', #143295 ) ;
#19314 = CARTESIAN_POINT ( 'NONE',  ( 77.58376352523144703, -6.110000000000001208, -3.741295971395164515E-16 ) ) ;
#19315 = PRESENTATION_LAYER_ASSIGNMENT (  '', '', ( #128099 ) ) ;
#19316 = ORIENTED_EDGE ( 'NONE', *, *, #48524, .T. ) ;
#19317 = CARTESIAN_POINT ( 'NONE',  ( -9.183988606268997046, 28.73617430169793607, 5.000000000000000000 ) ) ;
#19318 = LINE ( 'NONE', #98321, #57284 ) ;
#19319 = CARTESIAN_POINT ( 'NONE',  ( -32.99999999999976552, 10.55218569542905627, 5.000000000000000000 ) ) ;
#19320 = LINE ( 'NONE', #10559, #26981 ) ;
#19321 = ORIENTED_EDGE ( 'NONE', *, *, #80724, .F. ) ;
#19322 = EDGE_CURVE ( 'NONE', #141841, #22237, #102667, .T. ) ;
#19323 = CARTESIAN_POINT ( 'NONE',  ( -23.99451991528749062, 28.92564299267954908, 4.000000000000000000 ) ) ;
#19324 = CARTESIAN_POINT ( 'NONE',  ( 181.1500000000000057, -43.14999999999999147, -31.92499999999998295 ) ) ;
#19325 = VECTOR ( 'NONE', #99789, 1000.000000000000227 ) ;
#19326 = EDGE_LOOP ( 'NONE', ( #88045, #35657, #3359, #134927 ) ) ;
#19327 = AXIS2_PLACEMENT_3D ( 'NONE', #112418, #137022, #15904 ) ;
#19328 = CARTESIAN_POINT ( 'NONE',  ( 0.4283298879861147102, -1.252411602983660499, 3.977815754073098287 ) ) ;
#19329 = DIRECTION ( 'NONE',  ( 1.000000000000000000, 0.000000000000000000, 0.000000000000000000 ) ) ;
#19330 = EDGE_CURVE ( 'NONE', #68806, #106934, #63728, .T. ) ;
#19331 = PLANE ( 'NONE',  #130319 ) ;
#19332 = ORIENTED_EDGE ( 'NONE', *, *, #47579, .T. ) ;
#19334 = ORIENTED_EDGE ( 'NONE', *, *, #79856, .T. ) ;
#19333 = VECTOR ( 'NONE', #143147, 1000.000000000000227 ) ;
#19335 = FACE_BOUND ( 'NONE', #82899, .T. ) ;
#19336 = DIRECTION ( 'NONE',  ( -1.000000000000000000, -0.000000000000000000, -0.000000000000000000 ) ) ;
#19337 = EDGE_CURVE ( 'NONE', #112685, #81140, #57744, .T. ) ;
#19338 = CARTESIAN_POINT ( 'NONE',  ( 127.4302689125804733, -3.175000000000002043, 5.499261314031184789 ) ) ;
#19339 = CARTESIAN_POINT ( 'NONE',  ( -36.48921356237310221, -27.52281430457080802, 5.000000000000000000 ) ) ;
#19340 = ADVANCED_FACE ( 'NONE', ( #122238 ), #80907, .T. ) ;
#19341 = LINE ( 'NONE', #96158, #136042 ) ;
#19342 = VECTOR ( 'NONE', #83761, 1000.000000000000114 ) ;
#19343 = CARTESIAN_POINT ( 'NONE',  ( 56.99451991528749062, 28.92564299267978001, 4.000000000000000000 ) ) ;
#19345 = ADVANCED_FACE ( 'NONE', ( #88944 ), #111365, .F. ) ;
#19344 = SURFACE_STYLE_USAGE ( .BOTH. , #142564 ) ;
#19346 = ORIENTED_EDGE ( 'NONE', *, *, #89352, .F. ) ;
#19347 = VECTOR ( 'NONE', #8319, 1000.000000000000000 ) ;
#19348 = ORIENTED_EDGE ( 'NONE', *, *, #46008, .F. ) ;
#19349 = VERTEX_POINT ( 'NONE', #24372 ) ;
#19350 = ORIENTED_EDGE ( 'NONE', *, *, #57228, .F. ) ;
#19351 = AXIS2_PLACEMENT_3D ( 'NONE', #82429, #5548, #27304 ) ;
#19352 = CARTESIAN_POINT ( 'NONE',  ( -32.99999999999976552, -6.033600742197672950, 5.000000000000000000 ) ) ;
#19353 = CARTESIAN_POINT ( 'NONE',  ( -34.49999999999974420, -14.70932175296479549, -11.46312253303829287 ) ) ;
#19354 = PLANE ( 'NONE',  #1106 ) ;
#19355 = VERTEX_POINT ( 'NONE', #79527 ) ;
#19356 = DIRECTION ( 'NONE',  ( 0.000000000000000000, 0.000000000000000000, -1.000000000000000000 ) ) ;
#19357 = DIRECTION ( 'NONE',  ( -0.7071067811865486830, -0.7071067811865464625, 0.000000000000000000 ) ) ;
#19358 = CARTESIAN_POINT ( 'NONE',  ( -20.99999999999985079, -7.068876922607739921, 4.000000000000000000 ) ) ;
#19359 = CARTESIAN_POINT ( 'NONE',  ( 1.828169399223516400, 12.75929247661558996, 4.000000000000000000 ) ) ;
#19360 = VECTOR ( 'NONE', #106757, 1000.000000000000227 ) ;
#19361 = LINE ( 'NONE', #63613, #58397 ) ;
#19362 = ORIENTED_EDGE ( 'NONE', *, *, #134870, .T. ) ;
#19363 = DIRECTION ( 'NONE',  ( 0.7071067811865487940, 0.7071067811865463515, 0.000000000000000000 ) ) ;
#19364 = CARTESIAN_POINT ( 'NONE',  ( 0.000000000000000000, -0.4000000000000003553, 2.015694669338588429 ) ) ;
#19365 = EDGE_LOOP ( 'NONE', ( #113951, #13083, #125780, #48250 ) ) ;
#19366 = LINE ( 'NONE', #34350, #89783 ) ;
#19367 = ORIENTED_EDGE ( 'NONE', *, *, #41600, .T. ) ;
#19368 = ORIENTED_EDGE ( 'NONE', *, *, #97359, .F. ) ;
#19369 = AXIS2_PLACEMENT_3D ( 'NONE', #33965, #9285, #42707 ) ;
#19370 = CARTESIAN_POINT ( 'NONE',  ( 63.00043019189810423, -3.055000000000002380, 5.291415217122920289 ) ) ;
#19371 = ORIENTED_EDGE ( 'NONE', *, *, #136334, .F. ) ;
#19372 = ORIENTED_EDGE ( 'NONE', *, *, #102377, .T. ) ;
#19373 = CARTESIAN_POINT ( 'NONE',  ( 12.40000000000000213, 2.055000000000001492, 2.516649172247811554E-16 ) ) ;
#19374 = VECTOR ( 'NONE', #86070, 999.9999999999998863 ) ;
#19375 = FACE_OUTER_BOUND ( 'NONE', #17900, .T. ) ;
#19376 = CARTESIAN_POINT ( 'NONE',  ( 100.9170968585647756, 3.054999999999998828, 5.291415217122922066 ) ) ;
#19377 = CARTESIAN_POINT ( 'NONE',  ( -11.67183060077638501, -21.74070752338405654, 4.000000000000000000 ) ) ;
#19378 = EDGE_CURVE ( 'NONE', #107763, #57164, #34543, .T. ) ;
#19379 = LINE ( 'NONE', #83960, #35125 ) ;
#19380 = DIRECTION ( 'NONE',  ( -1.000000000000000000, 0.000000000000000000, 0.000000000000000000 ) ) ;
#19381 = FACE_OUTER_BOUND ( 'NONE', #46541, .T. ) ;
#19382 = VECTOR ( 'NONE', #70225, 1000.000000000000000 ) ;
#19383 = CARTESIAN_POINT ( 'NONE',  ( 90.83333333333332860, -6.884901960086287964, 3.974999999999998312 ) ) ;
#19384 = DIRECTION ( 'NONE',  ( -1.000000000000000000, -1.224606353822377258E-16, -0.000000000000000000 ) ) ;
#19385 = ORIENTED_EDGE ( 'NONE', *, *, #96005, .F. ) ;
#19386 = CARTESIAN_POINT ( 'NONE',  ( 34.92499999999998295, 1.701930566820966773, 4.500000000000000888 ) ) ;
#19387 = EDGE_LOOP ( 'NONE', ( #4705, #40824, #67869, #86844 ) ) ;
#19388 = VERTEX_POINT ( 'NONE', #89627 ) ;
#19389 = ORIENTED_EDGE ( 'NONE', *, *, #80983, .F. ) ;
#19390 = ORIENTED_EDGE ( 'NONE', *, *, #119507, .T. ) ;
#19391 = DIRECTION ( 'NONE',  ( 0.7071067811865487940, -0.7071067811865463515, 0.000000000000000000 ) ) ;
#19392 = CARTESIAN_POINT ( 'NONE',  ( 34.49999999999976552, -14.94567065516889848, 4.994342998332158778 ) ) ;
#19393 = EDGE_CURVE ( 'NONE', #95492, #123094, #25066, .T. ) ;
#19394 = DIRECTION ( 'NONE',  ( -0.000000000000000000, -0.3543493200069152693, 0.9351131265310292928 ) ) ;
#19395 = ORIENTED_EDGE ( 'NONE', *, *, #128914, .T. ) ;
#19396 = EDGE_CURVE ( 'NONE', #51247, #5949, #2596, .T. ) ;
#19397 = CARTESIAN_POINT ( 'NONE',  ( 0.4397996348757138296, -49.08473565290604768, 39.91868829876761282 ) ) ;
#19398 = ORIENTED_EDGE ( 'NONE', *, *, #123556, .T. ) ;
#19399 = AXIS2_PLACEMENT_3D ( 'NONE', #104581, #103150, #93713 ) ;
#19400 =( GEOMETRIC_REPRESENTATION_CONTEXT ( 3 ) GLOBAL_UNCERTAINTY_ASSIGNED_CONTEXT ( ( #57641 ) ) GLOBAL_UNIT_ASSIGNED_CONTEXT ( ( #49956, #73831, #29593 ) ) REPRESENTATION_CONTEXT ( 'NONE', 'WORKASPACE' ) );
#19401 = CARTESIAN_POINT ( 'NONE',  ( 3.624569808101886448, -6.871911579029512218, 3.967499999999996252 ) ) ;
#19402 = PLANE ( 'NONE',  #48485 ) ;
#19403 = CARTESIAN_POINT ( 'NONE',  ( 9.299744871391588674, -27.71228299555212971, 4.000000000000000000 ) ) ;
#19404 = EDGE_CURVE ( 'NONE', #52329, #80109, #1165, .T. ) ;
#19405 = DIRECTION ( 'NONE',  ( -0.7071067811865486830, 0.7071067811865464625, 0.000000000000000000 ) ) ;
#19406 = VERTEX_POINT ( 'NONE', #80216 ) ;
#19407 = ORIENTED_EDGE ( 'NONE', *, *, #52461, .T. ) ;
#19408 = ORIENTED_EDGE ( 'NONE', *, *, #12008, .T. ) ;
#19409 = CARTESIAN_POINT ( 'NONE',  ( 11.15159235450332176, 9.902892378096218942E-16, 0.000000000000000000 ) ) ;
#19410 = CARTESIAN_POINT ( 'NONE',  ( -28.49999999999980460, -1.533600742197721134, 5.000000000000000000 ) ) ;
#19411 = CARTESIAN_POINT ( 'NONE',  ( 17.51078643762690845, -27.52281430457043143, 5.000000000000000000 ) ) ;
#19412 = CIRCLE ( 'NONE', #63439, 5.968999999999998529 ) ;
#19413 = DIRECTION ( 'NONE',  ( 0.6830127018922181881, 0.6830127018922202975, -0.2588190451025214056 ) ) ;
#19414 = DIRECTION ( 'NONE',  ( -0.000000000000000000, 0.000000000000000000, 1.000000000000000000 ) ) ;
#19415 = EDGE_CURVE ( 'NONE', #36287, #6138, #46906, .T. ) ;
#19416 = DIRECTION ( 'NONE',  ( -1.000000000000000000, 0.000000000000000000, 0.000000000000000000 ) ) ;
#19417 = AXIS2_PLACEMENT_3D ( 'NONE', #108876, #8143, #85014 ) ;
#19418 = CARTESIAN_POINT ( 'NONE',  ( 30.77126352523143638, 4.472830434245839371, 4.472830434245842035 ) ) ;
#19419 = LINE ( 'NONE', #107831, #129691 ) ;
#19420 = DIRECTION ( 'NONE',  ( 0.7071067811865487940, 0.7071067811865463515, 0.000000000000000000 ) ) ;
#19421 = ORIENTED_EDGE ( 'NONE', *, *, #31210, .T. ) ;
#19422 = DIRECTION ( 'NONE',  ( 0.7071067811865487940, -0.7071067811865463515, 0.000000000000000000 ) ) ;
#19423 = EDGE_CURVE ( 'NONE', #101030, #47360, #57038, .T. ) ;
#19424 = DIRECTION ( 'NONE',  ( -1.000000000000000000, -0.000000000000000000, -0.000000000000000000 ) ) ;
#19425 = ORIENTED_EDGE ( 'NONE', *, *, #69245, .F. ) ;
#19426 = VECTOR ( 'NONE', #87177, 1000.000000000000227 ) ;
#19427 = CARTESIAN_POINT ( 'NONE',  ( -25.49999999999982236, 21.05218569542895324, 5.000000000000000000 ) ) ;
#19429 = EDGE_LOOP ( 'NONE', ( #46429, #139600, #23133, #116669 ) ) ;
#19428 = CARTESIAN_POINT ( 'NONE',  ( 53.19685992802465080, -48.66302742222551103, -38.53170190052302502 ) ) ;
#19430 = VECTOR ( 'NONE', #142273, 1000.000000000000000 ) ;
#19431 = CARTESIAN_POINT ( 'NONE',  ( -41.99451991528749062, 28.92564299267967343, 4.000000000000000000 ) ) ;
#19432 = ORIENTED_EDGE ( 'NONE', *, *, #96006, .T. ) ;
#19433 = DIRECTION ( 'NONE',  ( -1.000000000000000000, -3.115803279706882722E-16, 0.000000000000000000 ) ) ;
#19434 = EDGE_CURVE ( 'NONE', #72893, #51489, #134589, .T. ) ;
#19435 = EDGE_LOOP ( 'NONE', ( #86358, #47182, #125691, #122329 ) ) ;
#19436 = LINE ( 'NONE', #32470, #109115 ) ;
#19437 = EDGE_LOOP ( 'NONE', ( #31008, #130510, #1563, #135251 ) ) ;
#19438 = AXIS2_PLACEMENT_3D ( 'NONE', #131163, #33327, #31855 ) ;
#19439 = CARTESIAN_POINT ( 'NONE',  ( -12.70000000000000462, -22.26999999999999247, -39.79289321881346098 ) ) ;
#19440 = CARTESIAN_POINT ( 'NONE',  ( 118.9333603837962414, 2.130196079827431532, -7.949999999999997513 ) ) ;
#19442 = VECTOR ( 'NONE', #49194, 1000.000000000000114 ) ;
#19441 = CARTESIAN_POINT ( 'NONE',  ( 9.183988606268997046, 28.73617430169793607, 5.000000000000000000 ) ) ;
#19443 = PLANE ( 'NONE',  #28265 ) ;
#19445 = EDGE_CURVE ( 'NONE', #35802, #138104, #101211, .T. ) ;
#19444 = CARTESIAN_POINT ( 'NONE',  ( -25.49999999999981526, -7.912538124160678699, 4.000000000000000000 ) ) ;
#19446 = CARTESIAN_POINT ( 'NONE',  ( -32.20666063542130075, 21.75929247661549226, 4.998822639870715179 ) ) ;
#19447 = CARTESIAN_POINT ( 'NONE',  ( 1.458333333333333481, -3.047499999999997211, -5.278424836066143655 ) ) ;
#19448 = CARTESIAN_POINT ( 'NONE',  ( 16.89540314143521726, 2.126176841940962348, 7.934999999999988951 ) ) ;
#19449 = VECTOR ( 'NONE', #81704, 999.9999999999998863 ) ;
#19450 = DIRECTION ( 'NONE',  ( 0.000000000000000000, -1.000000000000000000, 0.000000000000000000 ) ) ;
#19451 = LINE ( 'NONE', #18712, #73279 ) ;
#19452 = ORIENTED_EDGE ( 'NONE', *, *, #69830, .F. ) ;
#19454 = EDGE_LOOP ( 'NONE', ( #57262, #47431, #73900, #45831 ) ) ;
#19453 = ADVANCED_FACE ( 'NONE', ( #113507 ), #459, .T. ) ;
#19455 = EDGE_CURVE ( 'NONE', #96026, #111517, #58491, .T. ) ;
#19456 = VECTOR ( 'NONE', #23463, 999.9999999999998863 ) ;
#19457 = CARTESIAN_POINT ( 'NONE',  ( 5.999999999999967137, 8.587461875839155212, 4.000000000000000000 ) ) ;
#19458 = VERTEX_POINT ( 'NONE', #78061 ) ;
#19459 = CARTESIAN_POINT ( 'NONE',  ( 3.489213562373097322, -27.52281430457057709, 5.000000000000000000 ) ) ;
#19460 = DIRECTION ( 'NONE',  ( 1.000000000000000000, -0.000000000000000000, 0.000000000000000000 ) ) ;
#19461 = LINE ( 'NONE', #7114, #122805 ) ;
#19462 = AXIS2_PLACEMENT_3D ( 'NONE', #110838, #89828, #123205 ) ;
#19463 = ORIENTED_EDGE ( 'NONE', *, *, #60595, .T. ) ;
#19464 = ADVANCED_FACE ( 'NONE', ( #12055 ), #103475, .F. ) ;
#19465 = CARTESIAN_POINT ( 'NONE',  ( -15.29974487139158867, -27.71228299555216879, 4.000000000000000000 ) ) ;
#19466 = CARTESIAN_POINT ( 'NONE',  ( 92.29166666666665719, 3.975000000000003642, -6.884901960086285300 ) ) ;
#19467 = CARTESIAN_POINT ( 'NONE',  ( -11.99999999999992362, -6.108550654416973202, -3.114665004254993708 ) ) ;
#19468 = EDGE_CURVE ( 'NONE', #2635, #75105, #90164, .T. ) ;
#19469 = EDGE_CURVE ( 'NONE', #30259, #109556, #77191, .T. ) ;
#19470 = CARTESIAN_POINT ( 'NONE',  ( 0.5457257104438434370, -52.10338527932237440, 40.45859298138252313 ) ) ;
#19472 = ORIENTED_EDGE ( 'NONE', *, *, #109533, .F. ) ;
#19471 = PLANE ( 'NONE',  #72951 ) ;
#19473 = CARTESIAN_POINT ( 'NONE',  ( 41.24999999999999289, -9.735942053221458872E-16, 7.950000000000000178 ) ) ;
#19474 = CARTESIAN_POINT ( 'NONE',  ( -32.99999999999975842, -13.39766691384885711, -10.96608748226458196 ) ) ;
#19475 = DIRECTION ( 'NONE',  ( 0.7071067811865486830, -0.7071067811865464625, -0.000000000000000000 ) ) ;
#19476 = LINE ( 'NONE', #119474, #93123 ) ;
#19477 = ORIENTED_EDGE ( 'NONE', *, *, #7015, .F. ) ;
#19478 = ORIENTED_EDGE ( 'NONE', *, *, #343, .T. ) ;
#19479 = ORIENTED_EDGE ( 'NONE', *, *, #100181, .T. ) ;
#19480 = CARTESIAN_POINT ( 'NONE',  ( 104.8545968585647756, -1.637169565754161615, 6.110000000000000320 ) ) ;
#19481 = AXIS2_PLACEMENT_3D ( 'NONE', #19034, #106734, #84328 ) ;
#19482 = VERTEX_POINT ( 'NONE', #2418 ) ;
#19483 = EDGE_CURVE ( 'NONE', #79735, #49213, #24907, .T. ) ;
#19484 = LINE ( 'NONE', #126803, #68607 ) ;
#19485 = ORIENTED_EDGE ( 'NONE', *, *, #60393, .F. ) ;
#19486 = EDGE_CURVE ( 'NONE', #96111, #5701, #109718, .T. ) ;
#19487 = CARTESIAN_POINT ( 'NONE',  ( 74.93749999999998579, 5.819803920172574863, -5.819803920172573086 ) ) ;
#19489 = COLOUR_RGB ( '', 0.31764706, 0.68627451, 0.89019608) ;
#19488 = LINE ( 'NONE', #110747, #11828 ) ;
#19490 = CARTESIAN_POINT ( 'NONE',  ( 91.93293019189812298, 1.637169565754156508, 6.110000000000000320 ) ) ;
#19491 = EDGE_LOOP ( 'NONE', ( #94928, #3413, #81208, #89970 ) ) ;
#19492 = CARTESIAN_POINT ( 'NONE',  ( 17.28242261357420517, -21.73023691814493219, 5.000000000000000888 ) ) ;
#19493 = CARTESIAN_POINT ( 'NONE',  ( 0.000000000000000000, 0.000000000000000000, 5.000000000000000000 ) ) ;
#19494 = DIRECTION ( 'NONE',  ( 0.7071067811865487940, 0.7071067811865463515, 0.000000000000000000 ) ) ;
#19495 = DIRECTION ( 'NONE',  ( 1.000000000000000000, 0.000000000000000000, 0.000000000000000000 ) ) ;
#19496 = ORIENTED_EDGE ( 'NONE', *, *, #82160, .T. ) ;
#19497 = EDGE_LOOP ( 'NONE', ( #110195, #73196, #97372, #135675 ) ) ;
#19498 = ORIENTED_EDGE ( 'NONE', *, *, #39453, .F. ) ;
#19499 = CARTESIAN_POINT ( 'NONE',  ( 14.99999999999989519, -7.447814304570745669, 5.000000000000000000 ) ) ;
#19500 = DIRECTION ( 'NONE',  ( 0.3543493200069162685, -0.000000000000000000, -0.9351131265310288487 ) ) ;
#19501 = CARTESIAN_POINT ( 'NONE',  ( 16.98373647476855197, -5.808823158059035485, -5.808823158059033709 ) ) ;
#19502 = VECTOR ( 'NONE', #17733, 1000.000000000000000 ) ;
#19503 = CARTESIAN_POINT ( 'NONE',  ( -77.99451991528749772, 28.92564299267992567, 4.000000000000000000 ) ) ;
#19504 = CARTESIAN_POINT ( 'NONE',  ( 7.139999999999994351, -35.14999999999999147, -39.79289321881344677 ) ) ;
#19505 = EDGE_CURVE ( 'NONE', #119204, #21635, #35834, .T. ) ;
#19507 = ADVANCED_FACE ( 'NONE', ( #1000 ), #101035, .F. ) ;
#19506 =( NAMED_UNIT ( * ) PLANE_ANGLE_UNIT ( ) SI_UNIT ( $, .RADIAN. ) );
#19508 = VECTOR ( 'NONE', #7492, 1000.000000000000227 ) ;
#19509 = VERTEX_POINT ( 'NONE', #77878 ) ;
#19510 = VERTEX_POINT ( 'NONE', #90912 ) ;
#19511 = VECTOR ( 'NONE', #20693, 1000.000000000000000 ) ;
#19512 = DIRECTION ( 'NONE',  ( 0.000000000000000000, 0.000000000000000000, 1.000000000000000000 ) ) ;
#19513 = ORIENTED_EDGE ( 'NONE', *, *, #77744, .F. ) ;
#19514 = ORIENTED_EDGE ( 'NONE', *, *, #59293, .T. ) ;
#19515 = EDGE_CURVE ( 'NONE', #8278, #81137, #45982, .T. ) ;
#19516 = PLANE ( 'NONE',  #83612 ) ;
#19517 = CARTESIAN_POINT ( 'NONE',  ( 56.99451991528749062, 28.92564299267978001, 4.000000000000000000 ) ) ;
#19518 = ORIENTED_EDGE ( 'NONE', *, *, #133090, .F. ) ;
#19519 =( GEOMETRIC_REPRESENTATION_CONTEXT ( 3 ) GLOBAL_UNCERTAINTY_ASSIGNED_CONTEXT ( ( #93804 ) ) GLOBAL_UNIT_ASSIGNED_CONTEXT ( ( #39029, #17272, #7802 ) ) REPRESENTATION_CONTEXT ( 'NONE', 'WORKASPACE' ) );
#19520 = CARTESIAN_POINT ( 'NONE',  ( 55.83333333333332860, -6.884901960086287964, 3.974999999999998312 ) ) ;
#19521 = CARTESIAN_POINT ( 'NONE',  ( -39.29974487139159578, -27.71228299555233576, 4.000000000000000000 ) ) ;
#19522 = DIRECTION ( 'NONE',  ( 0.000000000000000000, 0.000000000000000000, 1.000000000000000000 ) ) ;
#19523 =( BOUNDED_CURVE ( )  B_SPLINE_CURVE ( 3, ( #32333, #97566, #64243, #1093 ),
 .UNSPECIFIED., .F., .T. ) 
 B_SPLINE_CURVE_WITH_KNOTS ( ( 4, 4 ),
 ( 1.208578181583239486, 1.359146454359483336 ),
 .UNSPECIFIED. ) 
 CURVE ( )  GEOMETRIC_REPRESENTATION_ITEM ( )  RATIONAL_B_SPLINE_CURVE ( ( 1.000000000000000000, 0.9981116584018941973, 0.9981116584018941973, 1.000000000000000000 ) ) 
 REPRESENTATION_ITEM ( '' )  );
#19524 = DIRECTION ( 'NONE',  ( -0.7071067811865486830, -0.7071067811865464625, -0.000000000000000000 ) ) ;
#19525 = VERTEX_POINT ( 'NONE', #32975 ) ;
#19526 = CYLINDRICAL_SURFACE ( 'NONE', #88124, 6.094999999999989093 ) ;
#19527 = CARTESIAN_POINT ( 'NONE',  ( -8.218373117075001844, 21.74787736706806385, 4.999607392498049308 ) ) ;
#19529 = ORIENTED_EDGE ( 'NONE', *, *, #58261, .F. ) ;
#19528 = AXIS2_PLACEMENT_3D ( 'NONE', #139253, #108694, #51520 ) ;
#19530 = CARTESIAN_POINT ( 'NONE',  ( 25.40000000000002345, 4.163866272544239244, -6.757773473734751235 ) ) ;
#19531 = LINE ( 'NONE', #42018, #11009 ) ;
#19532 = VERTEX_POINT ( 'NONE', #123552 ) ;
#19533 = VERTEX_POINT ( 'NONE', #57573 ) ;
#19534 = LINE ( 'NONE', #85487, #117593 ) ;
#19535 = ORIENTED_EDGE ( 'NONE', *, *, #113801, .F. ) ;
#19536 = EDGE_LOOP ( 'NONE', ( #122, #77542, #92761, #82854 ) ) ;
#19537 = ORIENTED_EDGE ( 'NONE', *, *, #43585, .T. ) ;
#19538 = VECTOR ( 'NONE', #37042, 1000.000000000000000 ) ;
#19539 = CARTESIAN_POINT ( 'NONE',  ( 31.84959685856478373, 6.109999999999996767, 1.637169565754163836 ) ) ;
#19540 = AXIS2_PLACEMENT_3D ( 'NONE', #6316, #10461, #117245 ) ;
#19541 = VECTOR ( 'NONE', #78270, 1000.000000000000000 ) ;
#19542 = DIRECTION ( 'NONE',  ( 0.7071067811865487940, 0.7071067811865463515, 0.000000000000000000 ) ) ;
#19543 = DIRECTION ( 'NONE',  ( -0.000000000000000000, 0.3543493200069153248, 0.9351131265310292928 ) ) ;
#19544 = CARTESIAN_POINT ( 'NONE',  ( 24.43680103220814104, -12.74070752338415780, 9.898150129686316134 ) ) ;
#19545 = ADVANCED_FACE ( 'NONE', ( #24215 ), #68461, .F. ) ;
#19546 = DIRECTION ( 'NONE',  ( -0.3543493200069162685, -0.000000000000000000, -0.9351131265310288487 ) ) ;
#19547 = PLANE ( 'NONE',  #53921 ) ;
#19548 = AXIS2_PLACEMENT_3D ( 'NONE', #82322, #92435, #117748 ) ;
#19549 = CARTESIAN_POINT ( 'NONE',  ( 21.78162688292479743, 21.74787736706806029, 4.999607392498049308 ) ) ;
#19550 = LINE ( 'NONE', #63796, #25207 ) ;
#19551 = FACE_OUTER_BOUND ( 'NONE', #125075, .T. ) ;
#19552 = VERTEX_POINT ( 'NONE', #47441 ) ;
#19553 = VERTEX_POINT ( 'NONE', #124229 ) ;
#19554 = VERTEX_POINT ( 'NONE', #69155 ) ;
#19555 = ORIENTED_EDGE ( 'NONE', *, *, #111827, .T. ) ;
#19556 = LINE ( 'NONE', #63802, #42556 ) ;
#19557 = ORIENTED_EDGE ( 'NONE', *, *, #36160, .F. ) ;
#19559 = VERTEX_POINT ( 'NONE', #60433 ) ;
#19558 = EDGE_CURVE ( 'NONE', #21017, #43833, #58320, .T. ) ;
#19560 = DIRECTION ( 'NONE',  ( 1.000000000000000000, 0.000000000000000000, 0.000000000000000000 ) ) ;
#19561 = FACE_OUTER_BOUND ( 'NONE', #10584, .T. ) ;
#19562 = ADVANCED_FACE ( 'NONE', ( #27766 ), #25618, .T. ) ;
#19563 = EDGE_CURVE ( 'NONE', #8278, #80300, #19243, .T. ) ;
#19564 = FACE_OUTER_BOUND ( 'NONE', #108313, .T. ) ;
#19565 = VERTEX_POINT ( 'NONE', #28503 ) ;
#19566 = VERTEX_POINT ( 'NONE', #124936 ) ;
#19568 = EDGE_CURVE ( 'NONE', #106128, #81473, #15425, .T. ) ;
#19567 = CARTESIAN_POINT ( 'NONE',  ( -24.48921356237309510, -27.52281430457072631, 5.000000000000000000 ) ) ;
#19569 = ADVANCED_FACE ( 'NONE', ( #116210 ), #103873, .T. ) ;
#19570 = CARTESIAN_POINT ( 'NONE',  ( 0.000000000000000000, 0.000000000000000000, 5.000000000000000000 ) ) ;
#19571 = CARTESIAN_POINT ( 'NONE',  ( 11.58790314143521982, 6.871911579029515771, 3.967499999999989146 ) ) ;
#19572 = ORIENTED_EDGE ( 'NONE', *, *, #18793, .T. ) ;
#19573 = CARTESIAN_POINT ( 'NONE',  ( 93.24543019189812298, -5.291415217122919401, -3.055000000000000604 ) ) ;
#19574 =( NAMED_UNIT ( * ) PLANE_ANGLE_UNIT ( ) SI_UNIT ( $, .RADIAN. ) );
#19575 = EDGE_CURVE ( 'NONE', #12595, #139718, #49562, .T. ) ;
#19576 = LINE ( 'NONE', #63819, #48696 ) ;
#19577 = PLANE ( 'NONE',  #58146 ) ;
#19578 = EDGE_LOOP ( 'NONE', ( #82400, #124647, #132086, #88529 ) ) ;
#19579 = ORIENTED_EDGE ( 'NONE', *, *, #61115, .F. ) ;
#19580 = LINE ( 'NONE', #57777, #82084 ) ;
#19581 = ORIENTED_EDGE ( 'NONE', *, *, #55538, .F. ) ;
#19582 = CARTESIAN_POINT ( 'NONE',  ( 33.70701326429281153, -21.74070752338406365, 4.999753212805220670 ) ) ;
#19583 = CARTESIAN_POINT ( 'NONE',  ( 29.99451991528749417, 28.92564299267958816, 4.000000000000000000 ) ) ;
#19584 = CARTESIAN_POINT ( 'NONE',  ( -30.48921356237309510, -27.52281430457076894, 5.000000000000000000 ) ) ;
#19585 = DIRECTION ( 'NONE',  ( 0.6830127018922180770, -0.6830127018922204085, -0.2588190451025213501 ) ) ;
#19587 = ORIENTED_EDGE ( 'NONE', *, *, #105580, .F. ) ;
#19586 = AXIS2_PLACEMENT_3D ( 'NONE', #59350, #135472, #4146 ) ;
#19588 = FACE_OUTER_BOUND ( 'NONE', #140426, .T. ) ;
#19589 = ADVANCED_FACE ( 'NONE', ( #94443 ), #82191, .F. ) ;
#19590 = PLANE ( 'NONE',  #102213 ) ;
#19591 = CARTESIAN_POINT ( 'NONE',  ( -20.99999999999985079, -9.412538124160658271, 4.000000000000000000 ) ) ;
#19592 = ORIENTED_EDGE ( 'NONE', *, *, #60935, .F. ) ;
#19593 = CARTESIAN_POINT ( 'NONE',  ( 3.489213562373097322, -27.52281430457057709, 5.000000000000000000 ) ) ;
#19594 = EDGE_CURVE ( 'NONE', #18836, #47983, #16901, .T. ) ;
#19595 = DIRECTION ( 'NONE',  ( -1.000000000000000000, 0.000000000000000000, 0.000000000000000000 ) ) ;
#19596 = ORIENTED_EDGE ( 'NONE', *, *, #81058, .F. ) ;
#19598 = ORIENTED_EDGE ( 'NONE', *, *, #22169, .T. ) ;
#19597 = CARTESIAN_POINT ( 'NONE',  ( 3.681769877398668738E-15, -50.24077216217759911, -35.40405119785167898 ) ) ;
#19599 = EDGE_LOOP ( 'NONE', ( #50422, #137937, #4573 ) ) ;
#19600 = FACE_OUTER_BOUND ( 'NONE', #47956, .T. ) ;
#19601 = CARTESIAN_POINT ( 'NONE',  ( -10.49999999999992539, 12.05218569542904561, 5.000000000000000000 ) ) ;
#19603 = EDGE_CURVE ( 'NONE', #17066, #44633, #50254, .T. ) ;
#19602 = CIRCLE ( 'NONE', #38149, 1.898649999999994842 ) ;
#19604 = VERTEX_POINT ( 'NONE', #39382 ) ;
#19605 = PLANE ( 'NONE',  #220 ) ;
#19606 = DIRECTION ( 'NONE',  ( 0.3543493200069162685, -0.000000000000000000, -0.9351131265310288487 ) ) ;
#19607 = VECTOR ( 'NONE', #87049, 1000.000000000000000 ) ;
#19608 = CARTESIAN_POINT ( 'NONE',  ( -27.46160355370554029, -9.740707523384173783, 17.74957260769604517 ) ) ;
#19609 = LINE ( 'NONE', #63857, #90120 ) ;
#19611 = CARTESIAN_POINT ( 'NONE',  ( 0.1600000000000015299, -4.429882875875668091, -6.591932758761664957 ) ) ;
#19610 = CIRCLE ( 'NONE', #61280, 2.500000000000000888 ) ;
#19612 = CARTESIAN_POINT ( 'NONE',  ( 36.48921356237310221, -27.52281430457080802, 5.000000000000000000 ) ) ;
#19614 = EDGE_CURVE ( 'NONE', #82511, #11616, #83608, .T. ) ;
#19613 = CARTESIAN_POINT ( 'NONE',  ( 23.20710678118638626, 12.75929247661558996, 5.000000000000000000 ) ) ;
#19615 = DIRECTION ( 'NONE',  ( 0.6830127018922180770, -0.6830127018922204085, -0.2588190451025213501 ) ) ;
#19616 = CARTESIAN_POINT ( 'NONE',  ( 8.277185695429338352, -21.72500000000000142, 5.000000000000000000 ) ) ;
#19617 = DIRECTION ( 'NONE',  ( -0.7071067811865486830, -0.7071067811865464625, 0.000000000000000000 ) ) ;
#19618 = LINE ( 'NONE', #66017, #129335 ) ;
#19619 = DIRECTION ( 'NONE',  ( 1.000000000000000000, 1.224606353822377258E-16, 0.000000000000000000 ) ) ;
#19620 = CARTESIAN_POINT ( 'NONE',  ( 28.49999999999980460, -9.462702396500981550, -9.474982329943578918 ) ) ;
#19621 = VERTEX_POINT ( 'NONE', #116917 ) ;
#19622 = ORIENTED_EDGE ( 'NONE', *, *, #117102, .F. ) ;
#19623 = ORIENTED_EDGE ( 'NONE', *, *, #92384, .F. ) ;
#19624 = EDGE_CURVE ( 'NONE', #61647, #36536, #126361, .T. ) ;
#19625 = CARTESIAN_POINT ( 'NONE',  ( 111.2500000000000000, -9.735942053221458872E-16, 7.950000000000000178 ) ) ;
#19626 = ORIENTED_EDGE ( 'NONE', *, *, #30400, .T. ) ;
#19627 = VECTOR ( 'NONE', #106960, 1000.000000000000000 ) ;
#19628 = VERTEX_POINT ( 'NONE', #3825 ) ;
#19629 = EDGE_CURVE ( 'NONE', #136190, #51950, #17585, .T. ) ;
#19630 = ORIENTED_EDGE ( 'NONE', *, *, #66567, .F. ) ;
#19631 = CARTESIAN_POINT ( 'NONE',  ( -34.92500000000001137, -22.22500000000000142, 4.500000000000000888 ) ) ;
#19632 = CARTESIAN_POINT ( 'NONE',  ( -26.29289321881326913, 8.259292476615634371, 5.000000000000000000 ) ) ;
#19633 = ORIENTED_EDGE ( 'NONE', *, *, #58918, .F. ) ;
#19634 = DIRECTION ( 'NONE',  ( -0.7071067811865486830, -0.7071067811865464625, -0.000000000000000000 ) ) ;
#19635 = EDGE_CURVE ( 'NONE', #89978, #105099, #136518, .T. ) ;
#19636 = DIRECTION ( 'NONE',  ( 0.6830127018922180770, -0.6830127018922204085, -0.2588190451025213501 ) ) ;
#19637 = LINE ( 'NONE', #110901, #16272 ) ;
#19638 = CARTESIAN_POINT ( 'NONE',  ( 27.48921356237309155, -27.52281430457074762, 5.000000000000000000 ) ) ;
#19639 = CARTESIAN_POINT ( 'NONE',  ( 107.6254301918981042, 5.291415217122919401, 3.055000000000002824 ) ) ;
#19640 = ORIENTED_EDGE ( 'NONE', *, *, #64624, .F. ) ;
#19641 = CARTESIAN_POINT ( 'NONE',  ( 0.7928932188134563130, -11.24070752338416668, 5.000000000000000000 ) ) ;
#19642 = LINE ( 'NONE', #40009, #72864 ) ;
#19643 = DIRECTION ( 'NONE',  ( 0.7071067811865486830, -0.7071067811865464625, -0.000000000000000000 ) ) ;
#19644 = CARTESIAN_POINT ( 'NONE',  ( 13.49999999999991296, 12.05218569542904561, 5.000000000000000000 ) ) ;
#19645 = CARTESIAN_POINT ( 'NONE',  ( -2.994519915287485734, 28.92564299267940342, 4.000000000000000000 ) ) ;
#19646 = LINE ( 'NONE', #141434, #89291 ) ;
#19647 = AXIS2_PLACEMENT_3D ( 'NONE', #110549, #133766, #22123 ) ;
#19648 = CARTESIAN_POINT ( 'NONE',  ( -27.48921356237309155, -27.52281430457074762, 5.000000000000000000 ) ) ;
#19649 = VECTOR ( 'NONE', #23301, 1000.000000000000227 ) ;
#19650 = EDGE_LOOP ( 'NONE', ( #97032, #111590, #37336, #27979 ) ) ;
#19651 = VERTEX_POINT ( 'NONE', #6683 ) ;
#19652 = VECTOR ( 'NONE', #136882, 1000.000000000000227 ) ;
#19653 = CARTESIAN_POINT ( 'NONE',  ( 28.27083333333333215, -7.949999999999999289, -2.130196079827426203 ) ) ;
#19654 = ORIENTED_EDGE ( 'NONE', *, *, #44570, .T. ) ;
#19655 = VECTOR ( 'NONE', #55025, 1000.000000000000000 ) ;
#19656 = ADVANCED_FACE ( 'NONE', ( #91603 ), #104614, .F. ) ;
#19657 = CARTESIAN_POINT ( 'NONE',  ( 19.89359858452208130, 4.202752102959690472E-16, 0.000000000000000000 ) ) ;
#19658 = LINE ( 'NONE', #121804, #66378 ) ;
#19659 = CARTESIAN_POINT ( 'NONE',  ( 34.75611968250419181, -19.29434930147575500, 4.955485411084881164 ) ) ;
#19660 = EDGE_CURVE ( 'NONE', #128218, #26178, #71298, .T. ) ;
#19661 = CARTESIAN_POINT ( 'NONE',  ( 14.81601139373099585, 28.73617430169776910, 5.000000000000000000 ) ) ;
#19662 =( LENGTH_UNIT ( ) NAMED_UNIT ( * ) SI_UNIT ( .MILLI., .METRE. ) );
#19663 = CARTESIAN_POINT ( 'NONE',  ( 127.5162635252314516, -4.472830434245839371, 4.472830434245839371 ) ) ;
#19664 = ORIENTED_EDGE ( 'NONE', *, *, #120721, .F. ) ;
#19665 = CARTESIAN_POINT ( 'NONE',  ( 19.10840764549667270, 3.061616997868380183E-16, -2.500000000000001332 ) ) ;
#19666 = ORIENTED_EDGE ( 'NONE', *, *, #8166, .F. ) ;
#19667 = CARTESIAN_POINT ( 'NONE',  ( 70.95419371712955581, 6.884901960086283523, 3.975000000000002753 ) ) ;
#19668 =( NAMED_UNIT ( * ) PLANE_ANGLE_UNIT ( ) SI_UNIT ( $, .RADIAN. ) );
#19669 = LINE ( 'NONE', #9477, #90735 ) ;
#19670 = VERTEX_POINT ( 'NONE', #125673 ) ;
#19671 = EDGE_CURVE ( 'NONE', #63574, #52633, #81472, .T. ) ;
#19672 = CARTESIAN_POINT ( 'NONE',  ( 44.47959685856476852, 6.109999999999999432, 1.637169565754164280 ) ) ;
#19673 = ORIENTED_EDGE ( 'NONE', *, *, #83909, .F. ) ;
#19674 = DIRECTION ( 'NONE',  ( -0.7071067811865487940, 0.7071067811865463515, -0.000000000000000000 ) ) ;
#19675 = LINE ( 'NONE', #53761, #110996 ) ;
#19676 = PLANE ( 'NONE',  #61787 ) ;
#19677 = DIRECTION ( 'NONE',  ( -0.000000000000000000, 1.000000000000000000, -0.000000000000000000 ) ) ;
#19678 = ADVANCED_FACE ( 'NONE', ( #127075 ), #7421, .F. ) ;
#19679 = CARTESIAN_POINT ( 'NONE',  ( 37.09959685856476597, -6.109999999999997655, -1.637169565754160283 ) ) ;
#19680 = ORIENTED_EDGE ( 'NONE', *, *, #47251, .T. ) ;
#19681 = DIRECTION ( 'NONE',  ( -0.7071067811865487940, 0.7071067811865463515, -0.000000000000000000 ) ) ;
#19682 = VERTEX_POINT ( 'NONE', #107465 ) ;
#19683 = ORIENTED_EDGE ( 'NONE', *, *, #14347, .F. ) ;
#19684 = ORIENTED_EDGE ( 'NONE', *, *, #27489, .T. ) ;
#19685 = EDGE_CURVE ( 'NONE', #45742, #130861, #76841, .T. ) ;
#19686 = EDGE_CURVE ( 'NONE', #117528, #121710, #22391, .T. ) ;
#19687 = CARTESIAN_POINT ( 'NONE',  ( -42.48921356237308800, -27.52281430457085065, 5.000000000000000000 ) ) ;
#19688 = ORIENTED_EDGE ( 'NONE', *, *, #100798, .T. ) ;
#19689 = CARTESIAN_POINT ( 'NONE',  ( -12.29974487139158512, -27.71228299555214747, 4.000000000000000000 ) ) ;
#19690 = LINE ( 'NONE', #28454, #31705 ) ;
#19691 = CYLINDRICAL_SURFACE ( 'NONE', #124663, 0.5000000000000004441 ) ;
#19692 = DIRECTION ( 'NONE',  ( -1.000000000000000000, -0.000000000000000000, -0.000000000000000000 ) ) ;
#19693 = FACE_BOUND ( 'NONE', #99059, .T. ) ;
#19695 = ADVANCED_FACE ( 'NONE', ( #29896 ), #23100, .T. ) ;
#19694 = EDGE_LOOP ( 'NONE', ( #101159, #65643, #90517, #16740 ) ) ;
#19696 = CARTESIAN_POINT ( 'NONE',  ( -15.48921356237309510, -27.52281430457066236, 5.000000000000000000 ) ) ;
#19697 = LINE ( 'NONE', #42197, #18979 ) ;
#19698 = DIRECTION ( 'NONE',  ( -0.000000000000000000, 0.3543493200069153248, 0.9351131265310292928 ) ) ;
#19699 = ORIENTED_EDGE ( 'NONE', *, *, #11688, .T. ) ;
#19700 = SURFACE_SIDE_STYLE ('',( #8089 ) ) ;
#19701 = ORIENTED_EDGE ( 'NONE', *, *, #82221, .T. ) ;
#19702 = ORIENTED_EDGE ( 'NONE', *, *, #77580, .T. ) ;
#19703 = LINE ( 'NONE', #86417, #40240 ) ;
#19704 =( BOUNDED_CURVE ( )  B_SPLINE_CURVE ( 3, ( #132698, #110864, #143527, #121052 ),
 .UNSPECIFIED., .F., .T. ) 
 B_SPLINE_CURVE_WITH_KNOTS ( ( 4, 4 ),
 ( 1.964434688349486313, 3.503810798801452187 ),
 .UNSPECIFIED. ) 
 CURVE ( )  GEOMETRIC_REPRESENTATION_ITEM ( )  RATIONAL_B_SPLINE_CURVE ( ( 1.000000000000000000, 0.8120851936182275077, 0.8120851936182275077, 1.000000000000000000 ) ) 
 REPRESENTATION_ITEM ( '' )  );
#19705 = VERTEX_POINT ( 'NONE', #128526 ) ;
#19706 = VECTOR ( 'NONE', #84054, 1000.000000000000227 ) ;
#19707 = CARTESIAN_POINT ( 'NONE',  ( 61.30793019189810877, -6.109999999999998543, 1.637169565754158507 ) ) ;
#19708 = ORIENTED_EDGE ( 'NONE', *, *, #20399, .T. ) ;
#19709 = CARTESIAN_POINT ( 'NONE',  ( 22.49999999999984368, -12.66682484999664204, -0.6294897503863420285 ) ) ;
#19710 = DIRECTION ( 'NONE',  ( 0.000000000000000000, -1.000000000000000000, 0.000000000000000000 ) ) ;
#19711 = ORIENTED_EDGE ( 'NONE', *, *, #11241, .F. ) ;
#19712 = SURFACE_SIDE_STYLE ('',( #39358 ) ) ;
#19713 = CARTESIAN_POINT ( 'NONE',  ( 28.49999999999980460, -1.592773361805344789, -6.492772025301293937 ) ) ;
#19714 = DIRECTION ( 'NONE',  ( 0.7071067811865487940, 0.7071067811865463515, 0.000000000000000000 ) ) ;
#19715 = VECTOR ( 'NONE', #4209, 1000.000000000000000 ) ;
#19716 = PLANE ( 'NONE',  #101450 ) ;
#19717 = DIRECTION ( 'NONE',  ( 0.000000000000000000, 1.000000000000000000, 0.000000000000000000 ) ) ;
#19718 = LINE ( 'NONE', #54524, #44699 ) ;
#19719 = CARTESIAN_POINT ( 'NONE',  ( -1.499999999999990896, 11.52377502935403264, -1.522421517564079618 ) ) ;
#19720 = EDGE_LOOP ( 'NONE', ( #66178, #120470, #96565, #114117 ) ) ;
#19721 = EDGE_CURVE ( 'NONE', #66027, #114208, #110823, .T. ) ;
#19722 = EDGE_LOOP ( 'NONE', ( #90445, #128985, #23300, #46375 ) ) ;
#19723 = CARTESIAN_POINT ( 'NONE',  ( -27.77004279457773706, 21.73644205237998506, 5.000000000000000888 ) ) ;
#19724 = CARTESIAN_POINT ( 'NONE',  ( 184.1499999999998067, -3.180000000000061444, -31.92499999999998295 ) ) ;
#19725 = ORIENTED_EDGE ( 'NONE', *, *, #26345, .F. ) ;
#19726 = VERTEX_POINT ( 'NONE', #132658 ) ;
#19727 = ORIENTED_EDGE ( 'NONE', *, *, #61124, .F. ) ;
#19728 = FACE_OUTER_BOUND ( 'NONE', #7781, .T. ) ;
#19729 = DIRECTION ( 'NONE',  ( -1.000000000000000000, 0.000000000000000000, -0.000000000000000000 ) ) ;
#19731 = ADVANCED_FACE ( 'NONE', ( #99994 ), #10802, .F. ) ;
#19730 = ADVANCED_FACE ( 'NONE', ( #29191 ), #74138, .F. ) ;
#19732 = EDGE_CURVE ( 'NONE', #50892, #68263, #96556, .T. ) ;
#19733 = LINE ( 'NONE', #129939, #124954 ) ;
#19734 = ORIENTED_EDGE ( 'NONE', *, *, #60095, .F. ) ;
#19735 = LINE ( 'NONE', #108146, #87986 ) ;
#19736 = VECTOR ( 'NONE', #91191, 999.9999999999998863 ) ;
#19738 = EDGE_CURVE ( 'NONE', #44264, #21906, #128262, .T. ) ;
#19737 = DIRECTION ( 'NONE',  ( -0.3543493200069162685, -0.000000000000000000, -0.9351131265310288487 ) ) ;
#19739 = EDGE_CURVE ( 'NONE', #37058, #18032, #95875, .T. ) ;
#19740 = AXIS2_PLACEMENT_3D ( 'NONE', #140972, #7599, #51863 ) ;
#19741 = CARTESIAN_POINT ( 'NONE',  ( 13.77540314143521982, -2.126176841940958351, -7.934999999999989839 ) ) ;
#19742 = VECTOR ( 'NONE', #26440, 999.9999999999998863 ) ;
#19743 = EDGE_CURVE ( 'NONE', #133539, #100573, #77548, .T. ) ;
#19744 = EDGE_LOOP ( 'NONE', ( #13574, #46399, #79150, #27519 ) ) ;
#19745 = CARTESIAN_POINT ( 'NONE',  ( 121.8287635252314516, 0.000000000000000000, -6.109999999999999432 ) ) ;
#19746 = VECTOR ( 'NONE', #81834, 1000.000000000000227 ) ;
#19747 = EDGE_CURVE ( 'NONE', #59289, #96641, #67383, .T. ) ;
#19748 = CARTESIAN_POINT ( 'NONE',  ( 14.29289321881335795, 17.25929247661554911, 5.000000000000000000 ) ) ;
#19749 = CARTESIAN_POINT ( 'NONE',  ( -13.49999999999990763, -4.216083040037257312, -7.486842126848625156 ) ) ;
#19751 = ORIENTED_EDGE ( 'NONE', *, *, #83638, .F. ) ;
#19750 = CARTESIAN_POINT ( 'NONE',  ( 75.18398860626899705, 28.73617430169839793, 5.000000000000000000 ) ) ;
#19752 = FACE_OUTER_BOUND ( 'NONE', #15177, .T. ) ;
#19753 = VERTEX_POINT ( 'NONE', #88416 ) ;
#19754 = EDGE_CURVE ( 'NONE', #15438, #99234, #85701, .T. ) ;
#19755 = CARTESIAN_POINT ( 'NONE',  ( 0.6549448374538157092, 5.259292476615669010, 12.77922209995893965 ) ) ;
#19756 = CARTESIAN_POINT ( 'NONE',  ( 152.4000000000000057, -16.48000000000005016, 34.92499999999998295 ) ) ;
#19757 = LINE ( 'NONE', #19047, #98183 ) ;
#19758 = VERTEX_POINT ( 'NONE', #95157 ) ;
#19759 = EDGE_CURVE ( 'NONE', #142885, #91787, #11510, .T. ) ;
#19760 = DIRECTION ( 'NONE',  ( 0.000000000000000000, -1.000000000000000000, 0.000000000000000000 ) ) ;
#19761 = CARTESIAN_POINT ( 'NONE',  ( -23.58838509405152806, 22.22500000000000142, 4.777194822843820354 ) ) ;
#19762 = ORIENTED_EDGE ( 'NONE', *, *, #140990, .T. ) ;
#19763 = LINE ( 'NONE', #66153, #27698 ) ;
#19764 = EDGE_LOOP ( 'NONE', ( #6918, #97120, #36535, #70855 ) ) ;
#19765 = EDGE_CURVE ( 'NONE', #90132, #47491, #18285, .T. ) ;
#19766 = CARTESIAN_POINT ( 'NONE',  ( 11.62000000000000099, -2.055000000000000160, 2.789133085058098087E-16 ) ) ;
#19767 = CARTESIAN_POINT ( 'NONE',  ( 25.39999999999999858, -7.600000000000055600, -28.92499999999998650 ) ) ;
#19768 = ORIENTED_EDGE ( 'NONE', *, *, #52172, .T. ) ;
#19769 = VERTEX_POINT ( 'NONE', #40800 ) ;
#19770 = LINE ( 'NONE', #75601, #47334 ) ;
#19771 = CARTESIAN_POINT ( 'NONE',  ( 25.00000000000000000, 1.749999999999999778, 0.000000000000000000 ) ) ;
#19772 = EDGE_CURVE ( 'NONE', #77649, #94584, #32607, .T. ) ;
#19773 = CARTESIAN_POINT ( 'NONE',  ( 13.83290314143522082, -3.967499999999994476, 6.871911579029513106 ) ) ;
#19774 = CARTESIAN_POINT ( 'NONE',  ( -33.72281430457037743, -21.72499999999999432, 5.000000000000000000 ) ) ;
#19775 = CARTESIAN_POINT ( 'NONE',  ( -57.48921356237308800, -27.52281430457095368, 5.000000000000000000 ) ) ;
#19776 = DIRECTION ( 'NONE',  ( -0.000000000000000000, -0.3543493200069152693, 0.9351131265310292928 ) ) ;
#19777 = ORIENTED_EDGE ( 'NONE', *, *, #26301, .F. ) ;
#19778 = DIRECTION ( 'NONE',  ( 0.000000000000000000, -1.000000000000000000, 0.000000000000000000 ) ) ;
#19779 = CARTESIAN_POINT ( 'NONE',  ( -60.48921356237309510, -27.52281430457097500, 5.000000000000000000 ) ) ;
#19780 = DIRECTION ( 'NONE',  ( 0.7071067811865486830, -0.7071067811865464625, -0.000000000000000000 ) ) ;
#19781 = CARTESIAN_POINT ( 'NONE',  ( 126.7258888818563776, -5.807073093359954363, -3.403349999535261627 ) ) ;
#19782 = CARTESIAN_POINT ( 'NONE',  ( 37.24543019189811588, -5.291415217122919401, -3.055000000000000604 ) ) ;
#19783 = PLANE ( 'NONE',  #81139 ) ;
#19784 = EDGE_LOOP ( 'NONE', ( #54390, #136319, #10554, #86439 ) ) ;
#19785 = EDGE_CURVE ( 'NONE', #23904, #75615, #85001, .T. ) ;
#19786 = CARTESIAN_POINT ( 'NONE',  ( -15.18398860626900237, 28.73617430169797871, 5.000000000000000000 ) ) ;
#19787 = ORIENTED_EDGE ( 'NONE', *, *, #63774, .T. ) ;
#19788 = ADVANCED_FACE ( 'NONE', ( #136896 ), #91230, .T. ) ;
#19789 = ORIENTED_EDGE ( 'NONE', *, *, #76291, .T. ) ;
#19790 = CARTESIAN_POINT ( 'NONE',  ( -18.60241805642224122, 22.22500000000000142, -1.185236468576118085 ) ) ;
#19791 = FACE_OUTER_BOUND ( 'NONE', #126340, .T. ) ;
#19792 = EDGE_LOOP ( 'NONE', ( #14608, #19007, #112317, #32842 ) ) ;
#19793 = EDGE_CURVE ( 'NONE', #80757, #45698, #89812, .T. ) ;
#19794 = DIRECTION ( 'NONE',  ( 1.000000000000000000, 0.000000000000000000, 0.000000000000000000 ) ) ;
#19795 = DIRECTION ( 'NONE',  ( 1.000000000000000000, 0.000000000000000000, 0.000000000000000000 ) ) ;
#19796 = LINE ( 'NONE', #106797, #127387 ) ;
#19797 = CARTESIAN_POINT ( 'NONE',  ( 19.73159235450332005, 9.902892378096218942E-16, 0.000000000000000000 ) ) ;
#19798 = LINE ( 'NONE', #64038, #107865 ) ;
#19799 = VERTEX_POINT ( 'NONE', #126037 ) ;
#19800 = PLANE ( 'NONE',  #134818 ) ;
#19801 = PLANE ( 'NONE',  #102833 ) ;
#19802 = DIRECTION ( 'NONE',  ( 0.000000000000000000, 0.000000000000000000, -1.000000000000000000 ) ) ;
#19803 = FACE_OUTER_BOUND ( 'NONE', #48331, .T. ) ;
#19804 = EDGE_CURVE ( 'NONE', #57991, #39522, #13658, .T. ) ;
#19805 = DIRECTION ( 'NONE',  ( -0.7071067811865486830, -0.7071067811865464625, 0.000000000000000000 ) ) ;
#19806 = CARTESIAN_POINT ( 'NONE',  ( 52.43336038379623432, 2.130196079827431532, -7.949999999999997513 ) ) ;
#19807 = AXIS2_PLACEMENT_3D ( 'NONE', #118431, #96648, #115546 ) ;
#19808 = DIRECTION ( 'NONE',  ( -0.6830127018922181881, 0.6830127018922202975, -0.2588190451025214056 ) ) ;
#19809 = ORIENTED_EDGE ( 'NONE', *, *, #87652, .F. ) ;
#19810 = VERTEX_POINT ( 'NONE', #1355 ) ;
#19811 = CARTESIAN_POINT ( 'NONE',  ( 50.43750000000000000, 5.819803920172573974, -5.819803920172572198 ) ) ;
#19812 = CARTESIAN_POINT ( 'NONE',  ( 22.85159235450332105, 9.902892378096218942E-16, 0.000000000000000000 ) ) ;
#19813 = AXIS2_PLACEMENT_3D ( 'NONE', #30926, #86000, #130238 ) ;
#19814 = EDGE_CURVE ( 'NONE', #76846, #26526, #114371, .T. ) ;
#19815 = DIRECTION ( 'NONE',  ( -0.7071067811865486830, -0.7071067811865464625, 0.000000000000000000 ) ) ;
#19816 = DIRECTION ( 'NONE',  ( 0.7071067811865487940, 0.7071067811865463515, -0.000000000000000000 ) ) ;
#19817 = ORIENTED_EDGE ( 'NONE', *, *, #25779, .F. ) ;
#19818 = CARTESIAN_POINT ( 'NONE',  ( 2.683420388672089985, -6.740707523384216415, 11.88629033278123792 ) ) ;
#19819 = CARTESIAN_POINT ( 'NONE',  ( 43.75043019189810423, 3.055000000000002824, -5.291415217122919401 ) ) ;
#19820 = VERTEX_POINT ( 'NONE', #12953 ) ;
#19821 = CARTESIAN_POINT ( 'NONE',  ( 34.45011844616453800, -10.48371918836239125, 5.000000000000001776 ) ) ;
#19822 = ORIENTED_EDGE ( 'NONE', *, *, #12432, .F. ) ;
#19823 = ORIENTED_EDGE ( 'NONE', *, *, #15035, .F. ) ;
#19824 = CARTESIAN_POINT ( 'NONE',  ( -27.48921356237309155, -27.52281430457074762, 5.000000000000000000 ) ) ;
#19825 = CARTESIAN_POINT ( 'NONE',  ( 81.01669371712955581, 7.950000000000000178, -2.130196079827421318 ) ) ;
#19826 = DIRECTION ( 'NONE',  ( -1.000000000000000000, -0.000000000000000000, -0.000000000000000000 ) ) ;
#19827 = SURFACE_STYLE_FILL_AREA ( #107555 ) ;
#19828 = VERTEX_POINT ( 'NONE', #70268 ) ;
#19829 = EDGE_CURVE ( 'NONE', #3009, #98945, #102145, .T. ) ;
#19830 = FACE_OUTER_BOUND ( 'NONE', #114576, .T. ) ;
#19832 = ORIENTED_EDGE ( 'NONE', *, *, #63238, .F. ) ;
#19831 = LINE ( 'NONE', #101504, #114696 ) ;
#19833 = CARTESIAN_POINT ( 'NONE',  ( 85.89626352523144703, 4.472830434245840259, -4.472830434245838482 ) ) ;
#19834 = CARTESIAN_POINT ( 'NONE',  ( 2.816011393730999401, 28.73617430169785436, 5.000000000000000000 ) ) ;
#19835 = CARTESIAN_POINT ( 'NONE',  ( 28.49999999999981171, -1.533600742197719580, 5.000000000000000000 ) ) ;
#19836 = CARTESIAN_POINT ( 'NONE',  ( -17.99451991528748351, 28.92564299267950645, 4.000000000000000000 ) ) ;
#19837 = LINE ( 'NONE', #140900, #127331 ) ;
#19838 = LINE ( 'NONE', #53184, #131906 ) ;
#19839 = VECTOR ( 'NONE', #39662, 1000.000000000000000 ) ;
#19840 = EDGE_CURVE ( 'NONE', #129197, #49512, #124593, .T. ) ;
#19841 = AXIS2_PLACEMENT_3D ( 'NONE', #38743, #72128, #132194 ) ;
#19842 = VERTEX_POINT ( 'NONE', #26002 ) ;
#19843 = CONICAL_SURFACE ( 'NONE', #49992, 2.055000000000001048, 0.9599310885968758145 ) ;
#19844 = CARTESIAN_POINT ( 'NONE',  ( -19.05000000000000071, 3.174999999999997158, 5.000000000000000000 ) ) ;
#19845 = CARTESIAN_POINT ( 'NONE',  ( 70.78709685856478018, 3.054999999999997495, 5.291415217122919401 ) ) ;
#19846 = LINE ( 'NONE', #141652, #60407 ) ;
#19847 = FACE_OUTER_BOUND ( 'NONE', #130936, .T. ) ;
#19848 = LINE ( 'NONE', #8920, #96577 ) ;
#19849 = VERTEX_POINT ( 'NONE', #57951 ) ;
#19850 = ORIENTED_EDGE ( 'NONE', *, *, #91179, .F. ) ;
#19851 = VECTOR ( 'NONE', #119962, 1000.000000000000000 ) ;
#19852 = DIRECTION ( 'NONE',  ( 0.6830127018922180770, -0.6830127018922204085, -0.2588190451025213501 ) ) ;
#19853 = SURFACE_SIDE_STYLE ('',( #7541 ) ) ;
#19854 = ORIENTED_EDGE ( 'NONE', *, *, #18437, .T. ) ;
#19855 = EDGE_CURVE ( 'NONE', #42001, #94991, #26706, .T. ) ;
#19856 = ORIENTED_EDGE ( 'NONE', *, *, #29130, .T. ) ;
#19857 = EDGE_CURVE ( 'NONE', #113212, #8140, #123187, .T. ) ;
#19858 = LINE ( 'NONE', #55370, #72261 ) ;
#19859 = ORIENTED_EDGE ( 'NONE', *, *, #80033, .T. ) ;
#19860 = CARTESIAN_POINT ( 'NONE',  ( 18.15612307739229081, -22.22500000000000142, 4.000000000000000000 ) ) ;
#19861 = LINE ( 'NONE', #30772, #15552 ) ;
#19862 = CARTESIAN_POINT ( 'NONE',  ( 14.74000000000000021, 2.055000000000001492, 2.516649172247811554E-16 ) ) ;
#19863 = FACE_BOUND ( 'NONE', #132562, .T. ) ;
#19864 = EDGE_CURVE ( 'NONE', #46897, #96881, #80399, .T. ) ;
#19865 = FACE_OUTER_BOUND ( 'NONE', #118913, .T. ) ;
#19866 = CARTESIAN_POINT ( 'NONE',  ( 40.62086038379622721, -6.884901960086286188, 3.974999999999997424 ) ) ;
#19867 = LINE ( 'NONE', #64828, #68820 ) ;
#19869 = ORIENTED_EDGE ( 'NONE', *, *, #106004, .F. ) ;
#19868 = LINE ( 'NONE', #8945, #92147 ) ;
#19870 = DIRECTION ( 'NONE',  ( -0.7071067811865486830, -0.7071067811865464625, 0.000000000000000000 ) ) ;
#19871 = ORIENTED_EDGE ( 'NONE', *, *, #15596, .T. ) ;
#19872 = ORIENTED_EDGE ( 'NONE', *, *, #84150, .T. ) ;
#19873 = CARTESIAN_POINT ( 'NONE',  ( 83.47459685856478018, 1.637169565754164280, -6.109999999999996767 ) ) ;
#19874 = EDGE_LOOP ( 'NONE', ( #84755, #105957, #108645, #135459 ) ) ;
#19875 = FACE_OUTER_BOUND ( 'NONE', #46866, .T. ) ;
#19876 = FACE_OUTER_BOUND ( 'NONE', #107929, .T. ) ;
#19877 = ORIENTED_EDGE ( 'NONE', *, *, #73535, .F. ) ;
#19878 = CARTESIAN_POINT ( 'NONE',  ( -31.49999999999977973, 19.39370406404964697, 1.459788787078273753 ) ) ;
#19879 = LINE ( 'NONE', #75716, #132797 ) ;
#19880 = CARTESIAN_POINT ( 'NONE',  ( -22.43312800248727967, -21.74070752338406010, 6.915939825044126188 ) ) ;
#19881 = CARTESIAN_POINT ( 'NONE',  ( 12.18398860626900060, 28.73617430169795739, 5.000000000000000000 ) ) ;
#19882 = LINE ( 'NONE', #118487, #68987 ) ;
#19883 = FACE_OUTER_BOUND ( 'NONE', #30071, .T. ) ;
#19884 = LINE ( 'NONE', #63446, #86370 ) ;
#19885 = CARTESIAN_POINT ( 'NONE',  ( -28.82816939922332011, 18.75929247661552779, 4.000000000000000000 ) ) ;
#19886 = EDGE_LOOP ( 'NONE', ( #35198, #92694, #86276, #126892 ) ) ;
#19887 = DIRECTION ( 'NONE',  ( 0.7071067811865487940, -0.7071067811865463515, 0.000000000000000000 ) ) ;
#19888 = VERTEX_POINT ( 'NONE', #2800 ) ;
#19889 = LINE ( 'NONE', #84477, #10186 ) ;
#19890 = DIRECTION ( 'NONE',  ( 0.7071067811865487940, 0.7071067811865463515, 0.000000000000000000 ) ) ;
#19891 = ORIENTED_EDGE ( 'NONE', *, *, #138410, .T. ) ;
#19892 = ORIENTED_EDGE ( 'NONE', *, *, #80883, .F. ) ;
#19893 = VERTEX_POINT ( 'NONE', #114425 ) ;
#19894 = CARTESIAN_POINT ( 'NONE',  ( 34.12543019189810423, 5.291415217122919401, 3.055000000000002824 ) ) ;
#19895 = ORIENTED_EDGE ( 'NONE', *, *, #5053, .F. ) ;
#19896 = DIRECTION ( 'NONE',  ( -1.000000000000000000, -1.224606353822377258E-16, -0.000000000000000000 ) ) ;
#19897 = VECTOR ( 'NONE', #141263, 1000.000000000000000 ) ;
#19898 = EDGE_CURVE ( 'NONE', #14772, #26574, #134790, .T. ) ;
#19899 = CARTESIAN_POINT ( 'NONE',  ( 21.48330628287043709, 6.094999999999991758, 1.633150327867687102 ) ) ;
#19900 = CARTESIAN_POINT ( 'NONE',  ( -5.900168161225546548, 12.95172380562260805, -24.96972421923774377 ) ) ;
#19901 = ADVANCED_FACE ( 'NONE', ( #81844 ), #58686, .T. ) ;
#19902 = VERTEX_POINT ( 'NONE', #68125 ) ;
#19903 = AXIS2_PLACEMENT_3D ( 'NONE', #69095, #6431, #82632 ) ;
#19904 = FACE_OUTER_BOUND ( 'NONE', #72633, .T. ) ;
#19906 = ORIENTED_EDGE ( 'NONE', *, *, #65832, .T. ) ;
#19905 = EDGE_CURVE ( 'NONE', #74597, #109521, #12252, .T. ) ;
#19907 = CARTESIAN_POINT ( 'NONE',  ( 39.29974487139159578, -27.71228299555233576, 4.000000000000000000 ) ) ;
#19908 = DIRECTION ( 'NONE',  ( 0.000000000000000000, -0.3543493200069153248, -0.9351131265310291818 ) ) ;
#19910 = EDGE_LOOP ( 'NONE', ( #100919, #24405, #30412, #138541 ) ) ;
#19909 = LINE ( 'NONE', #108319, #79608 ) ;
#19911 = ORIENTED_EDGE ( 'NONE', *, *, #41416, .F. ) ;
#19912 = EDGE_CURVE ( 'NONE', #114730, #125554, #101404, .T. ) ;
#19913 =( BOUNDED_CURVE ( )  B_SPLINE_CURVE ( 3, ( #80333, #124522, #58612, #102784 ),
 .UNSPECIFIED., .F., .F. ) 
 B_SPLINE_CURVE_WITH_KNOTS ( ( 4, 4 ),
 ( 1.964434688349490532, 3.503810798801449522 ),
 .UNSPECIFIED. ) 
 CURVE ( )  GEOMETRIC_REPRESENTATION_ITEM ( )  RATIONAL_B_SPLINE_CURVE ( ( 1.000000000000000000, 0.8120851936182292841, 0.8120851936182292841, 1.000000000000000000 ) ) 
 REPRESENTATION_ITEM ( '' )  );
#19914 = DIRECTION ( 'NONE',  ( -0.000000000000000000, 0.3543493200069153248, 0.9351131265310292928 ) ) ;
#19915 = DIRECTION ( 'NONE',  ( 0.3543493200069162685, -0.000000000000000000, -0.9351131265310288487 ) ) ;
#19916 = ORIENTED_EDGE ( 'NONE', *, *, #108484, .T. ) ;
#19917 = DIRECTION ( 'NONE',  ( 0.000000000000000000, 0.000000000000000000, 1.000000000000000000 ) ) ;
#19918 = EDGE_LOOP ( 'NONE', ( #120774, #85903, #137024, #19237 ) ) ;
#19919 = ORIENTED_EDGE ( 'NONE', *, *, #137486, .F. ) ;
#19920 = VERTEX_POINT ( 'NONE', #35486 ) ;
#19922 = ADVANCED_FACE ( 'NONE', ( #56537 ), #68814, .F. ) ;
#19921 = VECTOR ( 'NONE', #5752, 1000.000000000000227 ) ;
#19923 = DIRECTION ( 'NONE',  ( 0.6830127018922180770, -0.6830127018922204085, -0.2588190451025213501 ) ) ;
#19924 = LINE ( 'NONE', #99623, #64662 ) ;
#19925 = DIRECTION ( 'NONE',  ( -0.3543493200069162685, -0.000000000000000000, -0.9351131265310288487 ) ) ;
#19926 = DIRECTION ( 'NONE',  ( -1.000000000000000000, -1.224606353822377258E-16, -0.000000000000000000 ) ) ;
#19927 = EDGE_CURVE ( 'NONE', #63317, #33976, #100712, .T. ) ;
#19928 = CARTESIAN_POINT ( 'NONE',  ( -23.81601139373100295, 28.73617430169770870, 5.000000000000000000 ) ) ;
#19929 = CARTESIAN_POINT ( 'NONE',  ( -34.49999999999975131, 19.46425560840030400, 4.994342998332171213 ) ) ;
#19930 = EDGE_CURVE ( 'NONE', #27059, #67630, #47098, .T. ) ;
#19931 = VERTEX_POINT ( 'NONE', #113716 ) ;
#19932 = DIRECTION ( 'NONE',  ( -0.6830127018922181881, 0.6830127018922202975, -0.2588190451025214056 ) ) ;
#19933 = ORIENTED_EDGE ( 'NONE', *, *, #4077, .T. ) ;
#19934 = FACE_OUTER_BOUND ( 'NONE', #122280, .T. ) ;
#19935 = EDGE_CURVE ( 'NONE', #22706, #58114, #128864, .T. ) ;
#19936 = AXIS2_PLACEMENT_3D ( 'NONE', #111112, #11803, #56090 ) ;
#19937 = CARTESIAN_POINT ( 'NONE',  ( 59.99451991528749772, 28.92564299267980132, 4.000000000000000000 ) ) ;
#19938 = AXIS2_PLACEMENT_3D ( 'NONE', #15159, #123965, #103596 ) ;
#19939 = ORIENTED_EDGE ( 'NONE', *, *, #123751, .F. ) ;
#19940 = CARTESIAN_POINT ( 'NONE',  ( 0.000000000000000000, 0.000000000000000000, 5.000000000000000000 ) ) ;
#19941 = CARTESIAN_POINT ( 'NONE',  ( 2.999999999999992450, -19.44781430457064175, 5.000000000000000000 ) ) ;
#19942 = ORIENTED_EDGE ( 'NONE', *, *, #25430, .T. ) ;
#19943 = AXIS2_PLACEMENT_3D ( 'NONE', #126968, #27659, #22474 ) ;
#19944 = ORIENTED_EDGE ( 'NONE', *, *, #118294, .F. ) ;
#19945 = CARTESIAN_POINT ( 'NONE',  ( 6.813491353976342424, -15.74070752338412049, 8.904080028138924519 ) ) ;
#19946 = CARTESIAN_POINT ( 'NONE',  ( 27.00000000000000355, 0.000000000000000000, 6.349999999999999645 ) ) ;
#19947 = UNCERTAINTY_MEASURE_WITH_UNIT (LENGTH_MEASURE( 1.000000000000000082E-05 ), #57177, 'distance_accuracy_value', 'NONE');
#19948 = CARTESIAN_POINT ( 'NONE',  ( 1.516262732464673579, -0.3999999999999997446, -2.467792535850613866 ) ) ;
#19949 = VECTOR ( 'NONE', #114470, 1000.000000000000000 ) ;
#19950 = DIRECTION ( 'NONE',  ( 1.000000000000000000, 0.000000000000000000, 0.000000000000000000 ) ) ;
#19951 = DIRECTION ( 'NONE',  ( -0.000000000000000000, -0.3543493200069152693, 0.9351131265310292928 ) ) ;
#19952 = CARTESIAN_POINT ( 'NONE',  ( 62.91209685856477307, 5.291415217122922066, -3.054999999999995275 ) ) ;
#19953 = LINE ( 'NONE', #120683, #2442 ) ;
#19954 = FILL_AREA_STYLE_COLOUR ( '', #122398 ) ;
#19955 = CARTESIAN_POINT ( 'NONE',  ( -12.20000000000000284, -34.64999999999999147, -40.00000000000000000 ) ) ;
#19956 = ORIENTED_EDGE ( 'NONE', *, *, #100741, .F. ) ;
#19957 = DIRECTION ( 'NONE',  ( 0.7071067811865487940, -0.7071067811865463515, 0.000000000000000000 ) ) ;
#19958 = EDGE_CURVE ( 'NONE', #134932, #56792, #106365, .T. ) ;
#19959 = ORIENTED_EDGE ( 'NONE', *, *, #54752, .F. ) ;
#19960 = DIRECTION ( 'NONE',  ( 0.3543493200069162685, -0.000000000000000000, -0.9351131265310288487 ) ) ;
#19961 = FILL_AREA_STYLE ('',( #52597 ) ) ;
#19962 = ORIENTED_EDGE ( 'NONE', *, *, #23476, .T. ) ;
#19963 = DIRECTION ( 'NONE',  ( 0.000000000000000000, -1.000000000000000000, 0.000000000000000000 ) ) ;
#19965 = VERTEX_POINT ( 'NONE', #128181 ) ;
#19964 = PLANE ( 'NONE',  #14112 ) ;
#19966 = DIRECTION ( 'NONE',  ( -0.3543493200069162685, -0.000000000000000000, -0.9351131265310288487 ) ) ;
#19967 = DIRECTION ( 'NONE',  ( -0.000000000000000000, -0.000000000000000000, 1.000000000000000000 ) ) ;
#19968 = DIRECTION ( 'NONE',  ( 0.7071067811865486830, -0.7071067811865464625, -0.000000000000000000 ) ) ;
#19969 = EDGE_LOOP ( 'NONE', ( #121939, #120565, #100707, #36953, #18668 ) ) ;
#19970 = ORIENTED_EDGE ( 'NONE', *, *, #2039, .T. ) ;
#19971 = CARTESIAN_POINT ( 'NONE',  ( 28.00000000000002487, -49.14999999999999147, -34.92499999999976978 ) ) ;
#19972 = LINE ( 'NONE', #118578, #30598 ) ;
#19973 = DIRECTION ( 'NONE',  ( 0.7071067811865487940, 0.7071067811865463515, 0.000000000000000000 ) ) ;
#19974 = CARTESIAN_POINT ( 'NONE',  ( 80.43336038379622721, 2.130196079827431532, -7.949999999999997513 ) ) ;
#19975 = LINE ( 'NONE', #41750, #129615 ) ;
#19976 = LINE ( 'NONE', #64223, #39110 ) ;
#19977 = ORIENTED_EDGE ( 'NONE', *, *, #119747, .F. ) ;
#19978 = DIRECTION ( 'NONE',  ( -0.6830127018922181881, 0.6830127018922202975, -0.2588190451025214056 ) ) ;
#19979 = ADVANCED_FACE ( 'NONE', ( #138328 ), #52035, .T. ) ;
#19980 = CARTESIAN_POINT ( 'NONE',  ( 27.18398860626900060, 28.73617430169806042, 5.000000000000000000 ) ) ;
#19981 = CARTESIAN_POINT ( 'NONE',  ( 29.31249999999999645, -4.461849672132299993, -4.461849672132299105 ) ) ;
#19982 = VECTOR ( 'NONE', #88861, 1000.000000000000227 ) ;
#19983 = ORIENTED_EDGE ( 'NONE', *, *, #87936, .T. ) ;
#19984 = DIRECTION ( 'NONE',  ( -0.7071067811865486830, -0.7071067811865464625, 0.000000000000000000 ) ) ;
#19985 = ORIENTED_EDGE ( 'NONE', *, *, #59368, .F. ) ;
#19986 = ADVANCED_FACE ( 'NONE', ( #6325 ), #37093, .T. ) ;
#19987 = CARTESIAN_POINT ( 'NONE',  ( 80.06293019189810423, 1.637169565754157174, 6.110000000000002984 ) ) ;
#19988 = DIRECTION ( 'NONE',  ( 0.7071067811865487940, 0.7071067811865463515, 0.000000000000000000 ) ) ;
#19989 = VECTOR ( 'NONE', #135876, 1000.000000000000000 ) ;
#19990 = CARTESIAN_POINT ( 'NONE',  ( 7.171830600776425868, 12.75929247661559529, 4.000000000000000000 ) ) ;
#19991 = ORIENTED_EDGE ( 'NONE', *, *, #1078, .T. ) ;
#19992 = DIRECTION ( 'NONE',  ( -0.7071067811865486830, 0.7071067811865464625, 0.000000000000000000 ) ) ;
#19993 = CARTESIAN_POINT ( 'NONE',  ( 34.49999999999976552, 21.05432934483073026, 4.994342998332161443 ) ) ;
#19994 = DIRECTION ( 'NONE',  ( -1.000000000000000000, -1.224606353822377258E-16, -0.000000000000000000 ) ) ;
#19995 = ADVANCED_FACE ( 'NONE', ( #38306 ), #49200, .F. ) ;
#19996 = CARTESIAN_POINT ( 'NONE',  ( 24.75860074219779605, 21.72500000000000853, 5.000000000000000000 ) ) ;
#19998 = VERTEX_POINT ( 'NONE', #18658 ) ;
#19997 = CARTESIAN_POINT ( 'NONE',  ( 34.45011844616451668, -8.997695858405966973, 5.000000000000000888 ) ) ;
#19999 = SURFACE_STYLE_USAGE ( .BOTH. , #88146 ) ;
#20000 = CARTESIAN_POINT ( 'NONE',  ( 0.000000000000000000, 0.000000000000000000, 5.000000000000000000 ) ) ;
#20001 = DIRECTION ( 'NONE',  ( 0.7071067811865487940, 0.7071067811865463515, 0.000000000000000000 ) ) ;
#20002 = CARTESIAN_POINT ( 'NONE',  ( -6.489213562373093325, -27.52281430457059841, 5.000000000000000000 ) ) ;
#20003 = ORIENTED_EDGE ( 'NONE', *, *, #52298, .F. ) ;
#20004 = VECTOR ( 'NONE', #138837, 999.9999999999998863 ) ;
#20005 = ORIENTED_EDGE ( 'NONE', *, *, #33227, .F. ) ;
#20006 = CARTESIAN_POINT ( 'NONE',  ( 60.81293019189811133, -1.637169565754159617, -6.110000000000001208 ) ) ;
#20007 = ORIENTED_EDGE ( 'NONE', *, *, #141487, .F. ) ;
#20008 = DIRECTION ( 'NONE',  ( -0.6830127018922181881, 0.6830127018922202975, -0.2588190451025214056 ) ) ;
#20009 = CARTESIAN_POINT ( 'NONE',  ( -7.069960254864042781, -0.7407075233842770334, 13.87443053587612418 ) ) ;
#20010 = CARTESIAN_POINT ( 'NONE',  ( 15.48921356237309510, -27.52281430457066236, 5.000000000000000000 ) ) ;
#20011 = CARTESIAN_POINT ( 'NONE',  ( -1.828169399223515512, 21.75929247661549581, 4.000000000000000000 ) ) ;
#20012 = ORIENTED_EDGE ( 'NONE', *, *, #141990, .T. ) ;
#20013 = CARTESIAN_POINT ( 'NONE',  ( 28.49999999999980815, -7.420205493532869845, -2.617629953481187766 ) ) ;
#20014 = CARTESIAN_POINT ( 'NONE',  ( -15.32816939922341781, -15.74070752338412049, 4.000000000000000000 ) ) ;
#20015 = VERTEX_POINT ( 'NONE', #29541 ) ;
#20016 = EDGE_CURVE ( 'NONE', #80619, #102502, #117249, .T. ) ;
#20017 = AXIS2_PLACEMENT_3D ( 'NONE', #69295, #46127, #79500 ) ;
#20018 = CARTESIAN_POINT ( 'NONE',  ( 21.45983838949727129, 18.75929247661552068, 8.305906642995537936 ) ) ;
#20019 = PLANE ( 'NONE',  #96583 ) ;
#20020 = CARTESIAN_POINT ( 'NONE',  ( 54.48921356237310221, -27.52281430457093236, 5.000000000000000000 ) ) ;
#20021 = VERTEX_POINT ( 'NONE', #84663 ) ;
#20022 = ORIENTED_EDGE ( 'NONE', *, *, #96906, .T. ) ;
#20023 = EDGE_CURVE ( 'NONE', #135612, #63645, #95517, .T. ) ;
#20024 = VECTOR ( 'NONE', #77309, 1000.000000000000000 ) ;
#20025 = CARTESIAN_POINT ( 'NONE',  ( 12.48921356237309155, -27.52281430457064104, 5.000000000000000000 ) ) ;
#20026 = EDGE_CURVE ( 'NONE', #91029, #68485, #113452, .T. ) ;
#20027 = CARTESIAN_POINT ( 'NONE',  ( 34.92499999999998295, -14.24070752338413293, 4.255531930566171184 ) ) ;
#20028 = CARTESIAN_POINT ( 'NONE',  ( 127.8677689125804733, -6.349999999999999645, 1.701477371937628158 ) ) ;
#20029 = DIRECTION ( 'NONE',  ( -0.7071067811865487940, 0.7071067811865463515, 0.000000000000000000 ) ) ;
#20030 = CARTESIAN_POINT ( 'NONE',  ( -18.70701326429291456, -21.74070752338405654, 4.999753212805221558 ) ) ;
#20031 = VECTOR ( 'NONE', #47723, 1000.000000000000000 ) ;
#20032 = VECTOR ( 'NONE', #104722, 999.9999999999998863 ) ;
#20033 = CARTESIAN_POINT ( 'NONE',  ( 8.000000000000007105, 1.469576158976826708E-15, 0.000000000000000000 ) ) ;
#20034 =( LENGTH_UNIT ( ) NAMED_UNIT ( * ) SI_UNIT ( .MILLI., .METRE. ) );
#20035 = ORIENTED_EDGE ( 'NONE', *, *, #77447, .T. ) ;
#20036 = VECTOR ( 'NONE', #1254, 1000.000000000000000 ) ;
#20038 = ORIENTED_EDGE ( 'NONE', *, *, #70056, .F. ) ;
#20037 = VECTOR ( 'NONE', #81691, 1000.000000000000000 ) ;
#20039 = CARTESIAN_POINT ( 'NONE',  ( 111.3287635252314516, 0.000000000000000000, -6.109999999999998543 ) ) ;
#20040 = VERTEX_POINT ( 'NONE', #16522 ) ;
#20041 = ORIENTED_EDGE ( 'NONE', *, *, #15596, .F. ) ;
#20042 = CARTESIAN_POINT ( 'NONE',  ( 184.0776099992040429, -48.13855614193184351, 37.56434003615978412 ) ) ;
#20043 = ADVANCED_FACE ( 'NONE', ( #139781 ), #41147, .T. ) ;
#20044 = DIRECTION ( 'NONE',  ( -4.681814790819591790E-17, -0.3543493200069152693, 0.9351131265310292928 ) ) ;
#20045 = DIRECTION ( 'NONE',  ( -0.7071067811865487940, 0.7071067811865463515, 0.000000000000000000 ) ) ;
#20046 = VERTEX_POINT ( 'NONE', #5636 ) ;
#20047 = CARTESIAN_POINT ( 'NONE',  ( 15.32816939922342669, 14.25929247661556865, 4.000000000000000000 ) ) ;
#20048 = DIRECTION ( 'NONE',  ( 0.7071067811865486830, -0.7071067811865464625, -0.000000000000000000 ) ) ;
#20050 = FACE_OUTER_BOUND ( 'NONE', #80990, .T. ) ;
#20049 = DIRECTION ( 'NONE',  ( -0.6830127018922180770, -0.6830127018922204085, -0.2588190451025213501 ) ) ;
#20051 = DIRECTION ( 'NONE',  ( 0.7071067811865486830, -0.7071067811865464625, -0.000000000000000000 ) ) ;
#20052 = CARTESIAN_POINT ( 'NONE',  ( 18.29974487139159223, -27.71228299555219010, 4.000000000000000000 ) ) ;
#20053 = ORIENTED_EDGE ( 'NONE', *, *, #45032, .T. ) ;
#20054 = CARTESIAN_POINT ( 'NONE',  ( 0.5685132242927012358, 0.4000000000000001887, -2.467792535850613866 ) ) ;
#20055 = LINE ( 'NONE', #8437, #125259 ) ;
#20056 = ORIENTED_EDGE ( 'NONE', *, *, #127769, .F. ) ;
#20057 = DIRECTION ( 'NONE',  ( 0.000000000000000000, -1.000000000000000000, 0.000000000000000000 ) ) ;
#20058 = ORIENTED_EDGE ( 'NONE', *, *, #79142, .F. ) ;
#20059 = ORIENTED_EDGE ( 'NONE', *, *, #141111, .F. ) ;
#20060 = VERTEX_POINT ( 'NONE', #7784 ) ;
#20061 = CARTESIAN_POINT ( 'NONE',  ( 66.35459685856476142, -1.637169565754161615, 6.110000000000000320 ) ) ;
#20062 = ORIENTED_EDGE ( 'NONE', *, *, #132851, .T. ) ;
#20063 = VERTEX_POINT ( 'NONE', #137628 ) ;
#20064 = DIRECTION ( 'NONE',  ( 0.7071067811865487940, 0.7071067811865463515, 0.000000000000000000 ) ) ;
#20065 = EDGE_CURVE ( 'NONE', #80065, #90172, #94089, .T. ) ;
#20066 = VECTOR ( 'NONE', #123185, 1000.000000000000000 ) ;
#20068 =( BOUNDED_CURVE ( )  B_SPLINE_CURVE ( 3, ( #92409, #59137, #124347, #123663 ),
 .UNSPECIFIED., .F., .T. ) 
 B_SPLINE_CURVE_WITH_KNOTS ( ( 4, 4 ),
 ( 2.099584536334365925, 2.152415457235772767 ),
 .UNSPECIFIED. ) 
 CURVE ( )  GEOMETRIC_REPRESENTATION_ITEM ( )  RATIONAL_B_SPLINE_CURVE ( ( 1.000000000000000000, 0.9997674213408587196, 0.9997674213408587196, 1.000000000000000000 ) ) 
 REPRESENTATION_ITEM ( '' )  );
#20067 = CARTESIAN_POINT ( 'NONE',  ( 102.6670968585647756, -3.055000000000000160, -5.291415217122921177 ) ) ;
#20069 = CARTESIAN_POINT ( 'NONE',  ( -5.999999999999956479, 12.83542986846996570, -1.025386466790356943 ) ) ;
#20070 = ADVANCED_FACE ( 'NONE', ( #15775 ), #82521, .T. ) ;
#20071 = LINE ( 'NONE', #75907, #62858 ) ;
#20072 = ORIENTED_EDGE ( 'NONE', *, *, #112858, .T. ) ;
#20073 = DIRECTION ( 'NONE',  ( -0.7071067811865486830, 0.7071067811865464625, 0.000000000000000000 ) ) ;
#20074 = VECTOR ( 'NONE', #15183, 1000.000000000000000 ) ;
#20075 = LINE ( 'NONE', #133167, #7605 ) ;
#20076 = ADVANCED_FACE ( 'NONE', ( #126709 ), #27396, .F. ) ;
#20077 = ADVANCED_FACE ( 'NONE', ( #83234 ), #49911, .T. ) ;
#20078 = LINE ( 'NONE', #31694, #79264 ) ;
#20079 = DIRECTION ( 'NONE',  ( 0.6830127018922180770, 0.6830127018922202975, -0.2588190451025213501 ) ) ;
#20080 = ORIENTED_EDGE ( 'NONE', *, *, #33468, .T. ) ;
#20081 = DIRECTION ( 'NONE',  ( 1.000000000000000000, 0.000000000000000000, 0.000000000000000000 ) ) ;
#20082 = VERTEX_POINT ( 'NONE', #72401 ) ;
#20083 = EDGE_LOOP ( 'NONE', ( #21368, #29209, #41960 ) ) ;
#20084 = EDGE_LOOP ( 'NONE', ( #87176, #128799, #53750, #81221 ) ) ;
#20085 = CARTESIAN_POINT ( 'NONE',  ( 117.7454301918981230, -5.291415217122918513, -3.055000000000000160 ) ) ;
#20086 = ORIENTED_EDGE ( 'NONE', *, *, #55881, .T. ) ;
#20087 = CARTESIAN_POINT ( 'NONE',  ( -35.99451991528749772, 28.92564299267963079, 4.000000000000000000 ) ) ;
#20088 = FACE_OUTER_BOUND ( 'NONE', #76548, .T. ) ;
#20089 = EDGE_CURVE ( 'NONE', #116410, #115114, #17254, .T. ) ;
#20090 = CARTESIAN_POINT ( 'NONE',  ( -14.99451991528749595, 28.92564299267948513, 4.000000000000000000 ) ) ;
#20091 = EDGE_CURVE ( 'NONE', #16237, #75959, #99070, .T. ) ;
#20092 = ORIENTED_EDGE ( 'NONE', *, *, #55127, .F. ) ;
#20093 = CARTESIAN_POINT ( 'NONE',  ( 3.060608989244792966, -48.47007572038103262, 38.12657027910959329 ) ) ;
#20094 = ORIENTED_EDGE ( 'NONE', *, *, #27883, .T. ) ;
#20095 = ADVANCED_FACE ( 'NONE', ( #65071 ), #119397, .F. ) ;
#20096 = AXIS2_PLACEMENT_3D ( 'NONE', #11665, #70424, #137784 ) ;
#20097 = CARTESIAN_POINT ( 'NONE',  ( 0.8537364747685527444, -5.808823158059035485, -5.808823158059033709 ) ) ;
#20098 = CARTESIAN_POINT ( 'NONE',  ( 11.70025512860841133, -27.71228299555198049, 4.000000000000000000 ) ) ;
#20099 = CARTESIAN_POINT ( 'NONE',  ( 9.208651418775088970, 2.500000000000000888, 0.000000000000000000 ) ) ;
#20100 = PRESENTATION_LAYER_ASSIGNMENT (  '', '', ( #10780 ) ) ;
#20101 = CARTESIAN_POINT ( 'NONE',  ( 39.35416666666666430, -2.130196079827501698, -7.949999999999956657 ) ) ;
#20102 = ORIENTED_EDGE ( 'NONE', *, *, #64266, .T. ) ;
#20103 = ORIENTED_EDGE ( 'NONE', *, *, #18591, .F. ) ;
#20104 = ORIENTED_EDGE ( 'NONE', *, *, #68236, .T. ) ;
#20105 = CARTESIAN_POINT ( 'NONE',  ( -32.99999999999976552, -18.03360074219755660, 5.000000000000000000 ) ) ;
#20106 = FILL_AREA_STYLE_COLOUR ( '', #41770 ) ;
#20107 = ADVANCED_FACE ( 'NONE', ( #87516 ), #141161, .F. ) ;
#20108 = CARTESIAN_POINT ( 'NONE',  ( -12.20000000000000462, -21.76999999999999247, 0.000000000000000000 ) ) ;
#20109 = DIRECTION ( 'NONE',  ( 1.000000000000000000, 0.000000000000000000, 0.000000000000000000 ) ) ;
#20110 = CYLINDRICAL_SURFACE ( 'NONE', #129043, 2.500000000000000444 ) ;
#20111 = PLANE ( 'NONE',  #59932 ) ;
#20112 = CARTESIAN_POINT ( 'NONE',  ( 26.68793019189810067, 6.110000000000002984, -1.637169565754156730 ) ) ;
#20113 =( NAMED_UNIT ( * ) PLANE_ANGLE_UNIT ( ) SI_UNIT ( $, .RADIAN. ) );
#20114 = LINE ( 'NONE', #64360, #25766 ) ;
#20115 = VERTEX_POINT ( 'NONE', #52726 ) ;
#20116 = CARTESIAN_POINT ( 'NONE',  ( -26.54016161050243738, 18.75929247661552779, 8.305906642995426026 ) ) ;
#20117 = EDGE_CURVE ( 'NONE', #136035, #29037, #120100, .T. ) ;
#20118 = VERTEX_POINT ( 'NONE', #88237 ) ;
#20119 = LINE ( 'NONE', #507, #8237 ) ;
#20120 = ORIENTED_EDGE ( 'NONE', *, *, #4892, .T. ) ;
#20121 = CARTESIAN_POINT ( 'NONE',  ( 22.88982677111772546, -22.22499999999999787, 4.785647885939350310 ) ) ;
#20123 = ORIENTED_EDGE ( 'NONE', *, *, #112509, .T. ) ;
#20122 = FACE_OUTER_BOUND ( 'NONE', #92955, .T. ) ;
#20124 = VECTOR ( 'NONE', #51442, 1000.000000000000000 ) ;
#20125 = LINE ( 'NONE', #33211, #19073 ) ;
#20126 = EDGE_CURVE ( 'NONE', #44653, #60654, #73049, .T. ) ;
#20127 = ORIENTED_EDGE ( 'NONE', *, *, #39901, .T. ) ;
#20128 = LINE ( 'NONE', #516, #36912 ) ;
#20129 = ORIENTED_EDGE ( 'NONE', *, *, #99935, .F. ) ;
#20130 = CARTESIAN_POINT ( 'NONE',  ( -19.21071296386495675, 9.141836041257182188, 4.000000000000000000 ) ) ;
#20131 = EDGE_LOOP ( 'NONE', ( #15149, #27108, #123065, #80900 ) ) ;
#20132 = VECTOR ( 'NONE', #44523, 1000.000000000000000 ) ;
#20134 = VECTOR ( 'NONE', #80640, 1000.000000000000227 ) ;
#20133 = AXIS2_PLACEMENT_3D ( 'NONE', #100816, #121828, #21106 ) ;
#20135 = ADVANCED_FACE ( 'NONE', ( #130323 ), #9185, .T. ) ;
#20137 = CARTESIAN_POINT ( 'NONE',  ( 109.0166937171295416, 7.950000000000001066, -2.130196079827421318 ) ) ;
#20136 = CIRCLE ( 'NONE', #34043, 2.999999999999999112 ) ;
#20138 = DIRECTION ( 'NONE',  ( -0.000000000000000000, 0.000000000000000000, 1.000000000000000000 ) ) ;
#20139 = CARTESIAN_POINT ( 'NONE',  ( 23.20710678118638626, 15.75929247661555443, 5.000000000000000000 ) ) ;
#20140 = DIRECTION ( 'NONE',  ( 0.7071067811865487940, 0.7071067811865463515, 0.000000000000000000 ) ) ;
#20141 = DIRECTION ( 'NONE',  ( -0.7071067811865486830, -0.7071067811865464625, 0.000000000000000000 ) ) ;
#20142 = AXIS2_PLACEMENT_3D ( 'NONE', #133208, #78813, #101261 ) ;
#20143 = CARTESIAN_POINT ( 'NONE',  ( 22.49999999999984723, -4.912538124160710673, 4.000000000000000000 ) ) ;
#20144 = CARTESIAN_POINT ( 'NONE',  ( 6.854166666666666075, 1.633150327867695095, 6.094999999999988205 ) ) ;
#20145 = CARTESIAN_POINT ( 'NONE',  ( 12.52040314143522082, 7.934999999999988951, -2.126176841940961904 ) ) ;
#20146 = VECTOR ( 'NONE', #117527, 1000.000000000000000 ) ;
#20147 = DIRECTION ( 'NONE',  ( -0.000000000000000000, 0.3543493200069153248, 0.9351131265310292928 ) ) ;
#20148 = LINE ( 'NONE', #131075, #87232 ) ;
#20149 = EDGE_LOOP ( 'NONE', ( #85106, #37189, #137791, #83566 ) ) ;
#20150 = VERTEX_POINT ( 'NONE', #64338 ) ;
#20151 = DIRECTION ( 'NONE',  ( 0.7071067811865487940, 0.7071067811865463515, 0.000000000000000000 ) ) ;
#20152 = VERTEX_POINT ( 'NONE', #33175 ) ;
#20153 = CARTESIAN_POINT ( 'NONE',  ( 0.000000000000000000, 9.735942053221458872E-16, -7.950000000000000178 ) ) ;
#20154 = ORIENTED_EDGE ( 'NONE', *, *, #33278, .T. ) ;
#20155 = CARTESIAN_POINT ( 'NONE',  ( 3.710381658649934078, -2.500000000000000000, 3.061616997868383634E-16 ) ) ;
#20156 = PLANE ( 'NONE',  #30276 ) ;
#20157 = EDGE_CURVE ( 'NONE', #68874, #138697, #21544, .T. ) ;
#20158 = CARTESIAN_POINT ( 'NONE',  ( 0.07085943933668231720, -51.15040958483978528, 36.98623100868706359 ) ) ;
#20160 = ORIENTED_EDGE ( 'NONE', *, *, #59867, .T. ) ;
#20159 = CARTESIAN_POINT ( 'NONE',  ( 25.49999999999983302, -14.94781430457066840, 5.000000000000000000 ) ) ;
#20161 = DIRECTION ( 'NONE',  ( -0.000000000000000000, 0.000000000000000000, 1.000000000000000000 ) ) ;
#20162 = VECTOR ( 'NONE', #119733, 1000.000000000000000 ) ;
#20163 = LINE ( 'NONE', #31786, #114624 ) ;
#20164 = CARTESIAN_POINT ( 'NONE',  ( 10.49999999999992539, -16.91253812416058722, 4.000000000000000000 ) ) ;
#20165 = PLANE ( 'NONE',  #82679 ) ;
#20166 = LINE ( 'NONE', #72483, #14473 ) ;
#20167 = VERTEX_POINT ( 'NONE', #97668 ) ;
#20168 = ORIENTED_EDGE ( 'NONE', *, *, #82617, .F. ) ;
#20169 = ORIENTED_EDGE ( 'NONE', *, *, #127353, .T. ) ;
#20170 = CARTESIAN_POINT ( 'NONE',  ( 100.1879301918980900, 6.110000000000002984, -1.637169565754156730 ) ) ;
#20171 = CIRCLE ( 'NONE', #47958, 2.055000000000000604 ) ;
#20172 = ORIENTED_EDGE ( 'NONE', *, *, #20023, .F. ) ;
#20173 = CARTESIAN_POINT ( 'NONE',  ( 128.2885478629722229, -48.75494892434343797, 38.51155878621300843 ) ) ;
#20174 = VECTOR ( 'NONE', #57862, 999.9999999999998863 ) ;
#20175 = LINE ( 'NONE', #119485, #87105 ) ;
#20176 = VERTEX_POINT ( 'NONE', #42610 ) ;
#20177 = FACE_OUTER_BOUND ( 'NONE', #117338, .T. ) ;
#20178 = CARTESIAN_POINT ( 'NONE',  ( 24.18398860626899705, 28.73617430169804265, 5.000000000000000000 ) ) ;
#20179 = CARTESIAN_POINT ( 'NONE',  ( 95.57876352523145158, -7.482591942790325086E-16, 6.109999999999998543 ) ) ;
#20180 = EDGE_LOOP ( 'NONE', ( #106856, #16890, #91685 ) ) ;
#20181 = LINE ( 'NONE', #76021, #42003 ) ;
#20182 = CARTESIAN_POINT ( 'NONE',  ( 72.75000000000000000, -9.735942053221458872E-16, 7.950000000000000178 ) ) ;
#20183 = STYLED_ITEM ( 'NONE', ( #50659 ), #12196 ) ;
#20184 = CARTESIAN_POINT ( 'NONE',  ( 12.18398860626900060, 28.73617430169795739, 5.000000000000000000 ) ) ;
#20185 = DIRECTION ( 'NONE',  ( 1.000000000000000000, 0.000000000000000000, 0.000000000000000000 ) ) ;
#20186 = ORIENTED_EDGE ( 'NONE', *, *, #8912, .T. ) ;
#20187 = VERTEX_POINT ( 'NONE', #77384 ) ;
#20188 = VECTOR ( 'NONE', #85304, 1000.000000000000000 ) ;
#20189 = EDGE_CURVE ( 'NONE', #47526, #58114, #76667, .T. ) ;
#20190 = ORIENTED_EDGE ( 'NONE', *, *, #47947, .T. ) ;
#20191 = CARTESIAN_POINT ( 'NONE',  ( 28.35824297541122263, 15.75929247661555799, 19.34181609438693172 ) ) ;
#20192 = EDGE_CURVE ( 'NONE', #100169, #142746, #142616, .T. ) ;
#20193 = FACE_OUTER_BOUND ( 'NONE', #73958, .T. ) ;
#20194 = CARTESIAN_POINT ( 'NONE',  ( 14.06706980810188590, 2.126176841940952134, -7.934999999999992504 ) ) ;
#20195 = CARTESIAN_POINT ( 'NONE',  ( 12.19999999999999574, -21.76999999999999247, -40.00000000000000000 ) ) ;
#20196 = CARTESIAN_POINT ( 'NONE',  ( -5.999999999999953815, -18.03360074219754949, 5.000000000000000000 ) ) ;
#20197 = ORIENTED_EDGE ( 'NONE', *, *, #18787, .T. ) ;
#20198 = VECTOR ( 'NONE', #13258, 1000.000000000000000 ) ;
#20199 = VECTOR ( 'NONE', #26083, 1000.000000000000000 ) ;
#20201 = ORIENTED_EDGE ( 'NONE', *, *, #83780, .T. ) ;
#20200 = EDGE_CURVE ( 'NONE', #125896, #64781, #120839, .T. ) ;
#20202 = CARTESIAN_POINT ( 'NONE',  ( -63.48921356237309510, -27.52281430457099631, 5.000000000000000000 ) ) ;
#20203 = EDGE_LOOP ( 'NONE', ( #115251, #128342, #132191, #140285 ) ) ;
#20204 = ORIENTED_EDGE ( 'NONE', *, *, #25985, .F. ) ;
#20205 = ADVANCED_FACE ( 'NONE', ( #86809 ), #131027, .F. ) ;
#20206 = CARTESIAN_POINT ( 'NONE',  ( 27.29974487139158512, -27.71228299555225405, 4.000000000000000000 ) ) ;
#20207 = CARTESIAN_POINT ( 'NONE',  ( 34.92499999999998295, 22.22500000000000142, 4.500000000000000888 ) ) ;
#20208 = ORIENTED_EDGE ( 'NONE', *, *, #59351, .T. ) ;
#20209 = CARTESIAN_POINT ( 'NONE',  ( 56.85416666666666430, -2.130196079827425759, -7.950000000000000178 ) ) ;
#20210 = LINE ( 'NONE', #19521, #6689 ) ;
#20211 = DIRECTION ( 'NONE',  ( 0.6830127018922180770, -0.6830127018922204085, -0.2588190451025213501 ) ) ;
#20212 = LINE ( 'NONE', #84108, #53026 ) ;
#20213 = EDGE_CURVE ( 'NONE', #60103, #61060, #99572, .T. ) ;
#20214 = ADVANCED_FACE ( 'NONE', ( #98396 ), #10636, .F. ) ;
#20215 = FACE_OUTER_BOUND ( 'NONE', #44590, .T. ) ;
#20216 = ORIENTED_EDGE ( 'NONE', *, *, #133433, .F. ) ;
#20217 = CARTESIAN_POINT ( 'NONE',  ( -9.706123077391888287, 22.22500000000000142, 4.000000000000000000 ) ) ;
#20218 = CONICAL_SURFACE ( 'NONE', #41146, 1.249999999999969802, 0.2617993877991415808 ) ;
#20219 = ORIENTED_EDGE ( 'NONE', *, *, #10006, .F. ) ;
#20220 = PLANE ( 'NONE',  #80578 ) ;
#20221 = CARTESIAN_POINT ( 'NONE',  ( 19.65643278553995543, -1.111889603260001858, -31.77067279039590986 ) ) ;
#20222 = VERTEX_POINT ( 'NONE', #133180 ) ;
#20223 = CARTESIAN_POINT ( 'NONE',  ( -8.700255128608413102, -27.71228299555199825, 4.000000000000000000 ) ) ;
#20224 = EDGE_LOOP ( 'NONE', ( #140393, #132355, #25041 ) ) ;
#20225 = CARTESIAN_POINT ( 'NONE',  ( 14.99999999999989519, 14.87792677143810316, -11.06722581663436777 ) ) ;
#20226 = ORIENTED_EDGE ( 'NONE', *, *, #364, .T. ) ;
#20227 = ORIENTED_EDGE ( 'NONE', *, *, #13494, .F. ) ;
#20228 = VECTOR ( 'NONE', #54342, 1000.000000000000000 ) ;
#20229 = ORIENTED_EDGE ( 'NONE', *, *, #49999, .T. ) ;
#20231 = VECTOR ( 'NONE', #78489, 999.9999999999998863 ) ;
#20230 = AXIS2_PLACEMENT_3D ( 'NONE', #86585, #119181, #42373 ) ;
#20232 = VECTOR ( 'NONE', #129133, 1000.000000000000000 ) ;
#20233 = CARTESIAN_POINT ( 'NONE',  ( 29.66209685856477307, -5.291415217122919401, 3.054999999999997939 ) ) ;
#20234 = CARTESIAN_POINT ( 'NONE',  ( 0.000000000000000000, 0.000000000000000000, 5.000000000000000000 ) ) ;
#20235 = DIRECTION ( 'NONE',  ( 0.7071067811865486830, -0.7071067811865464625, -0.000000000000000000 ) ) ;
#20236 = CARTESIAN_POINT ( 'NONE',  ( -12.18398860626900060, 28.73617430169795739, 5.000000000000000000 ) ) ;
#20237 = CARTESIAN_POINT ( 'NONE',  ( 127.0212635252314328, -4.472830434245838482, -4.472830434245840259 ) ) ;
#20238 = CARTESIAN_POINT ( 'NONE',  ( -22.17183060077631396, 21.75929247661548871, 4.000000000000000000 ) ) ;
#20239 = EDGE_CURVE ( 'NONE', #121929, #10073, #74519, .T. ) ;
#20240 = LINE ( 'NONE', #77533, #140834 ) ;
#20241 = DIRECTION ( 'NONE',  ( 0.6830127018922181881, 0.6830127018922202975, -0.2588190451025214056 ) ) ;
#20242 = VECTOR ( 'NONE', #117870, 1000.000000000000000 ) ;
#20243 = CARTESIAN_POINT ( 'NONE',  ( 34.53569095963128177, 22.21392809009763170, 4.239552123775266246 ) ) ;
#20244 = EDGE_CURVE ( 'NONE', #31644, #123367, #6936, .T. ) ;
#20245 = EDGE_CURVE ( 'NONE', #70018, #98898, #78790, .T. ) ;
#20246 = CARTESIAN_POINT ( 'NONE',  ( -27.29974487139158512, -27.71228299555225405, 4.000000000000000000 ) ) ;
#20247 = FACE_OUTER_BOUND ( 'NONE', #114675, .T. ) ;
#20248 = DIRECTION ( 'NONE',  ( -0.7071067811865486830, -0.7071067811865464625, 0.000000000000000000 ) ) ;
#20249 = EDGE_LOOP ( 'NONE', ( #131931, #50261, #41231, #47102, #79541 ) ) ;
#20250 = EDGE_LOOP ( 'NONE', ( #91747, #71998, #20484, #93898 ) ) ;
#20251 = ORIENTED_EDGE ( 'NONE', *, *, #128910, .F. ) ;
#20252 = ORIENTED_EDGE ( 'NONE', *, *, #116490, .F. ) ;
#20253 = DIRECTION ( 'NONE',  ( 0.7071067811865487940, 0.7071067811865463515, -0.000000000000000000 ) ) ;
#20254 = ORIENTED_EDGE ( 'NONE', *, *, #31858, .T. ) ;
#20255 = EDGE_CURVE ( 'NONE', #36664, #121857, #1872, .T. ) ;
#20256 = ORIENTED_EDGE ( 'NONE', *, *, #56479, .F. ) ;
#20257 = DIRECTION ( 'NONE',  ( 0.7071067811865486830, -0.7071067811865464625, -0.000000000000000000 ) ) ;
#20258 = CARTESIAN_POINT ( 'NONE',  ( -20.99999999999984723, 11.96639925780213609, 5.000000000000000000 ) ) ;
#20259 = EDGE_CURVE ( 'NONE', #32784, #60759, #89648, .T. ) ;
#20260 = EDGE_CURVE ( 'NONE', #106881, #99164, #100540, .T. ) ;
#20261 = DIRECTION ( 'NONE',  ( -0.7071067811865487940, 0.7071067811865463515, -0.000000000000000000 ) ) ;
#20262 = EDGE_LOOP ( 'NONE', ( #12774, #134651, #68506, #82454 ) ) ;
#20263 = VECTOR ( 'NONE', #62738, 1000.000000000000000 ) ;
#20264 = LINE ( 'NONE', #52884, #134462 ) ;
#20265 = ORIENTED_EDGE ( 'NONE', *, *, #85066, .F. ) ;
#20266 = LINE ( 'NONE', #132663, #69942 ) ;
#20267 = LINE ( 'NONE', #64509, #58936 ) ;
#20268 = ADVANCED_FACE ( 'NONE', ( #58513 ), #123004, .F. ) ;
#20269 = CARTESIAN_POINT ( 'NONE',  ( 9.692069808101887674, -7.934999999999991616, -2.126176841940955242 ) ) ;
#20270 = ORIENTED_EDGE ( 'NONE', *, *, #137451, .F. ) ;
#20271 = CARTESIAN_POINT ( 'NONE',  ( 95.14126352523143737, 4.472830434245837594, 4.472830434245841147 ) ) ;
#20272 = ADVANCED_FACE ( 'NONE', ( #125127 ), #25820, .F. ) ;
#20273 = CARTESIAN_POINT ( 'NONE',  ( 8.129312396003866681, -8.710846131291567929, 3.794790648306943126 ) ) ;
#20274 = DIRECTION ( 'NONE',  ( 0.7071067811865487940, 0.7071067811865463515, 0.000000000000000000 ) ) ;
#20275 = DIRECTION ( 'NONE',  ( 0.7071067811865487940, 0.7071067811865463515, 0.000000000000000000 ) ) ;
#20276 = VERTEX_POINT ( 'NONE', #23681 ) ;
#20277 = ORIENTED_EDGE ( 'NONE', *, *, #115615, .F. ) ;
#20278 = CARTESIAN_POINT ( 'NONE',  ( 23.99999999999982592, 11.58746187583913390, 4.000000000000000000 ) ) ;
#20279 = ORIENTED_EDGE ( 'NONE', *, *, #39665, .T. ) ;
#20280 = CARTESIAN_POINT ( 'NONE',  ( 72.29974487139158157, -27.71228299555256669, 4.000000000000000000 ) ) ;
#20281 = LINE ( 'NONE', #50796, #16343 ) ;
#20282 = EDGE_CURVE ( 'NONE', #48369, #113729, #102688, .T. ) ;
#20283 = CARTESIAN_POINT ( 'NONE',  ( 51.48921356237309510, -27.52281430457091460, 5.000000000000000000 ) ) ;
#20284 = DIRECTION ( 'NONE',  ( 0.3543493200069162685, -0.000000000000000000, -0.9351131265310288487 ) ) ;
#20285 = EDGE_LOOP ( 'NONE', ( #60216, #140157, #51340, #139141 ) ) ;
#20286 = CARTESIAN_POINT ( 'NONE',  ( -15.29974487139158867, -27.71228299555216879, 4.000000000000000000 ) ) ;
#20287 = CARTESIAN_POINT ( 'NONE',  ( -18.48921356237309510, -27.52281430457068367, 5.000000000000000000 ) ) ;
#20288 = FACE_OUTER_BOUND ( 'NONE', #110438, .T. ) ;
#20289 = EDGE_LOOP ( 'NONE', ( #23084, #48301, #45252, #98899 ) ) ;
#20290 = DIRECTION ( 'NONE',  ( 0.000000000000000000, -1.000000000000000000, 0.000000000000000000 ) ) ;
#20291 = EDGE_CURVE ( 'NONE', #7925, #132295, #34726, .T. ) ;
#20292 = DIRECTION ( 'NONE',  ( 0.7071067811865487940, -0.7071067811865463515, 0.000000000000000000 ) ) ;
#20293 = ORIENTED_EDGE ( 'NONE', *, *, #23596, .T. ) ;
#20295 = ORIENTED_EDGE ( 'NONE', *, *, #106437, .F. ) ;
#20294 = LINE ( 'NONE', #10146, #85726 ) ;
#20296 = ORIENTED_EDGE ( 'NONE', *, *, #108090, .T. ) ;
#20297 = CARTESIAN_POINT ( 'NONE',  ( 0.000000000000000000, 0.000000000000000000, 7.950000000000000178 ) ) ;
#20299 = EDGE_CURVE ( 'NONE', #82496, #6537, #136008, .T. ) ;
#20298 = LINE ( 'NONE', #131226, #11318 ) ;
#20300 = ORIENTED_EDGE ( 'NONE', *, *, #27127, .T. ) ;
#20301 = CARTESIAN_POINT ( 'NONE',  ( 7.139999999999956160, -60.26999999999998892, -11.72188031596273206 ) ) ;
#20302 = EDGE_CURVE ( 'NONE', #24994, #6521, #14931, .T. ) ;
#20303 = FACE_OUTER_BOUND ( 'NONE', #116482, .T. ) ;
#20304 = ADVANCED_FACE ( 'NONE', ( #33863 ), #69346, .F. ) ;
#20305 = DIRECTION ( 'NONE',  ( 0.000000000000000000, -1.000000000000000000, 0.000000000000000000 ) ) ;
#20306 = CARTESIAN_POINT ( 'NONE',  ( 32.49999999999998579, 0.000000000000000000, -7.950000000000000178 ) ) ;
#20307 = CARTESIAN_POINT ( 'NONE',  ( -20.67183060077632106, -6.740707523384212863, 4.000000000000000000 ) ) ;
#20308 = DIRECTION ( 'NONE',  ( 0.7071067811865486830, -0.7071067811865464625, -0.000000000000000000 ) ) ;
#20309 = CARTESIAN_POINT ( 'NONE',  ( -33.48921356237309510, -27.52281430457078670, 5.000000000000000000 ) ) ;
#20310 = DIRECTION ( 'NONE',  ( 0.7071067811865487940, 0.7071067811865463515, -0.000000000000000000 ) ) ;
#20311 = PLANE ( 'NONE',  #92962 ) ;
#20312 = CARTESIAN_POINT ( 'NONE',  ( 26.43999999999999773, 9.521314400968980422E-16, 0.000000000000000000 ) ) ;
#20313 = EDGE_CURVE ( 'NONE', #117224, #104204, #103358, .T. ) ;
#20314 = DIRECTION ( 'NONE',  ( -0.000000000000000000, -0.3543493200069152693, 0.9351131265310292928 ) ) ;
#20315 = FACE_OUTER_BOUND ( 'NONE', #14944, .T. ) ;
#20316 = ORIENTED_EDGE ( 'NONE', *, *, #58492, .F. ) ;
#20317 = VERTEX_POINT ( 'NONE', #46187 ) ;
#20318 = ORIENTED_EDGE ( 'NONE', *, *, #37705, .F. ) ;
#20319 = CARTESIAN_POINT ( 'NONE',  ( 99.58333333333332860, 6.884901960086290629, -3.974999999999994316 ) ) ;
#20320 = VECTOR ( 'NONE', #79249, 1000.000000000000000 ) ;
#20321 = EDGE_LOOP ( 'NONE', ( #120258, #37792, #37700, #100204 ) ) ;
#20322 = ORIENTED_EDGE ( 'NONE', *, *, #31460, .F. ) ;
#20323 = ORIENTED_EDGE ( 'NONE', *, *, #83411, .T. ) ;
#20324 = LINE ( 'NONE', #140011, #121910 ) ;
#20325 = DIRECTION ( 'NONE',  ( 0.6830127018922180770, -0.6830127018922204085, -0.2588190451025213501 ) ) ;
#20326 = ORIENTED_EDGE ( 'NONE', *, *, #16731, .F. ) ;
#20327 = AXIS2_PLACEMENT_3D ( 'NONE', #48274, #61347, #136705 ) ;
#20328 = CARTESIAN_POINT ( 'NONE',  ( 0.000000000000000000, 0.000000000000000000, 0.000000000000000000 ) ) ;
#20329 = CARTESIAN_POINT ( 'NONE',  ( 25.39999999999999858, -43.14999999999999147, 40.92499999999998295 ) ) ;
#20330 = VECTOR ( 'NONE', #87994, 1000.000000000000227 ) ;
#20331 = CARTESIAN_POINT ( 'NONE',  ( -7.499999999999947597, -5.568876922607761237, 4.000000000000000000 ) ) ;
#20332 = FACE_OUTER_BOUND ( 'NONE', #7406, .T. ) ;
#20333 = CARTESIAN_POINT ( 'NONE',  ( 104.8545968585647756, -1.637169565754161615, 6.110000000000000320 ) ) ;
#20334 = VERTEX_POINT ( 'NONE', #48287 ) ;
#20335 = CARTESIAN_POINT ( 'NONE',  ( -36.18398860626899705, 28.73617430169812437, 5.000000000000000000 ) ) ;
#20336 = DIRECTION ( 'NONE',  ( -0.6830127018922180770, -0.6830127018922204085, -0.2588190451025213501 ) ) ;
#20338 = DIRECTION ( 'NONE',  ( -0.000000000000000000, -0.3543493200069152693, 0.9351131265310292928 ) ) ;
#20337 = VECTOR ( 'NONE', #137956, 1000.000000000000000 ) ;
#20339 = CARTESIAN_POINT ( 'NONE',  ( 23.47916666666666785, 6.094999999999988205, -1.633150327867694651 ) ) ;
#20340 = CARTESIAN_POINT ( 'NONE',  ( 0.1425507193225278857, -0.5999999999999994227, -3.725915899842271894 ) ) ;
#20341 = AXIS2_PLACEMENT_3D ( 'NONE', #91567, #5238, #116168 ) ;
#20342 = CARTESIAN_POINT ( 'NONE',  ( 30.85002705046288085, -5.819803920172572198, -5.819803920172572198 ) ) ;
#20343 = CARTESIAN_POINT ( 'NONE',  ( 7.139999999999989910, -35.05528132343074788, 17.90627459364450402 ) ) ;
#20344 = VERTEX_POINT ( 'NONE', #78081 ) ;
#20345 = VERTEX_POINT ( 'NONE', #57770 ) ;
#20346 = CARTESIAN_POINT ( 'NONE',  ( 30.60416666666665719, 2.130196079827422206, 7.950000000000001954 ) ) ;
#20347 = ORIENTED_EDGE ( 'NONE', *, *, #3928, .F. ) ;
#20348 = DIRECTION ( 'NONE',  ( -1.000000000000000000, -1.224606353822377258E-16, -0.000000000000000000 ) ) ;
#20349 = EDGE_CURVE ( 'NONE', #13343, #59700, #122256, .T. ) ;
#20350 = CARTESIAN_POINT ( 'NONE',  ( -34.92500000000001137, 22.22500000000000142, 4.500000000000000888 ) ) ;
#20351 = CARTESIAN_POINT ( 'NONE',  ( 11.15159235450332176, 2.500000000000001332, 0.000000000000000000 ) ) ;
#20352 = LINE ( 'NONE', #30556, #58476 ) ;
#20353 = CARTESIAN_POINT ( 'NONE',  ( 24.29974487139158867, -27.71228299555223273, 4.000000000000000000 ) ) ;
#20354 = DIRECTION ( 'NONE',  ( -0.7071067811865486830, -0.7071067811865464625, -0.000000000000000000 ) ) ;
#20355 = CARTESIAN_POINT ( 'NONE',  ( 119.9329301918981230, 1.637169565754156508, 6.110000000000000320 ) ) ;
#20356 = ORIENTED_EDGE ( 'NONE', *, *, #124443, .T. ) ;
#20357 = ORIENTED_EDGE ( 'NONE', *, *, #69861, .F. ) ;
#20358 = CARTESIAN_POINT ( 'NONE',  ( 50.99451991528749062, 28.92564299267973738, 4.000000000000000000 ) ) ;
#20359 = LINE ( 'NONE', #130602, #117201 ) ;
#20361 =( BOUNDED_CURVE ( )  B_SPLINE_CURVE ( 3, ( #134388, #123529, #24192, #69871 ),
 .UNSPECIFIED., .F., .T. ) 
 B_SPLINE_CURVE_WITH_KNOTS ( ( 4, 4 ),
 ( 0.2663372438543372689, 1.570796326794905440 ),
 .UNSPECIFIED. ) 
 CURVE ( )  GEOMETRIC_REPRESENTATION_ITEM ( )  RATIONAL_B_SPLINE_CURVE ( ( 1.000000000000000000, 0.8631550219135034618, 0.8631550219135034618, 1.000000000000000000 ) ) 
 REPRESENTATION_ITEM ( '' )  );
#20360 =( NAMED_UNIT ( * ) PLANE_ANGLE_UNIT ( ) SI_UNIT ( $, .RADIAN. ) );
#20362 = AXIS2_PLACEMENT_3D ( 'NONE', #79169, #10285, #2239 ) ;
#20363 = EDGE_CURVE ( 'NONE', #8673, #26139, #45466, .T. ) ;
#20364 = CARTESIAN_POINT ( 'NONE',  ( 17.53719725875415847, -2.055000000000000160, 0.000000000000000000 ) ) ;
#20365 = ORIENTED_EDGE ( 'NONE', *, *, #43242, .F. ) ;
#20366 = CARTESIAN_POINT ( 'NONE',  ( 45.64626352523142572, -4.472830434245840259, 4.472830434245839371 ) ) ;
#20367 = EDGE_CURVE ( 'NONE', #49145, #30768, #12076, .T. ) ;
#20368 = ORIENTED_EDGE ( 'NONE', *, *, #94592, .T. ) ;
#20369 = DIRECTION ( 'NONE',  ( 0.6830127018922180770, -0.6830127018922204085, -0.2588190451025213501 ) ) ;
#20370 = LINE ( 'NONE', #18966, #90221 ) ;
#20371 = FACE_OUTER_BOUND ( 'NONE', #90766, .T. ) ;
#20372 = VECTOR ( 'NONE', #83027, 1000.000000000000000 ) ;
#20373 = LINE ( 'NONE', #21824, #9002 ) ;
#20374 = ADVANCED_FACE ( 'NONE', ( #56361 ), #133876, .F. ) ;
#20375 = EDGE_CURVE ( 'NONE', #17766, #3015, #2623, .T. ) ;
#20376 = CARTESIAN_POINT ( 'NONE',  ( 39.14126352523145869, 4.472830434245836706, 4.472830434245840259 ) ) ;
#20377 = VERTEX_POINT ( 'NONE', #106944 ) ;
#20378 = EDGE_CURVE ( 'NONE', #110736, #26697, #72238, .T. ) ;
#20379 = CARTESIAN_POINT ( 'NONE',  ( 2.510786437626908008, -27.52281430457053446, 5.000000000000000000 ) ) ;
#20380 = ORIENTED_EDGE ( 'NONE', *, *, #56667, .T. ) ;
#20381 = ORIENTED_EDGE ( 'NONE', *, *, #14629, .F. ) ;
#20382 = ORIENTED_EDGE ( 'NONE', *, *, #66737, .T. ) ;
#20383 = EDGE_CURVE ( 'NONE', #2653, #20040, #116406, .T. ) ;
#20384 = CARTESIAN_POINT ( 'NONE',  ( -36.48921356237310221, -27.52281430457080802, 5.000000000000000000 ) ) ;
#20385 = ORIENTED_EDGE ( 'NONE', *, *, #8457, .T. ) ;
#20386 = DIRECTION ( 'NONE',  ( 0.7071067811865487940, -0.7071067811865463515, 0.000000000000000000 ) ) ;
#20387 = CARTESIAN_POINT ( 'NONE',  ( -14.29298673570684919, -21.74070752338405299, 4.999753212805220670 ) ) ;
#20388 = LINE ( 'NONE', #103998, #36684 ) ;
#20389 = EDGE_CURVE ( 'NONE', #98744, #133141, #83813, .T. ) ;
#20390 = DIRECTION ( 'NONE',  ( -0.6830127018922181881, 0.6830127018922202975, -0.2588190451025214056 ) ) ;
#20391 = FACE_BOUND ( 'NONE', #97604, .T. ) ;
#20392 = VERTEX_POINT ( 'NONE', #51158 ) ;
#20393 = FILL_AREA_STYLE_COLOUR ( '', #89656 ) ;
#20394 = LINE ( 'NONE', #64642, #431 ) ;
#20395 = DIRECTION ( 'NONE',  ( 0.7071067811865487940, 0.7071067811865463515, -0.000000000000000000 ) ) ;
#20396 = VERTEX_POINT ( 'NONE', #17094 ) ;
#20397 = CARTESIAN_POINT ( 'NONE',  ( -13.49999999999988987, 19.46639925780206326, 5.000000000000000000 ) ) ;
#20398 = ORIENTED_EDGE ( 'NONE', *, *, #9364, .T. ) ;
#20400 = VERTEX_POINT ( 'NONE', #38847 ) ;
#20399 = EDGE_CURVE ( 'NONE', #125435, #30701, #26540, .T. ) ;
#20401 = EDGE_CURVE ( 'NONE', #131359, #2907, #78530, .T. ) ;
#20402 = LINE ( 'NONE', #107431, #5409 ) ;
#20403 = ORIENTED_EDGE ( 'NONE', *, *, #127332, .T. ) ;
#20404 = CARTESIAN_POINT ( 'NONE',  ( 53.87043019189811588, -3.055000000000001492, 5.291415217122917625 ) ) ;
#20405 = EDGE_LOOP ( 'NONE', ( #119023, #141331, #94218, #17127 ) ) ;
#20406 = VECTOR ( 'NONE', #19013, 1000.000000000000000 ) ;
#20407 = LINE ( 'NONE', #8098, #2435 ) ;
#20408 = ORIENTED_EDGE ( 'NONE', *, *, #2345, .T. ) ;
#20409 = DIRECTION ( 'NONE',  ( 0.7071067811865486830, -0.7071067811865464625, -0.000000000000000000 ) ) ;
#20410 = EDGE_CURVE ( 'NONE', #53550, #55005, #105503, .T. ) ;
#20411 = VERTEX_POINT ( 'NONE', #28702 ) ;
#20412 = CARTESIAN_POINT ( 'NONE',  ( -29.99999999999978684, -9.412538124160658271, 4.000000000000000000 ) ) ;
#20413 = DIRECTION ( 'NONE',  ( 0.000000000000000000, 0.000000000000000000, 1.000000000000000000 ) ) ;
#20414 = EDGE_CURVE ( 'NONE', #98313, #62440, #38146, .T. ) ;
#20415 = FACE_OUTER_BOUND ( 'NONE', #38271, .T. ) ;
#20416 = DIRECTION ( 'NONE',  ( 0.7071067811865487940, -0.7071067811865463515, 0.000000000000000000 ) ) ;
#20417 = CARTESIAN_POINT ( 'NONE',  ( 9.707106781186483957, 11.25929247661560417, 5.000000000000000000 ) ) ;
#20418 = EDGE_CURVE ( 'NONE', #103755, #122205, #125871, .T. ) ;
#20419 = DIRECTION ( 'NONE',  ( -1.000000000000000000, -1.224606353822377258E-16, -0.000000000000000000 ) ) ;
#20420 = DIRECTION ( 'NONE',  ( 1.000000000000000000, 0.000000000000000000, 0.000000000000000000 ) ) ;
#20421 = VERTEX_POINT ( 'NONE', #106205 ) ;
#20422 = ORIENTED_EDGE ( 'NONE', *, *, #75495, .T. ) ;
#20423 = ORIENTED_EDGE ( 'NONE', *, *, #107742, .T. ) ;
#20424 = CARTESIAN_POINT ( 'NONE',  ( 19.14997294953710494, -4.461849672132299105, 4.461849672132299993 ) ) ;
#20425 = VECTOR ( 'NONE', #131693, 1000.000000000000227 ) ;
#20427 = DIRECTION ( 'NONE',  ( 0.7071067811865487940, 0.7071067811865463515, 0.000000000000000000 ) ) ;
#20426 = VECTOR ( 'NONE', #33360, 1000.000000000000000 ) ;
#20428 = VERTEX_POINT ( 'NONE', #59894 ) ;
#20429 = EDGE_CURVE ( 'NONE', #135404, #27690, #27234, .T. ) ;
#20431 = VERTEX_POINT ( 'NONE', #50445 ) ;
#20430 = VECTOR ( 'NONE', #75518, 1000.000000000000000 ) ;
#20432 = DIRECTION ( 'NONE',  ( -0.5735764363510503783, -0.8191520442889886899, 0.000000000000000000 ) ) ;
#20433 = CARTESIAN_POINT ( 'NONE',  ( 23.99451991528749062, 28.92564299267954908, 4.000000000000000000 ) ) ;
#20434 = PLANE ( 'NONE',  #57943 ) ;
#20435 = VERTEX_POINT ( 'NONE', #114930 ) ;
#20436 = DIRECTION ( 'NONE',  ( -0.6830127018922180770, -0.6830127018922204085, -0.2588190451025213501 ) ) ;
#20437 = CIRCLE ( 'NONE', #101482, 5.968999999999998529 ) ;
#20438 = AXIS2_PLACEMENT_3D ( 'NONE', #127593, #97050, #73922 ) ;
#20439 = DIRECTION ( 'NONE',  ( -0.7071067811865486830, -0.7071067811865464625, -0.000000000000000000 ) ) ;
#20440 = CARTESIAN_POINT ( 'NONE',  ( 16.25456980810188767, -6.871911579029512218, 3.967499999999996252 ) ) ;
#20441 = LINE ( 'NONE', #120445, #103977 ) ;
#20442 = VERTEX_POINT ( 'NONE', #137453 ) ;
#20443 = CARTESIAN_POINT ( 'NONE',  ( 120.0787635252314516, -7.482591942790327058E-16, 6.109999999999999432 ) ) ;
#20444 = EDGE_CURVE ( 'NONE', #55587, #100624, #94630, .T. ) ;
#20445 = CARTESIAN_POINT ( 'NONE',  ( -2.816011393730999401, 28.73617430169785436, 5.000000000000000000 ) ) ;
#20446 = DIRECTION ( 'NONE',  ( -0.000000000000000000, 0.3543493200069153248, 0.9351131265310292928 ) ) ;
#20448 = ORIENTED_EDGE ( 'NONE', *, *, #21739, .T. ) ;
#20447 = CARTESIAN_POINT ( 'NONE',  ( -2.207106781186518596, -8.240707523384196875, 5.000000000000000000 ) ) ;
#20449 = VECTOR ( 'NONE', #131406, 1000.000000000000227 ) ;
#20450 = LINE ( 'NONE', #9566, #64739 ) ;
#20451 = ORIENTED_EDGE ( 'NONE', *, *, #20255, .F. ) ;
#20452 = CARTESIAN_POINT ( 'NONE',  ( 28.49999999999980460, 1.466399257802250222, 5.000000000000000000 ) ) ;
#20453 = EDGE_CURVE ( 'NONE', #59176, #35299, #104809, .T. ) ;
#20454 = CARTESIAN_POINT ( 'NONE',  ( -6.640000000000001457, -35.14999999999999147, -40.00000000000000000 ) ) ;
#20455 = ORIENTED_EDGE ( 'NONE', *, *, #114654, .F. ) ;
#20456 = VECTOR ( 'NONE', #64380, 1000.000000000000000 ) ;
#20457 = LINE ( 'NONE', #64707, #90504 ) ;
#20458 = DIRECTION ( 'NONE',  ( -0.3543493200069162685, -0.000000000000000000, -0.9351131265310288487 ) ) ;
#20459 = VERTEX_POINT ( 'NONE', #115645 ) ;
#20460 = VECTOR ( 'NONE', #71006, 1000.000000000000000 ) ;
#20461 = DIRECTION ( 'NONE',  ( -0.6830127018922181881, 0.6830127018922202975, -0.2588190451025214056 ) ) ;
#20463 = VECTOR ( 'NONE', #111979, 1000.000000000000114 ) ;
#20462 = DIRECTION ( 'NONE',  ( 0.7071067811865486830, -0.7071067811865464625, -0.000000000000000000 ) ) ;
#20464 = ORIENTED_EDGE ( 'NONE', *, *, #32071, .F. ) ;
#20465 = VECTOR ( 'NONE', #42042, 1000.000000000000227 ) ;
#20466 = CARTESIAN_POINT ( 'NONE',  ( 4.229166666666666963, -6.094999999999989093, 1.633150327867691542 ) ) ;
#20467 = DIRECTION ( 'NONE',  ( 0.7071067811865487940, 0.7071067811865463515, 0.000000000000000000 ) ) ;
#20468 = VERTEX_POINT ( 'NONE', #49026 ) ;
#20469 = ORIENTED_EDGE ( 'NONE', *, *, #4660, .T. ) ;
#20470 = CARTESIAN_POINT ( 'NONE',  ( -5.045674110341171311E-14, -40.42999999999999261, -39.50000000000000000 ) ) ;
#20471 = DIRECTION ( 'NONE',  ( -1.000000000000000000, -0.000000000000000000, -0.000000000000000000 ) ) ;
#20472 = DIRECTION ( 'NONE',  ( -1.000000000000000000, 0.000000000000000000, 0.000000000000000000 ) ) ;
#20473 = EDGE_CURVE ( 'NONE', #118275, #6107, #82364, .T. ) ;
#20474 = DIRECTION ( 'NONE',  ( 0.7071067811865487940, 0.7071067811865463515, 0.000000000000000000 ) ) ;
#20475 = CARTESIAN_POINT ( 'NONE',  ( 0.000000000000000000, -4.600000000000055600, -28.92500000000000071 ) ) ;
#20476 = VERTEX_POINT ( 'NONE', #71480 ) ;
#20477 =( NAMED_UNIT ( * ) SI_UNIT ( $, .STERADIAN. ) SOLID_ANGLE_UNIT ( ) );
#20478 = LINE ( 'NONE', #108907, #86108 ) ;
#20479 = DIRECTION ( 'NONE',  ( 0.7071067811865487940, 0.7071067811865463515, -0.000000000000000000 ) ) ;
#20480 = AXIS2_PLACEMENT_3D ( 'NONE', #123167, #70246, #57212 ) ;
#20481 = CARTESIAN_POINT ( 'NONE',  ( 33.89126352523143737, -4.472830434245839371, -4.472830434245839371 ) ) ;
#20482 = LINE ( 'NONE', #29235, #16304 ) ;
#20483 = AXIS2_PLACEMENT_3D ( 'NONE', #135701, #80616, #15303 ) ;
#20484 = ORIENTED_EDGE ( 'NONE', *, *, #15981, .F. ) ;
#20485 = ORIENTED_EDGE ( 'NONE', *, *, #69966, .F. ) ;
#20486 = CARTESIAN_POINT ( 'NONE',  ( 5.510786437626906675, -27.52281430457051314, 5.000000000000000000 ) ) ;
#20487 = EDGE_LOOP ( 'NONE', ( #44205, #95094, #19273, #8040 ) ) ;
#20488 = VERTEX_POINT ( 'NONE', #17772 ) ;
#20489 = DIRECTION ( 'NONE',  ( 0.6830127018922180770, -0.6830127018922204085, -0.2588190451025213501 ) ) ;
#20490 = ORIENTED_EDGE ( 'NONE', *, *, #98378, .F. ) ;
#20491 = CARTESIAN_POINT ( 'NONE',  ( -55.65468426143998215, -25.33999999999998920, 15.47043909406156281 ) ) ;
#20492 = CARTESIAN_POINT ( 'NONE',  ( -16.49999999999988631, 18.43112307739199451, 4.000000000000000000 ) ) ;
#20493 = CARTESIAN_POINT ( 'NONE',  ( -33.70612307739173019, 22.22500000000000142, 4.000000000000000000 ) ) ;
#20494 = LINE ( 'NONE', #108929, #118175 ) ;
#20495 = CARTESIAN_POINT ( 'NONE',  ( 127.3129301918980900, -1.637169565754159617, -6.110000000000001208 ) ) ;
#20496 = VERTEX_POINT ( 'NONE', #16339 ) ;
#20497 = CARTESIAN_POINT ( 'NONE',  ( 4.499999999999966249, -20.53675388469230256, 2.352720554255903540 ) ) ;
#20498 = PLANE ( 'NONE',  #127878 ) ;
#20499 = DIRECTION ( 'NONE',  ( 1.000000000000000000, 0.000000000000000000, 0.000000000000000000 ) ) ;
#20500 = DIRECTION ( 'NONE',  ( 0.000000000000000000, -0.000000000000000000, 1.000000000000000000 ) ) ;
#20501 = FACE_OUTER_BOUND ( 'NONE', #5902, .T. ) ;
#20502 = CARTESIAN_POINT ( 'NONE',  ( -18.18398860626898994, 28.73617430169800002, 5.000000000000000000 ) ) ;
#20503 = DIRECTION ( 'NONE',  ( 0.000000000000000000, 1.000000000000000000, 0.000000000000000000 ) ) ;
#20504 = CARTESIAN_POINT ( 'NONE',  ( 60.45419371712955581, 6.884901960086283523, 3.975000000000002753 ) ) ;
#20505 = CARTESIAN_POINT ( 'NONE',  ( -12.69999999999998153, 0.000000000000000000, 0.000000000000000000 ) ) ;
#20506 = ORIENTED_EDGE ( 'NONE', *, *, #129606, .T. ) ;
#20507 = VERTEX_POINT ( 'NONE', #6880 ) ;
#20508 = CARTESIAN_POINT ( 'NONE',  ( 56.99999999999999289, 0.000000000000000000, -7.950000000000000178 ) ) ;
#20509 = DIRECTION ( 'NONE',  ( 1.000000000000000000, 0.000000000000000000, 0.000000000000000000 ) ) ;
#20510 = CARTESIAN_POINT ( 'NONE',  ( -21.18398860626899349, 28.73617430169802134, 5.000000000000000000 ) ) ;
#20511 = DIRECTION ( 'NONE',  ( -0.7071067811865487940, 0.7071067811865463515, -0.000000000000000000 ) ) ;
#20512 = VERTEX_POINT ( 'NONE', #139621 ) ;
#20513 = B_SPLINE_CURVE_WITH_KNOTS ( 'NONE', 3,
 ( #108404, #21450, #120003, #131645 ),
 .UNSPECIFIED., .F., .F.,
 ( 4, 4 ),
 ( 0.008519363277820954025, 0.008755597426397561736 ),
 .UNSPECIFIED. ) ;
#20514 = CARTESIAN_POINT ( 'NONE',  ( 8.999999999999932498, -11.35517001088071787, -1.126524801160087241 ) ) ;
#20515 = CARTESIAN_POINT ( 'NONE',  ( -18.51665438641032679, 22.22500000000000142, 4.500000000000000888 ) ) ;
#20516 = CARTESIAN_POINT ( 'NONE',  ( 50.89626352523143993, 4.472830434245840259, -4.472830434245839371 ) ) ;
#20517 = ORIENTED_EDGE ( 'NONE', *, *, #9344, .F. ) ;
#20518 = EDGE_CURVE ( 'NONE', #35500, #46353, #40302, .T. ) ;
#20519 = ADVANCED_FACE ( 'NONE', ( #5469 ), #29377, .F. ) ;
#20520 = CARTESIAN_POINT ( 'NONE',  ( 15.68879807097514956, -1.757674993583058898, 4.000000000000000000 ) ) ;
#20521 = ORIENTED_EDGE ( 'NONE', *, *, #100711, .T. ) ;
#20522 = ORIENTED_EDGE ( 'NONE', *, *, #46730, .F. ) ;
#20523 = FACE_OUTER_BOUND ( 'NONE', #77765, .T. ) ;
#20524 = AXIS2_PLACEMENT_3D ( 'NONE', #38316, #18665, #62941 ) ;
#20525 = VECTOR ( 'NONE', #38432, 1000.000000000000000 ) ;
#20526 = DIRECTION ( 'NONE',  ( -0.7071067811865486830, 0.7071067811865464625, 0.000000000000000000 ) ) ;
#20527 = LINE ( 'NONE', #51775, #60538 ) ;
#20528 = ADVANCED_FACE ( 'NONE', ( #120661 ), #106152, .T. ) ;
#20529 = FACE_OUTER_BOUND ( 'NONE', #37565, .T. ) ;
#20530 = VERTEX_POINT ( 'NONE', #42446 ) ;
#20531 = CARTESIAN_POINT ( 'NONE',  ( 6.066782984417857350, 4.584330080086930965E-16, 0.000000000000000000 ) ) ;
#20532 = ADVANCED_FACE ( 'NONE', ( #107655 ), #98915, .F. ) ;
#20533 = EDGE_CURVE ( 'NONE', #10965, #86617, #22069, .T. ) ;
#20535 = VERTEX_POINT ( 'NONE', #141748 ) ;
#20534 = CARTESIAN_POINT ( 'NONE',  ( 9.379139616203772789, -5.278424836066145431, -3.047499999999993658 ) ) ;
#20536 = CARTESIAN_POINT ( 'NONE',  ( 84.58376352523144703, -6.110000000000001208, -3.741295971395164515E-16 ) ) ;
#20537 = DIRECTION ( 'NONE',  ( 1.000000000000000000, 1.224606353822377258E-16, 0.000000000000000000 ) ) ;
#20538 = DIRECTION ( 'NONE',  ( -0.6830127018922181881, 0.6830127018922202975, -0.2588190451025214056 ) ) ;
#20539 = DIRECTION ( 'NONE',  ( 0.7071067811865487940, -0.7071067811865463515, 0.000000000000000000 ) ) ;
#20541 = DIRECTION ( 'NONE',  ( 0.6830127018922180770, -0.6830127018922204085, -0.2588190451025213501 ) ) ;
#20540 = CIRCLE ( 'NONE', #6319, 2.500000000000000888 ) ;
#20542 = LINE ( 'NONE', #41599, #92549 ) ;
#20543 = AXIS2_PLACEMENT_3D ( 'NONE', #69934, #134447, #80086 ) ;
#20544 = EDGE_CURVE ( 'NONE', #40999, #106934, #94174, .T. ) ;
#20545 = EDGE_CURVE ( 'NONE', #93784, #20276, #4285, .T. ) ;
#20546 = ORIENTED_EDGE ( 'NONE', *, *, #56137, .F. ) ;
#20547 = CARTESIAN_POINT ( 'NONE',  ( 70.64126352523145158, 4.472830434245836706, 4.472830434245840259 ) ) ;
#20548 = CARTESIAN_POINT ( 'NONE',  ( 12.71159235450332048, 9.902892378096218942E-16, 0.000000000000000000 ) ) ;
#20549 = EDGE_CURVE ( 'NONE', #28258, #75489, #11166, .T. ) ;
#20550 = CARTESIAN_POINT ( 'NONE',  ( -6.005480084712508493, 28.92564299267933947, 4.000000000000000000 ) ) ;
#20551 = CARTESIAN_POINT ( 'NONE',  ( -39.48921356237310221, -27.52281430457082934, 5.000000000000000000 ) ) ;
#20552 = ORIENTED_EDGE ( 'NONE', *, *, #12926, .T. ) ;
#20553 = ORIENTED_EDGE ( 'NONE', *, *, #79910, .T. ) ;
#20554 = VECTOR ( 'NONE', #122472, 1000.000000000000000 ) ;
#20555 = EDGE_CURVE ( 'NONE', #31876, #60798, #65642, .T. ) ;
#20556 = DIRECTION ( 'NONE',  ( -1.000000000000000000, -0.000000000000000000, -0.000000000000000000 ) ) ;
#20557 = LINE ( 'NONE', #64813, #70055 ) ;
#20558 = EDGE_LOOP ( 'NONE', ( #52405, #95987, #46902, #57347 ) ) ;
#20559 = EDGE_CURVE ( 'NONE', #23712, #8256, #29810, .T. ) ;
#20560 = ORIENTED_EDGE ( 'NONE', *, *, #96696, .F. ) ;
#20561 = VECTOR ( 'NONE', #9066, 1000.000000000000000 ) ;
#20562 = CARTESIAN_POINT ( 'NONE',  ( 31.82816939922330945, -8.240707523384191546, 4.000000000000000000 ) ) ;
#20563 = VERTEX_POINT ( 'NONE', #96747 ) ;
#20564 = DIRECTION ( 'NONE',  ( -0.7071067811865486830, -0.7071067811865464625, 0.000000000000000000 ) ) ;
#20565 = CARTESIAN_POINT ( 'NONE',  ( -8.688897854252501031E-13, 0.5999999999999986455, 3.228722604634024940 ) ) ;
#20566 = VECTOR ( 'NONE', #132712, 1000.000000000000000 ) ;
#20567 = VECTOR ( 'NONE', #127347, 1000.000000000000000 ) ;
#20568 = AXIS2_PLACEMENT_3D ( 'NONE', #11366, #23713, #12817 ) ;
#20569 = EDGE_CURVE ( 'NONE', #48401, #9427, #40988, .T. ) ;
#20571 = VECTOR ( 'NONE', #97690, 1000.000000000000000 ) ;
#20570 = CARTESIAN_POINT ( 'NONE',  ( 39.48921356237310221, -27.52281430457082934, 5.000000000000000000 ) ) ;
#20572 = FACE_BOUND ( 'NONE', #60605, .T. ) ;
#20573 = LINE ( 'NONE', #85129, #121928 ) ;
#20574 = DIRECTION ( 'NONE',  ( -1.000000000000000000, 2.310445909535201824E-14, 0.000000000000000000 ) ) ;
#20575 = CARTESIAN_POINT ( 'NONE',  ( 16.44013779566152778, 2.499999999999998224, 3.061616997868380183E-16 ) ) ;
#20577 = EDGE_LOOP ( 'NONE', ( #89543, #29638, #135775, #99379 ) ) ;
#20576 = DIRECTION ( 'NONE',  ( 0.7071067811865486830, -0.7071067811865464625, -0.000000000000000000 ) ) ;
#20578 = EDGE_CURVE ( 'NONE', #21546, #62052, #124712, .T. ) ;
#20579 = VECTOR ( 'NONE', #59878, 1000.000000000000227 ) ;
#20580 = DIRECTION ( 'NONE',  ( -0.7071067811865486830, -0.7071067811865464625, -0.000000000000000000 ) ) ;
#20581 = ITEM_DEFINED_TRANSFORMATION ( 'NONE', 'NONE', #123437,  #127880 ) ;
#20582 = VERTEX_POINT ( 'NONE', #108337 ) ;
#20583 = EDGE_LOOP ( 'NONE', ( #92176, #135819, #5486, #35988 ) ) ;
#20584 = CARTESIAN_POINT ( 'NONE',  ( 86.68293019189812298, -1.637169565754158951, -6.109999999999998543 ) ) ;
#20585 = ORIENTED_EDGE ( 'NONE', *, *, #9944, .F. ) ;
#20586 = CARTESIAN_POINT ( 'NONE',  ( -48.48921356237309510, -27.52281430457089328, 5.000000000000000000 ) ) ;
#20587 = EDGE_CURVE ( 'NONE', #138203, #137069, #121388, .T. ) ;
#20588 = ORIENTED_EDGE ( 'NONE', *, *, #77123, .T. ) ;
#20589 = LINE ( 'NONE', #8266, #99962 ) ;
#20590 = VECTOR ( 'NONE', #92318, 1000.000000000000000 ) ;
#20591 = LINE ( 'NONE', #108288, #5441 ) ;
#20592 = EDGE_CURVE ( 'NONE', #90110, #32128, #129408, .T. ) ;
#20593 = DIRECTION ( 'NONE',  ( 1.000000000000000000, 0.000000000000000000, 0.000000000000000000 ) ) ;
#20594 = CARTESIAN_POINT ( 'NONE',  ( -18.48921356237309510, -27.52281430457068367, 5.000000000000000000 ) ) ;
#20595 = DIRECTION ( 'NONE',  ( -0.000000000000000000, 0.3543493200069153248, 0.9351131265310292928 ) ) ;
#20596 = EDGE_CURVE ( 'NONE', #116174, #41627, #54734, .T. ) ;
#20597 = DIRECTION ( 'NONE',  ( 0.7071067811865486830, -0.7071067811865464625, -0.000000000000000000 ) ) ;
#20598 = CARTESIAN_POINT ( 'NONE',  ( -74.99451991528749772, 28.92564299267990435, 4.000000000000000000 ) ) ;
#20599 = VERTEX_POINT ( 'NONE', #85185 ) ;
#20600 = CARTESIAN_POINT ( 'NONE',  ( -19.93618820137057668, -0.2700000000508183118, -36.99999999997771738 ) ) ;
#20601 = ORIENTED_EDGE ( 'NONE', *, *, #33616, .T. ) ;
#20602 = DIRECTION ( 'NONE',  ( -0.6830127018922180770, -0.6830127018922204085, -0.2588190451025213501 ) ) ;
#20603 = EDGE_CURVE ( 'NONE', #130004, #1441, #20643, .T. ) ;
#20604 = CARTESIAN_POINT ( 'NONE',  ( -3.299744871391591339, -27.71228299555208352, 4.000000000000000000 ) ) ;
#20605 = EDGE_CURVE ( 'NONE', #115095, #79885, #108522, .T. ) ;
#20606 = ORIENTED_EDGE ( 'NONE', *, *, #71520, .T. ) ;
#20607 = EDGE_LOOP ( 'NONE', ( #30855, #95117, #128674, #48057 ) ) ;
#20608 = EDGE_LOOP ( 'NONE', ( #140635, #95346, #87197, #25133, #131366 ) ) ;
#20609 = CARTESIAN_POINT ( 'NONE',  ( 38.79209685856477563, -5.291415217122921177, 3.054999999999999272 ) ) ;
#20610 = VERTEX_POINT ( 'NONE', #97487 ) ;
#20611 = CARTESIAN_POINT ( 'NONE',  ( 46.06249999999999289, -5.819803920172573086, -5.819803920172573974 ) ) ;
#20612 = ADVANCED_FACE ( 'NONE', ( #64897 ), #140299, .F. ) ;
#20613 = LINE ( 'NONE', #77188, #123434 ) ;
#20614 = CARTESIAN_POINT ( 'NONE',  ( 25.71247294953710849, 0.000000000000000000, 6.094999999999989981 ) ) ;
#20615 = CARTESIAN_POINT ( 'NONE',  ( 8.706187397278121409, 10.29068361123369080, -28.65696959968947866 ) ) ;
#20616 = VERTEX_POINT ( 'NONE', #98231 ) ;
#20617 = EDGE_CURVE ( 'NONE', #42725, #55653, #142455, .T. ) ;
#20618 = DIRECTION ( 'NONE',  ( 0.7071067811865487940, 0.7071067811865463515, 0.000000000000000000 ) ) ;
#20619 = EDGE_LOOP ( 'NONE', ( #24510, #60680, #80621, #105849 ) ) ;
#20620 = PRESENTATION_STYLE_ASSIGNMENT (( #54014 ) ) ;
#20621 = CARTESIAN_POINT ( 'NONE',  ( -21.48921356237309155, -27.52281430457070499, 5.000000000000000000 ) ) ;
#20623 = ORIENTED_EDGE ( 'NONE', *, *, #125511, .F. ) ;
#20622 = DIRECTION ( 'NONE',  ( -0.000000000000000000, -0.3543493200069152693, 0.9351131265310292928 ) ) ;
#20624 = EDGE_LOOP ( 'NONE', ( #17204, #38842, #85294 ) ) ;
#20625 = CARTESIAN_POINT ( 'NONE',  ( 57.48921356237308800, -27.52281430457095368, 5.000000000000000000 ) ) ;
#20626 = DIRECTION ( 'NONE',  ( -1.000000000000000000, -0.000000000000000000, 0.000000000000000000 ) ) ;
#20627 = CARTESIAN_POINT ( 'NONE',  ( 33.51665438641022376, 22.22500000000000142, 4.500000000000000888 ) ) ;
#20628 = VERTEX_POINT ( 'NONE', #57599 ) ;
#20629 = CARTESIAN_POINT ( 'NONE',  ( -34.82816939922328459, 18.75929247661553134, 4.000000000000000000 ) ) ;
#20630 = ORIENTED_EDGE ( 'NONE', *, *, #29720, .T. ) ;
#20631 = ORIENTED_EDGE ( 'NONE', *, *, #117298, .F. ) ;
#20632 = VERTEX_POINT ( 'NONE', #101786 ) ;
#20633 = DIRECTION ( 'NONE',  ( -0.000000000000000000, -0.3543493200069152693, 0.9351131265310292928 ) ) ;
#20634 = CARTESIAN_POINT ( 'NONE',  ( 2.999999999999999112, -47.62213595499956398, -36.92499999999996874 ) ) ;
#20635 = AXIS2_PLACEMENT_3D ( 'NONE', #124380, #69299, #62003 ) ;
#20636 = VECTOR ( 'NONE', #27086, 1000.000000000000227 ) ;
#20637 = VECTOR ( 'NONE', #48203, 999.9999999999998863 ) ;
#20638 = LINE ( 'NONE', #119930, #90108 ) ;
#20639 = LINE ( 'NONE', #141745, #134807 ) ;
#20640 = AXIS2_PLACEMENT_3D ( 'NONE', #137578, #91242, #79678 ) ;
#20641 = DIRECTION ( 'NONE',  ( -0.7071067811865486830, -0.7071067811865464625, 0.000000000000000000 ) ) ;
#20642 = EDGE_CURVE ( 'NONE', #20115, #3959, #34395, .T. ) ;
#20643 = LINE ( 'NONE', #33005, #140946 ) ;
#20644 = ORIENTED_EDGE ( 'NONE', *, *, #68373, .F. ) ;
#20646 = EDGE_CURVE ( 'NONE', #103659, #126053, #46757, .T. ) ;
#20645 = FACE_OUTER_BOUND ( 'NONE', #4714, .T. ) ;
#20647 = VERTEX_POINT ( 'NONE', #135167 ) ;
#20648 = VECTOR ( 'NONE', #85567, 1000.000000000000227 ) ;
#20649 = LINE ( 'NONE', #87358, #70312 ) ;
#20650 = DIRECTION ( 'NONE',  ( -0.7071067811865487940, 0.7071067811865463515, 0.000000000000000000 ) ) ;
#20651 = ORIENTED_EDGE ( 'NONE', *, *, #109350, .F. ) ;
#20652 = LINE ( 'NONE', #96069, #34423 ) ;
#20653 = PLANE ( 'NONE',  #109207 ) ;
#20654 = ORIENTED_EDGE ( 'NONE', *, *, #3760, .F. ) ;
#20655 = ORIENTED_EDGE ( 'NONE', *, *, #100375, .F. ) ;
#20656 = DIRECTION ( 'NONE',  ( 0.3543493200069162685, -0.000000000000000000, -0.9351131265310288487 ) ) ;
#20657 = CARTESIAN_POINT ( 'NONE',  ( -29.20666063542132207, 21.75929247661549226, 4.998822639870711626 ) ) ;
#20658 = PLANE ( 'NONE',  #84027 ) ;
#20659 = AXIS2_PLACEMENT_3D ( 'NONE', #68678, #70823, #104104 ) ;
#20660 = CONICAL_SURFACE ( 'NONE', #101702, 2.500000000000000444, 0.9599310885968830309 ) ;
#20661 =( NAMED_UNIT ( * ) SI_UNIT ( $, .STERADIAN. ) SOLID_ANGLE_UNIT ( ) );
#20662 = PLANE ( 'NONE',  #25045 ) ;
#20663 = CARTESIAN_POINT ( 'NONE',  ( 65.09959685856478018, -6.109999999999998543, -1.637169565754160727 ) ) ;
#20664 = EDGE_CURVE ( 'NONE', #125758, #97364, #122096, .T. ) ;
#20665 = FACE_OUTER_BOUND ( 'NONE', #28382, .T. ) ;
#20667 = PLANE ( 'NONE',  #53061 ) ;
#20666 = VECTOR ( 'NONE', #120523, 1000.000000000000000 ) ;
#20668 = EDGE_CURVE ( 'NONE', #123227, #3179, #35863, .T. ) ;
#20669 = FACE_OUTER_BOUND ( 'NONE', #62637, .T. ) ;
#20670 = DIRECTION ( 'NONE',  ( 0.000000000000000000, 0.000000000000000000, 1.000000000000000000 ) ) ;
#20671 = VERTEX_POINT ( 'NONE', #80079 ) ;
#20672 = DIRECTION ( 'NONE',  ( 0.000000000000000000, -1.000000000000000000, -9.130123557772669567E-17 ) ) ;
#20673 = EDGE_LOOP ( 'NONE', ( #115253, #55507, #37706, #39695 ) ) ;
#20674 = CARTESIAN_POINT ( 'NONE',  ( -6.183988606268994381, 28.73617430169791476, 5.000000000000000000 ) ) ;
#20675 = PLANE ( 'NONE',  #98505 ) ;
#20676 = ORIENTED_EDGE ( 'NONE', *, *, #20244, .F. ) ;
#20677 = AXIS2_PLACEMENT_3D ( 'NONE', #130612, #41425, #97201 ) ;
#20678 = AXIS2_PLACEMENT_3D ( 'NONE', #67814, #142488, #112002 ) ;
#20679 = VECTOR ( 'NONE', #21405, 1000.000000000000000 ) ;
#20680 = DIRECTION ( 'NONE',  ( -0.7071067811865487940, 0.7071067811865463515, -0.000000000000000000 ) ) ;
#20682 = VERTEX_POINT ( 'NONE', #102529 ) ;
#20681 = FACE_OUTER_BOUND ( 'NONE', #67045, .T. ) ;
#20683 = CARTESIAN_POINT ( 'NONE',  ( 0.2569208697893813897, 0.3999999999999995781, 2.015694669338588429 ) ) ;
#20684 = EDGE_CURVE ( 'NONE', #2974, #44911, #79377, .T. ) ;
#20685 = DIRECTION ( 'NONE',  ( -0.5735764363510499342, -0.8191520442889891340, 0.000000000000000000 ) ) ;
#20686 = CARTESIAN_POINT ( 'NONE',  ( -45.18398860626900415, 28.73617430169818832, 5.000000000000000000 ) ) ;
#20687 = ORIENTED_EDGE ( 'NONE', *, *, #128065, .F. ) ;
#20688 = ORIENTED_EDGE ( 'NONE', *, *, #119837, .T. ) ;
#20689 = DIRECTION ( 'NONE',  ( -0.000000000000000000, -0.3543493200069152693, 0.9351131265310292928 ) ) ;
#20690 = DIRECTION ( 'NONE',  ( -1.000000000000000000, -1.224606353822377258E-16, -0.000000000000000000 ) ) ;
#20691 = VECTOR ( 'NONE', #141971, 999.9999999999998863 ) ;
#20692 = VECTOR ( 'NONE', #97494, 1000.000000000000227 ) ;
#20693 = DIRECTION ( 'NONE',  ( -0.7071067811865487940, 0.7071067811865463515, 0.000000000000000000 ) ) ;
#20694 = DIRECTION ( 'NONE',  ( -1.000000000000000000, 0.000000000000000000, -0.000000000000000000 ) ) ;
#20695 = CARTESIAN_POINT ( 'NONE',  ( 87.87086038379622721, 6.884901960086289741, -3.974999999999993427 ) ) ;
#20696 = FACE_OUTER_BOUND ( 'NONE', #18329, .T. ) ;
#20697 = CARTESIAN_POINT ( 'NONE',  ( 3.250000000000000000, 4.999999999999997335, -7.627214432543508948 ) ) ;
#20698 = ORIENTED_EDGE ( 'NONE', *, *, #61850, .T. ) ;
#20699 = CARTESIAN_POINT ( 'NONE',  ( -78.29974487139158157, -27.71228299555260577, 4.000000000000000000 ) ) ;
#20700 = DIRECTION ( 'NONE',  ( 0.6830127018922180770, -0.6830127018922204085, -0.2588190451025213501 ) ) ;
#20701 = CARTESIAN_POINT ( 'NONE',  ( 34.70833333333333570, 3.047499999999997655, 5.278424836066143655 ) ) ;
#20702 = VECTOR ( 'NONE', #131401, 1000.000000000000000 ) ;
#20703 = ORIENTED_EDGE ( 'NONE', *, *, #33250, .F. ) ;
#20704 = CARTESIAN_POINT ( 'NONE',  ( -0.000000000000000000, 22.27000000000000668, 0.000000000000000000 ) ) ;
#20705 = ORIENTED_EDGE ( 'NONE', *, *, #110949, .F. ) ;
#20706 = CARTESIAN_POINT ( 'NONE',  ( 72.18793019189810423, 6.110000000000002984, -1.637169565754156730 ) ) ;
#20707 = CARTESIAN_POINT ( 'NONE',  ( 0.000000000000000000, -43.14999999999999147, 40.92499999999998295 ) ) ;
#20708 = EDGE_CURVE ( 'NONE', #73712, #56655, #124255, .T. ) ;
#20709 = LINE ( 'NONE', #86713, #135027 ) ;
#20710 = ORIENTED_EDGE ( 'NONE', *, *, #85678, .F. ) ;
#20711 = CARTESIAN_POINT ( 'NONE',  ( 2.999999999999999112, -1.600000000000060929, 28.92500000000001847 ) ) ;
#20712 = DIRECTION ( 'NONE',  ( 0.7071067811865487940, -0.7071067811865463515, 0.000000000000000000 ) ) ;
#20713 = CARTESIAN_POINT ( 'NONE',  ( 39.48921356237310221, -27.52281430457082934, 5.000000000000000000 ) ) ;
#20714 = CARTESIAN_POINT ( 'NONE',  ( 0.1161069444170879233, -2.256103126841972450, 0.000000000000000000 ) ) ;
#20715 = EDGE_CURVE ( 'NONE', #115411, #63259, #67030, .T. ) ;
#20717 = ORIENTED_EDGE ( 'NONE', *, *, #112141, .F. ) ;
#20716 = CARTESIAN_POINT ( 'NONE',  ( -51.48921356237309510, -27.52281430457091460, 5.000000000000000000 ) ) ;
#20718 = FACE_OUTER_BOUND ( 'NONE', #104599, .T. ) ;
#20719 = CARTESIAN_POINT ( 'NONE',  ( 6.995075227788017713, -5.240707523384232402, 12.38332538355494172 ) ) ;
#20720 = CARTESIAN_POINT ( 'NONE',  ( 23.36654548503486950, 7.297668562427137573, 4.000000000000000000 ) ) ;
#20721 = CARTESIAN_POINT ( 'NONE',  ( 24.39999999999999858, -7.600000000000055600, -28.92499999999998650 ) ) ;
#20722 = EDGE_LOOP ( 'NONE', ( #37945, #88592, #43529, #2790 ) ) ;
#20724 = ORIENTED_EDGE ( 'NONE', *, *, #141367, .T. ) ;
#20723 = EDGE_CURVE ( 'NONE', #78949, #62812, #2038, .T. ) ;
#20725 = EDGE_CURVE ( 'NONE', #121857, #25213, #69179, .T. ) ;
#20726 = CARTESIAN_POINT ( 'NONE',  ( 61.68793019189811844, 6.110000000000002984, -1.637169565754156730 ) ) ;
#20727 = EDGE_LOOP ( 'NONE', ( #61146, #115564, #60193, #46760, #60390, #55987 ) ) ;
#20728 = EDGE_CURVE ( 'NONE', #69796, #18367, #80771, .T. ) ;
#20729 = DIRECTION ( 'NONE',  ( -0.7071067811865487940, 0.7071067811865463515, 0.000000000000000000 ) ) ;
#20730 = CARTESIAN_POINT ( 'NONE',  ( 48.29974487139158867, -27.71228299555239971, 4.000000000000000000 ) ) ;
#20731 = EDGE_CURVE ( 'NONE', #63490, #29342, #43686, .T. ) ;
#20732 = LINE ( 'NONE', #20010, #126726 ) ;
#20733 = DIRECTION ( 'NONE',  ( -1.000000000000000000, 0.000000000000000000, 0.000000000000000000 ) ) ;
#20734 = VERTEX_POINT ( 'NONE', #122831 ) ;
#20735 = EDGE_CURVE ( 'NONE', #29818, #67807, #1715, .T. ) ;
#20736 = CARTESIAN_POINT ( 'NONE',  ( 6.005480084712508493, 28.92564299267933947, 4.000000000000000000 ) ) ;
#20737 = EDGE_CURVE ( 'NONE', #116339, #96152, #69924, .T. ) ;
#20738 = ORIENTED_EDGE ( 'NONE', *, *, #73571, .T. ) ;
#20739 = EDGE_CURVE ( 'NONE', #119532, #139613, #55443, .T. ) ;
#20740 = DIRECTION ( 'NONE',  ( -0.000000000000000000, 1.000000000000000000, -0.000000000000000000 ) ) ;
#20741 = DIRECTION ( 'NONE',  ( 0.000000000000000000, -1.000000000000000000, 0.000000000000000000 ) ) ;
#20742 = AXIS2_PLACEMENT_3D ( 'NONE', #53065, #32048, #108144 ) ;
#20743 = AXIS2_PLACEMENT_3D ( 'NONE', #28709, #137460, #72953 ) ;
#20744 = VECTOR ( 'NONE', #41240, 1000.000000000000000 ) ;
#20745 = EDGE_LOOP ( 'NONE', ( #113299, #123864, #16675, #22529 ) ) ;
#20746 = ORIENTED_EDGE ( 'NONE', *, *, #82795, .F. ) ;
#20747 = AXIS2_PLACEMENT_3D ( 'NONE', #69876, #23466, #122779 ) ;
#20748 = EDGE_CURVE ( 'NONE', #140112, #55587, #302, .T. ) ;
#20749 = EDGE_CURVE ( 'NONE', #75175, #23274, #44604, .T. ) ;
#20750 = DIRECTION ( 'NONE',  ( -0.7071067811865486830, 0.7071067811865464625, 0.000000000000000000 ) ) ;
#20751 = CARTESIAN_POINT ( 'NONE',  ( 181.1500000000000057, -47.62213595499959951, 36.92500000000000426 ) ) ;
#20752 = CARTESIAN_POINT ( 'NONE',  ( 26.99999999999981881, 11.96639925780213609, 5.000000000000000000 ) ) ;
#20753 = CIRCLE ( 'NONE', #50897, 6.349999999999997868 ) ;
#20754 = CARTESIAN_POINT ( 'NONE',  ( -25.25154412867560438, -11.24070752338416845, 10.39518518046015139 ) ) ;
#20755 = EDGE_CURVE ( 'NONE', #30838, #28258, #1024, .T. ) ;
#20756 = CARTESIAN_POINT ( 'NONE',  ( 23.99999999999983302, -8.731860332648819778, -2.120594902707481744 ) ) ;
#20757 = ORIENTED_EDGE ( 'NONE', *, *, #35026, .F. ) ;
#20758 = VECTOR ( 'NONE', #121912, 1000.000000000000227 ) ;
#20759 = ORIENTED_EDGE ( 'NONE', *, *, #131723, .T. ) ;
#20760 = CARTESIAN_POINT ( 'NONE',  ( 108.5579301918981088, 6.110000000000000320, -1.637169565754156064 ) ) ;
#20761 = EDGE_LOOP ( 'NONE', ( #17221, #59005, #20837, #80904 ) ) ;
#20762 = ORIENTED_EDGE ( 'NONE', *, *, #87695, .T. ) ;
#20763 = CIRCLE ( 'NONE', #101803, 5.968999999999998529 ) ;
#20764 = AXIS2_PLACEMENT_3D ( 'NONE', #9249, #131084, #86157 ) ;
#20765 = CARTESIAN_POINT ( 'NONE',  ( 183.3316408629057719, -49.14999999999998437, 41.64499999999997470 ) ) ;
#20766 =( BOUNDED_CURVE ( )  B_SPLINE_CURVE ( 3, ( #96364, #52179, #28306, #140606 ),
 .UNSPECIFIED., .F., .F. ) 
 B_SPLINE_CURVE_WITH_KNOTS ( ( 4, 4 ),
 ( 4.350170835173037709, 4.500739107949217832 ),
 .UNSPECIFIED. ) 
 CURVE ( )  GEOMETRIC_REPRESENTATION_ITEM ( )  RATIONAL_B_SPLINE_CURVE ( ( 1.000000000000000000, 0.9981116584018958626, 0.9981116584018958626, 1.000000000000000000 ) ) 
 REPRESENTATION_ITEM ( '' )  );
#20767 = CARTESIAN_POINT ( 'NONE',  ( -5.510786437626906675, -27.52281430457051314, 5.000000000000000000 ) ) ;
#20768 = AXIS2_PLACEMENT_3D ( 'NONE', #66555, #128431, #29104 ) ;
#20769 = LINE ( 'NONE', #65022, #26290 ) ;
#20770 = ORIENTED_EDGE ( 'NONE', *, *, #118824, .F. ) ;
#20771 = DIRECTION ( 'NONE',  ( -0.000000000000000000, -0.3543493200069152693, 0.9351131265310292928 ) ) ;
#20772 = DIRECTION ( 'NONE',  ( 0.7071067811865487940, -0.7071067811865463515, 0.000000000000000000 ) ) ;
#20773 = PLANE ( 'NONE',  #29612 ) ;
#20774 = EDGE_CURVE ( 'NONE', #97401, #17549, #45306, .T. ) ;
#20775 = CARTESIAN_POINT ( 'NONE',  ( 2.233306282870438864, -6.094999999999989981, -1.633150327867689322 ) ) ;
#20776 = VECTOR ( 'NONE', #42889, 1000.000000000000227 ) ;
#20777 = LINE ( 'NONE', #9143, #49149 ) ;
#20778 = ORIENTED_EDGE ( 'NONE', *, *, #84282, .F. ) ;
#20779 = LINE ( 'NONE', #74484, #17135 ) ;
#20780 = CARTESIAN_POINT ( 'NONE',  ( 50.72916666666665719, 7.950000000000001954, -2.130196079827421762 ) ) ;
#20781 = VECTOR ( 'NONE', #57996, 1000.000000000000000 ) ;
#20782 = EDGE_LOOP ( 'NONE', ( #87112, #13999, #31338, #112756 ) ) ;
#20783 = ORIENTED_EDGE ( 'NONE', *, *, #129091, .F. ) ;
#20784 = AXIS2_PLACEMENT_3D ( 'NONE', #76998, #102309, #2955 ) ;
#20785 = ORIENTED_EDGE ( 'NONE', *, *, #7200, .F. ) ;
#20787 = VECTOR ( 'NONE', #2492, 1000.000000000000000 ) ;
#20786 = CARTESIAN_POINT ( 'NONE',  ( 59.20876352523143993, -7.482591942790329030E-16, 6.110000000000001208 ) ) ;
#20788 = VERTEX_POINT ( 'NONE', #35135 ) ;
#20789 = EDGE_CURVE ( 'NONE', #54960, #44135, #89481, .T. ) ;
#20790 = DIRECTION ( 'NONE',  ( 0.6830127018922180770, -0.6830127018922204085, -0.2588190451025213501 ) ) ;
#20791 = CARTESIAN_POINT ( 'NONE',  ( -18.18398860626898994, 28.73617430169800002, 5.000000000000000000 ) ) ;
#20792 = CARTESIAN_POINT ( 'NONE',  ( 99.31293019189810423, -1.637169565754159617, -6.110000000000001208 ) ) ;
#20793 = CARTESIAN_POINT ( 'NONE',  ( -63.48921356237309510, -27.52281430457099631, 5.000000000000000000 ) ) ;
#20794 = EDGE_CURVE ( 'NONE', #78146, #98048, #59739, .T. ) ;
#20796 = CARTESIAN_POINT ( 'NONE',  ( 21.76000000000000156, -2.055000000000000160, 0.000000000000000000 ) ) ;
#20795 = CARTESIAN_POINT ( 'NONE',  ( 0.07735795229993543132, 0.4000000000000001332, -2.152165010376131171 ) ) ;
#20797 = ORIENTED_EDGE ( 'NONE', *, *, #60978, .F. ) ;
#20798 = CARTESIAN_POINT ( 'NONE',  ( 4.499999999999972466, 8.900465351122155866, -2.516491619111523192 ) ) ;
#20799 = AXIS2_PLACEMENT_3D ( 'NONE', #78290, #122476, #23150 ) ;
#20800 = CARTESIAN_POINT ( 'NONE',  ( 15.27825451568563864, 8.259292476615637923, 11.78515199841153738 ) ) ;
#20801 = LINE ( 'NONE', #62920, #67662 ) ;
#20802 = DIRECTION ( 'NONE',  ( 0.6830127018922181881, 0.6830127018922202975, -0.2588190451025214056 ) ) ;
#20803 = VERTEX_POINT ( 'NONE', #61879 ) ;
#20804 = EDGE_CURVE ( 'NONE', #56431, #98546, #104638, .T. ) ;
#20805 = ORIENTED_EDGE ( 'NONE', *, *, #90278, .F. ) ;
#20806 = ORIENTED_EDGE ( 'NONE', *, *, #131462, .T. ) ;
#20807 = ORIENTED_EDGE ( 'NONE', *, *, #129401, .F. ) ;
#20808 = CARTESIAN_POINT ( 'NONE',  ( 121.3912635252314374, -4.472830434245838482, -4.472830434245838482 ) ) ;
#20809 = ORIENTED_EDGE ( 'NONE', *, *, #28124, .F. ) ;
#20810 = VECTOR ( 'NONE', #119049, 1000.000000000000000 ) ;
#20811 = CARTESIAN_POINT ( 'NONE',  ( -12.29974487139158512, -27.71228299555214747, 4.000000000000000000 ) ) ;
#20812 = EDGE_CURVE ( 'NONE', #14007, #142960, #136545, .T. ) ;
#20813 = CARTESIAN_POINT ( 'NONE',  ( 0.000000000000000000, 0.000000000000000000, 5.000000000000000000 ) ) ;
#20814 = ORIENTED_EDGE ( 'NONE', *, *, #7771, .T. ) ;
#20815 = DIRECTION ( 'NONE',  ( 0.7071067811865487940, 0.7071067811865463515, -0.000000000000000000 ) ) ;
#20816 = ORIENTED_EDGE ( 'NONE', *, *, #34704, .F. ) ;
#20817 = CARTESIAN_POINT ( 'NONE',  ( 14.85373647476855474, -5.808823158059035485, -5.808823158059033709 ) ) ;
#20818 = DIRECTION ( 'NONE',  ( -0.7071067811865486830, -0.7071067811865464625, -0.000000000000000000 ) ) ;
#20819 = DIRECTION ( 'NONE',  ( 0.7071067811865486830, -0.7071067811865464625, -0.000000000000000000 ) ) ;
#20820 = CARTESIAN_POINT ( 'NONE',  ( 11.04893972570927296, -8.462477794511665152, -4.317117199209826062 ) ) ;
#20821 = EDGE_LOOP ( 'NONE', ( #69813, #78266, #131174, #139786 ) ) ;
#20822 = EDGE_LOOP ( 'NONE', ( #142693, #35012, #97498, #98542 ) ) ;
#20823 = ORIENTED_EDGE ( 'NONE', *, *, #56935, .F. ) ;
#20824 = DIRECTION ( 'NONE',  ( 0.000000000000000000, 0.000000000000000000, 1.000000000000000000 ) ) ;
#20825 = CARTESIAN_POINT ( 'NONE',  ( -30.00000000000000355, 2.375000000000000000, 4.319999999999998508 ) ) ;
#20826 = PLANE ( 'NONE',  #105208 ) ;
#20827 = PLANE ( 'NONE',  #136248 ) ;
#20828 = CARTESIAN_POINT ( 'NONE',  ( -29.99451991528749417, 28.92564299267958816, 4.000000000000000000 ) ) ;
#20829 = VECTOR ( 'NONE', #136714, 1000.000000000000000 ) ;
#20830 = CARTESIAN_POINT ( 'NONE',  ( 24.18398860626899705, 28.73617430169804265, 5.000000000000000000 ) ) ;
#20831 = EDGE_CURVE ( 'NONE', #22070, #124953, #137289, .T. ) ;
#20832 = CARTESIAN_POINT ( 'NONE',  ( 33.68793019189809712, 6.110000000000002984, -1.637169565754156730 ) ) ;
#20833 = CARTESIAN_POINT ( 'NONE',  ( -0.3165796113278919188, -6.740707523384209310, 11.88629033278124503 ) ) ;
#20834 = LINE ( 'NONE', #125160, #41936 ) ;
#20835 = VERTEX_POINT ( 'NONE', #39407 ) ;
#20836 = CARTESIAN_POINT ( 'NONE',  ( 11.72733514412567857, 3.821174125832445049E-16, 0.000000000000000000 ) ) ;
#20837 = ORIENTED_EDGE ( 'NONE', *, *, #142868, .F. ) ;
#20838 = VECTOR ( 'NONE', #133510, 1000.000000000000000 ) ;
#20839 = AXIS2_PLACEMENT_3D ( 'NONE', #26037, #70298, #81141 ) ;
#20840 = VECTOR ( 'NONE', #24048, 1000.000000000000000 ) ;
#20841 = CARTESIAN_POINT ( 'NONE',  ( -33.48921356237309510, -27.52281430457078670, 5.000000000000000000 ) ) ;
#20842 = VERTEX_POINT ( 'NONE', #128547 ) ;
#20843 = VECTOR ( 'NONE', #44370, 1000.000000000000000 ) ;
#20844 = CARTESIAN_POINT ( 'NONE',  ( -19.05000000000000071, 3.174999999999997158, 5.000000000000000000 ) ) ;
#20846 = ORIENTED_EDGE ( 'NONE', *, *, #88302, .T. ) ;
#20845 = CARTESIAN_POINT ( 'NONE',  ( 4.499999999999970690, -13.91253812416061386, 4.000000000000000000 ) ) ;
#20847 = EDGE_CURVE ( 'NONE', #40538, #113538, #71542, .T. ) ;
#20848 = FACE_OUTER_BOUND ( 'NONE', #101353, .T. ) ;
#20849 = VERTEX_POINT ( 'NONE', #3854 ) ;
#20850 = VERTEX_POINT ( 'NONE', #83640 ) ;
#20851 = CARTESIAN_POINT ( 'NONE',  ( -27.18398860626900060, 28.73617430169806042, 5.000000000000000000 ) ) ;
#20852 = AXIS2_PLACEMENT_3D ( 'NONE', #123052, #134657, #23728 ) ;
#20853 = ORIENTED_EDGE ( 'NONE', *, *, #93635, .T. ) ;
#20854 =( NAMED_UNIT ( * ) PLANE_ANGLE_UNIT ( ) SI_UNIT ( $, .RADIAN. ) );
#20855 = CARTESIAN_POINT ( 'NONE',  ( 117.1833603837962272, -2.130196079827426203, 7.949999999999997513 ) ) ;
#20856 = CARTESIAN_POINT ( 'NONE',  ( 49.37086038379622011, 6.884901960086289741, -3.974999999999993427 ) ) ;
#20857 = CARTESIAN_POINT ( 'NONE',  ( -44.99451991528749772, 28.92564299267969474, 4.000000000000000000 ) ) ;
#20858 = DIRECTION ( 'NONE',  ( -0.7071067811865486830, -0.7071067811865464625, 0.000000000000000000 ) ) ;
#20859 = DIRECTION ( 'NONE',  ( 0.7071067811865486830, -0.7071067811865464625, -0.000000000000000000 ) ) ;
#20860 = CARTESIAN_POINT ( 'NONE',  ( 21.48921356237309155, -27.52281430457070499, 5.000000000000000000 ) ) ;
#20861 = CARTESIAN_POINT ( 'NONE',  ( 3.062499999999999556, 4.461849672132300881, 4.461849672132299105 ) ) ;
#20863 = VECTOR ( 'NONE', #6388, 1000.000000000000000 ) ;
#20862 = CARTESIAN_POINT ( 'NONE',  ( 16.16623647476855652, 7.934999999999990727, -1.457635852685135314E-15 ) ) ;
#20864 = DIRECTION ( 'NONE',  ( 0.7071067811865487940, 0.7071067811865463515, -0.000000000000000000 ) ) ;
#20865 = CARTESIAN_POINT ( 'NONE',  ( 8.292893218813395251, 17.25929247661554911, 5.000000000000000000 ) ) ;
#20866 = VERTEX_POINT ( 'NONE', #50277 ) ;
#20867 = ORIENTED_EDGE ( 'NONE', *, *, #38603, .F. ) ;
#20868 = VECTOR ( 'NONE', #8903, 999.9999999999998863 ) ;
#20869 = DIRECTION ( 'NONE',  ( 0.000000000000000000, 1.000000000000000000, -0.000000000000000000 ) ) ;
#20870 = EDGE_LOOP ( 'NONE', ( #47095, #79821, #115699, #848 ) ) ;
#20871 = CIRCLE ( 'NONE', #90319, 2.500000000000000888 ) ;
#20872 = CARTESIAN_POINT ( 'NONE',  ( -34.92500000000001137, -22.22500000000000142, 4.000000000000000000 ) ) ;
#20873 = CARTESIAN_POINT ( 'NONE',  ( -0.005480084712502889671, 28.92564299267938210, 4.000000000000000000 ) ) ;
#20874 = CARTESIAN_POINT ( 'NONE',  ( 34.42499999999998295, 20.97718569542917777, 5.000000000000000000 ) ) ;
#20875 = VERTEX_POINT ( 'NONE', #28530 ) ;
#20876 = VECTOR ( 'NONE', #136969, 1000.000000000000000 ) ;
#20877 = CARTESIAN_POINT ( 'NONE',  ( 11.51078643762690490, -27.52281430457047406, 5.000000000000000000 ) ) ;
#20878 = CARTESIAN_POINT ( 'NONE',  ( -34.42500000000001137, 0.000000000000000000, 4.500000000000000888 ) ) ;
#20879 = CARTESIAN_POINT ( 'NONE',  ( -48.18398860626899705, 28.73617430169820608, 5.000000000000000000 ) ) ;
#20880 = FACE_OUTER_BOUND ( 'NONE', #126952, .T. ) ;
#20881 = VECTOR ( 'NONE', #85202, 999.9999999999998863 ) ;
#20882 = CARTESIAN_POINT ( 'NONE',  ( 0.000000000000000000, 0.000000000000000000, 0.000000000000000000 ) ) ;
#20884 = ORIENTED_EDGE ( 'NONE', *, *, #74135, .F. ) ;
#20883 = DIRECTION ( 'NONE',  ( 0.7071067811865487940, 0.7071067811865463515, 0.000000000000000000 ) ) ;
#20885 = CARTESIAN_POINT ( 'NONE',  ( -9.792893218813388145, -2.240707523384257716, 5.000000000000000000 ) ) ;
#20886 = CARTESIAN_POINT ( 'NONE',  ( 69.54166666666667140, -3.975000000000002753, 6.884901960086286188 ) ) ;
#20887 = CARTESIAN_POINT ( 'NONE',  ( -3.489213562373097322, -27.52281430457057709, 5.000000000000000000 ) ) ;
#20888 = PLANE ( 'NONE',  #58620 ) ;
#20889 = ORIENTED_EDGE ( 'NONE', *, *, #41118, .F. ) ;
#20890 = EDGE_LOOP ( 'NONE', ( #46424, #32225, #33089, #10114 ) ) ;
#20891 = ORIENTED_EDGE ( 'NONE', *, *, #82760, .T. ) ;
#20892 = EDGE_CURVE ( 'NONE', #124072, #93762, #139456, .T. ) ;
#20893 = CARTESIAN_POINT ( 'NONE',  ( 93.77126352523141861, 4.472830434245839371, 4.472830434245842035 ) ) ;
#20894 = PRESENTATION_LAYER_ASSIGNMENT (  '', '', ( #134345 ) ) ;
#20895 = ORIENTED_EDGE ( 'NONE', *, *, #12027, .F. ) ;
#20896 = ADVANCED_FACE ( 'NONE', ( #103205 ), #15450, .T. ) ;
#20897 = CARTESIAN_POINT ( 'NONE',  ( 21.79333936457832266, 21.75929247661549226, 4.998822639870715179 ) ) ;
#20898 = EDGE_CURVE ( 'NONE', #99900, #46818, #82215, .T. ) ;
#20899 = AXIS2_PLACEMENT_3D ( 'NONE', #78482, #66889, #134296 ) ;
#20900 = EDGE_LOOP ( 'NONE', ( #133613, #108987, #28886, #795 ) ) ;
#20901 = EDGE_CURVE ( 'NONE', #108597, #80743, #138599, .T. ) ;
#20902 = CARTESIAN_POINT ( 'NONE',  ( 4.495848767239241539, 4.584330080086930965E-16, 0.000000000000000000 ) ) ;
#20903 = CARTESIAN_POINT ( 'NONE',  ( 184.1500000000000057, -30.18000000000009564, -15.92500000000064375 ) ) ;
#20904 = CARTESIAN_POINT ( 'NONE',  ( 82.74543019189812298, -5.291415217122918513, -3.055000000000000160 ) ) ;
#20905 = EDGE_LOOP ( 'NONE', ( #81602, #79944, #50641, #109015 ) ) ;
#20906 = LINE ( 'NONE', #54302, #120734 ) ;
#20907 = CARTESIAN_POINT ( 'NONE',  ( 114.8958333333333428, -2.130196079827447075, 7.949999999999988631 ) ) ;
#20908 = VECTOR ( 'NONE', #84830, 1000.000000000000227 ) ;
#20909 = ORIENTED_EDGE ( 'NONE', *, *, #38996, .T. ) ;
#20910 = ORIENTED_EDGE ( 'NONE', *, *, #77573, .F. ) ;
#20911 = EDGE_CURVE ( 'NONE', #136433, #125587, #126385, .T. ) ;
#20912 = ORIENTED_EDGE ( 'NONE', *, *, #74609, .F. ) ;
#20913 = DIRECTION ( 'NONE',  ( -0.7071067811865486830, 0.7071067811865464625, 0.000000000000000000 ) ) ;
#20914 = EDGE_CURVE ( 'NONE', #43938, #125881, #94467, .T. ) ;
#20915 = CARTESIAN_POINT ( 'NONE',  ( -54.18398860626899705, 28.73617430169825226, 5.000000000000000000 ) ) ;
#20916 = CARTESIAN_POINT ( 'NONE',  ( 14.79623647476855375, 7.934999999999990727, -1.457635852685135314E-15 ) ) ;
#20917 = LINE ( 'NONE', #110766, #37310 ) ;
#20918 = AXIS2_PLACEMENT_3D ( 'NONE', #122862, #112695, #23549 ) ;
#20919 = DIRECTION ( 'NONE',  ( 0.3543493200069162685, -0.000000000000000000, -0.9351131265310288487 ) ) ;
#20920 = ADVANCED_FACE ( 'NONE', ( #103901 ), #48137, .F. ) ;
#20921 = CARTESIAN_POINT ( 'NONE',  ( 16.27785539607886633, 3.061616997868383634E-16, -2.500000000000000444 ) ) ;
#20922 = SURFACE_STYLE_FILL_AREA ( #139175 ) ;
#20923 = ORIENTED_EDGE ( 'NONE', *, *, #111149, .T. ) ;
#20924 =( BOUNDED_CURVE ( )  B_SPLINE_CURVE ( 2, ( #19473, #128945, #107187, #131098, #18735, #52101, #107876, #118776, #41217, #85422, #52790, #96989, #108579 ),
 .UNSPECIFIED., .F., .T. ) 
 B_SPLINE_CURVE_WITH_KNOTS ( ( 3, 2, 2, 2, 2, 2, 3 ),
 ( 0.8166666666666666519, 0.8194444444444444198, 0.8222222222222221877, 0.8249999999999999556, 0.8277777777777778345, 0.8305555555555557135, 0.8333333333333334814 ),
 .UNSPECIFIED. ) 
 CURVE ( )  GEOMETRIC_REPRESENTATION_ITEM ( )  RATIONAL_B_SPLINE_CURVE ( ( 1.000000000000000000, 0.9659258262890683122, 1.000000000000000000, 0.9659258262890683122, 1.000000000000000000, 0.9659258262890683122, 1.000000000000000000, 0.9659258262890683122, 1.000000000000000000, 0.9659258262890683122, 1.000000000000000000, 0.9659258262890669799, 1.000000000000001332 ) ) 
 REPRESENTATION_ITEM ( '' )  );
#20925 = ORIENTED_EDGE ( 'NONE', *, *, #26688, .F. ) ;
#20926 = DIRECTION ( 'NONE',  ( -0.6830127018922181881, 0.6830127018922202975, -0.2588190451025214056 ) ) ;
#20927 = ORIENTED_EDGE ( 'NONE', *, *, #96818, .T. ) ;
#20928 = ORIENTED_EDGE ( 'NONE', *, *, #22211, .F. ) ;
#20929 = ADVANCED_FACE ( 'NONE', ( #29214 ), #73459, .T. ) ;
#20930 = VECTOR ( 'NONE', #101811, 1000.000000000000000 ) ;
#20931 = AXIS2_PLACEMENT_3D ( 'NONE', #38061, #59131, #138803 ) ;
#20932 = CARTESIAN_POINT ( 'NONE',  ( 15.18398860626900237, 28.73617430169797871, 5.000000000000000000 ) ) ;
#20933 = ORIENTED_EDGE ( 'NONE', *, *, #63964, .T. ) ;
#20934 = CARTESIAN_POINT ( 'NONE',  ( 45.18398860626900415, 28.73617430169818832, 5.000000000000000000 ) ) ;
#20935 = DIRECTION ( 'NONE',  ( 1.000000000000000000, 1.224606353822377258E-16, 0.000000000000000000 ) ) ;
#20936 = CARTESIAN_POINT ( 'NONE',  ( -23.99999999999983302, 13.93112307739204425, 4.000000000000000000 ) ) ;
#20937 = EDGE_CURVE ( 'NONE', #49762, #74191, #30673, .T. ) ;
#20938 = FACE_OUTER_BOUND ( 'NONE', #130709, .T. ) ;
#20939 = AXIS2_PLACEMENT_3D ( 'NONE', #43466, #88417, #66657 ) ;
#20940 = AXIS2_PLACEMENT_3D ( 'NONE', #42645, #75267, #96946 ) ;
#20941 = AXIS2_PLACEMENT_3D ( 'NONE', #7800, #86828, #96228 ) ;
#20942 = CARTESIAN_POINT ( 'NONE',  ( 119.2708333333333286, -7.949999999999998401, -2.130196079827426203 ) ) ;
#20943 = ORIENTED_EDGE ( 'NONE', *, *, #112698, .F. ) ;
#20944 = VECTOR ( 'NONE', #140774, 1000.000000000000000 ) ;
#20945 = CARTESIAN_POINT ( 'NONE',  ( 17.99999999999987566, 13.93112307739204425, 4.000000000000000000 ) ) ;
#20946 = ORIENTED_EDGE ( 'NONE', *, *, #66917, .F. ) ;
#20947 = CARTESIAN_POINT ( 'NONE',  ( 19.86926087748564740, -2.706703797573569936, -33.83166409453657764 ) ) ;
#20948 = ORIENTED_EDGE ( 'NONE', *, *, #12634, .T. ) ;
#20949 = DIRECTION ( 'NONE',  ( 0.7071067811865486830, -0.7071067811865464625, -0.000000000000000000 ) ) ;
#20950 = VERTEX_POINT ( 'NONE', #53859 ) ;
#20951 = LINE ( 'NONE', #43437, #8809 ) ;
#20952 = ORIENTED_EDGE ( 'NONE', *, *, #108637, .F. ) ;
#20953 = VERTEX_POINT ( 'NONE', #21197 ) ;
#20954 = VECTOR ( 'NONE', #60146, 1000.000000000000000 ) ;
#20955 = EDGE_LOOP ( 'NONE', ( #49144, #24771, #44806, #127232 ) ) ;
#20956 = ADVANCED_FACE ( 'NONE', ( #40822 ), #74166, .F. ) ;
#20957 = PLANE ( 'NONE',  #257 ) ;
#20958 = CARTESIAN_POINT ( 'NONE',  ( 24.79593897580385331, 4.791522900035168675, 4.000000000000000000 ) ) ;
#20959 = FACE_OUTER_BOUND ( 'NONE', #142818, .T. ) ;
#20960 = CARTESIAN_POINT ( 'NONE',  ( 124.5420968585647756, 5.291415217122923842, -3.054999999999996163 ) ) ;
#20961 = PLANE ( 'NONE',  #28912 ) ;
#20962 = FACE_OUTER_BOUND ( 'NONE', #117845, .T. ) ;
#20963 = DIRECTION ( 'NONE',  ( -0.7071067811865486830, -0.7071067811865464625, 0.000000000000000000 ) ) ;
#20964 = VECTOR ( 'NONE', #72971, 1000.000000000000227 ) ;
#20965 = LINE ( 'NONE', #12231, #109455 ) ;
#20966 = VECTOR ( 'NONE', #2744, 1000.000000000000000 ) ;
#20967 = LINE ( 'NONE', #9346, #36723 ) ;
#20968 = AXIS2_PLACEMENT_3D ( 'NONE', #53799, #33484, #140765 ) ;
#20969 = CARTESIAN_POINT ( 'NONE',  ( 184.1499999999998067, -3.180000000000061444, -34.92499999999998295 ) ) ;
#20970 = LINE ( 'NONE', #75377, #40127 ) ;
#20971 = EDGE_CURVE ( 'NONE', #24063, #78218, #106766, .T. ) ;
#20972 = ORIENTED_EDGE ( 'NONE', *, *, #50816, .T. ) ;
#20973 = AXIS2_PLACEMENT_3D ( 'NONE', #43009, #141602, #88660 ) ;
#20974 = EDGE_LOOP ( 'NONE', ( #78181, #9207, #1938, #100062 ) ) ;
#20975 = ORIENTED_EDGE ( 'NONE', *, *, #5932, .F. ) ;
#20976 = PLANE ( 'NONE',  #114343 ) ;
#20977 = EDGE_LOOP ( 'NONE', ( #113471, #52075 ) ) ;
#20978 = AXIS2_PLACEMENT_3D ( 'NONE', #42470, #29405, #41722 ) ;
#20979 = ORIENTED_EDGE ( 'NONE', *, *, #55629, .F. ) ;
#20980 = CARTESIAN_POINT ( 'NONE',  ( -15.18398860626900237, 28.73617430169797871, 5.000000000000000000 ) ) ;
#20981 = CARTESIAN_POINT ( 'NONE',  ( 18.48921356237309510, -27.52281430457068367, 5.000000000000000000 ) ) ;
#20982 = EDGE_CURVE ( 'NONE', #129488, #98003, #140818, .T. ) ;
#20983 = VECTOR ( 'NONE', #118370, 1000.000000000000227 ) ;
#20984 = CARTESIAN_POINT ( 'NONE',  ( -34.92500000000001137, 22.22500000000000142, 4.000000000000000000 ) ) ;
#20985 = ORIENTED_EDGE ( 'NONE', *, *, #37283, .T. ) ;
#20986 = PLANE ( 'NONE',  #67305 ) ;
#20987 = EDGE_LOOP ( 'NONE', ( #55607, #51871, #126124, #45801 ) ) ;
#20988 = CARTESIAN_POINT ( 'NONE',  ( -21.18398860626899349, 28.73617430169802134, 5.000000000000000000 ) ) ;
#20989 = DIRECTION ( 'NONE',  ( 0.7071067811865487940, 0.7071067811865463515, 0.000000000000000000 ) ) ;
#20990 = VECTOR ( 'NONE', #74370, 1000.000000000000000 ) ;
#20991 = CARTESIAN_POINT ( 'NONE',  ( 17.85873647476854842, 5.808823158059031044, -5.808823158059038150 ) ) ;
#20992 = ORIENTED_EDGE ( 'NONE', *, *, #124402, .T. ) ;
#20993 = CARTESIAN_POINT ( 'NONE',  ( 94.84959685856476597, 6.109999999999997655, 1.637169565754163836 ) ) ;
#20994 = CARTESIAN_POINT ( 'NONE',  ( 6.613632711652026153, -9.212947288752639352, -2.320845120914358795 ) ) ;
#20995 = FACE_OUTER_BOUND ( 'NONE', #91394, .T. ) ;
#20996 = DIRECTION ( 'NONE',  ( -0.000000000000000000, 0.000000000000000000, 1.000000000000000000 ) ) ;
#20997 = EDGE_LOOP ( 'NONE', ( #58818, #85114, #112359, #84989 ) ) ;
#20998 = FACE_OUTER_BOUND ( 'NONE', #66717, .T. ) ;
#20999 = ORIENTED_EDGE ( 'NONE', *, *, #136417, .F. ) ;
#21000 =( NAMED_UNIT ( * ) SI_UNIT ( $, .STERADIAN. ) SOLID_ANGLE_UNIT ( ) );
#21001 = AXIS2_PLACEMENT_3D ( 'NONE', #116806, #63186, #8023 ) ;
#21002 = EDGE_LOOP ( 'NONE', ( #131038, #138536, #12569, #67117 ) ) ;
#21003 = LINE ( 'NONE', #86291, #13897 ) ;
#21004 = DIRECTION ( 'NONE',  ( -0.7071067811865486830, -0.7071067811865464625, 0.000000000000000000 ) ) ;
#21005 = FACE_OUTER_BOUND ( 'NONE', #109700, .T. ) ;
#21006 = ORIENTED_EDGE ( 'NONE', *, *, #10496, .F. ) ;
#21007 = CARTESIAN_POINT ( 'NONE',  ( 24.41159235450331977, 9.902892378096218942E-16, 0.000000000000000000 ) ) ;
#21008 = EDGE_CURVE ( 'NONE', #56060, #102325, #97298, .T. ) ;
#21009 = CARTESIAN_POINT ( 'NONE',  ( -36.48921356237310221, -27.52281430457080802, 5.000000000000000000 ) ) ;
#21010 = ORIENTED_EDGE ( 'NONE', *, *, #7792, .T. ) ;
#21011 = DIRECTION ( 'NONE',  ( 0.7071067811865487940, -0.7071067811865463515, 0.000000000000000000 ) ) ;
#21012 = PRESENTATION_LAYER_ASSIGNMENT (  '', '', ( #95107 ) ) ;
#21013 = DIRECTION ( 'NONE',  ( -0.3543493200069163240, 0.000000000000000000, 0.9351131265310288487 ) ) ;
#21014 = ORIENTED_EDGE ( 'NONE', *, *, #135866, .T. ) ;
#21015 = EDGE_CURVE ( 'NONE', #88631, #6614, #109632, .T. ) ;
#21017 = VERTEX_POINT ( 'NONE', #87172 ) ;
#21016 = DIRECTION ( 'NONE',  ( -1.000000000000000000, -1.224606353822377258E-16, -0.000000000000000000 ) ) ;
#21018 = ORIENTED_EDGE ( 'NONE', *, *, #125686, .T. ) ;
#21019 = EDGE_CURVE ( 'NONE', #110441, #38956, #51712, .T. ) ;
#21020 = DIRECTION ( 'NONE',  ( -0.7071067811865487940, 0.7071067811865463515, 0.000000000000000000 ) ) ;
#21021 = DIRECTION ( 'NONE',  ( 0.7071067811865486830, -0.7071067811865464625, -0.000000000000000000 ) ) ;
#21023 = EDGE_LOOP ( 'NONE', ( #27264, #128030, #90952, #51082 ) ) ;
#21022 = AXIS2_PLACEMENT_3D ( 'NONE', #79948, #100931, #34996 ) ;
#21024 = CARTESIAN_POINT ( 'NONE',  ( 174.7500000000000000, 7.919999999999947526, 19.12499999999998224 ) ) ;
#21025 = CARTESIAN_POINT ( 'NONE',  ( 8.999999999999948486, 11.58746187583912324, 4.000000000000000000 ) ) ;
#21026 = CARTESIAN_POINT ( 'NONE',  ( 63.29974487139158867, -27.71228299555250274, 4.000000000000000000 ) ) ;
#21027 = DIRECTION ( 'NONE',  ( -1.000000000000000000, 1.248002500702738701E-15, 0.000000000000000000 ) ) ;
#21028 = PLANE ( 'NONE',  #99849 ) ;
#21029 = PLANE ( 'NONE',  #30554 ) ;
#21030 = CARTESIAN_POINT ( 'NONE',  ( 13.13598696172163116, 4.584330080086930965E-16, 0.000000000000000000 ) ) ;
#21031 = CARTESIAN_POINT ( 'NONE',  ( 6.299744871391586898, -27.71228299555210484, 4.000000000000000000 ) ) ;
#21032 = DIRECTION ( 'NONE',  ( 0.6830127018922181881, 0.6830127018922202975, -0.2588190451025214056 ) ) ;
#21033 = CARTESIAN_POINT ( 'NONE',  ( 24.39999999999999858, -1.600000000000094458, 34.92499999999998295 ) ) ;
#21034 = CIRCLE ( 'NONE', #65051, 2.500000000000000888 ) ;
#21035 = CARTESIAN_POINT ( 'NONE',  ( 27.99999999999996803, -57.14999999999999147, 49.92499999999997584 ) ) ;
#21036 = DIRECTION ( 'NONE',  ( 0.3543493200069162685, -0.000000000000000000, -0.9351131265310288487 ) ) ;
#21037 = ORIENTED_EDGE ( 'NONE', *, *, #7751, .F. ) ;
#21038 = ADVANCED_FACE ( 'NONE', ( #8837 ), #142290, .T. ) ;
#21039 = ORIENTED_EDGE ( 'NONE', *, *, #85365, .F. ) ;
#21040 = ORIENTED_EDGE ( 'NONE', *, *, #66440, .T. ) ;
#21041 = AXIS2_PLACEMENT_3D ( 'NONE', #109226, #141126, #130291 ) ;
#21042 = CARTESIAN_POINT ( 'NONE',  ( 105.7083333333333286, -3.974999999999999201, -6.884901960086287964 ) ) ;
#21043 = AXIS2_PLACEMENT_3D ( 'NONE', #120777, #54840, #110598 ) ;
#21044 = ORIENTED_EDGE ( 'NONE', *, *, #100632, .T. ) ;
#21045 = ORIENTED_EDGE ( 'NONE', *, *, #34532, .F. ) ;
#21046 = ORIENTED_EDGE ( 'NONE', *, *, #97206, .F. ) ;
#21047 = DIRECTION ( 'NONE',  ( 0.7071067811865486830, -0.7071067811865464625, -0.000000000000000000 ) ) ;
#21048 = CARTESIAN_POINT ( 'NONE',  ( -23.67183060077630685, -18.74070752338409918, 4.000000000000000000 ) ) ;
#21049 = VECTOR ( 'NONE', #48847, 1000.000000000000000 ) ;
#21050 = AXIS2_PLACEMENT_3D ( 'NONE', #45340, #101821, #133747 ) ;
#21051 = VECTOR ( 'NONE', #81682, 999.9999999999998863 ) ;
#21052 = EDGE_LOOP ( 'NONE', ( #64114, #20975, #33982, #105791 ) ) ;
#21053 = CARTESIAN_POINT ( 'NONE',  ( 12.75860074219786711, 21.72500000000000142, 5.000000000000000000 ) ) ;
#21054 = CIRCLE ( 'NONE', #111286, 2.500000000000000444 ) ;
#21055 = LINE ( 'NONE', #10179, #41818 ) ;
#21056 = DIRECTION ( 'NONE',  ( 0.000000000000000000, -1.000000000000000000, 0.000000000000000000 ) ) ;
#21057 = DIRECTION ( 'NONE',  ( 1.000000000000000000, -0.000000000000000000, 0.000000000000000000 ) ) ;
#21058 = ORIENTED_EDGE ( 'NONE', *, *, #437, .F. ) ;
#21059 = CARTESIAN_POINT ( 'NONE',  ( 7.578844083866184356, 10.86561545741349377, -28.20638205426730138 ) ) ;
#21060 = PLANE ( 'NONE',  #3337 ) ;
#21061 = VECTOR ( 'NONE', #13561, 1000.000000000000000 ) ;
#21062 = DIRECTION ( 'NONE',  ( 0.000000000000000000, -1.000000000000000000, 0.000000000000000000 ) ) ;
#21063 = LINE ( 'NONE', #43545, #19062 ) ;
#21064 = DIRECTION ( 'NONE',  ( -0.6830127018922181881, 0.6830127018922202975, -0.2588190451025214056 ) ) ;
#21065 = CARTESIAN_POINT ( 'NONE',  ( 30.70419371712955581, -6.884901960086285300, -3.975000000000000089 ) ) ;
#21066 = CARTESIAN_POINT ( 'NONE',  ( 83.99451991528748351, 28.92564299267996830, 4.000000000000000000 ) ) ;
#21067 = EDGE_CURVE ( 'NONE', #103751, #105472, #52393, .T. ) ;
#21068 = VERTEX_POINT ( 'NONE', #129971 ) ;
#21069 = VERTEX_POINT ( 'NONE', #42266 ) ;
#21070 = ADVANCED_FACE ( 'NONE', ( #32083 ), #130707, .F. ) ;
#21071 = CARTESIAN_POINT ( 'NONE',  ( 122.9379301918981042, -6.110000000000001208, 1.637169565754158951 ) ) ;
#21072 = ORIENTED_EDGE ( 'NONE', *, *, #78533, .F. ) ;
#21073 = MECHANICAL_DESIGN_GEOMETRIC_PRESENTATION_REPRESENTATION (  '', ( #83723 ), #41998 ) ;
#21074 = DIRECTION ( 'NONE',  ( 0.000000000000000000, -1.000000000000000000, 0.000000000000000000 ) ) ;
#21075 = EDGE_CURVE ( 'NONE', #16081, #139077, #42977, .T. ) ;
#21076 = VECTOR ( 'NONE', #106590, 1000.000000000000000 ) ;
#21077 = CARTESIAN_POINT ( 'NONE',  ( 29.30673006690383176, -3.740707523384248390, 12.88036043432860822 ) ) ;
#21078 = LINE ( 'NONE', #65346, #129011 ) ;
#21080 = EDGE_CURVE ( 'NONE', #89257, #67554, #54567, .T. ) ;
#21079 = DIRECTION ( 'NONE',  ( 0.6830127018922180770, -0.6830127018922204085, -0.2588190451025213501 ) ) ;
#21081 = EDGE_CURVE ( 'NONE', #42357, #35420, #106258, .T. ) ;
#21082 = CARTESIAN_POINT ( 'NONE',  ( 11.25346039003969523, 4.202752102959690472E-16, 0.000000000000000000 ) ) ;
#21083 = FACE_OUTER_BOUND ( 'NONE', #35476, .T. ) ;
#21084 = AXIS2_PLACEMENT_3D ( 'NONE', #101714, #82840, #80700 ) ;
#21085 = VECTOR ( 'NONE', #82972, 1000.000000000000000 ) ;
#21086 = CARTESIAN_POINT ( 'NONE',  ( 125.1829301918981372, -1.637169565754158951, -6.109999999999998543 ) ) ;
#21087 = VERTEX_POINT ( 'NONE', #62582 ) ;
#21088 = VECTOR ( 'NONE', #113686, 1000.000000000000000 ) ;
#21089 = ORIENTED_EDGE ( 'NONE', *, *, #92244, .F. ) ;
#21090 = DIRECTION ( 'NONE',  ( -0.000000000000000000, 0.000000000000000000, 1.000000000000000000 ) ) ;
#21091 = VECTOR ( 'NONE', #118191, 1000.000000000000227 ) ;
#21092 = CARTESIAN_POINT ( 'NONE',  ( -59.99451991528749772, 28.92564299267980132, 4.000000000000000000 ) ) ;
#21093 = EDGE_LOOP ( 'NONE', ( #129, #64610, #45669, #70940 ) ) ;
#21095 = EDGE_CURVE ( 'NONE', #12281, #110799, #129235, .T. ) ;
#21094 = CARTESIAN_POINT ( 'NONE',  ( 43.02126352523142572, -4.472830434245839371, -4.472830434245840259 ) ) ;
#21096 = EDGE_LOOP ( 'NONE', ( #39311, #38509, #29018, #34186 ) ) ;
#21097 = VECTOR ( 'NONE', #77595, 1000.000000000000000 ) ;
#21098 = LINE ( 'NONE', #55176, #79576 ) ;
#21099 = ADVANCED_FACE ( 'NONE', ( #118357 ), #8155, .F. ) ;
#21100 = CARTESIAN_POINT ( 'NONE',  ( 11.81601139373100651, 28.73617430169779041, 5.000000000000000000 ) ) ;
#21101 = DIRECTION ( 'NONE',  ( 0.7071067811865487940, 0.7071067811865463515, -0.000000000000000000 ) ) ;
#21102 = VECTOR ( 'NONE', #105607, 1000.000000000000000 ) ;
#21103 = EDGE_CURVE ( 'NONE', #114174, #96751, #1549, .T. ) ;
#21104 = CARTESIAN_POINT ( 'NONE',  ( 38.26626352523144448, 4.472830434245839371, -4.472830434245838482 ) ) ;
#21105 = EDGE_LOOP ( 'NONE', ( #107170, #45780, #130089, #131293 ) ) ;
#21106 = DIRECTION ( 'NONE',  ( 0.7071067811865487940, -0.7071067811865463515, 0.000000000000000000 ) ) ;
#21107 = ORIENTED_EDGE ( 'NONE', *, *, #21443, .F. ) ;
#21108 = ORIENTED_EDGE ( 'NONE', *, *, #45413, .F. ) ;
#21109 = VECTOR ( 'NONE', #67270, 1000.000000000000227 ) ;
#21110 = EDGE_CURVE ( 'NONE', #65170, #78582, #100895, .T. ) ;
#21111 = ORIENTED_EDGE ( 'NONE', *, *, #114605, .T. ) ;
#21112 = VECTOR ( 'NONE', #9206, 1000.000000000000227 ) ;
#21113 = PLANE ( 'NONE',  #99720 ) ;
#21114 = PRODUCT_DEFINITION_CONTEXT ( 'detailed design', #44916, 'design' ) ;
#21115 = ORIENTED_EDGE ( 'NONE', *, *, #130847, .F. ) ;
#21116 = DIRECTION ( 'NONE',  ( -1.000000000000000000, -1.224606353822377258E-16, -0.000000000000000000 ) ) ;
#21117 = VECTOR ( 'NONE', #100618, 1000.000000000000000 ) ;
#21118 = EDGE_CURVE ( 'NONE', #126057, #85488, #122644, .T. ) ;
#21119 = VECTOR ( 'NONE', #87355, 1000.000000000000000 ) ;
#21120 = CARTESIAN_POINT ( 'NONE',  ( 0.7071067811865432429, 2.259292476615688994, 5.000000000000000000 ) ) ;
#21121 = CARTESIAN_POINT ( 'NONE',  ( 1.953608656376216022E-15, -6.270000000000002238, -40.00000000000000000 ) ) ;
#21122 = FACE_BOUND ( 'NONE', #45974, .T. ) ;
#21123 = ORIENTED_EDGE ( 'NONE', *, *, #57683, .T. ) ;
#21124 = CARTESIAN_POINT ( 'NONE',  ( -5.999999999999960032, -1.068876922607802538, 4.000000000000000000 ) ) ;
#21125 = CARTESIAN_POINT ( 'NONE',  ( -39.18398860626899705, 28.73617430169814568, 5.000000000000000000 ) ) ;
#21126 = PLANE ( 'NONE',  #74081 ) ;
#21127 = ORIENTED_EDGE ( 'NONE', *, *, #98238, .T. ) ;
#21128 = EDGE_CURVE ( 'NONE', #124198, #89614, #11002, .T. ) ;
#21129 = CARTESIAN_POINT ( 'NONE',  ( 24.54580628287043709, 5.278424836066143655, -3.047499999999997655 ) ) ;
#21130 = ORIENTED_EDGE ( 'NONE', *, *, #102262, .T. ) ;
#21131 = EDGE_CURVE ( 'NONE', #62743, #116904, #112495, .T. ) ;
#21132 = ORIENTED_EDGE ( 'NONE', *, *, #106544, .T. ) ;
#21133 = CIRCLE ( 'NONE', #118292, 2.055000000000001048 ) ;
#21134 = LINE ( 'NONE', #69487, #86483 ) ;
#21135 = ORIENTED_EDGE ( 'NONE', *, *, #1559, .F. ) ;
#21136 = EDGE_CURVE ( 'NONE', #37795, #50134, #134258, .T. ) ;
#21137 = CARTESIAN_POINT ( 'NONE',  ( 44.97459685856478018, 1.637169565754164280, -6.109999999999996767 ) ) ;
#21138 = ORIENTED_EDGE ( 'NONE', *, *, #18077, .F. ) ;
#21139 = CARTESIAN_POINT ( 'NONE',  ( 12.19999999999999574, -59.76999999999998892, -39.50000000000000000 ) ) ;
#21140 = DIRECTION ( 'NONE',  ( 1.000000000000000000, 0.000000000000000000, 0.000000000000000000 ) ) ;
#21141 = LINE ( 'NONE', #61, #101973 ) ;
#21142 = EDGE_LOOP ( 'NONE', ( #73743, #118227, #111646, #10658 ) ) ;
#21143 = DIRECTION ( 'NONE',  ( -1.000000000000000000, -0.000000000000000000, -0.000000000000000000 ) ) ;
#21144 = CARTESIAN_POINT ( 'NONE',  ( 15.65467068707222076, 3.821174125832445049E-16, 0.000000000000000000 ) ) ;
#21146 = ADVANCED_FACE ( 'NONE', ( #45138 ), #138701, .T. ) ;
#21145 = VECTOR ( 'NONE', #133196, 1000.000000000000000 ) ;
#21147 = CIRCLE ( 'NONE', #42083, 5.968999999999998529 ) ;
#21148 = AXIS2_PLACEMENT_3D ( 'NONE', #1810, #80874, #70022 ) ;
#21149 = CARTESIAN_POINT ( 'NONE',  ( 28.49999999999979750, -7.533600742197658739, 5.000000000000000000 ) ) ;
#21150 =( LENGTH_UNIT ( ) NAMED_UNIT ( * ) SI_UNIT ( .MILLI., .METRE. ) );
#21151 = LINE ( 'NONE', #66112, #6536 ) ;
#21152 = CARTESIAN_POINT ( 'NONE',  ( 51.48921356237309510, -27.52281430457091460, 5.000000000000000000 ) ) ;
#21153 = CARTESIAN_POINT ( 'NONE',  ( 8.292986735706890045, -21.74070752338406365, 4.999753212805221558 ) ) ;
#21154 = VERTEX_POINT ( 'NONE', #100202 ) ;
#21155 = STYLED_ITEM ( 'NONE', ( #28915 ), #129368 ) ;
#21156 = ORIENTED_EDGE ( 'NONE', *, *, #49086, .T. ) ;
#21157 = VECTOR ( 'NONE', #7089, 1000.000000000000000 ) ;
#21158 = ORIENTED_EDGE ( 'NONE', *, *, #35191, .F. ) ;
#21159 = AXIS2_PLACEMENT_3D ( 'NONE', #114353, #102054, #15023 ) ;
#21160 = LINE ( 'NONE', #99405, #105182 ) ;
#21161 = CARTESIAN_POINT ( 'NONE',  ( -60.48921356237309510, -27.52281430457097500, 5.000000000000000000 ) ) ;
#21162 = ORIENTED_EDGE ( 'NONE', *, *, #127854, .T. ) ;
#21163 = VECTOR ( 'NONE', #51686, 1000.000000000000000 ) ;
#21164 = ORIENTED_EDGE ( 'NONE', *, *, #122239, .T. ) ;
#21165 = CARTESIAN_POINT ( 'NONE',  ( 63.48921356237309510, -27.52281430457099631, 5.000000000000000000 ) ) ;
#21166 = CARTESIAN_POINT ( 'NONE',  ( 75.48921356237309510, -27.52281430457107803, 5.000000000000000000 ) ) ;
#21167 = DIRECTION ( 'NONE',  ( 0.000000000000000000, -1.000000000000000000, 0.000000000000000000 ) ) ;
#21168 = ORIENTED_EDGE ( 'NONE', *, *, #124911, .F. ) ;
#21169 = MECHANICAL_DESIGN_GEOMETRIC_PRESENTATION_REPRESENTATION (  '', ( #72138 ), #44388 ) ;
#21170 = PLANE ( 'NONE',  #92615 ) ;
#21171 = FACE_OUTER_BOUND ( 'NONE', #97984, .T. ) ;
#21172 = CARTESIAN_POINT ( 'NONE',  ( 20.77540314143522338, -2.126176841940958351, -7.934999999999989839 ) ) ;
#21173 = DIRECTION ( 'NONE',  ( -1.000000000000000000, -1.224606353822377258E-16, -0.000000000000000000 ) ) ;
#21174 = EDGE_LOOP ( 'NONE', ( #23272, #118060, #1542, #89281, #19592 ) ) ;
#21175 = CARTESIAN_POINT ( 'NONE',  ( 119.6412635252314658, 4.472830434245837594, 4.472830434245841147 ) ) ;
#21176 = VECTOR ( 'NONE', #99567, 1000.000000000000000 ) ;
#21178 = EDGE_CURVE ( 'NONE', #116001, #49148, #111788, .T. ) ;
#21177 = DIRECTION ( 'NONE',  ( 0.7071067811865487940, 0.7071067811865463515, 0.000000000000000000 ) ) ;
#21179 = CARTESIAN_POINT ( 'NONE',  ( 39.48921356237310221, -27.52281430457082934, 5.000000000000000000 ) ) ;
#21181 = ORIENTED_EDGE ( 'NONE', *, *, #17957, .F. ) ;
#21180 = CARTESIAN_POINT ( 'NONE',  ( 29.99999999999979394, -0.8619312979531689178, -5.102805207349756067 ) ) ;
#21182 = DIRECTION ( 'NONE',  ( -0.5735764363510501562, 0.8191520442889890230, 1.003171929053521419E-16 ) ) ;
#21183 = ORIENTED_EDGE ( 'NONE', *, *, #108799, .F. ) ;
#21184 = LINE ( 'NONE', #55256, #127968 ) ;
#21185 = CARTESIAN_POINT ( 'NONE',  ( -33.48921356237309510, -27.52281430457078670, 5.000000000000000000 ) ) ;
#21186 = ORIENTED_EDGE ( 'NONE', *, *, #107466, .F. ) ;
#21187 = COLOUR_RGB ( '', 0.31764706, 0.68627451, 0.89019608) ;
#21188 = VECTOR ( 'NONE', #107210, 1000.000000000000000 ) ;
#21189 = AXIS2_PLACEMENT_3D ( 'NONE', #22205, #43284, #109944 ) ;
#21190 = CARTESIAN_POINT ( 'NONE',  ( 11.20710678118646442, -17.24070752338410983, 5.000000000000000000 ) ) ;
#21191 = CARTESIAN_POINT ( 'NONE',  ( 36.18398860626899705, 28.73617430169812437, 5.000000000000000000 ) ) ;
#21192 = ORIENTED_EDGE ( 'NONE', *, *, #108301, .F. ) ;
#21193 = CARTESIAN_POINT ( 'NONE',  ( -6.005480084712508493, 28.92564299267933947, 4.000000000000000000 ) ) ;
#21194 = CIRCLE ( 'NONE', #74413, 2.055000000000001048 ) ;
#21195 = DIRECTION ( 'NONE',  ( 0.7071067811865487940, 0.7071067811865463515, 0.000000000000000000 ) ) ;
#21196 = EDGE_LOOP ( 'NONE', ( #76379, #25365, #22746, #58093 ) ) ;
#21197 = CARTESIAN_POINT ( 'NONE',  ( -11.20710678118645731, -11.24070752338416845, 5.000000000000000000 ) ) ;
#21198 = ADVANCED_FACE ( 'NONE', ( #33540 ), #66860, .F. ) ;
#21200 = EDGE_LOOP ( 'NONE', ( #57446, #99083, #134219, #63905 ) ) ;
#21199 = CARTESIAN_POINT ( 'NONE',  ( 15.18398860626900237, 28.73617430169797871, 5.000000000000000000 ) ) ;
#21202 = ORIENTED_EDGE ( 'NONE', *, *, #5384, .T. ) ;
#21201 = EDGE_CURVE ( 'NONE', #134058, #90351, #119, .T. ) ;
#21203 = LINE ( 'NONE', #142980, #19426 ) ;
#21204 = CARTESIAN_POINT ( 'NONE',  ( -36.29974487139159578, -27.71228299555231445, 4.000000000000000000 ) ) ;
#21205 = VERTEX_POINT ( 'NONE', #44418 ) ;
#21206 = EDGE_CURVE ( 'NONE', #69406, #73447, #57424, .T. ) ;
#21207 = CARTESIAN_POINT ( 'NONE',  ( 24.29974487139158867, -27.71228299555223273, 4.000000000000000000 ) ) ;
#21208 = DIRECTION ( 'NONE',  ( 0.000000000000000000, -1.000000000000000000, 0.000000000000000000 ) ) ;
#21209 = DIRECTION ( 'NONE',  ( 0.6830127018922181881, 0.6830127018922202975, -0.2588190451025214056 ) ) ;
#21210 = ORIENTED_EDGE ( 'NONE', *, *, #129093, .T. ) ;
#21211 = ADVANCED_FACE ( 'NONE', ( #46582 ), #90767, .F. ) ;
#21212 = DIRECTION ( 'NONE',  ( -0.000000000000000000, 0.000000000000000000, 1.000000000000000000 ) ) ;
#21213 = DIRECTION ( 'NONE',  ( -0.6830127018922181881, 0.6830127018922202975, -0.2588190451025214056 ) ) ;
#21214 = CONICAL_SURFACE ( 'NONE', #79109, 2.500000000000000888, 0.9599310885968822538 ) ;
#21215 = DIRECTION ( 'NONE',  ( -1.000000000000000000, -3.115803279706882722E-16, -0.000000000000000000 ) ) ;
#21216 = AXIS2_PLACEMENT_3D ( 'NONE', #53110, #31387, #75610 ) ;
#21217 =( LENGTH_UNIT ( ) NAMED_UNIT ( * ) SI_UNIT ( .MILLI., .METRE. ) );
#21218 = CARTESIAN_POINT ( 'NONE',  ( 41.18293019189811588, -1.637169565754159173, -6.109999999999999432 ) ) ;
#21219 = CARTESIAN_POINT ( 'NONE',  ( -29.29289321881324426, -15.74070752338412760, 5.000000000000000000 ) ) ;
#21220 = ADVANCED_FACE ( 'NONE', ( #121215 ), #2148, .T. ) ;
#21221 = ORIENTED_EDGE ( 'NONE', *, *, #48712, .T. ) ;
#21222 = ORIENTED_EDGE ( 'NONE', *, *, #116855, .T. ) ;
#21223 = EDGE_LOOP ( 'NONE', ( #51974, #43810, #127555, #64712, #2731 ) ) ;
#21224 = VECTOR ( 'NONE', #101391, 1000.000000000000227 ) ;
#21225 = ORIENTED_EDGE ( 'NONE', *, *, #114486, .T. ) ;
#21226 = COLOUR_RGB ( '', 0.66274510, 0.83137255, 0.94901961) ;
#21227 = PLANE ( 'NONE',  #13147 ) ;
#21228 = LINE ( 'NONE', #97326, #106317 ) ;
#21229 = EDGE_CURVE ( 'NONE', #49159, #142584, #132850, .T. ) ;
#21230 = ORIENTED_EDGE ( 'NONE', *, *, #134713, .T. ) ;
#21231 =( BOUNDED_CURVE ( )  B_SPLINE_CURVE ( 3, ( #41719, #29402, #40321, #139642 ),
 .UNSPECIFIED., .F., .T. ) 
 B_SPLINE_CURVE_WITH_KNOTS ( ( 4, 4 ),
 ( 1.901594255663598299, 1.933014472006547635 ),
 .UNSPECIFIED. ) 
 CURVE ( )  GEOMETRIC_REPRESENTATION_ITEM ( )  RATIONAL_B_SPLINE_CURVE ( ( 1.000000000000000000, 0.9999177325257868620, 0.9999177325257868620, 1.000000000000000000 ) ) 
 REPRESENTATION_ITEM ( '' )  );
#21232 = CARTESIAN_POINT ( 'NONE',  ( -2.700255128608413990, -27.71228299555204089, 4.000000000000000000 ) ) ;
#21233 = CARTESIAN_POINT ( 'NONE',  ( -39.48921356237310221, -27.52281430457082934, 5.000000000000000000 ) ) ;
#21234 = CARTESIAN_POINT ( 'NONE',  ( 5.901564193917593570, 11.25929247661560240, 10.79108189686408359 ) ) ;
#21235 = LINE ( 'NONE', #40175, #3639 ) ;
#21236 = ORIENTED_EDGE ( 'NONE', *, *, #23124, .T. ) ;
#21237 = CARTESIAN_POINT ( 'NONE',  ( -12.69999999999998153, 0.000000000000000000, 0.000000000000000000 ) ) ;
#21238 = PLANE ( 'NONE',  #35271 ) ;
#21239 = ADVANCED_FACE ( 'NONE', ( #11722 ), #86223, .T. ) ;
#21241 = VECTOR ( 'NONE', #61725, 1000.000000000000000 ) ;
#21240 = CARTESIAN_POINT ( 'NONE',  ( 79.02083333333331439, 7.949999999999998401, 2.130196079827431532 ) ) ;
#21242 = LINE ( 'NONE', #108937, #128906 ) ;
#21243 = DIRECTION ( 'NONE',  ( 1.000000000000000000, 0.000000000000000000, 0.000000000000000000 ) ) ;
#21244 = CARTESIAN_POINT ( 'NONE',  ( 5.068407645496677105, 3.061616997868380183E-16, -2.500000000000001332 ) ) ;
#21245 = FACE_OUTER_BOUND ( 'NONE', #16314, .T. ) ;
#21246 = CARTESIAN_POINT ( 'NONE',  ( 58.85002705046289151, -5.819803920172572198, -5.819803920172572198 ) ) ;
#21247 = CARTESIAN_POINT ( 'NONE',  ( -31.49999999999978684, -20.94781430457059912, 5.000000000000000000 ) ) ;
#21248 = CARTESIAN_POINT ( 'NONE',  ( 72.18398860626899705, 28.73617430169837661, 5.000000000000000000 ) ) ;
#21249 = ORIENTED_EDGE ( 'NONE', *, *, #40569, .T. ) ;
#21250 = VERTEX_POINT ( 'NONE', #130447 ) ;
#21251 = CARTESIAN_POINT ( 'NONE',  ( 55.10416666666665009, 2.130196079827422206, 7.950000000000001954 ) ) ;
#21252 = DIRECTION ( 'NONE',  ( -0.000000000000000000, 0.000000000000000000, 1.000000000000000000 ) ) ;
#21253 = PLANE ( 'NONE',  #73997 ) ;
#21254 = ADVANCED_FACE ( 'NONE', ( #42007 ), #74641, .F. ) ;
#21255 = CARTESIAN_POINT ( 'NONE',  ( 17.54840764549667398, -2.500000000000000888, 0.000000000000000000 ) ) ;
#21256 = ORIENTED_EDGE ( 'NONE', *, *, #107927, .F. ) ;
#21257 = AXIS2_PLACEMENT_3D ( 'NONE', #123594, #24249, #88808 ) ;
#21258 = CARTESIAN_POINT ( 'NONE',  ( 127.0000000000000000, -4.017717506652945580, -5.045834523320674059 ) ) ;
#21260 = EDGE_CURVE ( 'NONE', #74923, #75266, #88372, .T. ) ;
#21259 = CARTESIAN_POINT ( 'NONE',  ( 13.27644930412397350, 4.689949953678146599, 5.000000000000000000 ) ) ;
#21262 = EDGE_CURVE ( 'NONE', #132813, #53796, #20210, .T. ) ;
#21261 = AXIS2_PLACEMENT_3D ( 'NONE', #75223, #119385, #141908 ) ;
#21263 = VECTOR ( 'NONE', #74096, 1000.000000000000000 ) ;
#21264 = CARTESIAN_POINT ( 'NONE',  ( 49.00043019189810423, -3.055000000000002380, 5.291415217122920289 ) ) ;
#21265 = ORIENTED_EDGE ( 'NONE', *, *, #5808, .T. ) ;
#21266 = ORIENTED_EDGE ( 'NONE', *, *, #47497, .F. ) ;
#21267 = ORIENTED_EDGE ( 'NONE', *, *, #107012, .F. ) ;
#21268 = VECTOR ( 'NONE', #112027, 1000.000000000000227 ) ;
#21269 = VECTOR ( 'NONE', #70875, 1000.000000000000000 ) ;
#21270 = CARTESIAN_POINT ( 'NONE',  ( 2.999999999999999112, 1.194621026894846283, 17.40906030209848510 ) ) ;
#21271 = EDGE_CURVE ( 'NONE', #84890, #30995, #33305, .T. ) ;
#21272 = LINE ( 'NONE', #11794, #110170 ) ;
#21273 = DIRECTION ( 'NONE',  ( -0.7071067811865486830, 0.7071067811865464625, 0.000000000000000000 ) ) ;
#21274 = CARTESIAN_POINT ( 'NONE',  ( 27.72281430457040940, -21.72500000000000142, 5.000000000000000000 ) ) ;
#21275 = ORIENTED_EDGE ( 'NONE', *, *, #105529, .F. ) ;
#21276 = EDGE_CURVE ( 'NONE', #124568, #61398, #9310, .T. ) ;
#21277 = PLANE ( 'NONE',  #26687 ) ;
#21278 = CARTESIAN_POINT ( 'NONE',  ( 27.48921356237309155, -27.52281430457074762, 5.000000000000000000 ) ) ;
#21280 = ORIENTED_EDGE ( 'NONE', *, *, #48904, .F. ) ;
#21279 = DIRECTION ( 'NONE',  ( 1.000000000000000000, 1.224606353822377258E-16, 0.000000000000000000 ) ) ;
#21281 = CARTESIAN_POINT ( 'NONE',  ( 83.70876352523143282, -7.482591942790329030E-16, 6.110000000000001208 ) ) ;
#21282 = EDGE_CURVE ( 'NONE', #34476, #65821, #104082, .T. ) ;
#21283 = DIRECTION ( 'NONE',  ( 0.000000000000000000, -1.000000000000000000, 0.000000000000000000 ) ) ;
#21284 = DIRECTION ( 'NONE',  ( 1.000000000000000000, 0.000000000000000000, 0.000000000000000000 ) ) ;
#21285 = CARTESIAN_POINT ( 'NONE',  ( 14.24139925780194105, 21.72500000000000142, 5.000000000000000000 ) ) ;
#21286 = CARTESIAN_POINT ( 'NONE',  ( -11.28769006033965461, -21.73547319004782352, 4.999917730833664642 ) ) ;
#21287 = FACE_OUTER_BOUND ( 'NONE', #76635, .T. ) ;
#21288 = EDGE_LOOP ( 'NONE', ( #59361, #93880, #143032, #29362 ) ) ;
#21289 = ADVANCED_FACE ( 'NONE', ( #42733 ), #74011, .T. ) ;
#21290 = LINE ( 'NONE', #54644, #47710 ) ;
#21291 = CARTESIAN_POINT ( 'NONE',  ( 68.45376352523143737, -6.109999999999998543, -3.741295971395162543E-16 ) ) ;
#21292 = CARTESIAN_POINT ( 'NONE',  ( 0.000000000000000000, 0.000000000000000000, 5.000000000000000000 ) ) ;
#21293 = DIRECTION ( 'NONE',  ( 0.6830127018922181881, 0.6830127018922202975, -0.2588190451025214056 ) ) ;
#21294 = CARTESIAN_POINT ( 'NONE',  ( -23.29298673570678702, -21.74070752338405299, 4.999753212805217117 ) ) ;
#21295 = ORIENTED_EDGE ( 'NONE', *, *, #108774, .T. ) ;
#21296 = ORIENTED_EDGE ( 'NONE', *, *, #70876, .T. ) ;
#21297 = PLANE ( 'NONE',  #97900 ) ;
#21298 = EDGE_CURVE ( 'NONE', #37141, #38602, #142734, .T. ) ;
#21299 = VERTEX_POINT ( 'NONE', #109387 ) ;
#21300 = VECTOR ( 'NONE', #5600, 1000.000000000000227 ) ;
#21301 = VERTEX_POINT ( 'NONE', #32555 ) ;
#21302 = MECHANICAL_DESIGN_GEOMETRIC_PRESENTATION_REPRESENTATION (  '', ( #51425 ), #58399 ) ;
#21303 = DIRECTION ( 'NONE',  ( 0.3543493200069162685, -0.000000000000000000, -0.9351131265310288487 ) ) ;
#21304 = ORIENTED_EDGE ( 'NONE', *, *, #57517, .T. ) ;
#21305 = VECTOR ( 'NONE', #44196, 1000.000000000000000 ) ;
#21306 = DIRECTION ( 'NONE',  ( -0.6830127018922180770, -0.6830127018922204085, -0.2588190451025213501 ) ) ;
#21307 = CARTESIAN_POINT ( 'NONE',  ( -11.99999999999990941, 17.96639925780208102, 5.000000000000000000 ) ) ;
#21308 = AXIS2_PLACEMENT_3D ( 'NONE', #138216, #17829, #62100 ) ;
#21309 = CARTESIAN_POINT ( 'NONE',  ( -13.43312800248734185, -21.74070752338406010, 6.915939825044106648 ) ) ;
#21310 = FACE_BOUND ( 'NONE', #136050, .T. ) ;
#21311 = DIRECTION ( 'NONE',  ( 0.6830127018922181881, 0.6830127018922202975, -0.2588190451025214056 ) ) ;
#21312 = CARTESIAN_POINT ( 'NONE',  ( 41.78752705046289151, 0.000000000000000000, -7.949999999999998401 ) ) ;
#21313 = CARTESIAN_POINT ( 'NONE',  ( 0.000000000000000000, 0.000000000000000000, 0.000000000000000000 ) ) ;
#21315 = EDGE_LOOP ( 'NONE', ( #121607, #8102, #124009, #109492, #56336, #13819, #34981, #37441, #114223, #79966, #7146, #84160, #52749, #44165, #61796, #143284, #91928, #140214, #88445, #47978 ) ) ;
#21314 = CARTESIAN_POINT ( 'NONE',  ( -11.29289321881337571, -15.74070752338412404, 5.000000000000000000 ) ) ;
#21316 = AXIS2_PLACEMENT_3D ( 'NONE', #88744, #132976, #11847 ) ;
#21317 = FACE_OUTER_BOUND ( 'NONE', #24839, .T. ) ;
#21318 = ORIENTED_EDGE ( 'NONE', *, *, #86028, .F. ) ;
#21319 = ADVANCED_FACE ( 'NONE', ( #10065 ), #43425, .T. ) ;
#21320 = ORIENTED_EDGE ( 'NONE', *, *, #94026, .F. ) ;
#21321 = CARTESIAN_POINT ( 'NONE',  ( 87.99543019189812298, 5.291415217122916737, 3.055000000000001936 ) ) ;
#21322 = EDGE_LOOP ( 'NONE', ( #56031, #56207, #113474, #107299 ) ) ;
#21323 = DIRECTION ( 'NONE',  ( -0.7071067811865486830, -0.7071067811865464625, -0.000000000000000000 ) ) ;
#21324 = DIRECTION ( 'NONE',  ( 0.000000000000000000, 1.000000000000000000, -0.000000000000000000 ) ) ;
#21325 = VECTOR ( 'NONE', #138976, 1000.000000000000000 ) ;
#21326 = VERTEX_POINT ( 'NONE', #65922 ) ;
#21327 = DIRECTION ( 'NONE',  ( -0.7071067811865487940, 0.7071067811865463515, -0.000000000000000000 ) ) ;
#21328 = AXIS2_PLACEMENT_3D ( 'NONE', #28189, #69581, #17299 ) ;
#21329 = EDGE_CURVE ( 'NONE', #57666, #2587, #77508, .T. ) ;
#21330 = DIRECTION ( 'NONE',  ( -1.000000000000000000, -0.000000000000000000, -0.000000000000000000 ) ) ;
#21331 = LINE ( 'NONE', #76438, #78511 ) ;
#21332 = CARTESIAN_POINT ( 'NONE',  ( 17.39159235450332019, 2.500000000000001332, 0.000000000000000000 ) ) ;
#21333 = DIRECTION ( 'NONE',  ( -0.7071067811865486830, -0.7071067811865464625, 0.000000000000000000 ) ) ;
#21334 = CARTESIAN_POINT ( 'NONE',  ( 27.09667064187388874, -2.240707523384257716, 15.26439735382758833 ) ) ;
#21335 = DIRECTION ( 'NONE',  ( -0.3543493200069162685, -0.000000000000000000, -0.9351131265310288487 ) ) ;
#21336 = CARTESIAN_POINT ( 'NONE',  ( -34.92500000000001137, 14.81665438641027777, 4.500000000000000888 ) ) ;
#21337 = ORIENTED_EDGE ( 'NONE', *, *, #74466, .F. ) ;
#21338 = AXIS2_PLACEMENT_3D ( 'NONE', #93420, #60092, #59397 ) ;
#21339 = PRESENTATION_STYLE_ASSIGNMENT (( #53997 ) ) ;
#21340 = ORIENTED_EDGE ( 'NONE', *, *, #87704, .F. ) ;
#21341 = DIRECTION ( 'NONE',  ( 0.7071067811865487940, -0.7071067811865463515, 0.000000000000000000 ) ) ;
#21342 = CARTESIAN_POINT ( 'NONE',  ( 12.69999999999999574, -22.33999999999998565, 3.000000000000000000 ) ) ;
#21343 = VERTEX_POINT ( 'NONE', #63064 ) ;
#21344 = VERTEX_POINT ( 'NONE', #107237 ) ;
#21345 = CARTESIAN_POINT ( 'NONE',  ( 33.54209685856476852, 5.291415217122923842, -3.054999999999996163 ) ) ;
#21346 = VECTOR ( 'NONE', #133400, 1000.000000000000227 ) ;
#21347 = ORIENTED_EDGE ( 'NONE', *, *, #113697, .T. ) ;
#21348 = FACE_OUTER_BOUND ( 'NONE', #11246, .T. ) ;
#21349 = CARTESIAN_POINT ( 'NONE',  ( -56.99451991528749062, 28.92564299267978001, 4.000000000000000000 ) ) ;
#21350 = CARTESIAN_POINT ( 'NONE',  ( 22.64997294953710139, -4.461849672132299105, 4.461849672132299993 ) ) ;
#21351 = CARTESIAN_POINT ( 'NONE',  ( 10.20209588485037777, 11.26426916695988467, -26.13888605657682973 ) ) ;
#21352 = EDGE_LOOP ( 'NONE', ( #88651, #26838, #93729, #126775 ) ) ;
#21353 = DIRECTION ( 'NONE',  ( -1.000000000000000000, -0.000000000000000000, -0.000000000000000000 ) ) ;
#21354 = EDGE_LOOP ( 'NONE', ( #3642, #100845, #40949, #41734 ) ) ;
#21355 = PLANE ( 'NONE',  #85837 ) ;
#21356 = LINE ( 'NONE', #98210, #114626 ) ;
#21357 = AXIS2_PLACEMENT_3D ( 'NONE', #39418, #69936, #38693 ) ;
#21358 = VECTOR ( 'NONE', #111212, 1000.000000000000000 ) ;
#21360 = ORIENTED_EDGE ( 'NONE', *, *, #51785, .F. ) ;
#21359 = CARTESIAN_POINT ( 'NONE',  ( 1.828169399223519953, 15.75929247661555443, 4.000000000000000000 ) ) ;
#21361 = VECTOR ( 'NONE', #134729, 1000.000000000000227 ) ;
#21362 = ORIENTED_EDGE ( 'NONE', *, *, #11552, .T. ) ;
#21363 = DIRECTION ( 'NONE',  ( 0.000000000000000000, 1.000000000000000000, -1.224646799147353207E-16 ) ) ;
#21364 = LINE ( 'NONE', #133700, #67765 ) ;
#21365 = VECTOR ( 'NONE', #112650, 1000.000000000000227 ) ;
#21366 = CARTESIAN_POINT ( 'NONE',  ( -24.98911971346034377, -22.02621442084248216, 4.990779571109220214 ) ) ;
#21368 = ORIENTED_EDGE ( 'NONE', *, *, #15378, .T. ) ;
#21367 = VECTOR ( 'NONE', #110096, 999.9999999999998863 ) ;
#21369 = DIRECTION ( 'NONE',  ( 0.000000000000000000, -1.000000000000000000, 0.000000000000000000 ) ) ;
#21370 = ORIENTED_EDGE ( 'NONE', *, *, #114039, .F. ) ;
#21371 = VERTEX_POINT ( 'NONE', #89853 ) ;
#21372 = DIRECTION ( 'NONE',  ( -0.7071067811865487940, 0.7071067811865463515, 0.000000000000000000 ) ) ;
#21373 = CARTESIAN_POINT ( 'NONE',  ( -19.49999999999987210, -4.216083040037264418, -7.486842126848610945 ) ) ;
#21374 = PRESENTATION_LAYER_ASSIGNMENT (  '', '', ( #125603 ) ) ;
#21375 = FACE_OUTER_BOUND ( 'NONE', #49474, .T. ) ;
#21376 = LINE ( 'NONE', #133019, #132684 ) ;
#21377 = DIRECTION ( 'NONE',  ( 1.000000000000000000, 0.000000000000000000, 0.000000000000000000 ) ) ;
#21378 = EDGE_CURVE ( 'NONE', #118711, #8834, #57271, .T. ) ;
#21379 = DIRECTION ( 'NONE',  ( -0.7071067811865486830, 0.7071067811865464625, 0.000000000000000000 ) ) ;
#21380 = CARTESIAN_POINT ( 'NONE',  ( -0.4892135623730947680, -27.52281430457055578, 5.000000000000000000 ) ) ;
#21381 = EDGE_CURVE ( 'NONE', #75731, #138987, #113759, .T. ) ;
#21383 = EDGE_LOOP ( 'NONE', ( #33975, #5445, #115443, #2240 ) ) ;
#21382 = EDGE_CURVE ( 'NONE', #122903, #96758, #136217, .T. ) ;
#21384 = LINE ( 'NONE', #65644, #99880 ) ;
#21385 = ORIENTED_EDGE ( 'NONE', *, *, #81843, .T. ) ;
#21386 = DIRECTION ( 'NONE',  ( -0.7071067811865487940, 0.7071067811865463515, -0.000000000000000000 ) ) ;
#21387 = EDGE_CURVE ( 'NONE', #50737, #78330, #45684, .T. ) ;
#21388 = EDGE_CURVE ( 'NONE', #30943, #71410, #67429, .T. ) ;
#21389 = DIRECTION ( 'NONE',  ( -0.6830127018922181881, 0.6830127018922202975, -0.2588190451025214056 ) ) ;
#21390 = LINE ( 'NONE', #67039, #20692 ) ;
#21391 = ORIENTED_EDGE ( 'NONE', *, *, #15540, .F. ) ;
#21392 = LINE ( 'NONE', #119249, #36793 ) ;
#21393 = PLANE ( 'NONE',  #118209 ) ;
#21394 = CARTESIAN_POINT ( 'NONE',  ( -17.99451991528748351, 28.92564299267950645, 4.000000000000000000 ) ) ;
#21395 = ORIENTED_EDGE ( 'NONE', *, *, #59320, .T. ) ;
#21396 = ORIENTED_EDGE ( 'NONE', *, *, #111910, .F. ) ;
#21397 = EDGE_CURVE ( 'NONE', #28705, #87694, #134099, .T. ) ;
#21398 = CARTESIAN_POINT ( 'NONE',  ( 55.18164086290604331, -52.14999999999999147, 41.64499999999997470 ) ) ;
#21399 = DIRECTION ( 'NONE',  ( -0.7071067811865487940, 0.7071067811865463515, 0.000000000000000000 ) ) ;
#21400 = DIRECTION ( 'NONE',  ( -0.7071067811865487940, 0.7071067811865463515, -0.000000000000000000 ) ) ;
#21401 = DIRECTION ( 'NONE',  ( 1.000000000000000000, 0.000000000000000000, 0.000000000000000000 ) ) ;
#21402 = CARTESIAN_POINT ( 'NONE',  ( 65.97459685856479439, 1.637169565754164280, -6.109999999999997655 ) ) ;
#21403 = DIRECTION ( 'NONE',  ( 0.7071067811865487940, 0.7071067811865463515, 0.000000000000000000 ) ) ;
#21404 = EDGE_CURVE ( 'NONE', #53303, #117033, #1396, .T. ) ;
#21405 = DIRECTION ( 'NONE',  ( 1.369518533665900312E-16, -1.000000000000000000, 0.000000000000000000 ) ) ;
#21406 = DIRECTION ( 'NONE',  ( -0.7071067811865486830, 0.7071067811865464625, 0.000000000000000000 ) ) ;
#21407 = CARTESIAN_POINT ( 'NONE',  ( 15.48921356237309510, -27.52281430457066236, 5.000000000000000000 ) ) ;
#21408 = PRESENTATION_LAYER_ASSIGNMENT (  '', '', ( #33030 ) ) ;
#21409 = EDGE_LOOP ( 'NONE', ( #36254, #48829, #9129, #64542 ) ) ;
#21410 = DIRECTION ( 'NONE',  ( -0.7071067811865486830, -0.7071067811865464625, -0.000000000000000000 ) ) ;
#21411 = ORIENTED_EDGE ( 'NONE', *, *, #93165, .T. ) ;
#21412 = PLANE ( 'NONE',  #47780 ) ;
#21414 = AXIS2_PLACEMENT_3D ( 'NONE', #103609, #36253, #49291 ) ;
#21413 = FACE_OUTER_BOUND ( 'NONE', #62760, .T. ) ;
#21415 = CARTESIAN_POINT ( 'NONE',  ( 32.20710678118632586, 15.75929247661555443, 5.000000000000000000 ) ) ;
#21416 = FACE_OUTER_BOUND ( 'NONE', #101919, .T. ) ;
#21417 = FILL_AREA_STYLE_COLOUR ( '', #13751 ) ;
#21418 = LINE ( 'NONE', #64930, #99560 ) ;
#21419 = LINE ( 'NONE', #19272, #63470 ) ;
#21420 = VERTEX_POINT ( 'NONE', #124634 ) ;
#21421 = EDGE_LOOP ( 'NONE', ( #52426, #103842, #90041, #24127, #20972 ) ) ;
#21422 = PLANE ( 'NONE',  #71827 ) ;
#21423 = DIRECTION ( 'NONE',  ( 0.000000000000000000, 0.000000000000000000, 1.000000000000000000 ) ) ;
#21424 = UNCERTAINTY_MEASURE_WITH_UNIT (LENGTH_MEASURE( 1.000000000000000082E-05 ), #3737, 'distance_accuracy_value', 'NONE');
#21425 = EDGE_CURVE ( 'NONE', #94597, #108664, #90594, .T. ) ;
#21426 = DIRECTION ( 'NONE',  ( 0.7071067811865487940, 0.7071067811865463515, 0.000000000000000000 ) ) ;
#21427 = CARTESIAN_POINT ( 'NONE',  ( 15.79580628287043709, -5.278424836066144543, 3.047499999999995879 ) ) ;
#21428 = CARTESIAN_POINT ( 'NONE',  ( 85.97502705046288440, -5.819803920172572198, 5.819803920172572198 ) ) ;
#21429 = DIRECTION ( 'NONE',  ( 0.3543493200069162685, -0.000000000000000000, -0.9351131265310288487 ) ) ;
#21430 = LINE ( 'NONE', #30146, #57661 ) ;
#21431 = ORIENTED_EDGE ( 'NONE', *, *, #33078, .F. ) ;
#21432 = CARTESIAN_POINT ( 'NONE',  ( 81.64583333333332860, 2.130196079827431976, -7.949999999999999289 ) ) ;
#21433 = LINE ( 'NONE', #76545, #118689 ) ;
#21434 = FACE_OUTER_BOUND ( 'NONE', #46842, .T. ) ;
#21435 = PLANE ( 'NONE',  #102962 ) ;
#21436 = ADVANCED_FACE ( 'NONE', ( #36902 ), #68858, .F. ) ;
#21437 = CONICAL_SURFACE ( 'NONE', #127933, 2.055000000000000604, 0.9599310885968764806 ) ;
#21438 = ORIENTED_EDGE ( 'NONE', *, *, #23323, .T. ) ;
#21439 = DIRECTION ( 'NONE',  ( -0.7071067811865486830, -0.7071067811865464625, 0.000000000000000000 ) ) ;
#21440 = EDGE_CURVE ( 'NONE', #127258, #127118, #92705, .T. ) ;
#21441 = ORIENTED_EDGE ( 'NONE', *, *, #72946, .F. ) ;
#21442 = CARTESIAN_POINT ( 'NONE',  ( 74.37543019189810423, -5.291415217122920289, -3.055000000000001492 ) ) ;
#21443 = EDGE_CURVE ( 'NONE', #99753, #23695, #67087, .T. ) ;
#21444 = ORIENTED_EDGE ( 'NONE', *, *, #87858, .F. ) ;
#21445 = AXIS2_PLACEMENT_3D ( 'NONE', #62308, #106467, #63039 ) ;
#21446 = FACE_OUTER_BOUND ( 'NONE', #28992, .T. ) ;
#21447 = EDGE_CURVE ( 'NONE', #2711, #41375, #58730, .T. ) ;
#21448 = DIRECTION ( 'NONE',  ( 0.7071067811865486830, -0.7071067811865464625, -0.000000000000000000 ) ) ;
#21449 = CARTESIAN_POINT ( 'NONE',  ( -7.499999999999958256, 16.08746187583909659, 4.000000000000000000 ) ) ;
#21450 = CARTESIAN_POINT ( 'NONE',  ( 0.03865117921958875769, -0.3999999999999998002, -2.083945894980139268 ) ) ;
#21451 = CARTESIAN_POINT ( 'NONE',  ( 55.18164086290604331, -52.14999999999999147, 41.64499999999997470 ) ) ;
#21453 = VERTEX_POINT ( 'NONE', #113027 ) ;
#21452 = CARTESIAN_POINT ( 'NONE',  ( -23.51078643762690490, -27.52281430457038880, 5.000000000000000000 ) ) ;
#21454 = CARTESIAN_POINT ( 'NONE',  ( 6.938893903907228378E-15, -19.44781430457063465, 5.000000000000000000 ) ) ;
#21455 = CARTESIAN_POINT ( 'NONE',  ( -57.18398860626899705, 28.73617430169827358, 5.000000000000000000 ) ) ;
#21456 = AXIS2_PLACEMENT_3D ( 'NONE', #132171, #21951, #32122 ) ;
#21457 = CARTESIAN_POINT ( 'NONE',  ( 76.54166666666667140, -3.975000000000002753, 6.884901960086286188 ) ) ;
#21458 = DIRECTION ( 'NONE',  ( 0.000000000000000000, 0.000000000000000000, -1.000000000000000000 ) ) ;
#21459 = EDGE_LOOP ( 'NONE', ( #133198, #15452, #128475, #84842, #26231 ) ) ;
#21460 = ORIENTED_EDGE ( 'NONE', *, *, #50499, .T. ) ;
#21461 = CARTESIAN_POINT ( 'NONE',  ( 66.50043019189810423, -3.055000000000002380, 5.291415217122920289 ) ) ;
#21462 = ORIENTED_EDGE ( 'NONE', *, *, #124486, .F. ) ;
#21463 = EDGE_CURVE ( 'NONE', #39863, #5780, #12295, .T. ) ;
#21464 = LINE ( 'NONE', #117869, #54514 ) ;
#21465 = DIRECTION ( 'NONE',  ( -0.6830127018922180770, -0.6830127018922204085, -0.2588190451025213501 ) ) ;
#21466 = DIRECTION ( 'NONE',  ( 0.000000000000000000, 0.000000000000000000, 1.000000000000000000 ) ) ;
#21467 = FILL_AREA_STYLE_COLOUR ( '', #77905 ) ;
#21468 = ORIENTED_EDGE ( 'NONE', *, *, #80186, .T. ) ;
#21469 = ORIENTED_EDGE ( 'NONE', *, *, #117723, .F. ) ;
#21470 = AXIS2_PLACEMENT_3D ( 'NONE', #120469, #78447, #21195 ) ;
#21471 = AXIS2_PLACEMENT_3D ( 'NONE', #114018, #80006, #35059 ) ;
#21472 = DIRECTION ( 'NONE',  ( -0.000000000000000000, 0.3543493200069153248, 0.9351131265310292928 ) ) ;
#21473 = CARTESIAN_POINT ( 'NONE',  ( -27.18398860626900060, 28.73617430169806042, 5.000000000000000000 ) ) ;
#21474 = VECTOR ( 'NONE', #94287, 1000.000000000000000 ) ;
#21475 = CIRCLE ( 'NONE', #91130, 2.500000000000000444 ) ;
#21476 = EDGE_LOOP ( 'NONE', ( #11148, #78784, #120786, #38436 ) ) ;
#21477 = DIRECTION ( 'NONE',  ( -0.6830127018922181881, 0.6830127018922202975, -0.2588190451025214056 ) ) ;
#21479 = CARTESIAN_POINT ( 'NONE',  ( 51.18398860626899705, 28.73617430169823095, 5.000000000000000000 ) ) ;
#21478 = COLOUR_RGB ( '', 0.08235294, 0.09019608, 0.10196078) ;
#21480 = CARTESIAN_POINT ( 'NONE',  ( -2.292893218813435219, -3.740707523384248390, 5.000000000000000000 ) ) ;
#21481 = STYLED_ITEM ( 'NONE', ( #29791 ), #66477 ) ;
#21482 = MECHANICAL_DESIGN_GEOMETRIC_PRESENTATION_REPRESENTATION (  '', ( #107047 ), #123324 ) ;
#21483 = ORIENTED_EDGE ( 'NONE', *, *, #109193, .T. ) ;
#21484 = EDGE_CURVE ( 'NONE', #15691, #6909, #15134, .T. ) ;
#21485 = DIRECTION ( 'NONE',  ( -0.7071067811865486830, 0.7071067811865464625, 0.000000000000000000 ) ) ;
#21486 = LINE ( 'NONE', #140398, #89456 ) ;
#21487 = EDGE_CURVE ( 'NONE', #36751, #117439, #13702, .T. ) ;
#21488 = CARTESIAN_POINT ( 'NONE',  ( 128.5969355792471447, -3.174999999999999378, -5.499261314031185677 ) ) ;
#21489 = CARTESIAN_POINT ( 'NONE',  ( 60.93750000000000000, 5.819803920172574863, -5.819803920172573086 ) ) ;
#21490 = DIRECTION ( 'NONE',  ( -0.6830127018922181881, 0.6830127018922202975, -0.2588190451025214056 ) ) ;
#21491 = DIRECTION ( 'NONE',  ( 1.301042606982605074E-16, -1.000000000000000000, 0.000000000000000000 ) ) ;
#21492 = SURFACE_STYLE_USAGE ( .BOTH. , #98343 ) ;
#21493 = EDGE_LOOP ( 'NONE', ( #25423, #69122, #98367, #55278 ) ) ;
#21494 = ADVANCED_FACE ( 'NONE', ( #135530 ), #125359, .T. ) ;
#21495 = VECTOR ( 'NONE', #128559, 1000.000000000000000 ) ;
#21496 = ORIENTED_EDGE ( 'NONE', *, *, #26001, .F. ) ;
#21497 = CARTESIAN_POINT ( 'NONE',  ( 109.1412635252314374, 4.472830434245835818, 4.472830434245840259 ) ) ;
#21498 = ORIENTED_EDGE ( 'NONE', *, *, #122931, .F. ) ;
#21499 = VERTEX_POINT ( 'NONE', #59416 ) ;
#21500 = CARTESIAN_POINT ( 'NONE',  ( 180.9285571751892121, -48.88296141031990061, 39.14553452061912253 ) ) ;
#21501 = EDGE_CURVE ( 'NONE', #132203, #60612, #102898, .T. ) ;
#21502 = PLANE ( 'NONE',  #47810 ) ;
#21504 = ADVANCED_FACE ( 'NONE', ( #70309 ), #103574, .T. ) ;
#21503 = DIRECTION ( 'NONE',  ( 0.7071067811865486830, -0.7071067811865464625, -0.000000000000000000 ) ) ;
#21505 = ORIENTED_EDGE ( 'NONE', *, *, #92284, .T. ) ;
#21506 = DIRECTION ( 'NONE',  ( 1.000000000000000000, 0.000000000000000000, 0.000000000000000000 ) ) ;
#21507 = LINE ( 'NONE', #131694, #109831 ) ;
#21509 = DIRECTION ( 'NONE',  ( -0.000000000000000000, 0.000000000000000000, 1.000000000000000000 ) ) ;
#21508 = LINE ( 'NONE', #1147, #98920 ) ;
#21510 = DIRECTION ( 'NONE',  ( -0.6830127018922181881, 0.6830127018922202975, -0.2588190451025214056 ) ) ;
#21511 = VECTOR ( 'NONE', #51242, 1000.000000000000000 ) ;
#21512 = DIRECTION ( 'NONE',  ( -0.7071067811865487940, 0.7071067811865463515, -0.000000000000000000 ) ) ;
#21513 = ORIENTED_EDGE ( 'NONE', *, *, #67389, .T. ) ;
#21514 = PLANE ( 'NONE',  #68094 ) ;
#21515 = FACE_OUTER_BOUND ( 'NONE', #132649, .T. ) ;
#21516 = ORIENTED_EDGE ( 'NONE', *, *, #87459, .F. ) ;
#21517 = ORIENTED_EDGE ( 'NONE', *, *, #77123, .F. ) ;
#21518 = ADVANCED_FACE ( 'NONE', ( #8351 ), #75109, .F. ) ;
#21519 = ORIENTED_EDGE ( 'NONE', *, *, #129201, .T. ) ;
#21520 = CARTESIAN_POINT ( 'NONE',  ( 64.45876352523144703, 0.000000000000000000, -6.110000000000001208 ) ) ;
#21521 = ORIENTED_EDGE ( 'NONE', *, *, #19927, .F. ) ;
#21522 = VECTOR ( 'NONE', #2089, 1000.000000000000227 ) ;
#21523 = CARTESIAN_POINT ( 'NONE',  ( 18.18398860626898994, 28.73617430169800002, 5.000000000000000000 ) ) ;
#21524 = CARTESIAN_POINT ( 'NONE',  ( 0.3374729495371057708, 6.094999999999989981, -1.119633336120465690E-15 ) ) ;
#21525 = CARTESIAN_POINT ( 'NONE',  ( 97.41709685856478984, 3.054999999999998828, 5.291415217122922066 ) ) ;
#21526 = DIRECTION ( 'NONE',  ( -0.7071067811865487940, 0.7071067811865463515, 0.000000000000000000 ) ) ;
#21527 = VECTOR ( 'NONE', #90307, 1000.000000000000000 ) ;
#21528 = ORIENTED_EDGE ( 'NONE', *, *, #66758, .F. ) ;
#21529 = CARTESIAN_POINT ( 'NONE',  ( -23.29289321881329400, 11.25929247661559707, 5.000000000000000000 ) ) ;
#21530 = CONICAL_SURFACE ( 'NONE', #28480, 2.500000000000000444, 0.9599310885968830309 ) ;
#21531 = LINE ( 'NONE', #65794, #70288 ) ;
#21532 = DIRECTION ( 'NONE',  ( 0.000000000000000000, 1.000000000000000000, 0.000000000000000000 ) ) ;
#21533 = CARTESIAN_POINT ( 'NONE',  ( 152.4000000000000057, -17.48000000000005016, -12.70000000000043272 ) ) ;
#21534 = VERTEX_POINT ( 'NONE', #30132 ) ;
#21535 = CARTESIAN_POINT ( 'NONE',  ( 19.73159235450332005, -2.500000000000000444, 3.061616997868384620E-16 ) ) ;
#21536 = ORIENTED_EDGE ( 'NONE', *, *, #54325, .F. ) ;
#21537 = VERTEX_POINT ( 'NONE', #49247 ) ;
#21538 = ORIENTED_EDGE ( 'NONE', *, *, #67424, .T. ) ;
#21539 = CARTESIAN_POINT ( 'NONE',  ( 119.3495968585647944, 6.109999999999996767, 1.637169565754163836 ) ) ;
#21541 = ORIENTED_EDGE ( 'NONE', *, *, #31406, .T. ) ;
#21540 = AXIS2_PLACEMENT_3D ( 'NONE', #41802, #52662, #44705 ) ;
#21542 = EDGE_CURVE ( 'NONE', #23904, #47125, #9049, .T. ) ;
#21543 = PLANE ( 'NONE',  #28345 ) ;
#21544 = LINE ( 'NONE', #20090, #18539 ) ;
#21545 = ADVANCED_FACE ( 'NONE', ( #85954 ), #93440, .T. ) ;
#21546 = VERTEX_POINT ( 'NONE', #74386 ) ;
#21547 = DIRECTION ( 'NONE',  ( 1.000000000000000000, 0.000000000000000000, 0.000000000000000000 ) ) ;
#21548 = VECTOR ( 'NONE', #102763, 1000.000000000000000 ) ;
#21549 = ORIENTED_EDGE ( 'NONE', *, *, #129668, .T. ) ;
#21550 = EDGE_CURVE ( 'NONE', #54699, #103560, #47352, .T. ) ;
#21551 = EDGE_CURVE ( 'NONE', #19553, #75708, #30880, .T. ) ;
#21552 = CARTESIAN_POINT ( 'NONE',  ( 15.43706980810188512, 2.126176841940952134, -7.934999999999993392 ) ) ;
#21553 = CARTESIAN_POINT ( 'NONE',  ( 29.99999999999979394, 1.552185695429152856, 5.000000000000000000 ) ) ;
#21554 = ADVANCED_FACE ( 'NONE', ( #64929 ), #97531, .T. ) ;
#21555 = DIRECTION ( 'NONE',  ( -0.000000000000000000, 1.000000000000000000, -0.000000000000000000 ) ) ;
#21556 = DIRECTION ( 'NONE',  ( -0.000000000000000000, -0.3543493200069152693, 0.9351131265310292928 ) ) ;
#21557 = VERTEX_POINT ( 'NONE', #130912 ) ;
#21558 = EDGE_LOOP ( 'NONE', ( #124030, #4507, #62677, #21817 ) ) ;
#21559 = ADVANCED_FACE ( 'NONE', ( #81889 ), #19270, .F. ) ;
#21560 = ORIENTED_EDGE ( 'NONE', *, *, #53348, .F. ) ;
#21561 = DIRECTION ( 'NONE',  ( -0.6830127018922180770, -0.6830127018922204085, -0.2588190451025213501 ) ) ;
#21562 = CARTESIAN_POINT ( 'NONE',  ( -15.18398860626900237, 28.73617430169797871, 5.000000000000000000 ) ) ;
#21563 = UNCERTAINTY_MEASURE_WITH_UNIT (LENGTH_MEASURE( 1.000000000000000082E-05 ), #129652, 'distance_accuracy_value', 'NONE');
#21564 = AXIS2_PLACEMENT_3D ( 'NONE', #102882, #3521, #14440 ) ;
#21565 = ADVANCED_FACE ( 'NONE', ( #86684 ), #53312, .F. ) ;
#21566 = DIRECTION ( 'NONE',  ( 0.7071067811865487940, 0.7071067811865463515, 0.000000000000000000 ) ) ;
#21567 = CARTESIAN_POINT ( 'NONE',  ( -22.49999999999984368, 22.01701374228153085, 2.453858888625680468 ) ) ;
#21568 = AXIS2_PLACEMENT_3D ( 'NONE', #130482, #84814, #118864 ) ;
#21569 = EDGE_CURVE ( 'NONE', #61826, #91561, #97997, .T. ) ;
#21570 = DIRECTION ( 'NONE',  ( 0.3543493200069162685, -0.000000000000000000, -0.9351131265310288487 ) ) ;
#21571 = CARTESIAN_POINT ( 'NONE',  ( 31.64626352523143638, -4.472830434245840259, 4.472830434245839371 ) ) ;
#21572 = CARTESIAN_POINT ( 'NONE',  ( -28.49999999999979394, -20.94781430457060623, 5.000000000000000000 ) ) ;
#21573 = CARTESIAN_POINT ( 'NONE',  ( 14.70692117890024697, 2.500000000000000888, 0.000000000000000000 ) ) ;
#21574 = ORIENTED_EDGE ( 'NONE', *, *, #37815, .F. ) ;
#21575 = DIRECTION ( 'NONE',  ( -1.000000000000000000, 0.000000000000000000, 0.000000000000000000 ) ) ;
#21576 = VECTOR ( 'NONE', #62486, 1000.000000000000000 ) ;
#21577 = ORIENTED_EDGE ( 'NONE', *, *, #135256, .T. ) ;
#21578 = LINE ( 'NONE', #110681, #22124 ) ;
#21579 = VERTEX_POINT ( 'NONE', #4947 ) ;
#21580 = EDGE_CURVE ( 'NONE', #123992, #38637, #115865, .T. ) ;
#21581 = CARTESIAN_POINT ( 'NONE',  ( 17.39997294953710494, 4.461849672132297329, -4.461849672132302658 ) ) ;
#21583 = ORIENTED_EDGE ( 'NONE', *, *, #20914, .T. ) ;
#21582 = LINE ( 'NONE', #33895, #127435 ) ;
#21584 = CARTESIAN_POINT ( 'NONE',  ( 23.14818355038130449, 17.25929247661554200, 8.802941693769255949 ) ) ;
#21585 = ORIENTED_EDGE ( 'NONE', *, *, #45221, .T. ) ;
#21586 = LINE ( 'NONE', #123771, #117904 ) ;
#21587 = VECTOR ( 'NONE', #66729, 1000.000000000000000 ) ;
#21588 = ORIENTED_EDGE ( 'NONE', *, *, #20429, .F. ) ;
#21589 = DIRECTION ( 'NONE',  ( 0.7071067811865487940, -0.7071067811865463515, 0.000000000000000000 ) ) ;
#21590 = ORIENTED_EDGE ( 'NONE', *, *, #127346, .F. ) ;
#21591 = EDGE_CURVE ( 'NONE', #79754, #51035, #64211, .T. ) ;
#21592 = LINE ( 'NONE', #88283, #26764 ) ;
#21593 = CARTESIAN_POINT ( 'NONE',  ( 113.5375270504628986, -9.735942053221456900E-16, 7.949999999999998401 ) ) ;
#21594 = DIRECTION ( 'NONE',  ( 0.3543493200069162685, -0.000000000000000000, -0.9351131265310288487 ) ) ;
#21595 = CARTESIAN_POINT ( 'NONE',  ( 11.67183060077639212, -3.740707523384244837, 4.000000000000000000 ) ) ;
#21596 = DIRECTION ( 'NONE',  ( -0.000000000000000000, 0.3543493200069153248, 0.9351131265310292928 ) ) ;
#21597 = CARTESIAN_POINT ( 'NONE',  ( 23.63159235450331863, 9.902892378096218942E-16, 0.000000000000000000 ) ) ;
#21598 = CARTESIAN_POINT ( 'NONE',  ( 34.42499999999998295, -13.45860074219782021, 5.000000000000000000 ) ) ;
#21599 = CARTESIAN_POINT ( 'NONE',  ( 16.77083333333333570, 6.094999999999991758, 1.633150327867687102 ) ) ;
#21600 = CARTESIAN_POINT ( 'NONE',  ( 17.18706980810188867, -2.126176841940956130, 7.934999999999990727 ) ) ;
#21601 = PLANE ( 'NONE',  #25851 ) ;
#21602 = LINE ( 'NONE', #109317, #140412 ) ;
#21603 = ORIENTED_EDGE ( 'NONE', *, *, #11465, .F. ) ;
#21604 = VECTOR ( 'NONE', #15593, 999.9999999999998863 ) ;
#21605 = ORIENTED_EDGE ( 'NONE', *, *, #120403, .T. ) ;
#21606 = CARTESIAN_POINT ( 'NONE',  ( 32.29289321881323360, -18.74070752338408852, 5.000000000000000000 ) ) ;
#21607 = ORIENTED_EDGE ( 'NONE', *, *, #1098, .T. ) ;
#21608 = ADVANCED_FACE ( 'NONE', ( #42482 ), #94130, .F. ) ;
#21609 = CARTESIAN_POINT ( 'NONE',  ( -34.49999999999975842, 4.464255608400450548, 4.994342998332166772 ) ) ;
#21610 = LINE ( 'NONE', #20153, #39326 ) ;
#21611 = FACE_OUTER_BOUND ( 'NONE', #65732, .T. ) ;
#21612 =( NAMED_UNIT ( * ) PLANE_ANGLE_UNIT ( ) SI_UNIT ( $, .RADIAN. ) );
#21613 = VERTEX_POINT ( 'NONE', #143187 ) ;
#21614 =( NAMED_UNIT ( * ) PLANE_ANGLE_UNIT ( ) SI_UNIT ( $, .RADIAN. ) );
#21615 = PLANE ( 'NONE',  #122847 ) ;
#21616 = EDGE_CURVE ( 'NONE', #71286, #21885, #122131, .T. ) ;
#21617 = VECTOR ( 'NONE', #123581, 1000.000000000000000 ) ;
#21618 = DIRECTION ( 'NONE',  ( 0.7071067811865487940, -0.7071067811865463515, 0.000000000000000000 ) ) ;
#21619 = CARTESIAN_POINT ( 'NONE',  ( 15.20840764549667767, -2.499999999999998224, 0.000000000000000000 ) ) ;
#21620 = CARTESIAN_POINT ( 'NONE',  ( 23.99999999999983302, -1.068876922607798985, 4.000000000000000000 ) ) ;
#21622 = ORIENTED_EDGE ( 'NONE', *, *, #98791, .T. ) ;
#21621 = FACE_OUTER_BOUND ( 'NONE', #53787, .T. ) ;
#21623 = DIRECTION ( 'NONE',  ( -0.7071067811865487940, 0.7071067811865463515, 0.000000000000000000 ) ) ;
#21624 = CARTESIAN_POINT ( 'NONE',  ( 71.00000000000000000, 0.000000000000000000, -7.950000000000000178 ) ) ;
#21625 = LINE ( 'NONE', #110038, #63194 ) ;
#21626 = LINE ( 'NONE', #33258, #1608 ) ;
#21627 = EDGE_CURVE ( 'NONE', #120820, #22844, #77256, .T. ) ;
#21628 = DIRECTION ( 'NONE',  ( 1.000000000000000000, 0.000000000000000000, 0.000000000000000000 ) ) ;
#21629 = VECTOR ( 'NONE', #21503, 1000.000000000000000 ) ;
#21630 = ORIENTED_EDGE ( 'NONE', *, *, #54, .F. ) ;
#21631 = ORIENTED_EDGE ( 'NONE', *, *, #9012, .T. ) ;
#21632 = EDGE_LOOP ( 'NONE', ( #54011, #42210, #52675, #41104 ) ) ;
#21633 = CARTESIAN_POINT ( 'NONE',  ( 92.16709685856477563, -3.055000000000000160, -5.291415217122921177 ) ) ;
#21634 = VECTOR ( 'NONE', #86657, 1000.000000000000000 ) ;
#21635 = VERTEX_POINT ( 'NONE', #46044 ) ;
#21636 = EDGE_CURVE ( 'NONE', #22385, #44324, #101098, .T. ) ;
#21637 = CARTESIAN_POINT ( 'NONE',  ( 131.5423521607622490, -49.05583548141699879, 39.86617647058824332 ) ) ;
#21638 = VECTOR ( 'NONE', #91623, 1000.000000000000000 ) ;
#21639 = CARTESIAN_POINT ( 'NONE',  ( 13.29826936130429260, 3.821174125832445049E-16, 0.000000000000000000 ) ) ;
#21640 = ORIENTED_EDGE ( 'NONE', *, *, #29899, .F. ) ;
#21641 = PLANE ( 'NONE',  #79215 ) ;
#21643 =( BOUNDED_CURVE ( )  B_SPLINE_CURVE ( 3, ( #68238, #112412, #35604, #69647 ),
 .UNSPECIFIED., .F., .F. ) 
 B_SPLINE_CURVE_WITH_KNOTS ( ( 4, 4 ),
 ( 1.901594255663624056, 1.933014472006568507 ),
 .UNSPECIFIED. ) 
 CURVE ( )  GEOMETRIC_REPRESENTATION_ITEM ( )  RATIONAL_B_SPLINE_CURVE ( ( 1.000000000000000000, 0.9999177325257868620, 0.9999177325257868620, 1.000000000000000000 ) ) 
 REPRESENTATION_ITEM ( '' )  );
#21642 = CARTESIAN_POINT ( 'NONE',  ( 13.49999999999990763, -7.533600742197660516, 5.000000000000000000 ) ) ;
#21644 = CARTESIAN_POINT ( 'NONE',  ( 87.99543019189812298, 5.291415217122916737, 3.055000000000001936 ) ) ;
#21645 = VERTEX_POINT ( 'NONE', #100409 ) ;
#21646 = CARTESIAN_POINT ( 'NONE',  ( -2.999999999999981792, -13.06887692260768219, 4.000000000000000000 ) ) ;
#21647 = VECTOR ( 'NONE', #48689, 1000.000000000000000 ) ;
#21648 = CARTESIAN_POINT ( 'NONE',  ( 116.5000000000000000, 0.000000000000000000, -7.950000000000000178 ) ) ;
#21649 = VERTEX_POINT ( 'NONE', #76528 ) ;
#21650 = ORIENTED_EDGE ( 'NONE', *, *, #45372, .T. ) ;
#21651 = EDGE_CURVE ( 'NONE', #18367, #96125, #87392, .T. ) ;
#21652 = EDGE_LOOP ( 'NONE', ( #99402, #123924, #42432, #131398 ) ) ;
#21653 = LINE ( 'NONE', #9291, #67659 ) ;
#21654 = ADVANCED_FACE ( 'NONE', ( #120703 ), #342, .F. ) ;
#21655 = CARTESIAN_POINT ( 'NONE',  ( 4.499999999999975131, 18.05218569542898521, 5.000000000000000000 ) ) ;
#21656 = EDGE_CURVE ( 'NONE', #66484, #119012, #121424, .T. ) ;
#21657 = CARTESIAN_POINT ( 'NONE',  ( 15.52540314143521982, 2.126176841940962348, 7.934999999999988951 ) ) ;
#21658 = VECTOR ( 'NONE', #54809, 1000.000000000000227 ) ;
#21659 = LINE ( 'NONE', #73382, #16362 ) ;
#21660 = CARTESIAN_POINT ( 'NONE',  ( 166.0564677593420981, 26.96999999999993847, 33.42388977641238057 ) ) ;
#21661 = CARTESIAN_POINT ( 'NONE',  ( 34.49999999999975842, -8.568876922607724822, 4.000000000000000000 ) ) ;
#21662 = AXIS2_PLACEMENT_3D ( 'NONE', #47598, #99784, #14199 ) ;
#21663 = ORIENTED_EDGE ( 'NONE', *, *, #92408, .T. ) ;
#21664 = ORIENTED_EDGE ( 'NONE', *, *, #90851, .T. ) ;
#21665 = CARTESIAN_POINT ( 'NONE',  ( 13.36246187583893530, 22.22500000000000142, 4.000000000000000000 ) ) ;
#21666 = ORIENTED_EDGE ( 'NONE', *, *, #102887, .T. ) ;
#21667 = ORIENTED_EDGE ( 'NONE', *, *, #38988, .T. ) ;
#21668 = VECTOR ( 'NONE', #47744, 999.9999999999998863 ) ;
#21670 = EDGE_CURVE ( 'NONE', #64780, #100429, #54769, .T. ) ;
#21669 = LINE ( 'NONE', #87634, #123784 ) ;
#21671 = ORIENTED_EDGE ( 'NONE', *, *, #102837, .F. ) ;
#21672 = DIRECTION ( 'NONE',  ( 0.7071067811865487940, 0.7071067811865463515, -0.000000000000000000 ) ) ;
#21673 = DIRECTION ( 'NONE',  ( 1.000000000000000000, 0.000000000000000000, 0.000000000000000000 ) ) ;
#21674 = ORIENTED_EDGE ( 'NONE', *, *, #4276, .F. ) ;
#21675 = DIRECTION ( 'NONE',  ( -1.000000000000000000, -1.224606353822377258E-16, -0.000000000000000000 ) ) ;
#21676 = CARTESIAN_POINT ( 'NONE',  ( -28.49999999999980460, 21.43112307739196254, 4.000000000000000000 ) ) ;
#21677 = ORIENTED_EDGE ( 'NONE', *, *, #51529, .F. ) ;
#21678 = DIRECTION ( 'NONE',  ( 0.000000000000000000, -1.000000000000000000, 0.000000000000000000 ) ) ;
#21679 = VERTEX_POINT ( 'NONE', #45341 ) ;
#21680 = CARTESIAN_POINT ( 'NONE',  ( 14.99999999999989875, -10.06887692260770528, 4.000000000000000000 ) ) ;
#21681 = VERTEX_POINT ( 'NONE', #22103 ) ;
#21682 = DIRECTION ( 'NONE',  ( -0.7071067811865487940, 0.7071067811865463515, -0.000000000000000000 ) ) ;
#21683 = ADVANCED_FACE ( 'NONE', ( #79414 ), #22789, .T. ) ;
#21684 = ORIENTED_EDGE ( 'NONE', *, *, #75596, .F. ) ;
#21685 = LINE ( 'NONE', #65934, #82980 ) ;
#21686 = ORIENTED_EDGE ( 'NONE', *, *, #60379, .T. ) ;
#21687 = ORIENTED_EDGE ( 'NONE', *, *, #70708, .T. ) ;
#21688 = CIRCLE ( 'NONE', #70373, 2.055000000000001048 ) ;
#21689 = ORIENTED_EDGE ( 'NONE', *, *, #15045, .T. ) ;
#21690 = CARTESIAN_POINT ( 'NONE',  ( -34.92500000000001137, -22.22500000000000142, 4.000000000000000000 ) ) ;
#21691 = DIRECTION ( 'NONE',  ( -0.000000000000000000, -0.3543493200069152693, 0.9351131265310292928 ) ) ;
#21692 = PLANE ( 'NONE',  #100484 ) ;
#21693 = PLANE ( 'NONE',  #29948 ) ;
#21694 = CARTESIAN_POINT ( 'NONE',  ( 6.183988606268994381, 28.73617430169791476, 5.000000000000000000 ) ) ;
#21695 = DIRECTION ( 'NONE',  ( -1.000000000000000000, 0.000000000000000000, 0.000000000000000000 ) ) ;
#21697 = CARTESIAN_POINT ( 'NONE',  ( 20.99999999999985789, 19.93112307739198386, 4.000000000000000000 ) ) ;
#21696 = AXIS2_PLACEMENT_3D ( 'NONE', #13308, #135830, #36516 ) ;
#21698 = LINE ( 'NONE', #89798, #34362 ) ;
#21699 = CARTESIAN_POINT ( 'NONE',  ( 39.48921356237310221, -27.52281430457082934, 5.000000000000000000 ) ) ;
#21700 = MECHANICAL_DESIGN_GEOMETRIC_PRESENTATION_REPRESENTATION (  '', ( #109659 ), #12478 ) ;
#21701 = FACE_OUTER_BOUND ( 'NONE', #125557, .T. ) ;
#21702 = ORIENTED_EDGE ( 'NONE', *, *, #56322, .T. ) ;
#21703 = ORIENTED_EDGE ( 'NONE', *, *, #112878, .F. ) ;
#21704 = EDGE_CURVE ( 'NONE', #137282, #130467, #85265, .T. ) ;
#21705 = EDGE_LOOP ( 'NONE', ( #63345, #109426, #92467, #51491 ) ) ;
#21706 = PLANE ( 'NONE',  #130503 ) ;
#21707 = ORIENTED_EDGE ( 'NONE', *, *, #76936, .F. ) ;
#21708 = VECTOR ( 'NONE', #73457, 1000.000000000000000 ) ;
#21709 = ORIENTED_EDGE ( 'NONE', *, *, #75912, .F. ) ;
#21710 = DIRECTION ( 'NONE',  ( 1.000000000000000000, 0.000000000000000000, 0.000000000000000000 ) ) ;
#21711 = CARTESIAN_POINT ( 'NONE',  ( 14.19163961620377279, 6.094999999999988205, -1.633150327867694651 ) ) ;
#21712 = CARTESIAN_POINT ( 'NONE',  ( 27.48921356237309155, -27.52281430457074762, 5.000000000000000000 ) ) ;
#21713 = PLANE ( 'NONE',  #64965 ) ;
#21714 = ORIENTED_EDGE ( 'NONE', *, *, #17517, .T. ) ;
#21715 = DIRECTION ( 'NONE',  ( 0.6830127018922181881, 0.6830127018922202975, -0.2588190451025214056 ) ) ;
#21716 = ORIENTED_EDGE ( 'NONE', *, *, #30041, .T. ) ;
#21717 = CIRCLE ( 'NONE', #70411, 2.055000000000000604 ) ;
#21719 = VECTOR ( 'NONE', #45958, 1000.000000000000000 ) ;
#21718 = DIRECTION ( 'NONE',  ( 0.000000000000000000, 1.000000000000000000, 0.000000000000000000 ) ) ;
#21720 = ADVANCED_FACE ( 'NONE', ( #57633 ), #113310, .T. ) ;
#21721 = VECTOR ( 'NONE', #112985, 1000.000000000000000 ) ;
#21722 = CARTESIAN_POINT ( 'NONE',  ( 20.04623647476855197, -7.934999999999990727, 4.858786175617117713E-16 ) ) ;
#21723 = ORIENTED_EDGE ( 'NONE', *, *, #54023, .F. ) ;
#21724 = CARTESIAN_POINT ( 'NONE',  ( 87.26626352523145158, 4.472830434245839371, -4.472830434245839371 ) ) ;
#21725 = EDGE_CURVE ( 'NONE', #1414, #50020, #78651, .T. ) ;
#21726 = LINE ( 'NONE', #110832, #140778 ) ;
#21727 = EDGE_CURVE ( 'NONE', #42250, #51263, #60491, .T. ) ;
#21728 = CARTESIAN_POINT ( 'NONE',  ( 55.32830738432631534, -52.14999999996970814, -41.05175048930665582 ) ) ;
#21729 = DIRECTION ( 'NONE',  ( 1.000000000000000000, 0.000000000000000000, 0.000000000000000000 ) ) ;
#21730 = ORIENTED_EDGE ( 'NONE', *, *, #15073, .F. ) ;
#21731 = EDGE_LOOP ( 'NONE', ( #41878, #82099, #76205, #100617 ) ) ;
#21732 = ADVANCED_FACE ( 'NONE', ( #26414 ), #113394, .F. ) ;
#21733 = EDGE_LOOP ( 'NONE', ( #22645, #42380, #73517, #79170 ) ) ;
#21734 = CARTESIAN_POINT ( 'NONE',  ( -16.49999999999988276, 5.696342897626497148, -7.587980461218440276 ) ) ;
#21736 = AXIS2_PLACEMENT_3D ( 'NONE', #12822, #122292, #11370 ) ;
#21735 = CARTESIAN_POINT ( 'NONE',  ( -23.03315071937583980, 7.620612595215163765, 4.000000000000000000 ) ) ;
#21737 = DIRECTION ( 'NONE',  ( -0.7071067811865487940, 0.7071067811865463515, -0.000000000000000000 ) ) ;
#21738 = CARTESIAN_POINT ( 'NONE',  ( 28.49999999999980105, 6.277155672890298632, -3.510561720659008067 ) ) ;
#21739 = EDGE_CURVE ( 'NONE', #65454, #124871, #104669, .T. ) ;
#21740 = CARTESIAN_POINT ( 'NONE',  ( 31.99806943317879515, -22.22500000000000142, 4.500000000000000888 ) ) ;
#21741 = VERTEX_POINT ( 'NONE', #49622 ) ;
#21742 = DIRECTION ( 'NONE',  ( 0.7071067811865486830, -0.7071067811865464625, -0.000000000000000000 ) ) ;
#21743 = EDGE_CURVE ( 'NONE', #14566, #19705, #101822, .T. ) ;
#21744 = DIRECTION ( 'NONE',  ( 0.3543493200069162685, -0.000000000000000000, -0.9351131265310288487 ) ) ;
#21745 = VERTEX_POINT ( 'NONE', #14807 ) ;
#21746 = CARTESIAN_POINT ( 'NONE',  ( -0.7928932188134494297, -11.24070752338417023, 5.000000000000000000 ) ) ;
#21747 = VECTOR ( 'NONE', #20633, 1000.000000000000000 ) ;
#21748 = DIRECTION ( 'NONE',  ( -0.7071067811865486830, -0.7071067811865464625, 0.000000000000000000 ) ) ;
#21749 = ORIENTED_EDGE ( 'NONE', *, *, #67272, .T. ) ;
#21750 = ADVANCED_FACE ( 'NONE', ( #4578 ), #93092, .F. ) ;
#21752 = ORIENTED_EDGE ( 'NONE', *, *, #119900, .F. ) ;
#21751 = DIRECTION ( 'NONE',  ( -0.3543493200069162685, -0.000000000000000000, -0.9351131265310288487 ) ) ;
#21753 = ORIENTED_EDGE ( 'NONE', *, *, #11456, .F. ) ;
#21754 = EDGE_CURVE ( 'NONE', #139296, #11674, #36559, .T. ) ;
#21755 = DIRECTION ( 'NONE',  ( -0.7071067811865486830, 0.7071067811865464625, 0.000000000000000000 ) ) ;
#21756 = FACE_OUTER_BOUND ( 'NONE', #40952, .T. ) ;
#21757 = ORIENTED_EDGE ( 'NONE', *, *, #142328, .T. ) ;
#21758 = CARTESIAN_POINT ( 'NONE',  ( -66.18398860626901126, 28.73617430169833753, 5.000000000000000000 ) ) ;
#21759 = EDGE_CURVE ( 'NONE', #58827, #7365, #35888, .T. ) ;
#21760 = LINE ( 'NONE', #41350, #140101 ) ;
#21762 = VECTOR ( 'NONE', #22735, 999.9999999999998863 ) ;
#21761 = DIRECTION ( 'NONE',  ( -1.000000000000000000, -0.000000000000000000, -0.000000000000000000 ) ) ;
#21763 = CARTESIAN_POINT ( 'NONE',  ( 33.18398860626899705, 28.73617430169810305, 5.000000000000000000 ) ) ;
#21764 = DIRECTION ( 'NONE',  ( 0.7071067811865487940, 0.7071067811865463515, 0.000000000000000000 ) ) ;
#21765 = CARTESIAN_POINT ( 'NONE',  ( 5.999999999999963585, -0.8619312979531862373, -5.102805207349813799 ) ) ;
#21766 = DIRECTION ( 'NONE',  ( -0.000000000000000000, 0.3543493200069153248, 0.9351131265310292928 ) ) ;
#21767 = DIRECTION ( 'NONE',  ( 0.7071067811865486830, -0.7071067811865464625, -0.000000000000000000 ) ) ;
#21768 = LINE ( 'NONE', #22446, #26006 ) ;
#21769 = DIRECTION ( 'NONE',  ( -0.3543493200069162685, -0.000000000000000000, -0.9351131265310288487 ) ) ;
#21770 = CARTESIAN_POINT ( 'NONE',  ( 110.8125000000000142, 5.819803920172571310, 5.819803920172576639 ) ) ;
#21771 = CARTESIAN_POINT ( 'NONE',  ( -23.60898926630779826, -0.6778661889157658882, 4.000000000000000000 ) ) ;
#21772 = ORIENTED_EDGE ( 'NONE', *, *, #135022, .T. ) ;
#21773 = VECTOR ( 'NONE', #70583, 1000.000000000000000 ) ;
#21774 = EDGE_LOOP ( 'NONE', ( #2942, #28355, #66343, #39487 ) ) ;
#21775 = CARTESIAN_POINT ( 'NONE',  ( 100.7500000000000000, -9.735942053221458872E-16, 7.950000000000000178 ) ) ;
#21776 = EDGE_LOOP ( 'NONE', ( #4871, #141106, #80781, #92146 ) ) ;
#21777 = ORIENTED_EDGE ( 'NONE', *, *, #84100, .T. ) ;
#21778 = ORIENTED_EDGE ( 'NONE', *, *, #20363, .F. ) ;
#21779 = ADVANCED_FACE ( 'NONE', ( #82240 ), #93798, .F. ) ;
#21780 = CARTESIAN_POINT ( 'NONE',  ( 0.000000000000000000, 0.000000000000000000, 5.000000000000000000 ) ) ;
#21781 = DIRECTION ( 'NONE',  ( 0.7071067811865487940, 0.7071067811865463515, 0.000000000000000000 ) ) ;
#21782 = EDGE_LOOP ( 'NONE', ( #58327, #133156, #67797, #67499 ) ) ;
#21783 = CARTESIAN_POINT ( 'NONE',  ( -22.49999999999984723, -4.216083040037270635, -7.486842126848605616 ) ) ;
#21784 = DIRECTION ( 'NONE',  ( 0.7071067811865487940, -0.7071067811865463515, 0.000000000000000000 ) ) ;
#21785 = LINE ( 'NONE', #31248, #108898 ) ;
#21786 = CARTESIAN_POINT ( 'NONE',  ( 34.49999999999975842, -17.91344420646039381, 1.358650452708543233 ) ) ;
#21787 = ORIENTED_EDGE ( 'NONE', *, *, #79210, .F. ) ;
#21788 = CARTESIAN_POINT ( 'NONE',  ( 21.79289321881330821, -5.240707523384228850, 5.000000000000000000 ) ) ;
#21789 = DIRECTION ( 'NONE',  ( -0.7071067811865487940, 0.7071067811865463515, -0.000000000000000000 ) ) ;
#21790 = AXIS2_PLACEMENT_3D ( 'NONE', #110457, #90152, #123537 ) ;
#21791 = LINE ( 'NONE', #70364, #77627 ) ;
#21792 = FACE_OUTER_BOUND ( 'NONE', #71306, .T. ) ;
#21793 = DIRECTION ( 'NONE',  ( 0.7071067811865487940, 0.7071067811865463515, 0.000000000000000000 ) ) ;
#21794 = CARTESIAN_POINT ( 'NONE',  ( 29.10002705046288085, 5.819803920172570422, 5.819803920172574863 ) ) ;
#21795 = ADVANCED_FACE ( 'NONE', ( #16200 ), #138025, .F. ) ;
#21796 = DIRECTION ( 'NONE',  ( 1.000000000000000000, 0.000000000000000000, 0.000000000000000000 ) ) ;
#21797 = VECTOR ( 'NONE', #136769, 1000.000000000000227 ) ;
#21798 = ORIENTED_EDGE ( 'NONE', *, *, #111751, .T. ) ;
#21799 = ORIENTED_EDGE ( 'NONE', *, *, #11913, .F. ) ;
#21800 = CARTESIAN_POINT ( 'NONE',  ( 117.8337635252314470, 6.110000000000001208, 1.122388791418549305E-15 ) ) ;
#21801 =( BOUNDED_CURVE ( )  B_SPLINE_CURVE ( 3, ( #73265, #106551, #9370, #7236 ),
 .UNSPECIFIED., .F., .T. ) 
 B_SPLINE_CURVE_WITH_KNOTS ( ( 4, 4 ),
 ( 1.570796326794895892, 1.837133570649240211 ),
 .UNSPECIFIED. ) 
 CURVE ( )  GEOMETRIC_REPRESENTATION_ITEM ( )  RATIONAL_B_SPLINE_CURVE ( ( 1.000000000000000000, 0.9940974367313470950, 0.9940974367313470950, 1.000000000000000000 ) ) 
 REPRESENTATION_ITEM ( '' )  );
#21802 = EDGE_LOOP ( 'NONE', ( #109164, #121829, #93633, #105213 ) ) ;
#21803 = CARTESIAN_POINT ( 'NONE',  ( 34.49999999999975842, -16.53574439159934073, 4.994342998332164107 ) ) ;
#21804 = EDGE_CURVE ( 'NONE', #10041, #21534, #127129, .T. ) ;
#21805 = CARTESIAN_POINT ( 'NONE',  ( 21.48921356237309155, -27.52281430457070499, 5.000000000000000000 ) ) ;
#21806 = CARTESIAN_POINT ( 'NONE',  ( 8.510786437626906675, -27.52281430457049183, 5.000000000000000000 ) ) ;
#21807 = FACE_OUTER_BOUND ( 'NONE', #82486, .T. ) ;
#21808 = CARTESIAN_POINT ( 'NONE',  ( -6.299744871391586898, -27.71228299555210484, 4.000000000000000000 ) ) ;
#21809 = CARTESIAN_POINT ( 'NONE',  ( 117.1620968585647802, -5.291415217122919401, 3.054999999999997939 ) ) ;
#21810 = VECTOR ( 'NONE', #112154, 1000.000000000000000 ) ;
#21811 = ORIENTED_EDGE ( 'NONE', *, *, #83733, .F. ) ;
#21812 = ADVANCED_FACE ( 'NONE', ( #82935 ), #48163, .F. ) ;
#21813 = ORIENTED_EDGE ( 'NONE', *, *, #2202, .F. ) ;
#21814 = CARTESIAN_POINT ( 'NONE',  ( -3.299744871391591339, -27.71228299555208352, 4.000000000000000000 ) ) ;
#21815 = DIRECTION ( 'NONE',  ( 1.000000000000000000, 0.000000000000000000, 0.000000000000000000 ) ) ;
#21816 = ORIENTED_EDGE ( 'NONE', *, *, #71120, .T. ) ;
#21817 = ORIENTED_EDGE ( 'NONE', *, *, #43951, .F. ) ;
#21818 = CARTESIAN_POINT ( 'NONE',  ( 36.31293019189809002, -1.637169565754159617, -6.110000000000001208 ) ) ;
#21819 = AXIS2_PLACEMENT_3D ( 'NONE', #50966, #82890, #16904 ) ;
#21820 = ADVANCED_FACE ( 'NONE', ( #116267 ), #2475, .F. ) ;
#21821 = ORIENTED_EDGE ( 'NONE', *, *, #138060, .F. ) ;
#21822 = FACE_OUTER_BOUND ( 'NONE', #46540, .T. ) ;
#21823 = LINE ( 'NONE', #124527, #101067 ) ;
#21824 = CARTESIAN_POINT ( 'NONE',  ( 21.48921356237309155, -27.52281430457070499, 5.000000000000000000 ) ) ;
#21825 =( BOUNDED_CURVE ( )  B_SPLINE_CURVE ( 3, ( #48154, #37274, #138016, #114795 ),
 .UNSPECIFIED., .F., .T. ) 
 B_SPLINE_CURVE_WITH_KNOTS ( ( 4, 4 ),
 ( 5.005968288816736056, 5.074607125596337198 ),
 .UNSPECIFIED. ) 
 CURVE ( )  GEOMETRIC_REPRESENTATION_ITEM ( )  RATIONAL_B_SPLINE_CURVE ( ( 1.000000000000000000, 0.9996074310407765395, 0.9996074310407765395, 1.000000000000000000 ) ) 
 REPRESENTATION_ITEM ( '' )  );
#21826 = COLOUR_RGB ( '', 0.40784314, 0.44705882, 0.49803922) ;
#21827 = VECTOR ( 'NONE', #90922, 1000.000000000000000 ) ;
#21828 = CARTESIAN_POINT ( 'NONE',  ( 27.03709685856478373, -3.054999999999998828, -5.291415217122919401 ) ) ;
#21829 = ORIENTED_EDGE ( 'NONE', *, *, #142541, .T. ) ;
#21830 = LINE ( 'NONE', #66073, #140494 ) ;
#21831 = VERTEX_POINT ( 'NONE', #14079 ) ;
#21832 = ORIENTED_EDGE ( 'NONE', *, *, #53790, .T. ) ;
#21833 = ORIENTED_EDGE ( 'NONE', *, *, #27453, .F. ) ;
#21834 = FACE_OUTER_BOUND ( 'NONE', #113773, .T. ) ;
#21835 = CARTESIAN_POINT ( 'NONE',  ( -75.18398860626899705, 28.73617430169839793, 5.000000000000000000 ) ) ;
#21836 = EDGE_CURVE ( 'NONE', #92930, #49206, #58379, .T. ) ;
#21837 = VERTEX_POINT ( 'NONE', #3206 ) ;
#21838 = CARTESIAN_POINT ( 'NONE',  ( 6.005480084712508493, 28.92564299267933947, 4.000000000000000000 ) ) ;
#21839 = DIRECTION ( 'NONE',  ( -0.7071067811865487940, 0.7071067811865463515, -0.000000000000000000 ) ) ;
#21840 = EDGE_CURVE ( 'NONE', #61158, #45578, #47496, .T. ) ;
#21841 = FACE_BOUND ( 'NONE', #70778, .T. ) ;
#21842 = ORIENTED_EDGE ( 'NONE', *, *, #72843, .T. ) ;
#21843 = CARTESIAN_POINT ( 'NONE',  ( 11.93159235450332112, -2.500000000000000000, 3.061616997868384127E-16 ) ) ;
#21844 = DIRECTION ( 'NONE',  ( -1.000000000000000000, -1.224606353822377258E-16, -0.000000000000000000 ) ) ;
#21845 = ADVANCED_FACE ( 'NONE', ( #25679 ), #81533, .T. ) ;
#21846 = ORIENTED_EDGE ( 'NONE', *, *, #25805, .T. ) ;
#21847 = DIRECTION ( 'NONE',  ( -0.000000000000000000, 0.3543493200069153248, 0.9351131265310292928 ) ) ;
#21848 = EDGE_LOOP ( 'NONE', ( #122430, #45087, #135707, #31509 ) ) ;
#21849 = EDGE_LOOP ( 'NONE', ( #47298, #14742, #87058, #79685 ) ) ;
#21850 = DIRECTION ( 'NONE',  ( 0.000000000000000000, 0.000000000000000000, 1.000000000000000000 ) ) ;
#21851 = ORIENTED_EDGE ( 'NONE', *, *, #42537, .T. ) ;
#21852 = CARTESIAN_POINT ( 'NONE',  ( 46.57876352523145158, -7.482591942790325086E-16, 6.109999999999998543 ) ) ;
#21853 = ORIENTED_EDGE ( 'NONE', *, *, #52776, .T. ) ;
#21854 = CARTESIAN_POINT ( 'NONE',  ( -72.18398860626899705, 28.73617430169837661, 5.000000000000000000 ) ) ;
#21855 = DIRECTION ( 'NONE',  ( -0.7071067811865487940, 0.7071067811865463515, -0.000000000000000000 ) ) ;
#21856 = FACE_OUTER_BOUND ( 'NONE', #105427, .T. ) ;
#21857 = VERTEX_POINT ( 'NONE', #62614 ) ;
#21858 = SPHERICAL_SURFACE ( 'NONE', #30645, 0.5000000000000000000 ) ;
#21859 = LINE ( 'NONE', #801, #115235 ) ;
#21860 = EDGE_CURVE ( 'NONE', #111536, #103780, #19796, .T. ) ;
#21861 = AXIS2_PLACEMENT_3D ( 'NONE', #110107, #53621, #54358 ) ;
#21862 = DIRECTION ( 'NONE',  ( 0.000000000000000000, -1.000000000000000000, 0.000000000000000000 ) ) ;
#21863 = CARTESIAN_POINT ( 'NONE',  ( 33.29974487139158867, -27.71228299555229313, 4.000000000000000000 ) ) ;
#21864 = CARTESIAN_POINT ( 'NONE',  ( -45.18398860626900415, 28.73617430169818832, 5.000000000000000000 ) ) ;
#21865 = CARTESIAN_POINT ( 'NONE',  ( -10.49999999999991296, 22.08746187583902199, 4.000000000000000000 ) ) ;
#21866 = LINE ( 'NONE', #87134, #50988 ) ;
#21867 = EDGE_LOOP ( 'NONE', ( #130970, #95805, #141935 ) ) ;
#21868 = ORIENTED_EDGE ( 'NONE', *, *, #120092, .F. ) ;
#21869 = VERTEX_POINT ( 'NONE', #86510 ) ;
#21870 = LINE ( 'NONE', #110286, #128384 ) ;
#21871 = CARTESIAN_POINT ( 'NONE',  ( 71.99451991528749772, 28.92564299267988304, 4.000000000000000000 ) ) ;
#21872 = EDGE_LOOP ( 'NONE', ( #133447, #115737, #32936, #91347 ) ) ;
#21873 = ORIENTED_EDGE ( 'NONE', *, *, #54268, .F. ) ;
#21874 = CARTESIAN_POINT ( 'NONE',  ( 163.1938454491095456, 26.96999999999994557, -34.65286652761894715 ) ) ;
#21875 = DIRECTION ( 'NONE',  ( 0.000000000000000000, 0.000000000000000000, 1.000000000000000000 ) ) ;
#21876 = LINE ( 'NONE', #110292, #67127 ) ;
#21877 = ORIENTED_EDGE ( 'NONE', *, *, #113518, .T. ) ;
#21878 = FACE_OUTER_BOUND ( 'NONE', #92946, .T. ) ;
#21879 = VECTOR ( 'NONE', #101024, 999.9999999999998863 ) ;
#21880 = LINE ( 'NONE', #99419, #51381 ) ;
#21881 = AXIS2_PLACEMENT_3D ( 'NONE', #26778, #47863, #13735 ) ;
#21882 = CARTESIAN_POINT ( 'NONE',  ( 28.79623647476855197, 7.934999999999990727, -1.457635852685135314E-15 ) ) ;
#21883 = EDGE_CURVE ( 'NONE', #120012, #56830, #116971, .T. ) ;
#21884 = CARTESIAN_POINT ( 'NONE',  ( 8.669897814527296021, 17.25929247661553845, 19.83885114516069237 ) ) ;
#21885 = VERTEX_POINT ( 'NONE', #74197 ) ;
#21886 = CARTESIAN_POINT ( 'NONE',  ( 118.0370968585647802, -3.054999999999999272, -5.291415217122919401 ) ) ;
#21887 = EDGE_CURVE ( 'NONE', #32991, #60304, #8862, .T. ) ;
#21888 = AXIS2_PLACEMENT_3D ( 'NONE', #97343, #18349, #83681 ) ;
#21889 = DIRECTION ( 'NONE',  ( 0.7071067811865487940, 0.7071067811865463515, 0.000000000000000000 ) ) ;
#21890 = LINE ( 'NONE', #79898, #33450 ) ;
#21892 = ORIENTED_EDGE ( 'NONE', *, *, #85244, .T. ) ;
#21891 = CARTESIAN_POINT ( 'NONE',  ( 69.29974487139159578, -27.71228299555254537, 4.000000000000000000 ) ) ;
#21893 = EDGE_LOOP ( 'NONE', ( #141497, #21684, #55337, #30469 ) ) ;
#21894 = CARTESIAN_POINT ( 'NONE',  ( -8.999999999999944933, 20.58746187583905041, 4.000000000000000000 ) ) ;
#21895 = LINE ( 'NONE', #840, #107128 ) ;
#21896 = ADVANCED_FACE ( 'NONE', ( #130000 ), #51019, .F. ) ;
#21897 = EDGE_CURVE ( 'NONE', #121709, #54552, #29246, .T. ) ;
#21898 = CARTESIAN_POINT ( 'NONE',  ( 121.0208333333333144, 7.949999999999998401, 2.130196079827431532 ) ) ;
#21899 = ORIENTED_EDGE ( 'NONE', *, *, #75961, .T. ) ;
#21900 = AXIS2_PLACEMENT_3D ( 'NONE', #32280, #3695, #43162 ) ;
#21901 = LINE ( 'NONE', #1543, #111282 ) ;
#21902 = LINE ( 'NONE', #66150, #46853 ) ;
#21903 = EDGE_LOOP ( 'NONE', ( #133136, #14746, #123489, #40478 ) ) ;
#21904 = CARTESIAN_POINT ( 'NONE',  ( 65.99451991528749772, 28.92564299267984396, 4.000000000000000000 ) ) ;
#21905 = FACE_OUTER_BOUND ( 'NONE', #79134, .T. ) ;
#21906 = VERTEX_POINT ( 'NONE', #96608 ) ;
#21907 = EDGE_CURVE ( 'NONE', #75102, #20507, #129265, .T. ) ;
#21908 = DIRECTION ( 'NONE',  ( 0.000000000000000000, -1.000000000000000000, 0.000000000000000000 ) ) ;
#21910 = ORIENTED_EDGE ( 'NONE', *, *, #92421, .T. ) ;
#21909 = DIRECTION ( 'NONE',  ( 0.000000000000000000, 1.000000000000000000, 0.000000000000000000 ) ) ;
#21911 = EDGE_CURVE ( 'NONE', #109724, #38733, #85768, .T. ) ;
#21912 = VERTEX_POINT ( 'NONE', #140850 ) ;
#21913 = DIRECTION ( 'NONE',  ( 0.000000000000000000, -1.000000000000000000, 0.000000000000000000 ) ) ;
#21914 = DIRECTION ( 'NONE',  ( -1.000000000000000000, -0.000000000000000000, -0.000000000000000000 ) ) ;
#21915 = ORIENTED_EDGE ( 'NONE', *, *, #5476, .F. ) ;
#21916 = EDGE_CURVE ( 'NONE', #138157, #13042, #130738, .T. ) ;
#21917 = CARTESIAN_POINT ( 'NONE',  ( -3.489213562373097322, -27.52281430457057709, 5.000000000000000000 ) ) ;
#21918 = VECTOR ( 'NONE', #125509, 1000.000000000000227 ) ;
#21919 = VECTOR ( 'NONE', #28875, 1000.000000000000000 ) ;
#21920 = CARTESIAN_POINT ( 'NONE',  ( -1.499999999999984901, -16.91253812416058722, 4.000000000000000000 ) ) ;
#21921 = CARTESIAN_POINT ( 'NONE',  ( 42.48921356237308800, -27.52281430457085065, 5.000000000000000000 ) ) ;
#21922 = VERTEX_POINT ( 'NONE', #6737 ) ;
#21923 = CARTESIAN_POINT ( 'NONE',  ( 15.70612307739184565, 22.22500000000000142, 4.000000000000000000 ) ) ;
#21924 = DIRECTION ( 'NONE',  ( 0.6830127018922180770, -0.6830127018922204085, -0.2588190451025213501 ) ) ;
#21925 = ADVANCED_FACE ( 'NONE', ( #39443 ), #61911, .F. ) ;
#21926 = LINE ( 'NONE', #98073, #8852 ) ;
#21927 = CARTESIAN_POINT ( 'NONE',  ( 31.26626352523144092, 4.472830434245839371, -4.472830434245839371 ) ) ;
#21928 = CARTESIAN_POINT ( 'NONE',  ( 17.99999999999987566, -21.41253812416053748, 4.000000000000000000 ) ) ;
#21929 = ORIENTED_EDGE ( 'NONE', *, *, #26645, .T. ) ;
#21930 = ORIENTED_EDGE ( 'NONE', *, *, #129621, .T. ) ;
#21931 = CARTESIAN_POINT ( 'NONE',  ( 125.5416666666666572, -3.975000000000002753, 6.884901960086286188 ) ) ;
#21932 = ORIENTED_EDGE ( 'NONE', *, *, #15821, .T. ) ;
#21933 = ORIENTED_EDGE ( 'NONE', *, *, #913, .T. ) ;
#21934 = EDGE_CURVE ( 'NONE', #48771, #27746, #97332, .T. ) ;
#21935 = CARTESIAN_POINT ( 'NONE',  ( 34.92499999999998295, 22.22500000000000142, 4.000000000000000000 ) ) ;
#21936 = DIRECTION ( 'NONE',  ( -0.6830127018922180770, -0.6830127018922204085, -0.2588190451025213501 ) ) ;
#21937 = EDGE_LOOP ( 'NONE', ( #81963, #142145, #58983, #65040 ) ) ;
#21938 = LINE ( 'NONE', #133577, #115640 ) ;
#21939 = CARTESIAN_POINT ( 'NONE',  ( 23.67183060077630330, 20.25929247661551003, 4.000000000000000000 ) ) ;
#21940 = CARTESIAN_POINT ( 'NONE',  ( -8.671830600776413434, -15.74070752338412404, 4.000000000000000000 ) ) ;
#21941 = CARTESIAN_POINT ( 'NONE',  ( 17.84878961325748037, 4.584330080086930965E-16, 0.000000000000000000 ) ) ;
#21942 = CARTESIAN_POINT ( 'NONE',  ( 123.0837635252314470, -6.110000000000001208, -3.741295971395164515E-16 ) ) ;
#21943 = VERTEX_POINT ( 'NONE', #140171 ) ;
#21944 = EDGE_CURVE ( 'NONE', #45954, #60787, #75629, .T. ) ;
#21945 = DIRECTION ( 'NONE',  ( 0.7071067811865487940, 0.7071067811865463515, -0.000000000000000000 ) ) ;
#21946 = FACE_OUTER_BOUND ( 'NONE', #37669, .T. ) ;
#21947 = EDGE_CURVE ( 'NONE', #124891, #98488, #105375, .T. ) ;
#21948 = LINE ( 'NONE', #110364, #77392 ) ;
#21949 = CARTESIAN_POINT ( 'NONE',  ( 5.207106781186511490, -14.24070752338413648, 5.000000000000000000 ) ) ;
#21950 = DIRECTION ( 'NONE',  ( -0.7071067811865486830, -0.7071067811865464625, -0.000000000000000000 ) ) ;
#21951 = DIRECTION ( 'NONE',  ( 0.000000000000000000, 0.000000000000000000, 1.000000000000000000 ) ) ;
#21952 = CARTESIAN_POINT ( 'NONE',  ( -19.17183060077633883, -14.24070752338413648, 4.000000000000000000 ) ) ;
#21953 = CARTESIAN_POINT ( 'NONE',  ( 52.14169371712954160, -2.130196079827424871, -7.949999999999999289 ) ) ;
#21954 = ADVANCED_FACE ( 'NONE', ( #74934 ), #72819, .T. ) ;
#21955 = CARTESIAN_POINT ( 'NONE',  ( 3.183988606268992161, 28.73617430169789699, 5.000000000000000000 ) ) ;
#21956 = DIRECTION ( 'NONE',  ( -0.7071067811865486830, 0.7071067811865464625, 0.000000000000000000 ) ) ;
#21957 = ORIENTED_EDGE ( 'NONE', *, *, #113042, .T. ) ;
#21958 = ORIENTED_EDGE ( 'NONE', *, *, #121016, .T. ) ;
#21959 = CARTESIAN_POINT ( 'NONE',  ( 49.12500000000000000, -7.950000000000000178, -4.867971026610729436E-16 ) ) ;
#21960 = DIRECTION ( 'NONE',  ( 0.000000000000000000, -1.000000000000000000, 0.000000000000000000 ) ) ;
#21961 = LINE ( 'NONE', #66207, #129518 ) ;
#21962 = ORIENTED_EDGE ( 'NONE', *, *, #28723, .T. ) ;
#21963 = CARTESIAN_POINT ( 'NONE',  ( 34.82816939922328459, 3.759292476615678336, 4.000000000000000000 ) ) ;
#21964 = AXIS2_PLACEMENT_3D ( 'NONE', #73236, #39168, #106522 ) ;
#21965 = LINE ( 'NONE', #88680, #42189 ) ;
#21966 = CARTESIAN_POINT ( 'NONE',  ( 35.87543019189811133, -5.291415217122920289, -3.055000000000001492 ) ) ;
#21967 = ORIENTED_EDGE ( 'NONE', *, *, #50144, .T. ) ;
#21968 = ORIENTED_EDGE ( 'NONE', *, *, #130750, .F. ) ;
#21969 = ORIENTED_EDGE ( 'NONE', *, *, #100100, .F. ) ;
#21970 = FACE_OUTER_BOUND ( 'NONE', #75342, .T. ) ;
#21971 = CARTESIAN_POINT ( 'NONE',  ( -34.92500000000001137, 21.72500000000000142, 5.000000000000000000 ) ) ;
#21972 = DIRECTION ( 'NONE',  ( 0.7071067811865487940, 0.7071067811865463515, 0.000000000000000000 ) ) ;
#21973 = LINE ( 'NONE', #66221, #55672 ) ;
#21974 = VERTEX_POINT ( 'NONE', #6032 ) ;
#21975 = CARTESIAN_POINT ( 'NONE',  ( -28.17183060077628198, 12.75929247661558286, 4.000000000000000000 ) ) ;
#21977 = ORIENTED_EDGE ( 'NONE', *, *, #33830, .F. ) ;
#21976 = DIRECTION ( 'NONE',  ( -0.000000000000000000, 0.000000000000000000, 1.000000000000000000 ) ) ;
#21978 = CARTESIAN_POINT ( 'NONE',  ( 85.31293019189811844, -1.637169565754159617, -6.110000000000001208 ) ) ;
#21979 = CARTESIAN_POINT ( 'NONE',  ( 14.87500000000000178, -6.094999999999989981, 3.732111120401553285E-16 ) ) ;
#21980 = DIRECTION ( 'NONE',  ( 0.6830127018922180770, -0.6830127018922204085, -0.2588190451025213501 ) ) ;
#21981 = CARTESIAN_POINT ( 'NONE',  ( 23.29320749275911595, 20.25929247661551358, 20.83292124670809642 ) ) ;
#21982 = CARTESIAN_POINT ( 'NONE',  ( 34.75611968250419181, 19.70565069852384354, 4.955485411084880276 ) ) ;
#21983 = AXIS2_PLACEMENT_3D ( 'NONE', #96987, #31082, #75998 ) ;
#21984 = ORIENTED_EDGE ( 'NONE', *, *, #83069, .F. ) ;
#21985 = LINE ( 'NONE', #11808, #82444 ) ;
#21986 = CARTESIAN_POINT ( 'NONE',  ( 70.93293019189810877, 1.637169565754156508, 6.110000000000000320 ) ) ;
#21987 = STYLED_ITEM ( 'NONE', ( #79246 ), #90242 ) ;
#21988 = CARTESIAN_POINT ( 'NONE',  ( 0.1600000000000009748, -7.113645484598424495, 3.515717980648092045 ) ) ;
#21989 = CARTESIAN_POINT ( 'NONE',  ( 25.39999999999999858, -16.48000000000005016, -12.70000000000045404 ) ) ;
#21990 =( LENGTH_UNIT ( ) NAMED_UNIT ( * ) SI_UNIT ( .MILLI., .METRE. ) );
#21991 = EDGE_LOOP ( 'NONE', ( #141786, #92607, #36848, #80062 ) ) ;
#21992 = ORIENTED_EDGE ( 'NONE', *, *, #41328, .F. ) ;
#21993 = CARTESIAN_POINT ( 'NONE',  ( 11.47599861414542843, 22.03583458319438648, 4.979811245910084949 ) ) ;
#21994 = ORIENTED_EDGE ( 'NONE', *, *, #54527, .F. ) ;
#21995 = VECTOR ( 'NONE', #115145, 1000.000000000000000 ) ;
#21996 = LINE ( 'NONE', #109731, #79187 ) ;
#21997 = ORIENTED_EDGE ( 'NONE', *, *, #60183, .T. ) ;
#21998 = DIRECTION ( 'NONE',  ( -0.7071067811865487940, 0.7071067811865463515, 0.000000000000000000 ) ) ;
#21999 = DIRECTION ( 'NONE',  ( 0.000000000000000000, 0.000000000000000000, 1.000000000000000000 ) ) ;
#22000 = FACE_OUTER_BOUND ( 'NONE', #118143, .T. ) ;
#22001 = CARTESIAN_POINT ( 'NONE',  ( -7.140000000000001457, -35.76999999999998892, -7.899272885403731514 ) ) ;
#22002 = ADVANCED_FACE ( 'NONE', ( #50308 ), #138748, .F. ) ;
#22003 = FACE_BOUND ( 'NONE', #47709, .T. ) ;
#22004 = CARTESIAN_POINT ( 'NONE',  ( -24.48921356237309510, -27.52281430457072631, 5.000000000000000000 ) ) ;
#22005 = DIRECTION ( 'NONE',  ( 0.000000000000000000, -1.000000000000000000, 0.000000000000000000 ) ) ;
#22006 = EDGE_CURVE ( 'NONE', #25093, #99900, #117653, .T. ) ;
#22007 = DIRECTION ( 'NONE',  ( 0.6830127018922180770, -0.6830127018922204085, -0.2588190451025213501 ) ) ;
#22009 = VERTEX_POINT ( 'NONE', #28560 ) ;
#22008 = LINE ( 'NONE', #231, #20330 ) ;
#22010 = DIRECTION ( 'NONE',  ( -1.000000000000000000, -0.000000000000000000, -0.000000000000000000 ) ) ;
#22011 = ITEM_DEFINED_TRANSFORMATION ( 'NONE', 'NONE', #650,  #127880 ) ;
#22012 = MECHANICAL_DESIGN_GEOMETRIC_PRESENTATION_REPRESENTATION (  '', ( #103055 ), #24307 ) ;
#22013 = VERTEX_POINT ( 'NONE', #18339 ) ;
#22014 = VECTOR ( 'NONE', #97467, 1000.000000000000227 ) ;
#22015 = ORIENTED_EDGE ( 'NONE', *, *, #97317, .T. ) ;
#22016 = CARTESIAN_POINT ( 'NONE',  ( 72.97459685856478018, 1.637169565754164280, -6.109999999999996767 ) ) ;
#22017 = ORIENTED_EDGE ( 'NONE', *, *, #88915, .F. ) ;
#22018 = CARTESIAN_POINT ( 'NONE',  ( -24.18398860626899705, 28.73617430169804265, 5.000000000000000000 ) ) ;
#22020 = EDGE_CURVE ( 'NONE', #9775, #90465, #51743, .T. ) ;
#22019 = VECTOR ( 'NONE', #37590, 1000.000000000000000 ) ;
#22021 = PLANE ( 'NONE',  #95267 ) ;
#22022 = VERTEX_POINT ( 'NONE', #43703 ) ;
#22023 = LINE ( 'NONE', #90889, #90774 ) ;
#22024 = ADVANCED_FACE ( 'NONE', ( #87209 ), #121950, .T. ) ;
#22025 = CARTESIAN_POINT ( 'NONE',  ( 32.99999999999976552, 14.87792677143811026, -11.06722581663432337 ) ) ;
#22026 = LINE ( 'NONE', #4309, #43731 ) ;
#22027 = DIRECTION ( 'NONE',  ( -0.7071067811865486830, -0.7071067811865464625, 0.000000000000000000 ) ) ;
#22028 = DIRECTION ( 'NONE',  ( -0.000000000000000000, -0.3543493200069152693, 0.9351131265310292928 ) ) ;
#22029 = CARTESIAN_POINT ( 'NONE',  ( -1.499999999999980460, 8.319652575858389909, -8.582050562765831003 ) ) ;
#22030 = DIRECTION ( 'NONE',  ( 1.000000000000000000, 0.000000000000000000, 0.000000000000000000 ) ) ;
#22031 = DIRECTION ( 'NONE',  ( -0.6830127018922180770, -0.6830127018922204085, -0.2588190451025213501 ) ) ;
#22032 = EDGE_LOOP ( 'NONE', ( #133697, #54661, #37369, #100716 ) ) ;
#22033 = ADVANCED_FACE ( 'NONE', ( #100930 ), #77077, .F. ) ;
#22034 = EDGE_LOOP ( 'NONE', ( #16635, #67585, #8510, #127008 ) ) ;
#22035 = CARTESIAN_POINT ( 'NONE',  ( 4.499999999999968914, -7.533600742197662292, 5.000000000000000000 ) ) ;
#22036 = ORIENTED_EDGE ( 'NONE', *, *, #82722, .T. ) ;
#22037 = ORIENTED_EDGE ( 'NONE', *, *, #52077, .T. ) ;
#22038 = FACE_OUTER_BOUND ( 'NONE', #120546, .T. ) ;
#22039 = VERTEX_POINT ( 'NONE', #122678 ) ;
#22040 = CARTESIAN_POINT ( 'NONE',  ( 130.7379471109758242, -48.51956544822604656, -36.87500513592858198 ) ) ;
#22041 = LINE ( 'NONE', #43116, #51607 ) ;
#22042 = CARTESIAN_POINT ( 'NONE',  ( 23.96247294953710849, -7.464222240803106570E-16, -6.094999999999989981 ) ) ;
#22043 = DIRECTION ( 'NONE',  ( 0.7071067811865487940, 0.7071067811865463515, 0.000000000000000000 ) ) ;
#22044 = VERTEX_POINT ( 'NONE', #67635 ) ;
#22045 = CARTESIAN_POINT ( 'NONE',  ( 12.70710678118646619, -3.740707523384243505, 5.000000000000000000 ) ) ;
#22046 = ADVANCED_FACE ( 'NONE', ( #11760 ), #45871, .F. ) ;
#22047 = EDGE_LOOP ( 'NONE', ( #39713, #52697, #116089, #79360, #93251 ) ) ;
#22048 = DIRECTION ( 'NONE',  ( 0.000000000000000000, 0.000000000000000000, 1.000000000000000000 ) ) ;
#22050 = VERTEX_POINT ( 'NONE', #20493 ) ;
#22049 = CARTESIAN_POINT ( 'NONE',  ( -62.99451991528749772, 28.92564299267982264, 4.000000000000000000 ) ) ;
#22051 = VERTEX_POINT ( 'NONE', #88655 ) ;
#22052 = DIRECTION ( 'NONE',  ( -0.000000000000000000, 0.3543493200069153248, 0.9351131265310292928 ) ) ;
#22053 = CARTESIAN_POINT ( 'NONE',  ( 25.39999999999999858, 0.000000000000000000, 6.094999999999989093 ) ) ;
#22054 = ADVANCED_FACE ( 'NONE', ( #9617 ), #143014, .F. ) ;
#22055 = EDGE_CURVE ( 'NONE', #35909, #108000, #23363, .T. ) ;
#22056 = FACE_OUTER_BOUND ( 'NONE', #56220, .T. ) ;
#22057 = VERTEX_POINT ( 'NONE', #21940 ) ;
#22058 = DIRECTION ( 'NONE',  ( -0.7071067811865486830, -0.7071067811865464625, 0.000000000000000000 ) ) ;
#22059 = ORIENTED_EDGE ( 'NONE', *, *, #60870, .F. ) ;
#22060 = DIRECTION ( 'NONE',  ( -0.6830127018922181881, 0.6830127018922202975, -0.2588190451025214056 ) ) ;
#22061 = CARTESIAN_POINT ( 'NONE',  ( 33.32816939922329880, -18.74070752338408852, 4.000000000000000000 ) ) ;
#22062 = DIRECTION ( 'NONE',  ( 0.6830127018922181881, 0.6830127018922202975, -0.2588190451025214056 ) ) ;
#22063 = EDGE_CURVE ( 'NONE', #30172, #93902, #133579, .T. ) ;
#22064 = DIRECTION ( 'NONE',  ( 0.000000000000000000, 0.000000000000000000, 1.000000000000000000 ) ) ;
#22065 =( BOUNDED_CURVE ( )  B_SPLINE_CURVE ( 3, ( #68892, #59451, #124672, #100782 ),
 .UNSPECIFIED., .F., .F. ) 
 B_SPLINE_CURVE_WITH_KNOTS ( ( 4, 4 ),
 ( 3.794322559382541371, 3.828945978481788526 ),
 .UNSPECIFIED. ) 
 CURVE ( )  GEOMETRIC_REPRESENTATION_ITEM ( )  RATIONAL_B_SPLINE_CURVE ( ( 1.000000000000000000, 0.9999001040657221617, 0.9999001040657221617, 1.000000000000000000 ) ) 
 REPRESENTATION_ITEM ( '' )  );
#22066 = CARTESIAN_POINT ( 'NONE',  ( 23.99999999999983302, -13.06887692260768041, 4.000000000000000000 ) ) ;
#22067 = DIRECTION ( 'NONE',  ( 0.6830127018922180770, -0.6830127018922204085, -0.2588190451025213501 ) ) ;
#22068 = ADVANCED_FACE ( 'NONE', ( #90046 ), #32113, .F. ) ;
#22069 = LINE ( 'NONE', #75770, #41406 ) ;
#22070 = VERTEX_POINT ( 'NONE', #98090 ) ;
#22071 = ADVANCED_FACE ( 'NONE', ( #77772 ), #108928, .T. ) ;
#22072 = CARTESIAN_POINT ( 'NONE',  ( 36.48921356237310221, -27.52281430457080802, 5.000000000000000000 ) ) ;
#22073 = VERTEX_POINT ( 'NONE', #131435 ) ;
#22074 = CARTESIAN_POINT ( 'NONE',  ( 72.29974487139158157, -27.71228299555256669, 4.000000000000000000 ) ) ;
#22075 = FILL_AREA_STYLE_COLOUR ( '', #114528 ) ;
#22076 = VECTOR ( 'NONE', #114157, 1000.000000000000000 ) ;
#22077 = CARTESIAN_POINT ( 'NONE',  ( -34.92499999999997584, 2.729999999999987104, -36.39086428169088094 ) ) ;
#22078 = VERTEX_POINT ( 'NONE', #87917 ) ;
#22079 = CARTESIAN_POINT ( 'NONE',  ( 23.20710678118638626, 9.759292476615614831, 5.000000000000000000 ) ) ;
#22080 = CARTESIAN_POINT ( 'NONE',  ( 8.207106781186492839, 18.75929247661552779, 5.000000000000000000 ) ) ;
#22081 = EDGE_CURVE ( 'NONE', #133528, #104648, #56770, .T. ) ;
#22082 = LINE ( 'NONE', #99643, #62988 ) ;
#22083 = VECTOR ( 'NONE', #22147, 999.9999999999998863 ) ;
#22084 = ORIENTED_EDGE ( 'NONE', *, *, #132924, .F. ) ;
#22085 = FILL_AREA_STYLE ('',( #121402 ) ) ;
#22086 = CARTESIAN_POINT ( 'NONE',  ( 13.49999999999990763, -4.216083040037239549, -7.486842126848689105 ) ) ;
#22087 = LINE ( 'NONE', #57615, #60859 ) ;
#22088 = SURFACE_SIDE_STYLE ('',( #121406 ) ) ;
#22089 = EDGE_CURVE ( 'NONE', #134528, #105677, #34260, .T. ) ;
#22090 = CARTESIAN_POINT ( 'NONE',  ( 33.29974487139158867, -27.71228299555229313, 4.000000000000000000 ) ) ;
#22091 = CARTESIAN_POINT ( 'NONE',  ( 66.26626352523145158, 4.472830434245839371, -4.472830434245839371 ) ) ;
#22092 = DIRECTION ( 'NONE',  ( 0.6830127018922181881, 0.6830127018922202975, -0.2588190451025214056 ) ) ;
#22093 = CARTESIAN_POINT ( 'NONE',  ( -30.70710678118633297, 14.25929247661557042, 5.000000000000000000 ) ) ;
#22094 = AXIS2_PLACEMENT_3D ( 'NONE', #69391, #25866, #93265 ) ;
#22095 = CARTESIAN_POINT ( 'NONE',  ( -51.18398860626899705, 28.73617430169823095, 5.000000000000000000 ) ) ;
#22096 = ORIENTED_EDGE ( 'NONE', *, *, #10443, .F. ) ;
#22097 = CARTESIAN_POINT ( 'NONE',  ( -57.18398860626899705, 28.73617430169827358, 5.000000000000000000 ) ) ;
#22098 = ORIENTED_EDGE ( 'NONE', *, *, #78909, .F. ) ;
#22099 = DIRECTION ( 'NONE',  ( -0.000000000000000000, -0.3543493200069152693, 0.9351131265310292928 ) ) ;
#22100 = FACE_OUTER_BOUND ( 'NONE', #71314, .T. ) ;
#22101 = DIRECTION ( 'NONE',  ( -1.000000000000000000, -1.224606353822377258E-16, -0.000000000000000000 ) ) ;
#22102 = CARTESIAN_POINT ( 'NONE',  ( -5.999999999999970690, 17.58746187583908238, 4.000000000000000000 ) ) ;
#22103 = CARTESIAN_POINT ( 'NONE',  ( -20.99999999999985079, -15.03360074219758502, 5.000000000000000000 ) ) ;
#22104 = DIRECTION ( 'NONE',  ( -0.000000000000000000, 0.3543493200069153248, 0.9351131265310292928 ) ) ;
#22105 = CARTESIAN_POINT ( 'NONE',  ( -21.79289321881330466, -2.240707523384257716, 5.000000000000000000 ) ) ;
#22106 = ORIENTED_EDGE ( 'NONE', *, *, #68604, .F. ) ;
#22107 = VERTEX_POINT ( 'NONE', #132161 ) ;
#22108 = DIRECTION ( 'NONE',  ( -0.7071067811865486830, -0.7071067811865464625, -0.000000000000000000 ) ) ;
#22109 = EDGE_CURVE ( 'NONE', #108363, #53838, #120505, .T. ) ;
#22110 = FACE_OUTER_BOUND ( 'NONE', #96633, .T. ) ;
#22111 = VECTOR ( 'NONE', #101483, 1000.000000000000000 ) ;
#22113 = EDGE_CURVE ( 'NONE', #3531, #36808, #66186, .T. ) ;
#22112 = CARTESIAN_POINT ( 'NONE',  ( 26.99451991528749417, 28.92564299267956685, 4.000000000000000000 ) ) ;
#22114 = CARTESIAN_POINT ( 'NONE',  ( 88.60002705046288440, 5.819803920172570422, 5.819803920172574863 ) ) ;
#22116 = EDGE_CURVE ( 'NONE', #40495, #45983, #55308, .T. ) ;
#22115 = CARTESIAN_POINT ( 'NONE',  ( -48.18398860626899705, 28.73617430169820608, 5.000000000000000000 ) ) ;
#22117 = PLANE ( 'NONE',  #117715 ) ;
#22118 = ORIENTED_EDGE ( 'NONE', *, *, #75621, .T. ) ;
#22119 = CARTESIAN_POINT ( 'NONE',  ( 71.14583333333332860, 2.130196079827431976, -7.949999999999999289 ) ) ;
#22120 = VECTOR ( 'NONE', #12431, 1000.000000000000000 ) ;
#22121 = DIRECTION ( 'NONE',  ( 0.7071067811865487940, 0.7071067811865463515, 0.000000000000000000 ) ) ;
#22122 = DIRECTION ( 'NONE',  ( 0.6830127018922180770, -0.6830127018922204085, -0.2588190451025213501 ) ) ;
#22123 = DIRECTION ( 'NONE',  ( -0.7071067811865486830, -0.7071067811865464625, 0.000000000000000000 ) ) ;
#22124 = VECTOR ( 'NONE', #131052, 1000.000000000000000 ) ;
#22125 = ORIENTED_EDGE ( 'NONE', *, *, #117938, .F. ) ;
#22126 = DIRECTION ( 'NONE',  ( -1.000000000000000000, -1.224606353822377258E-16, -0.000000000000000000 ) ) ;
#22127 = VERTEX_POINT ( 'NONE', #22622 ) ;
#22128 = CARTESIAN_POINT ( 'NONE',  ( 15.18398860626900237, 28.73617430169797871, 5.000000000000000000 ) ) ;
#22129 = CARTESIAN_POINT ( 'NONE',  ( 79.62543019189810423, 5.291415217122919401, 3.055000000000002824 ) ) ;
#22130 = CARTESIAN_POINT ( 'NONE',  ( 39.18398860626899705, 28.73617430169814568, 5.000000000000000000 ) ) ;
#22131 = ORIENTED_EDGE ( 'NONE', *, *, #15863, .F. ) ;
#22132 = CARTESIAN_POINT ( 'NONE',  ( -5.292986735706916690, -21.74070752338406010, 4.999753212805220670 ) ) ;
#22133 = DIRECTION ( 'NONE',  ( 0.7071067811865487940, 0.7071067811865463515, 0.000000000000000000 ) ) ;
#22134 = CARTESIAN_POINT ( 'NONE',  ( 7.499999999999951150, -5.947814304570770538, 5.000000000000000000 ) ) ;
#22135 = DIRECTION ( 'NONE',  ( -1.000000000000000000, -0.000000000000000000, -0.000000000000000000 ) ) ;
#22136 = DIRECTION ( 'NONE',  ( 0.6830127018922180770, -0.6830127018922204085, -0.2588190451025213501 ) ) ;
#22138 = ORIENTED_EDGE ( 'NONE', *, *, #84518, .T. ) ;
#22137 = PLANE ( 'NONE',  #26747 ) ;
#22139 = PLANE ( 'NONE',  #27607 ) ;
#22140 = DIRECTION ( 'NONE',  ( -0.000000000000000000, 0.000000000000000000, 1.000000000000000000 ) ) ;
#22141 = CARTESIAN_POINT ( 'NONE',  ( 77.27083333333332860, -7.949999999999998401, -2.130196079827426203 ) ) ;
#22142 = CARTESIAN_POINT ( 'NONE',  ( 19.05000000000000071, 3.174999999999997158, 5.000000000000000000 ) ) ;
#22143 = ORIENTED_EDGE ( 'NONE', *, *, #14981, .T. ) ;
#22144 = ORIENTED_EDGE ( 'NONE', *, *, #20804, .F. ) ;
#22145 = CARTESIAN_POINT ( 'NONE',  ( 64.60459685856477563, 1.637169565754164946, -6.109999999999999432 ) ) ;
#22146 = VERTEX_POINT ( 'NONE', #124119 ) ;
#22147 = DIRECTION ( 'NONE',  ( 0.5735764363510453823, -0.8191520442889923537, 1.003171929053525486E-16 ) ) ;
#22148 = CARTESIAN_POINT ( 'NONE',  ( -14.51078643762690490, -27.52281430457045275, 5.000000000000000000 ) ) ;
#22149 = DIRECTION ( 'NONE',  ( 0.6830127018922181881, 0.6830127018922202975, -0.2588190451025214056 ) ) ;
#22150 = ADVANCED_FACE ( 'NONE', ( #92915 ), #38544, .T. ) ;
#22151 = CARTESIAN_POINT ( 'NONE',  ( 0.000000000000000000, 0.000000000000000000, 5.000000000000000000 ) ) ;
#22152 = CARTESIAN_POINT ( 'NONE',  ( -31.92499999999997584, 2.729999999999987104, -36.39086428169088094 ) ) ;
#22153 = ORIENTED_EDGE ( 'NONE', *, *, #82299, .F. ) ;
#22154 = ORIENTED_EDGE ( 'NONE', *, *, #68561, .F. ) ;
#22155 = LINE ( 'NONE', #66415, #100086 ) ;
#22156 = CARTESIAN_POINT ( 'NONE',  ( -11.70025512860841133, -27.71228299555198049, 4.000000000000000000 ) ) ;
#22157 = ORIENTED_EDGE ( 'NONE', *, *, #40578, .T. ) ;
#22158 = CARTESIAN_POINT ( 'NONE',  ( -18.10180811604841011, 9.068207373850700748, 5.000000000000000000 ) ) ;
#22159 = PLANE ( 'NONE',  #34142 ) ;
#22160 = CARTESIAN_POINT ( 'NONE',  ( -15.32816939922342492, -6.740707523384209310, 4.000000000000000000 ) ) ;
#22161 = ORIENTED_EDGE ( 'NONE', *, *, #9603, .F. ) ;
#22162 = EDGE_CURVE ( 'NONE', #42348, #89916, #60320, .T. ) ;
#22163 = ADVANCED_FACE ( 'NONE', ( #24796 ), #93641, .F. ) ;
#22164 = FACE_BOUND ( 'NONE', #53001, .T. ) ;
#22165 = LINE ( 'NONE', #107051, #59380 ) ;
#22166 = LINE ( 'NONE', #130974, #127655 ) ;
#22167 = CARTESIAN_POINT ( 'NONE',  ( 24.48921356237309510, -27.52281430457072631, 5.000000000000000000 ) ) ;
#22168 = EDGE_CURVE ( 'NONE', #41309, #81522, #5158, .T. ) ;
#22169 = EDGE_CURVE ( 'NONE', #48106, #66483, #4405, .T. ) ;
#22170 = DIRECTION ( 'NONE',  ( 0.6830127018922180770, -0.6830127018922204085, -0.2588190451025213501 ) ) ;
#22171 = DIRECTION ( 'NONE',  ( 1.000000000000000000, 0.000000000000000000, 0.000000000000000000 ) ) ;
#22173 = ORIENTED_EDGE ( 'NONE', *, *, #97475, .F. ) ;
#22172 = VECTOR ( 'NONE', #114946, 1000.000000000000000 ) ;
#22174 = ORIENTED_EDGE ( 'NONE', *, *, #10418, .T. ) ;
#22175 = CARTESIAN_POINT ( 'NONE',  ( 99.80793019189812298, -6.109999999999998543, 1.637169565754158507 ) ) ;
#22176 =( BOUNDED_CURVE ( )  B_SPLINE_CURVE ( 3, ( #19053, #75590, #19761, #128541 ),
 .UNSPECIFIED., .F., .T. ) 
 B_SPLINE_CURVE_WITH_KNOTS ( ( 4, 4 ),
 ( 2.001653308786153218, 3.503810798801451742 ),
 .UNSPECIFIED. ) 
 CURVE ( )  GEOMETRIC_REPRESENTATION_ITEM ( )  RATIONAL_B_SPLINE_CURVE ( ( 1.000000000000000000, 0.8206354192515201706, 0.8206354192515201706, 1.000000000000000000 ) ) 
 REPRESENTATION_ITEM ( '' )  );
#22177 = ORIENTED_EDGE ( 'NONE', *, *, #52232, .T. ) ;
#22178 = COLOUR_RGB ( '', 0.09019608, 0.27058824, 0.51372549) ;
#22179 = EDGE_CURVE ( 'NONE', #25257, #391, #113225, .T. ) ;
#22180 = ORIENTED_EDGE ( 'NONE', *, *, #7979, .T. ) ;
#22181 = CARTESIAN_POINT ( 'NONE',  ( -36.18398860626899705, 28.73617430169812437, 5.000000000000000000 ) ) ;
#22182 = DIRECTION ( 'NONE',  ( -0.7071067811865486830, -0.7071067811865464625, 0.000000000000000000 ) ) ;
#22183 = ADVANCED_FACE ( 'NONE', ( #137870 ), #69046, .F. ) ;
#22184 = DIRECTION ( 'NONE',  ( 3.071323233543530392E-32, -2.242629915582283412E-16, 1.000000000000000000 ) ) ;
#22185 = VERTEX_POINT ( 'NONE', #81358 ) ;
#22186 = LINE ( 'NONE', #25048, #120162 ) ;
#22187 = FACE_OUTER_BOUND ( 'NONE', #139916, .T. ) ;
#22188 = LINE ( 'NONE', #84790, #57000 ) ;
#22189 = VECTOR ( 'NONE', #28257, 1000.000000000000227 ) ;
#22190 = CARTESIAN_POINT ( 'NONE',  ( 8.999999999999937828, 2.342191155542461267, -5.001666872980106149 ) ) ;
#22191 = EDGE_CURVE ( 'NONE', #111999, #107725, #125565, .T. ) ;
#22192 = CARTESIAN_POINT ( 'NONE',  ( -6.758600742197917732, 21.72500000000000142, 5.000000000000000000 ) ) ;
#22193 = EDGE_CURVE ( 'NONE', #2860, #925, #48709, .T. ) ;
#22194 = CARTESIAN_POINT ( 'NONE',  ( 0.3479702768469047913, 1.285727409420016176, 3.988060179666636618 ) ) ;
#22195 = ORIENTED_EDGE ( 'NONE', *, *, #48238, .F. ) ;
#22196 = CARTESIAN_POINT ( 'NONE',  ( -1.499999999999987566, -5.568876922607757685, 4.000000000000000000 ) ) ;
#22197 = DIRECTION ( 'NONE',  ( -0.3543493200069162685, -0.000000000000000000, -0.9351131265310288487 ) ) ;
#22198 = ORIENTED_EDGE ( 'NONE', *, *, #8714, .T. ) ;
#22199 = ORIENTED_EDGE ( 'NONE', *, *, #15823, .T. ) ;
#22200 = ORIENTED_EDGE ( 'NONE', *, *, #21378, .F. ) ;
#22201 = CARTESIAN_POINT ( 'NONE',  ( 56.00043019189809712, -3.055000000000002380, 5.291415217122920289 ) ) ;
#22202 = EDGE_CURVE ( 'NONE', #82994, #125640, #15321, .T. ) ;
#22203 = VERTEX_POINT ( 'NONE', #80631 ) ;
#22204 = VECTOR ( 'NONE', #112213, 1000.000000000000000 ) ;
#22205 = CARTESIAN_POINT ( 'NONE',  ( 54.18398860626899705, 28.73617430169825226, 5.000000000000000000 ) ) ;
#22206 = AXIS2_PLACEMENT_3D ( 'NONE', #6065, #27140, #16231 ) ;
#22207 = CARTESIAN_POINT ( 'NONE',  ( -0.5375270504628941737, -7.464222240803106570E-16, -6.094999999999989981 ) ) ;
#22208 = CARTESIAN_POINT ( 'NONE',  ( 101.2087635252314470, -7.482591942790329030E-16, 6.110000000000001208 ) ) ;
#22209 = LINE ( 'NONE', #43288, #68070 ) ;
#22210 = AXIS2_PLACEMENT_3D ( 'NONE', #18931, #6582, #50857 ) ;
#22211 = EDGE_CURVE ( 'NONE', #119191, #76747, #68355, .T. ) ;
#22212 = VERTEX_POINT ( 'NONE', #135035 ) ;
#22213 = DIRECTION ( 'NONE',  ( -1.000000000000000000, -0.000000000000000000, -0.000000000000000000 ) ) ;
#22214 = VECTOR ( 'NONE', #82069, 1000.000000000000227 ) ;
#22215 = LINE ( 'NONE', #20800, #19325 ) ;
#22217 = ADVANCED_FACE ( 'NONE', ( #92183 ), #71189, .F. ) ;
#22216 = CARTESIAN_POINT ( 'NONE',  ( -30.42356297102625717, -22.22500000000000142, 3.294237237169319599 ) ) ;
#22218 = ORIENTED_EDGE ( 'NONE', *, *, #3710, .F. ) ;
#22219 = DIRECTION ( 'NONE',  ( -0.7071067811865487940, 0.7071067811865463515, -0.000000000000000000 ) ) ;
#22220 = ORIENTED_EDGE ( 'NONE', *, *, #70681, .F. ) ;
#22221 = EDGE_CURVE ( 'NONE', #113128, #62841, #106456, .T. ) ;
#22222 = VERTEX_POINT ( 'NONE', #101643 ) ;
#22223 = VERTEX_POINT ( 'NONE', #2300 ) ;
#22224 = CARTESIAN_POINT ( 'NONE',  ( 121.5370968585647802, -3.054999999999998828, -5.291415217122919401 ) ) ;
#22225 = EDGE_CURVE ( 'NONE', #19559, #133451, #103087, .T. ) ;
#22226 = DIRECTION ( 'NONE',  ( -0.000000000000000000, 1.000000000000000000, -0.000000000000000000 ) ) ;
#22227 = CARTESIAN_POINT ( 'NONE',  ( 8.510786437626906675, -27.52281430457049183, 5.000000000000000000 ) ) ;
#22228 = ORIENTED_EDGE ( 'NONE', *, *, #81664, .F. ) ;
#22229 = DIRECTION ( 'NONE',  ( -0.3543493200069162685, -0.000000000000000000, -0.9351131265310288487 ) ) ;
#22230 = ORIENTED_EDGE ( 'NONE', *, *, #108130, .F. ) ;
#22231 = CARTESIAN_POINT ( 'NONE',  ( 10.04123647476855297, 0.000000000000000000, 7.934999999999990727 ) ) ;
#22232 = CARTESIAN_POINT ( 'NONE',  ( -28.49999999999979750, 0.4497235411627178991, -5.599840258123606418 ) ) ;
#22233 = CARTESIAN_POINT ( 'NONE',  ( -34.92499999999999005, 1.196650378695320427, -30.59010235425025215 ) ) ;
#22234 = ADVANCED_FACE ( 'NONE', ( #90799 ), #3040, .F. ) ;
#22235 = LINE ( 'NONE', #23690, #123105 ) ;
#22236 = ORIENTED_EDGE ( 'NONE', *, *, #62733, .T. ) ;
#22237 = VERTEX_POINT ( 'NONE', #14647 ) ;
#22238 = ORIENTED_EDGE ( 'NONE', *, *, #117375, .F. ) ;
#22239 = FACE_OUTER_BOUND ( 'NONE', #101063, .T. ) ;
#22240 = AXIS2_PLACEMENT_3D ( 'NONE', #136785, #37496, #81732 ) ;
#22241 = DIRECTION ( 'NONE',  ( -0.000000000000000000, 0.3543493200069153248, 0.9351131265310292928 ) ) ;
#22242 = EDGE_CURVE ( 'NONE', #29201, #121119, #36401, .T. ) ;
#22243 = LINE ( 'NONE', #67969, #80705 ) ;
#22244 = CARTESIAN_POINT ( 'NONE',  ( -14.11732500641695509, -0.1862019290248694003, 4.000000000000000000 ) ) ;
#22245 = DIRECTION ( 'NONE',  ( 0.000000000000000000, -1.000000000000000000, 0.000000000000000000 ) ) ;
#22246 = LINE ( 'NONE', #56385, #67209 ) ;
#22247 = CARTESIAN_POINT ( 'NONE',  ( 21.76000000000000156, 9.521314400968980422E-16, 0.000000000000000000 ) ) ;
#22248 = EDGE_LOOP ( 'NONE', ( #12815, #2961, #143267 ) ) ;
#22249 = DIRECTION ( 'NONE',  ( -0.000000000000000000, 0.000000000000000000, 1.000000000000000000 ) ) ;
#22250 = VECTOR ( 'NONE', #46785, 1000.000000000000227 ) ;
#22251 = ORIENTED_EDGE ( 'NONE', *, *, #44468, .F. ) ;
#22252 = PLANE ( 'NONE',  #75446 ) ;
#22253 = ORIENTED_EDGE ( 'NONE', *, *, #26505, .F. ) ;
#22254 = DIRECTION ( 'NONE',  ( 1.000000000000000000, 1.224606353822377258E-16, 0.000000000000000000 ) ) ;
#22256 = EDGE_LOOP ( 'NONE', ( #127565, #13290, #8907, #120617 ) ) ;
#22255 = PLANE ( 'NONE',  #76557 ) ;
#22257 = LINE ( 'NONE', #110001, #141835 ) ;
#22258 = ORIENTED_EDGE ( 'NONE', *, *, #88510, .T. ) ;
#22259 = EDGE_LOOP ( 'NONE', ( #132083, #56128 ) ) ;
#22260 = LINE ( 'NONE', #66526, #102317 ) ;
#22261 = ORIENTED_EDGE ( 'NONE', *, *, #60384, .T. ) ;
#22262 = AXIS2_PLACEMENT_3D ( 'NONE', #99573, #112619, #80036 ) ;
#22263 = ADVANCED_FACE ( 'NONE', ( #7310 ), #63879, .F. ) ;
#22264 = CARTESIAN_POINT ( 'NONE',  ( 114.9958603837962272, -3.974999999999998312, -6.884901960086286188 ) ) ;
#22265 = FACE_OUTER_BOUND ( 'NONE', #34885, .T. ) ;
#22266 = VECTOR ( 'NONE', #65746, 1000.000000000000000 ) ;
#22267 = DIRECTION ( 'NONE',  ( 0.000000000000000000, 1.000000000000000000, 0.000000000000000000 ) ) ;
#22268 = DIRECTION ( 'NONE',  ( -0.000000000000000000, 0.000000000000000000, -1.000000000000000000 ) ) ;
#22269 = CARTESIAN_POINT ( 'NONE',  ( -32.47599861414528277, 22.03583458319437938, 4.979811245910089390 ) ) ;
#22270 = CARTESIAN_POINT ( 'NONE',  ( 14.87500000000000178, -6.094999999999989981, 3.732111120401553285E-16 ) ) ;
#22271 = CARTESIAN_POINT ( 'NONE',  ( 17.33290314143522082, -3.967499999999994476, 6.871911579029513106 ) ) ;
#22272 = CARTESIAN_POINT ( 'NONE',  ( 66.48921356237309510, -27.52281430457101763, 5.000000000000000000 ) ) ;
#22273 = CARTESIAN_POINT ( 'NONE',  ( -6.299744871391586898, -27.71228299555210484, 4.000000000000000000 ) ) ;
#22274 = ORIENTED_EDGE ( 'NONE', *, *, #134730, .T. ) ;
#22275 = ORIENTED_EDGE ( 'NONE', *, *, #89769, .F. ) ;
#22276 = CARTESIAN_POINT ( 'NONE',  ( 26.20710678118636494, 18.75929247661552068, 5.000000000000000000 ) ) ;
#22277 = EDGE_LOOP ( 'NONE', ( #133100, #98973, #102516, #65036 ) ) ;
#22278 = VECTOR ( 'NONE', #10588, 999.9999999999998863 ) ;
#22279 = CYLINDRICAL_SURFACE ( 'NONE', #64203, 2.500000000000000000 ) ;
#22280 = LINE ( 'NONE', #113597, #124984 ) ;
#22281 = CARTESIAN_POINT ( 'NONE',  ( 32.49999999999998579, 0.000000000000000000, -7.950000000000000178 ) ) ;
#22282 = DIRECTION ( 'NONE',  ( 0.3543493200069163240, -0.000000000000000000, -0.9351131265310288487 ) ) ;
#22283 = EDGE_LOOP ( 'NONE', ( #99470, #44289, #67365, #37546 ) ) ;
#22284 = CARTESIAN_POINT ( 'NONE',  ( -30.48921356237309510, -27.52281430457076894, 5.000000000000000000 ) ) ;
#22285 = CARTESIAN_POINT ( 'NONE',  ( -25.39999999999996305, 0.000000000000000000, 0.000000000000000000 ) ) ;
#22286 = VECTOR ( 'NONE', #51964, 1000.000000000000000 ) ;
#22287 = DIRECTION ( 'NONE',  ( 0.000000000000000000, 0.000000000000000000, -1.000000000000000000 ) ) ;
#22288 = LINE ( 'NONE', #78151, #30962 ) ;
#22290 = VERTEX_POINT ( 'NONE', #82767 ) ;
#22289 = CARTESIAN_POINT ( 'NONE',  ( -31.82334089840007607, 5.259292476615665457, 15.86257073897105130 ) ) ;
#22291 = CARTESIAN_POINT ( 'NONE',  ( 6.540657738503846907, 4.202752102959690472E-16, 0.000000000000000000 ) ) ;
#22292 = CARTESIAN_POINT ( 'NONE',  ( -33.79289321881321939, -8.240707523384195099, 5.000000000000000000 ) ) ;
#22293 = PLANE ( 'NONE',  #104847 ) ;
#22294 = DIRECTION ( 'NONE',  ( 0.000000000000000000, 0.000000000000000000, 1.000000000000000000 ) ) ;
#22295 = AXIS2_PLACEMENT_3D ( 'NONE', #68393, #21980, #87964 ) ;
#22296 = CARTESIAN_POINT ( 'NONE',  ( 25.49999999999982236, 21.05218569542895324, 5.000000000000000000 ) ) ;
#22297 = VECTOR ( 'NONE', #141653, 1000.000000000000000 ) ;
#22298 = ORIENTED_EDGE ( 'NONE', *, *, #138071, .T. ) ;
#22299 = ORIENTED_EDGE ( 'NONE', *, *, #72244, .T. ) ;
#22300 = VERTEX_POINT ( 'NONE', #129105 ) ;
#22301 = VECTOR ( 'NONE', #4028, 1000.000000000000227 ) ;
#22302 = CARTESIAN_POINT ( 'NONE',  ( 88.66709685856477563, -3.055000000000000160, -5.291415217122921177 ) ) ;
#22303 = ORIENTED_EDGE ( 'NONE', *, *, #241, .T. ) ;
#22304 = FACE_OUTER_BOUND ( 'NONE', #64503, .T. ) ;
#22305 = DIRECTION ( 'NONE',  ( 0.000000000000000000, 0.000000000000000000, 1.000000000000000000 ) ) ;
#22307 = AXIS2_PLACEMENT_3D ( 'NONE', #14461, #136229, #36916 ) ;
#22306 = DIRECTION ( 'NONE',  ( 0.7071067811865487940, 0.7071067811865463515, 0.000000000000000000 ) ) ;
#22308 = CARTESIAN_POINT ( 'NONE',  ( 20.99999999999985079, -18.41253812416056590, 4.000000000000000000 ) ) ;
#22309 = ORIENTED_EDGE ( 'NONE', *, *, #23651, .T. ) ;
#22310 = FACE_OUTER_BOUND ( 'NONE', #99579, .T. ) ;
#22311 = CARTESIAN_POINT ( 'NONE',  ( 28.49999999999980460, 21.43112307739196254, 4.000000000000000000 ) ) ;
#22312 = CARTESIAN_POINT ( 'NONE',  ( 88.57876352523145158, -7.482591942790325086E-16, 6.109999999999998543 ) ) ;
#22313 = ORIENTED_EDGE ( 'NONE', *, *, #83440, .T. ) ;
#22314 = CARTESIAN_POINT ( 'NONE',  ( -26.14994871458959480, -8.240707523384193323, 17.25253755692233071 ) ) ;
#22315 = EDGE_CURVE ( 'NONE', #86742, #116142, #117495, .T. ) ;
#22316 = LINE ( 'NONE', #11441, #116437 ) ;
#22317 = EDGE_LOOP ( 'NONE', ( #69648, #134974, #78260, #54533, #37720 ) ) ;
#22318 = ORIENTED_EDGE ( 'NONE', *, *, #50395, .F. ) ;
#22319 = ORIENTED_EDGE ( 'NONE', *, *, #54477, .F. ) ;
#22320 = CARTESIAN_POINT ( 'NONE',  ( 27.48921356237309155, -27.52281430457074762, 5.000000000000000000 ) ) ;
#22321 = EDGE_CURVE ( 'NONE', #91520, #50934, #85592, .T. ) ;
#22322 = ADVANCED_FACE ( 'NONE', ( #17487 ), #108040, .F. ) ;
#22323 = PLANE ( 'NONE',  #105481 ) ;
#22324 = CARTESIAN_POINT ( 'NONE',  ( 13.77540314143521982, -2.126176841940958351, -7.934999999999988951 ) ) ;
#22325 = LINE ( 'NONE', #10051, #30366 ) ;
#22326 = LINE ( 'NONE', #31118, #128997 ) ;
#22327 = DIRECTION ( 'NONE',  ( -0.7071067811865486830, -0.7071067811865464625, -0.000000000000000000 ) ) ;
#22328 = EDGE_CURVE ( 'NONE', #65622, #29125, #73327, .T. ) ;
#22329 = EDGE_CURVE ( 'NONE', #22380, #13798, #40690, .T. ) ;
#22330 = CARTESIAN_POINT ( 'NONE',  ( -21.48921356237309155, -27.52281430457070499, 5.000000000000000000 ) ) ;
#22331 = AXIS2_PLACEMENT_3D ( 'NONE', #67016, #128180, #62208 ) ;
#22332 = EDGE_CURVE ( 'NONE', #48528, #131664, #84894, .T. ) ;
#22333 = VERTEX_POINT ( 'NONE', #128414 ) ;
#22334 = ORIENTED_EDGE ( 'NONE', *, *, #49438, .F. ) ;
#22336 = EDGE_CURVE ( 'NONE', #129163, #43341, #72646, .T. ) ;
#22335 = CARTESIAN_POINT ( 'NONE',  ( 0.000000000000000000, -4.600000000000055600, -28.92500000000000071 ) ) ;
#22337 = VERTEX_POINT ( 'NONE', #118213 ) ;
#22338 = ORIENTED_EDGE ( 'NONE', *, *, #24835, .F. ) ;
#22339 = VECTOR ( 'NONE', #85612, 1000.000000000000000 ) ;
#22340 = ADVANCED_FACE ( 'NONE', ( #18919 ), #5873, .F. ) ;
#22341 = EDGE_CURVE ( 'NONE', #42198, #962, #8706, .T. ) ;
#22342 = CARTESIAN_POINT ( 'NONE',  ( 0.000000000000000000, 0.000000000000000000, 5.000000000000000000 ) ) ;
#22343 = VERTEX_POINT ( 'NONE', #27647 ) ;
#22344 = DIRECTION ( 'NONE',  ( 0.6830127018922180770, -0.6830127018922204085, -0.2588190451025213501 ) ) ;
#22345 = PLANE ( 'NONE',  #81941 ) ;
#22346 = DIRECTION ( 'NONE',  ( 0.7071067811865486830, -0.7071067811865464625, -0.000000000000000000 ) ) ;
#22347 = VECTOR ( 'NONE', #41535, 1000.000000000000000 ) ;
#22348 = DIRECTION ( 'NONE',  ( 1.000000000000000000, 0.000000000000000000, 0.000000000000000000 ) ) ;
#22349 = CARTESIAN_POINT ( 'NONE',  ( -2.999999999999978240, 16.93112307739200872, 4.000000000000000000 ) ) ;
#22350 = ORIENTED_EDGE ( 'NONE', *, *, #112077, .F. ) ;
#22351 = EDGE_CURVE ( 'NONE', #139777, #10041, #52959, .T. ) ;
#22352 = SURFACE_SIDE_STYLE ('',( #57909 ) ) ;
#22354 = ORIENTED_EDGE ( 'NONE', *, *, #14990, .T. ) ;
#22353 = VECTOR ( 'NONE', #28981, 1000.000000000000000 ) ;
#22355 = CARTESIAN_POINT ( 'NONE',  ( -25.49999999999981881, 10.08746187583913922, 4.000000000000000000 ) ) ;
#22356 = VERTEX_POINT ( 'NONE', #74765 ) ;
#22357 = DIRECTION ( 'NONE',  ( 0.7071067811865487940, 0.7071067811865463515, 0.000000000000000000 ) ) ;
#22358 = ORIENTED_EDGE ( 'NONE', *, *, #14618, .T. ) ;
#22359 = DIRECTION ( 'NONE',  ( 0.6830127018922180770, -0.6830127018922202975, -0.2588190451025213501 ) ) ;
#22360 = EDGE_LOOP ( 'NONE', ( #25490, #80496, #53408, #87337 ) ) ;
#22361 = VERTEX_POINT ( 'NONE', #97156 ) ;
#22362 = EDGE_CURVE ( 'NONE', #27746, #53886, #141422, .T. ) ;
#22363 = ORIENTED_EDGE ( 'NONE', *, *, #91810, .T. ) ;
#22364 = VECTOR ( 'NONE', #100154, 1000.000000000000000 ) ;
#22365 = DIRECTION ( 'NONE',  ( 0.6830127018922180770, -0.6830127018922204085, -0.2588190451025213501 ) ) ;
#22366 = DIRECTION ( 'NONE',  ( -0.7071067811865487940, 0.7071067811865463515, 0.000000000000000000 ) ) ;
#22367 = DIRECTION ( 'NONE',  ( -1.000000000000000000, -1.369518533665900312E-16, 0.000000000000000000 ) ) ;
#22368 = DIRECTION ( 'NONE',  ( -0.7071067811865486830, 0.7071067811865464625, 0.000000000000000000 ) ) ;
#22369 = AXIS2_PLACEMENT_3D ( 'NONE', #27173, #125801, #14874 ) ;
#22370 = CARTESIAN_POINT ( 'NONE',  ( 127.1670968585647756, -3.055000000000000160, -5.291415217122921177 ) ) ;
#22371 = DIRECTION ( 'NONE',  ( -1.000000000000000000, -1.224606353822377258E-16, -0.000000000000000000 ) ) ;
#22372 = PRODUCT_DEFINITION_SHAPE ( 'NONE', 'NONE',  #87323 ) ;
#22373 = DIRECTION ( 'NONE',  ( 0.3543493200069162685, -0.000000000000000000, -0.9351131265310288487 ) ) ;
#22374 = CARTESIAN_POINT ( 'NONE',  ( 0.000000000000000000, -30.18000000000009564, -12.70000000000045404 ) ) ;
#22375 = FACE_OUTER_BOUND ( 'NONE', #38093, .T. ) ;
#22376 = ADVANCED_FACE ( 'NONE', ( #61062 ), #105903, .F. ) ;
#22377 = ORIENTED_EDGE ( 'NONE', *, *, #80164, .F. ) ;
#22378 = CARTESIAN_POINT ( 'NONE',  ( -50.99451991528749062, 28.92564299267973738, 4.000000000000000000 ) ) ;
#22379 = DIRECTION ( 'NONE',  ( 0.7071067811865487940, 0.7071067811865463515, 0.000000000000000000 ) ) ;
#22380 = VERTEX_POINT ( 'NONE', #50140 ) ;
#22381 = ADVANCED_FACE ( 'NONE', ( #94337 ), #39268, .F. ) ;
#22382 = VERTEX_POINT ( 'NONE', #12323 ) ;
#22383 = EDGE_LOOP ( 'NONE', ( #44938, #88409, #95510 ) ) ;
#22384 = DIRECTION ( 'NONE',  ( -0.7071067811865486830, -0.7071067811865464625, 0.000000000000000000 ) ) ;
#22385 = VERTEX_POINT ( 'NONE', #99315 ) ;
#22386 = EDGE_CURVE ( 'NONE', #11167, #2296, #87044, .T. ) ;
#22387 = ORIENTED_EDGE ( 'NONE', *, *, #30216, .T. ) ;
#22388 = CARTESIAN_POINT ( 'NONE',  ( -11.99451991528749417, 28.92564299267946382, 4.000000000000000000 ) ) ;
#22389 = CARTESIAN_POINT ( 'NONE',  ( 106.6833603837962272, -2.130196079827426203, 7.949999999999996625 ) ) ;
#22390 =( GEOMETRIC_REPRESENTATION_CONTEXT ( 3 ) GLOBAL_UNCERTAINTY_ASSIGNED_CONTEXT ( ( #101105 ) ) GLOBAL_UNIT_ASSIGNED_CONTEXT ( ( #21990, #108985, #142373 ) ) REPRESENTATION_CONTEXT ( 'NONE', 'WORKASPACE' ) );
#22391 = LINE ( 'NONE', #118331, #33391 ) ;
#22392 = DIRECTION ( 'NONE',  ( 0.3543493200069162685, -0.000000000000000000, -0.9351131265310288487 ) ) ;
#22393 = EDGE_LOOP ( 'NONE', ( #68227, #68323, #22953, #139223 ) ) ;
#22394 = DIRECTION ( 'NONE',  ( -0.7071067811865486830, 0.7071067811865464625, 0.000000000000000000 ) ) ;
#22395 = EDGE_LOOP ( 'NONE', ( #28654, #31700, #49735, #105031 ) ) ;
#22396 = VECTOR ( 'NONE', #87085, 1000.000000000000000 ) ;
#22399 = CONICAL_SURFACE ( 'NONE', #61789, 4.487534009422227577, 0.08726646259971666819 ) ;
#22398 = DIRECTION ( 'NONE',  ( -1.000000000000000000, -1.224606353822377258E-16, -0.000000000000000000 ) ) ;
#22397 = VECTOR ( 'NONE', #107406, 1000.000000000000000 ) ;
#22400 = VECTOR ( 'NONE', #52783, 1000.000000000000000 ) ;
#22401 = CARTESIAN_POINT ( 'NONE',  ( 17.27540314143521627, -2.126176841940958351, -7.934999999999989839 ) ) ;
#22402 = ORIENTED_EDGE ( 'NONE', *, *, #2885, .F. ) ;
#22403 = CARTESIAN_POINT ( 'NONE',  ( 85.51626352523145158, -4.472830434245839371, 4.472830434245839371 ) ) ;
#22404 = DIRECTION ( 'NONE',  ( -0.7071067811865486830, -0.7071067811865464625, 0.000000000000000000 ) ) ;
#22405 = EDGE_CURVE ( 'NONE', #124775, #80852, #719, .T. ) ;
#22406 = CARTESIAN_POINT ( 'NONE',  ( 27.48921356237309155, -27.52281430457074762, 5.000000000000000000 ) ) ;
#22407 = EDGE_LOOP ( 'NONE', ( #46622, #11570, #9179, #3624, #109864, #137690 ) ) ;
#22408 = VECTOR ( 'NONE', #54982, 1000.000000000000000 ) ;
#22409 = ORIENTED_EDGE ( 'NONE', *, *, #44892, .F. ) ;
#22410 = EDGE_LOOP ( 'NONE', ( #83547, #50713, #97423, #21574 ) ) ;
#22411 = DIRECTION ( 'NONE',  ( 0.6830127018922181881, 0.6830127018922202975, -0.2588190451025214056 ) ) ;
#22412 = LINE ( 'NONE', #12972, #12 ) ;
#22413 = DIRECTION ( 'NONE',  ( 0.3543493200069162685, -0.000000000000000000, -0.9351131265310288487 ) ) ;
#22414 = AXIS2_PLACEMENT_3D ( 'NONE', #128448, #29119, #116117 ) ;
#22415 = CARTESIAN_POINT ( 'NONE',  ( 16.78952603566995805, -0.07140279771002741582, -34.10863443292984698 ) ) ;
#22416 = CARTESIAN_POINT ( 'NONE',  ( 55.56056557994607914, -57.14999999999999147, 39.86617647058822200 ) ) ;
#22417 = LINE ( 'NONE', #10826, #70499 ) ;
#22418 = ORIENTED_EDGE ( 'NONE', *, *, #102075, .T. ) ;
#22419 = DIRECTION ( 'NONE',  ( 0.000000000000000000, -1.000000000000000000, 0.000000000000000000 ) ) ;
#22420 = ADVANCED_FACE ( 'NONE', ( #109505 ), #116564, .F. ) ;
#22421 = DIRECTION ( 'NONE',  ( 0.7071067811865486830, -0.7071067811865464625, -0.000000000000000000 ) ) ;
#22422 = DIRECTION ( 'NONE',  ( 0.6830127018922180770, -0.6830127018922204085, -0.2588190451025213501 ) ) ;
#22423 = VERTEX_POINT ( 'NONE', #64573 ) ;
#22424 = CARTESIAN_POINT ( 'NONE',  ( -34.49999999999975842, 22.21934299833216997, 4.348028800457638177 ) ) ;
#22425 = CARTESIAN_POINT ( 'NONE',  ( -23.99451991528749062, 28.92564299267954908, 4.000000000000000000 ) ) ;
#22426 = ORIENTED_EDGE ( 'NONE', *, *, #121619, .T. ) ;
#22429 = EDGE_CURVE ( 'NONE', #121175, #22931, #100069, .T. ) ;
#22428 = VERTEX_POINT ( 'NONE', #9439 ) ;
#22427 = LINE ( 'NONE', #119599, #27788 ) ;
#22430 = VERTEX_POINT ( 'NONE', #53720 ) ;
#22431 = PLANE ( 'NONE',  #67923 ) ;
#22433 = VECTOR ( 'NONE', #44384, 1000.000000000000000 ) ;
#22432 = PLANE ( 'NONE',  #136362 ) ;
#22434 = VERTEX_POINT ( 'NONE', #31947 ) ;
#22435 = LINE ( 'NONE', #111623, #79057 ) ;
#22436 = DIRECTION ( 'NONE',  ( 0.000000000000000000, 0.000000000000000000, -1.000000000000000000 ) ) ;
#22437 = CIRCLE ( 'NONE', #8554, 5.968999999999998529 ) ;
#22438 = DIRECTION ( 'NONE',  ( 0.3543493200069162685, -0.000000000000000000, -0.9351131265310288487 ) ) ;
#22439 = PLANE ( 'NONE',  #4474 ) ;
#22440 = EDGE_CURVE ( 'NONE', #87797, #71583, #27947, .T. ) ;
#22441 = CARTESIAN_POINT ( 'NONE',  ( -6.328169399223481761, -6.740707523384218192, 4.000000000000000000 ) ) ;
#22442 = CARTESIAN_POINT ( 'NONE',  ( 3.668467411598555383, -18.74070752338408496, 20.73178291233841719 ) ) ;
#22443 = CARTESIAN_POINT ( 'NONE',  ( 31.49999999999977973, -14.56887692260766443, 4.000000000000000000 ) ) ;
#22444 = DIRECTION ( 'NONE',  ( -0.6830127018922181881, 0.6830127018922202975, -0.2588190451025214056 ) ) ;
#22445 = CARTESIAN_POINT ( 'NONE',  ( 20.39540314143521726, 2.126176841940962348, 7.934999999999989839 ) ) ;
#22447 = CONICAL_SURFACE ( 'NONE', #8557, 1.898649999999993065, 1.029744258676648316 ) ;
#22446 = CARTESIAN_POINT ( 'NONE',  ( 32.99999999999977263, 7.007997736742474615, -8.085015511992036608 ) ) ;
#22448 = DIRECTION ( 'NONE',  ( -1.000000000000000000, -0.000000000000000000, -0.000000000000000000 ) ) ;
#22449 = FACE_OUTER_BOUND ( 'NONE', #86826, .T. ) ;
#22450 = CARTESIAN_POINT ( 'NONE',  ( -6.005480084712508493, 28.92564299267933947, 4.000000000000000000 ) ) ;
#22451 = ORIENTED_EDGE ( 'NONE', *, *, #21947, .F. ) ;
#22453 = ADVANCED_FACE ( 'NONE', ( #67464 ), #78315, .F. ) ;
#22452 =( BOUNDED_CURVE ( )  B_SPLINE_CURVE ( 2, ( #84748, #85436, #30360, #71753, #105066, #5727, #28942, #49995, #94178, #127534, #29630, #73183, #73873 ),
 .UNSPECIFIED., .F., .F. ) 
 B_SPLINE_CURVE_WITH_KNOTS ( ( 3, 2, 2, 2, 2, 2, 3 ),
 ( 0.2000000000000000666, 0.2083333333333333981, 0.2166666666666667018, 0.2250000000000000333, 0.2333333333333333648, 0.2416666666666666963, 0.2500000000000000000 ),
 .UNSPECIFIED. ) 
 CURVE ( )  GEOMETRIC_REPRESENTATION_ITEM ( )  RATIONAL_B_SPLINE_CURVE ( ( 0.9999999999999997780, 0.9659258262890685343, 1.000000000000000000, 0.9659258262890683122, 1.000000000000000000, 0.9659258262890683122, 1.000000000000000000, 0.9659258262890683122, 1.000000000000000000, 0.9659258262890683122, 1.000000000000000000, 0.9659258262890683122, 1.000000000000000000 ) ) 
 REPRESENTATION_ITEM ( '' )  );
#22454 = EDGE_LOOP ( 'NONE', ( #25449, #69268, #91917, #58359 ) ) ;
#22455 = CARTESIAN_POINT ( 'NONE',  ( 102.2083333333333286, -3.974999999999999201, -6.884901960086287964 ) ) ;
#22456 = ADVANCED_FACE ( 'NONE', ( #142159 ), #88486, .F. ) ;
#22457 = ORIENTED_EDGE ( 'NONE', *, *, #128123, .T. ) ;
#22458 = ORIENTED_EDGE ( 'NONE', *, *, #75768, .T. ) ;
#22459 = VERTEX_POINT ( 'NONE', #122505 ) ;
#22460 = CIRCLE ( 'NONE', #15511, 2.500000000000000444 ) ;
#22461 = FACE_OUTER_BOUND ( 'NONE', #57239, .T. ) ;
#22462 = DIRECTION ( 'NONE',  ( 1.000000000000000000, 0.000000000000000000, 0.000000000000000000 ) ) ;
#22463 = VERTEX_POINT ( 'NONE', #111655 ) ;
#22464 = CARTESIAN_POINT ( 'NONE',  ( -27.48921356237309155, -27.52281430457074762, 5.000000000000000000 ) ) ;
#22465 = CARTESIAN_POINT ( 'NONE',  ( 8.816011393731004731, 28.73617430169781173, 5.000000000000000000 ) ) ;
#22466 = CARTESIAN_POINT ( 'NONE',  ( -18.29974487139159223, -27.71228299555219010, 4.000000000000000000 ) ) ;
#22467 = DIRECTION ( 'NONE',  ( 0.7071067811865487940, 0.7071067811865463515, 0.000000000000000000 ) ) ;
#22468 = ORIENTED_EDGE ( 'NONE', *, *, #27887, .F. ) ;
#22469 = EDGE_CURVE ( 'NONE', #78949, #99639, #110197, .T. ) ;
#22470 = LINE ( 'NONE', #45018, #118243 ) ;
#22471 = DIRECTION ( 'NONE',  ( -0.6830127018922180770, -0.6830127018922204085, -0.2588190451025213501 ) ) ;
#22472 = CARTESIAN_POINT ( 'NONE',  ( -19.49999999999986144, -2.947814304570804289, 5.000000000000000000 ) ) ;
#22473 = FACE_OUTER_BOUND ( 'NONE', #30191, .T. ) ;
#22474 = DIRECTION ( 'NONE',  ( 0.7071067811865487940, -0.7071067811865463515, 0.000000000000000000 ) ) ;
#22475 = CARTESIAN_POINT ( 'NONE',  ( -45.29974487139158867, -27.71228299555237840, 4.000000000000000000 ) ) ;
#22476 = CARTESIAN_POINT ( 'NONE',  ( 22.60343192894629638, -14.24070752338413293, 19.24067776001730934 ) ) ;
#22477 = ORIENTED_EDGE ( 'NONE', *, *, #68076, .F. ) ;
#22478 = ORIENTED_EDGE ( 'NONE', *, *, #136792, .T. ) ;
#22479 = CARTESIAN_POINT ( 'NONE',  ( 119.5837635252314470, -6.110000000000001208, -3.741295971395164515E-16 ) ) ;
#22480 = VECTOR ( 'NONE', #102462, 999.9999999999998863 ) ;
#22481 = ORIENTED_EDGE ( 'NONE', *, *, #32698, .T. ) ;
#22482 = DIRECTION ( 'NONE',  ( -4.681814790819591790E-17, -0.3543493200069152693, 0.9351131265310292928 ) ) ;
#22483 = DIRECTION ( 'NONE',  ( 0.000000000000000000, 0.2631995976047524777, 0.9647414015272156584 ) ) ;
#22484 = DIRECTION ( 'NONE',  ( -0.7071067811865487940, 0.7071067811865463515, 0.000000000000000000 ) ) ;
#22485 = CARTESIAN_POINT ( 'NONE',  ( -9.707013264292978505, -21.74070752338405654, 4.999753212805220670 ) ) ;
#22486 = CARTESIAN_POINT ( 'NONE',  ( 115.7037635252314516, 6.109999999999998543, 1.122388791418548911E-15 ) ) ;
#22487 = ORIENTED_EDGE ( 'NONE', *, *, #113509, .F. ) ;
#22488 = VERTEX_POINT ( 'NONE', #10868 ) ;
#22489 = DIRECTION ( 'NONE',  ( -0.000000000000000000, 0.000000000000000000, 1.000000000000000000 ) ) ;
#22490 = CARTESIAN_POINT ( 'NONE',  ( 24.70710678118636494, 5.259292476615655687, 5.000000000000000000 ) ) ;
#22491 = EDGE_LOOP ( 'NONE', ( #62485, #96850, #66413, #19944, #93711 ) ) ;
#22492 = ORIENTED_EDGE ( 'NONE', *, *, #69820, .T. ) ;
#22493 = AXIS2_PLACEMENT_3D ( 'NONE', #86919, #10052, #75335 ) ;
#22494 = CARTESIAN_POINT ( 'NONE',  ( 36.89626352523143993, 4.472830434245840259, -4.472830434245839371 ) ) ;
#22495 = ORIENTED_EDGE ( 'NONE', *, *, #131907, .T. ) ;
#22496 = CARTESIAN_POINT ( 'NONE',  ( 25.49999999999982947, 12.05218569542904561, 5.000000000000000000 ) ) ;
#22497 = EDGE_CURVE ( 'NONE', #47367, #32623, #77616, .T. ) ;
#22498 = CARTESIAN_POINT ( 'NONE',  ( -34.47516574401892342, -8.971932658884083978, 4.998110765256835286 ) ) ;
#22499 = LINE ( 'NONE', #109543, #43840 ) ;
#22500 = AXIS2_PLACEMENT_3D ( 'NONE', #133119, #122188, #111319 ) ;
#22501 = VECTOR ( 'NONE', #33297, 1000.000000000000000 ) ;
#22503 = EDGE_CURVE ( 'NONE', #89327, #62049, #131260, .T. ) ;
#22502 = AXIS2_PLACEMENT_3D ( 'NONE', #36952, #91371, #26096 ) ;
#22504 = CARTESIAN_POINT ( 'NONE',  ( 31.99543019189811233, 5.291415217122916737, 3.055000000000001936 ) ) ;
#22505 = EDGE_CURVE ( 'NONE', #7925, #13538, #21055, .T. ) ;
#22506 = VERTEX_POINT ( 'NONE', #98617 ) ;
#22508 = ADVANCED_FACE ( 'NONE', ( #26075 ), #36242, .F. ) ;
#22507 = PLANE ( 'NONE',  #3862 ) ;
#22509 = ORIENTED_EDGE ( 'NONE', *, *, #89192, .T. ) ;
#22510 = ORIENTED_EDGE ( 'NONE', *, *, #114779, .F. ) ;
#22511 = VECTOR ( 'NONE', #91208, 1000.000000000000000 ) ;
#22512 = ORIENTED_EDGE ( 'NONE', *, *, #65951, .T. ) ;
#22513 = EDGE_CURVE ( 'NONE', #56805, #68414, #58754, .T. ) ;
#22514 = FACE_OUTER_BOUND ( 'NONE', #116631, .T. ) ;
#22515 = PLANE ( 'NONE',  #468 ) ;
#22516 = ORIENTED_EDGE ( 'NONE', *, *, #136201, .T. ) ;
#22517 = CARTESIAN_POINT ( 'NONE',  ( 6.066782984417857350, 4.584330080086930965E-16, 0.000000000000000000 ) ) ;
#22518 = EDGE_CURVE ( 'NONE', #14912, #36342, #24667, .T. ) ;
#22519 = CARTESIAN_POINT ( 'NONE',  ( -30.18398860626900060, 28.73617430169808173, 5.000000000000000000 ) ) ;
#22520 = SURFACE_STYLE_FILL_AREA ( #77668 ) ;
#22521 = CARTESIAN_POINT ( 'NONE',  ( 2.999999999999981792, 12.25461709320621218, -10.07315571508696550 ) ) ;
#22522 = EDGE_CURVE ( 'NONE', #32821, #129523, #103599, .T. ) ;
#22523 = FACE_BOUND ( 'NONE', #120254, .T. ) ;
#22524 = ORIENTED_EDGE ( 'NONE', *, *, #40272, .T. ) ;
#22525 = EDGE_CURVE ( 'NONE', #71456, #71262, #125391, .T. ) ;
#22526 = LINE ( 'NONE', #67525, #88443 ) ;
#22527 = ORIENTED_EDGE ( 'NONE', *, *, #131088, .F. ) ;
#22528 = DIRECTION ( 'NONE',  ( -0.000000000000000000, -1.000000000000000000, -0.000000000000000000 ) ) ;
#22529 = ORIENTED_EDGE ( 'NONE', *, *, #99440, .T. ) ;
#22530 = AXIS2_PLACEMENT_3D ( 'NONE', #141715, #130855, #31520 ) ;
#22531 = ORIENTED_EDGE ( 'NONE', *, *, #108806, .T. ) ;
#22532 = DIRECTION ( 'NONE',  ( -0.000000000000000000, -0.3543493200069152693, 0.9351131265310292928 ) ) ;
#22533 = EDGE_CURVE ( 'NONE', #63799, #38880, #4236, .T. ) ;
#22534 = ORIENTED_EDGE ( 'NONE', *, *, #101467, .F. ) ;
#22535 = CARTESIAN_POINT ( 'NONE',  ( 50.66209685856478018, -5.291415217122919401, 3.054999999999997939 ) ) ;
#22536 = VERTEX_POINT ( 'NONE', #123968 ) ;
#22537 = LINE ( 'NONE', #100846, #99616 ) ;
#22538 = SURFACE_STYLE_USAGE ( .BOTH. , #121860 ) ;
#22539 = DIRECTION ( 'NONE',  ( 0.7071067811865487940, -0.7071067811865463515, 0.000000000000000000 ) ) ;
#22540 = EDGE_LOOP ( 'NONE', ( #85478, #104753, #35434, #15432 ) ) ;
#22541 = DIRECTION ( 'NONE',  ( 0.7071067811865487940, 0.7071067811865463515, 0.000000000000000000 ) ) ;
#22542 = DIRECTION ( 'NONE',  ( 1.000000000000000000, 0.000000000000000000, -0.000000000000000000 ) ) ;
#22543 = AXIS2_PLACEMENT_3D ( 'NONE', #54128, #21465, #75162 ) ;
#22544 = CARTESIAN_POINT ( 'NONE',  ( 20.99999999999985079, 4.384688058510579189, -7.090945410444635222 ) ) ;
#22545 = CARTESIAN_POINT ( 'NONE',  ( 7.499999999999956479, 3.052185695429141976, 5.000000000000000000 ) ) ;
#22546 = PLANE ( 'NONE',  #36596 ) ;
#22547 = CARTESIAN_POINT ( 'NONE',  ( 29.29289321881325137, 2.259292476615696099, 5.000000000000000000 ) ) ;
#22548 = CARTESIAN_POINT ( 'NONE',  ( -15.48921356237309510, -27.52281430457066236, 5.000000000000000000 ) ) ;
#22549 = ORIENTED_EDGE ( 'NONE', *, *, #16848, .F. ) ;
#22550 = ADVANCED_FACE ( 'NONE', ( #79787 ), #124662, .F. ) ;
#22551 = ORIENTED_EDGE ( 'NONE', *, *, #37365, .T. ) ;
#22552 = ORIENTED_EDGE ( 'NONE', *, *, #42010, .T. ) ;
#22553 = CARTESIAN_POINT ( 'NONE',  ( -9.005480084712511157, 28.92564299267931816, 4.000000000000000000 ) ) ;
#22554 = CARTESIAN_POINT ( 'NONE',  ( 30.48921356237309510, -27.52281430457076894, 5.000000000000000000 ) ) ;
#22555 = ORIENTED_EDGE ( 'NONE', *, *, #42660, .T. ) ;
#22556 = ORIENTED_EDGE ( 'NONE', *, *, #84416, .F. ) ;
#22557 = CARTESIAN_POINT ( 'NONE',  ( 23.81601139373100295, 28.73617430169770870, 5.000000000000000000 ) ) ;
#22558 = CARTESIAN_POINT ( 'NONE',  ( 60.18398860626900415, 28.73617430169829490, 5.000000000000000000 ) ) ;
#22559 = VERTEX_POINT ( 'NONE', #114482 ) ;
#22560 = PLANE ( 'NONE',  #129675 ) ;
#22561 = ADVANCED_FACE ( 'NONE', ( #26772 ), #47859, .T. ) ;
#22562 = CARTESIAN_POINT ( 'NONE',  ( 181.1500000000000057, 0.000000000000000000, 31.92499999999998295 ) ) ;
#22563 = CARTESIAN_POINT ( 'NONE',  ( 31.56706980810188767, 2.126176841940952134, -7.934999999999993392 ) ) ;
#22564 = FACE_OUTER_BOUND ( 'NONE', #24900, .T. ) ;
#22565 = ORIENTED_EDGE ( 'NONE', *, *, #31891, .F. ) ;
#22566 = CARTESIAN_POINT ( 'NONE',  ( 110.3079301918980946, -6.109999999999999432, 1.637169565754158507 ) ) ;
#22567 = MECHANICAL_DESIGN_GEOMETRIC_PRESENTATION_REPRESENTATION (  '', ( #85107 ), #27242 ) ;
#22569 = EDGE_CURVE ( 'NONE', #45966, #82836, #2125, .T. ) ;
#22568 = LINE ( 'NONE', #87865, #88235 ) ;
#22570 = CARTESIAN_POINT ( 'NONE',  ( 20.51159235450331764, 2.500000000000001332, 0.000000000000000000 ) ) ;
#22572 = EDGE_LOOP ( 'NONE', ( #123361, #100491, #115822, #136836 ) ) ;
#22571 = DIRECTION ( 'NONE',  ( 0.7071067811865486830, -0.7071067811865464625, -0.000000000000000000 ) ) ;
#22573 = CARTESIAN_POINT ( 'NONE',  ( 42.18398860626899705, 28.73617430169816700, 5.000000000000000000 ) ) ;
#22574 = ORIENTED_EDGE ( 'NONE', *, *, #105326, .T. ) ;
#22575 = DIRECTION ( 'NONE',  ( -0.6830127018922180770, -0.6830127018922204085, -0.2588190451025213501 ) ) ;
#22576 = DIRECTION ( 'NONE',  ( 0.000000000000000000, -3.469446951953615372E-15, 1.000000000000000000 ) ) ;
#22577 = DIRECTION ( 'NONE',  ( -0.6830127018922180770, -0.6830127018922204085, -0.2588190451025213501 ) ) ;
#22578 = CARTESIAN_POINT ( 'NONE',  ( 6.628407645496676714, 9.139736423841732040E-16, 0.000000000000000000 ) ) ;
#22579 = ORIENTED_EDGE ( 'NONE', *, *, #38590, .T. ) ;
#22580 = CARTESIAN_POINT ( 'NONE',  ( 24.48921356237309510, -27.52281430457072631, 5.000000000000000000 ) ) ;
#22581 = VECTOR ( 'NONE', #44649, 999.9999999999998863 ) ;
#22582 = ADVANCED_FACE ( 'NONE', ( #81916 ), #90626, .F. ) ;
#22583 = DIRECTION ( 'NONE',  ( 0.7071067811865486830, -0.7071067811865464625, -0.000000000000000000 ) ) ;
#22584 = DIRECTION ( 'NONE',  ( 0.000000000000000000, -1.000000000000000000, 0.000000000000000000 ) ) ;
#22585 = ORIENTED_EDGE ( 'NONE', *, *, #143458, .F. ) ;
#22586 = DIRECTION ( 'NONE',  ( -0.000000000000000000, 0.3543493200069153248, 0.9351131265310292928 ) ) ;
#22587 = VECTOR ( 'NONE', #47612, 1000.000000000000000 ) ;
#22588 = DIRECTION ( 'NONE',  ( -1.000000000000000000, -1.224606353822377258E-16, -0.000000000000000000 ) ) ;
#22589 = ORIENTED_EDGE ( 'NONE', *, *, #59113, .F. ) ;
#22590 = CARTESIAN_POINT ( 'NONE',  ( -68.99451991528748351, 28.92564299267986172, 4.000000000000000000 ) ) ;
#22593 = ADVANCED_FACE ( 'NONE', ( #115172 ), #15847, .F. ) ;
#22592 = ORIENTED_EDGE ( 'NONE', *, *, #71343, .F. ) ;
#22591 = CARTESIAN_POINT ( 'NONE',  ( -19.05499999999999261, 3.130000000000007887, -2.396719511207313368E-16 ) ) ;
#22594 = APPLICATION_CONTEXT ( 'automotive_design' ) ;
#22595 = ORIENTED_EDGE ( 'NONE', *, *, #126752, .T. ) ;
#22596 = FACE_OUTER_BOUND ( 'NONE', #70736, .T. ) ;
#22597 = DIRECTION ( 'NONE',  ( 0.6830127018922180770, -0.6830127018922204085, -0.2588190451025213501 ) ) ;
#22598 = AXIS2_PLACEMENT_3D ( 'NONE', #82491, #38976, #81074 ) ;
#22599 = ORIENTED_EDGE ( 'NONE', *, *, #28561, .F. ) ;
#22600 = AXIS2_PLACEMENT_3D ( 'NONE', #127777, #28463, #74098 ) ;
#22601 = CARTESIAN_POINT ( 'NONE',  ( -34.92500000000001137, -22.22500000000000142, 4.000000000000000000 ) ) ;
#22602 = LINE ( 'NONE', #99458, #123208 ) ;
#22603 = ORIENTED_EDGE ( 'NONE', *, *, #128025, .F. ) ;
#22604 = PLANE ( 'NONE',  #125312 ) ;
#22605 = CARTESIAN_POINT ( 'NONE',  ( 2.999999999999979128, -18.41253812416056945, 4.000000000000000000 ) ) ;
#22606 = LINE ( 'NONE', #68339, #9990 ) ;
#22607 = CARTESIAN_POINT ( 'NONE',  ( -5.999999999999970690, -16.02097659208072855, -11.96015758381207483 ) ) ;
#22608 = CARTESIAN_POINT ( 'NONE',  ( 128.1208603837962130, -6.884901960086286188, 3.974999999999997424 ) ) ;
#22609 = CARTESIAN_POINT ( 'NONE',  ( 18.32840764549667512, 9.139736423841732040E-16, 0.000000000000000000 ) ) ;
#22610 = EDGE_CURVE ( 'NONE', #121879, #65772, #49760, .T. ) ;
#22611 = EDGE_LOOP ( 'NONE', ( #50215, #59343, #48469, #36546 ) ) ;
#22612 = VERTEX_POINT ( 'NONE', #23937 ) ;
#22613 = CARTESIAN_POINT ( 'NONE',  ( 2.700255128608413990, -27.71228299555204089, 4.000000000000000000 ) ) ;
#22614 = ADVANCED_FACE ( 'NONE', ( #68885 ), #74217, .F. ) ;
#22615 = ORIENTED_EDGE ( 'NONE', *, *, #130929, .F. ) ;
#22616 = ORIENTED_EDGE ( 'NONE', *, *, #75264, .T. ) ;
#22617 = CARTESIAN_POINT ( 'NONE',  ( -7.499999999999947597, -11.56887692260769818, 4.000000000000000000 ) ) ;
#22618 = CARTESIAN_POINT ( 'NONE',  ( -8.475998614145453303, 22.03583458319437938, 4.979811245910092055 ) ) ;
#22619 = VERTEX_POINT ( 'NONE', #13025 ) ;
#22620 = FILL_AREA_STYLE ('',( #43003 ) ) ;
#22621 = FACE_OUTER_BOUND ( 'NONE', #86197, .T. ) ;
#22622 = CARTESIAN_POINT ( 'NONE',  ( 10.82816939922345689, -5.240707523384232402, 4.000000000000000000 ) ) ;
#22623 = LINE ( 'NONE', #133581, #7016 ) ;
#22624 = CARTESIAN_POINT ( 'NONE',  ( 119.8754301918981184, -5.291415217122920289, -3.055000000000001492 ) ) ;
#22625 = VERTEX_POINT ( 'NONE', #13730 ) ;
#22626 = EDGE_CURVE ( 'NONE', #42005, #96774, #102221, .T. ) ;
#22627 = LINE ( 'NONE', #20497, #34879 ) ;
#22628 = LINE ( 'NONE', #77082, #118636 ) ;
#22629 = CIRCLE ( 'NONE', #17968, 5.968999999999998529 ) ;
#22630 = LINE ( 'NONE', #99487, #58899 ) ;
#22631 = PRESENTATION_STYLE_ASSIGNMENT (( #95225 ) ) ;
#22632 = DIRECTION ( 'NONE',  ( 0.000000000000000000, -1.000000000000000000, 0.000000000000000000 ) ) ;
#22633 =( BOUNDED_CURVE ( )  B_SPLINE_CURVE ( 3, ( #20657, #141762, #119949, #40319 ),
 .UNSPECIFIED., .F., .T. ) 
 B_SPLINE_CURVE_WITH_KNOTS ( ( 4, 4 ),
 ( 1.864375635226939387, 1.933014472006533868 ),
 .UNSPECIFIED. ) 
 CURVE ( )  GEOMETRIC_REPRESENTATION_ITEM ( )  RATIONAL_B_SPLINE_CURVE ( ( 1.000000000000000000, 0.9996074310407766506, 0.9996074310407766506, 1.000000000000000000 ) ) 
 REPRESENTATION_ITEM ( '' )  );
#22634 = DIRECTION ( 'NONE',  ( 0.6830127018922181881, 0.6830127018922202975, -0.2588190451025214056 ) ) ;
#22635 = CARTESIAN_POINT ( 'NONE',  ( 103.0375270504628986, -9.735942053221456900E-16, 7.949999999999998401 ) ) ;
#22636 = PRODUCT_DEFINITION ( 'UNKNOWN', '', #37846, #63247 ) ;
#22637 = CARTESIAN_POINT ( 'NONE',  ( 46.45419371712955581, 6.884901960086283523, 3.975000000000002753 ) ) ;
#22638 = DIRECTION ( 'NONE',  ( 0.7071067811865487940, 0.7071067811865463515, 0.000000000000000000 ) ) ;
#22639 = DIRECTION ( 'NONE',  ( -0.7071067811865486830, 0.7071067811865464625, 0.000000000000000000 ) ) ;
#22640 = ORIENTED_EDGE ( 'NONE', *, *, #125985, .T. ) ;
#22641 = ORIENTED_EDGE ( 'NONE', *, *, #79714, .F. ) ;
#22642 = CARTESIAN_POINT ( 'NONE',  ( 41.68749999999997868, -5.819803920172573086, 5.819803920172572198 ) ) ;
#22643 = FACE_OUTER_BOUND ( 'NONE', #32085, .T. ) ;
#22644 = CARTESIAN_POINT ( 'NONE',  ( 17.99999999999988276, -16.44781430457067373, 5.000000000000000000 ) ) ;
#22645 = ORIENTED_EDGE ( 'NONE', *, *, #92410, .F. ) ;
#22646 = CARTESIAN_POINT ( 'NONE',  ( -0.3439913038278733515, -1.278150760195258862, 3.986088164604868478 ) ) ;
#22647 = EDGE_CURVE ( 'NONE', #140847, #95118, #47170, .T. ) ;
#22648 = LINE ( 'NONE', #45894, #44597 ) ;
#22649 = CARTESIAN_POINT ( 'NONE',  ( 36.45876352523143282, 0.000000000000000000, -6.110000000000001208 ) ) ;
#22650 = VERTEX_POINT ( 'NONE', #18727 ) ;
#22651 = DIRECTION ( 'NONE',  ( 1.000000000000000000, 0.000000000000000000, 0.000000000000000000 ) ) ;
#22652 = ORIENTED_EDGE ( 'NONE', *, *, #30985, .F. ) ;
#22653 = VERTEX_POINT ( 'NONE', #7119 ) ;
#22654 = DIRECTION ( 'NONE',  ( 1.000000000000000000, 0.000000000000000000, 0.000000000000000000 ) ) ;
#22655 = PLANE ( 'NONE',  #40770 ) ;
#22656 = FILL_AREA_STYLE_COLOUR ( '', #141646 ) ;
#22657 = AXIS2_PLACEMENT_3D ( 'NONE', #47583, #67912, #36647 ) ;
#22658 = FACE_OUTER_BOUND ( 'NONE', #20577, .T. ) ;
#22659 = ORIENTED_EDGE ( 'NONE', *, *, #123635, .T. ) ;
#22660 = DIRECTION ( 'NONE',  ( 0.7071067811865486830, -0.7071067811865464625, -0.000000000000000000 ) ) ;
#22661 = EDGE_LOOP ( 'NONE', ( #41402, #43038, #130511, #115633 ) ) ;
#22662 = CARTESIAN_POINT ( 'NONE',  ( 82.68793019189810423, 6.110000000000002984, -1.637169565754156730 ) ) ;
#22663 = DIRECTION ( 'NONE',  ( -0.000000000000000000, 0.000000000000000000, 1.000000000000000000 ) ) ;
#22664 = DIRECTION ( 'NONE',  ( -0.000000000000000000, -0.3543493200069152693, 0.9351131265310292928 ) ) ;
#22665 = LINE ( 'NONE', #21981, #111685 ) ;
#22666 = LINE ( 'NONE', #98139, #118083 ) ;
#22667 = PRESENTATION_STYLE_ASSIGNMENT (( #30752 ) ) ;
#22668 = EDGE_CURVE ( 'NONE', #106721, #128260, #5709, .T. ) ;
#22669 = ORIENTED_EDGE ( 'NONE', *, *, #48260, .T. ) ;
#22670 = CARTESIAN_POINT ( 'NONE',  ( 87.43336038379622721, 2.130196079827431532, -7.949999999999996625 ) ) ;
#22671 = CARTESIAN_POINT ( 'NONE',  ( 62.47459685856478018, 1.637169565754164058, -6.109999999999996767 ) ) ;
#22672 = EDGE_CURVE ( 'NONE', #38343, #97996, #62277, .T. ) ;
#22673 = LINE ( 'NONE', #67689, #115802 ) ;
#22674 = DIRECTION ( 'NONE',  ( -0.7071067811865486830, -0.7071067811865464625, -0.000000000000000000 ) ) ;
#22675 = DIRECTION ( 'NONE',  ( -0.6830127018922180770, -0.6830127018922204085, -0.2588190451025213501 ) ) ;
#22676 = ORIENTED_EDGE ( 'NONE', *, *, #91169, .T. ) ;
#22677 = DIRECTION ( 'NONE',  ( 0.7071067811865487940, -0.7071067811865463515, 0.000000000000000000 ) ) ;
#22678 = ORIENTED_EDGE ( 'NONE', *, *, #75299, .T. ) ;
#22679 = EDGE_CURVE ( 'NONE', #49576, #83993, #73852, .T. ) ;
#22680 = EDGE_CURVE ( 'NONE', #49245, #42277, #128246, .T. ) ;
#22681 = CARTESIAN_POINT ( 'NONE',  ( 33.97743759385590323, 22.27000000000000668, -13.09127955744558847 ) ) ;
#22682 = VERTEX_POINT ( 'NONE', #82588 ) ;
#22683 = LINE ( 'NONE', #45235, #95536 ) ;
#22684 = PLANE ( 'NONE',  #3952 ) ;
#22685 = AXIS2_PLACEMENT_3D ( 'NONE', #27405, #137639, #128873 ) ;
#22686 = CARTESIAN_POINT ( 'NONE',  ( 40.98012225071428105, -17.24070752338409562, 20.23474786156478089 ) ) ;
#22687 = VECTOR ( 'NONE', #137222, 1000.000000000000000 ) ;
#22688 = EDGE_CURVE ( 'NONE', #53362, #116882, #30218, .T. ) ;
#22689 = FACE_BOUND ( 'NONE', #71688, .T. ) ;
#22690 = EDGE_CURVE ( 'NONE', #107445, #52778, #112802, .T. ) ;
#22691 = CARTESIAN_POINT ( 'NONE',  ( 2.999999999999981792, -6.108550654416958992, -3.114665004254960845 ) ) ;
#22692 = LINE ( 'NONE', #13971, #35260 ) ;
#22693 = CARTESIAN_POINT ( 'NONE',  ( 75.18398860626899705, 28.73617430169839793, 5.000000000000000000 ) ) ;
#22695 = EDGE_LOOP ( 'NONE', ( #84259, #140302, #39994, #16378 ) ) ;
#22694 = LINE ( 'NONE', #12560, #15734 ) ;
#22696 = AXIS2_PLACEMENT_3D ( 'NONE', #9149, #30235, #63619 ) ;
#22697 = VECTOR ( 'NONE', #121684, 1000.000000000000000 ) ;
#22698 = FACE_OUTER_BOUND ( 'NONE', #25280, .T. ) ;
#22699 = ADVANCED_FACE ( 'NONE', ( #28921 ), #63007, .F. ) ;
#22700 = ORIENTED_EDGE ( 'NONE', *, *, #17630, .F. ) ;
#22701 = ORIENTED_EDGE ( 'NONE', *, *, #114547, .F. ) ;
#22702 = CARTESIAN_POINT ( 'NONE',  ( 72.39126352523145158, -4.472830434245838482, -4.472830434245838482 ) ) ;
#22703 = ORIENTED_EDGE ( 'NONE', *, *, #83532, .F. ) ;
#22704 = DIRECTION ( 'NONE',  ( -0.6830127018922180770, -0.6830127018922204085, -0.2588190451025213501 ) ) ;
#22705 = DIRECTION ( 'NONE',  ( 0.000000000000000000, -1.000000000000000000, 0.000000000000000000 ) ) ;
#22706 = VERTEX_POINT ( 'NONE', #73161 ) ;
#22707 = LINE ( 'NONE', #11120, #44424 ) ;
#22708 = EDGE_CURVE ( 'NONE', #2860, #124916, #118023, .T. ) ;
#22709 = DIRECTION ( 'NONE',  ( -0.7071067811865487940, 0.7071067811865463515, 0.000000000000000000 ) ) ;
#22710 = LINE ( 'NONE', #100325, #90079 ) ;
#22711 = CARTESIAN_POINT ( 'NONE',  ( 30.70710678118632941, 5.259292476615665457, 5.000000000000000000 ) ) ;
#22712 = DIRECTION ( 'NONE',  ( 0.3543493200069163240, -0.000000000000000000, -0.9351131265310288487 ) ) ;
#22714 = FACE_OUTER_BOUND ( 'NONE', #60543, .T. ) ;
#22713 = CARTESIAN_POINT ( 'NONE',  ( 14.99999999999989519, -15.41253812416060143, 4.000000000000000000 ) ) ;
#22715 = DIRECTION ( 'NONE',  ( 0.7071067811865486830, -0.7071067811865464625, -0.000000000000000000 ) ) ;
#22716 = PLANE ( 'NONE',  #60201 ) ;
#22717 = VERTEX_POINT ( 'NONE', #138394 ) ;
#22718 = EDGE_CURVE ( 'NONE', #76267, #104640, #41208, .T. ) ;
#22719 = CARTESIAN_POINT ( 'NONE',  ( 0.000000000000000000, -22.26999999999999247, -40.00000000000000000 ) ) ;
#22720 = VERTEX_POINT ( 'NONE', #128937 ) ;
#22721 = DIRECTION ( 'NONE',  ( 0.7071067811865486830, -0.7071067811865464625, -0.000000000000000000 ) ) ;
#22722 = LINE ( 'NONE', #122788, #67541 ) ;
#22723 = ORIENTED_EDGE ( 'NONE', *, *, #86269, .F. ) ;
#22724 = VECTOR ( 'NONE', #126739, 1000.000000000000000 ) ;
#22725 = ORIENTED_EDGE ( 'NONE', *, *, #100152, .F. ) ;
#22726 = VECTOR ( 'NONE', #128336, 1000.000000000000000 ) ;
#22727 = ORIENTED_EDGE ( 'NONE', *, *, #129548, .T. ) ;
#22728 = DIRECTION ( 'NONE',  ( 0.6830127018922180770, -0.6830127018922204085, -0.2588190451025213501 ) ) ;
#22729 = ADVANCED_FACE ( 'NONE', ( #38374 ), #61581, .F. ) ;
#22730 = ORIENTED_EDGE ( 'NONE', *, *, #14629, .T. ) ;
#22731 = DIRECTION ( 'NONE',  ( -0.7071067811865486830, -0.7071067811865464625, -0.000000000000000000 ) ) ;
#22732 = ADVANCED_FACE ( 'NONE', ( #27468 ), #29610, .F. ) ;
#22733 = DIRECTION ( 'NONE',  ( -0.7071067811865486830, -0.7071067811865464625, 0.000000000000000000 ) ) ;
#22734 = CARTESIAN_POINT ( 'NONE',  ( 0.06706980810188606368, 2.126176841940952134, -7.934999999999993392 ) ) ;
#22735 = DIRECTION ( 'NONE',  ( -0.7071067811865487940, 0.7071067811865463515, -0.000000000000000000 ) ) ;
#22736 = ORIENTED_EDGE ( 'NONE', *, *, #9737, .T. ) ;
#22737 = PLANE ( 'NONE',  #96616 ) ;
#22738 = LINE ( 'NONE', #111191, #30270 ) ;
#22739 = DIRECTION ( 'NONE',  ( 0.7071067811865487940, -0.7071067811865463515, 0.000000000000000000 ) ) ;
#22741 = EDGE_LOOP ( 'NONE', ( #117758, #57753, #96799, #78039 ) ) ;
#22740 = CARTESIAN_POINT ( 'NONE',  ( 28.73493329717932099, 12.75929247661559351, 18.34774599283949570 ) ) ;
#22742 = VERTEX_POINT ( 'NONE', #115892 ) ;
#22743 = CARTESIAN_POINT ( 'NONE',  ( -23.99999999999983302, -16.60178936734450517, 0.8616154019346934367 ) ) ;
#22744 = CARTESIAN_POINT ( 'NONE',  ( -29.99999999999978684, 20.96639925780205616, 5.000000000000000000 ) ) ;
#22745 = DIRECTION ( 'NONE',  ( 0.3543493200069162685, -0.000000000000000000, -0.9351131265310288487 ) ) ;
#22746 = ORIENTED_EDGE ( 'NONE', *, *, #102383, .F. ) ;
#22747 = CARTESIAN_POINT ( 'NONE',  ( -13.49999999999989342, -20.94781430457062754, 5.000000000000000000 ) ) ;
#22748 = CARTESIAN_POINT ( 'NONE',  ( 34.42499999999998295, -15.02281430457044742, 5.000000000000000000 ) ) ;
#22749 = VERTEX_POINT ( 'NONE', #140518 ) ;
#22750 = ADVANCED_FACE ( 'NONE', ( #105045 ), #51400, .F. ) ;
#22751 = CARTESIAN_POINT ( 'NONE',  ( 0.000000000000000000, 0.000000000000000000, 5.000000000000000000 ) ) ;
#22752 = LINE ( 'NONE', #97484, #136465 ) ;
#22753 = DIRECTION ( 'NONE',  ( 1.000000000000000000, 0.000000000000000000, -0.000000000000000000 ) ) ;
#22754 = DIRECTION ( 'NONE',  ( -0.6830127018922180770, -0.6830127018922204085, -0.2588190451025213501 ) ) ;
#22755 = PLANE ( 'NONE',  #47127 ) ;
#22756 = CARTESIAN_POINT ( 'NONE',  ( 8.510786437626906675, -27.52281430457049183, 5.000000000000000000 ) ) ;
#22758 = EDGE_CURVE ( 'NONE', #20875, #84665, #49975, .T. ) ;
#22757 = VERTEX_POINT ( 'NONE', #60885 ) ;
#22759 = CARTESIAN_POINT ( 'NONE',  ( 96.18336038379621300, -2.130196079827426203, 7.949999999999996625 ) ) ;
#22760 = ORIENTED_EDGE ( 'NONE', *, *, #57288, .T. ) ;
#22761 = LINE ( 'NONE', #25654, #35532 ) ;
#22762 = CARTESIAN_POINT ( 'NONE',  ( 10.82816939922345689, 15.75929247661555799, 4.000000000000000000 ) ) ;
#22763 = ORIENTED_EDGE ( 'NONE', *, *, #118800, .F. ) ;
#22764 = FACE_OUTER_BOUND ( 'NONE', #2048, .T. ) ;
#22765 = PLANE ( 'NONE',  #37208 ) ;
#22766 = FACE_OUTER_BOUND ( 'NONE', #10827, .T. ) ;
#22767 = VERTEX_POINT ( 'NONE', #126784 ) ;
#22768 = CARTESIAN_POINT ( 'NONE',  ( -2.999999999999975575, -15.41253812416059787, 4.000000000000000000 ) ) ;
#22769 = CARTESIAN_POINT ( 'NONE',  ( -57.48921356237308800, -27.52281430457095368, 5.000000000000000000 ) ) ;
#22770 = UNCERTAINTY_MEASURE_WITH_UNIT (LENGTH_MEASURE( 1.000000000000000082E-05 ), #123847, 'distance_accuracy_value', 'NONE');
#22771 = DIRECTION ( 'NONE',  ( 1.000000000000000000, 1.224606353822377258E-16, 0.000000000000000000 ) ) ;
#22772 = CARTESIAN_POINT ( 'NONE',  ( 10.11017322888203651, -22.22500000000000853, 4.785647885939353863 ) ) ;
#22773 = CARTESIAN_POINT ( 'NONE',  ( 58.97459685856478018, 1.637169565754164280, -6.109999999999997655 ) ) ;
#22774 = DIRECTION ( 'NONE',  ( -0.7071067811865486830, -0.7071067811865464625, 0.000000000000000000 ) ) ;
#22775 = DIRECTION ( 'NONE',  ( 0.3543493200069162685, -0.000000000000000000, -0.9351131265310288487 ) ) ;
#22776 = CARTESIAN_POINT ( 'NONE',  ( 31.87086038379621655, 6.884901960086289741, -3.974999999999993427 ) ) ;
#22777 = CARTESIAN_POINT ( 'NONE',  ( 80.99451991528748351, 28.92564299267994699, 4.000000000000000000 ) ) ;
#22778 = EDGE_CURVE ( 'NONE', #70701, #71611, #72472, .T. ) ;
#22779 = ORIENTED_EDGE ( 'NONE', *, *, #137503, .T. ) ;
#22780 = EDGE_LOOP ( 'NONE', ( #43854, #77497, #92588, #50747 ) ) ;
#22781 = CARTESIAN_POINT ( 'NONE',  ( -3.183988606268992161, 28.73617430169789699, 5.000000000000000000 ) ) ;
#22782 = DIRECTION ( 'NONE',  ( 0.000000000000000000, 6.938893903907227589E-15, -1.000000000000000000 ) ) ;
#22783 = AXIS2_PLACEMENT_3D ( 'NONE', #118663, #107769, #75196 ) ;
#22784 = VECTOR ( 'NONE', #36183, 1000.000000000000000 ) ;
#22785 = VECTOR ( 'NONE', #97979, 999.9999999999998863 ) ;
#22786 = DIRECTION ( 'NONE',  ( -0.000000000000000000, 0.000000000000000000, 1.000000000000000000 ) ) ;
#22787 = CARTESIAN_POINT ( 'NONE',  ( 60.18398860626900415, 28.73617430169829490, 5.000000000000000000 ) ) ;
#22788 = VECTOR ( 'NONE', #59834, 1000.000000000000227 ) ;
#22789 = CYLINDRICAL_SURFACE ( 'NONE', #97138, 9.119999999999999218 ) ;
#22790 = EDGE_CURVE ( 'NONE', #33217, #66395, #71731, .T. ) ;
#22791 = CARTESIAN_POINT ( 'NONE',  ( -66.48921356237309510, -27.52281430457101763, 5.000000000000000000 ) ) ;
#22792 = DIRECTION ( 'NONE',  ( 1.000000000000000000, 0.000000000000000000, 0.000000000000000000 ) ) ;
#22793 = ORIENTED_EDGE ( 'NONE', *, *, #124181, .T. ) ;
#22794 = EDGE_CURVE ( 'NONE', #100764, #64995, #87582, .T. ) ;
#22795 = ORIENTED_EDGE ( 'NONE', *, *, #28799, .F. ) ;
#22796 = DIRECTION ( 'NONE',  ( -1.000000000000000000, -0.000000000000000000, -0.000000000000000000 ) ) ;
#22797 = DIRECTION ( 'NONE',  ( -1.000000000000000000, -0.000000000000000000, -0.000000000000000000 ) ) ;
#22798 = UNCERTAINTY_MEASURE_WITH_UNIT (LENGTH_MEASURE( 1.000000000000000082E-05 ), #9007, 'distance_accuracy_value', 'NONE');
#22799 = VECTOR ( 'NONE', #73939, 1000.000000000000000 ) ;
#22800 = AXIS2_PLACEMENT_3D ( 'NONE', #35871, #114787, #24936 ) ;
#22801 = CARTESIAN_POINT ( 'NONE',  ( -28.82816939922332011, -14.24070752338413826, 4.000000000000000000 ) ) ;
#22802 = CARTESIAN_POINT ( 'NONE',  ( 16.96247294953710849, -7.464222240803106570E-16, -6.094999999999989981 ) ) ;
#22803 = CARTESIAN_POINT ( 'NONE',  ( 73.57919371712957002, 3.975000000000002753, -6.884901960086283523 ) ) ;
#22804 = DIRECTION ( 'NONE',  ( 0.6830127018922180770, -0.6830127018922204085, -0.2588190451025213501 ) ) ;
#22805 = EDGE_CURVE ( 'NONE', #62799, #101394, #66551, .T. ) ;
#22806 = CARTESIAN_POINT ( 'NONE',  ( 34.92499999999998295, 18.75929247661552779, 4.255531930566162302 ) ) ;
#22807 = ORIENTED_EDGE ( 'NONE', *, *, #85201, .F. ) ;
#22808 = CARTESIAN_POINT ( 'NONE',  ( 69.10416666666665719, 2.130196079827422206, 7.950000000000001954 ) ) ;
#22809 = ADVANCED_FACE ( 'NONE', ( #96982 ), #8537, .F. ) ;
#22810 = DIRECTION ( 'NONE',  ( 0.000000000000000000, 0.000000000000000000, 1.000000000000000000 ) ) ;
#22811 = LINE ( 'NONE', #95235, #78660 ) ;
#22812 = FACE_OUTER_BOUND ( 'NONE', #30277, .T. ) ;
#22813 = PRESENTATION_LAYER_ASSIGNMENT (  '', '', ( #52835 ) ) ;
#22814 = ORIENTED_EDGE ( 'NONE', *, *, #38822, .T. ) ;
#22815 = EDGE_CURVE ( 'NONE', #117989, #120212, #32500, .T. ) ;
#22816 = DIRECTION ( 'NONE',  ( 1.000000000000000000, 0.000000000000000000, 0.000000000000000000 ) ) ;
#22817 = ORIENTED_EDGE ( 'NONE', *, *, #8599, .T. ) ;
#22818 = VECTOR ( 'NONE', #116983, 1000.000000000000000 ) ;
#22819 = DIRECTION ( 'NONE',  ( -0.7071067811865486830, -0.7071067811865464625, 0.000000000000000000 ) ) ;
#22820 = CARTESIAN_POINT ( 'NONE',  ( 67.66709685856477563, -3.055000000000000160, -5.291415217122921177 ) ) ;
#22821 = CARTESIAN_POINT ( 'NONE',  ( -63.18398860626900415, 28.73617430169831621, 5.000000000000000000 ) ) ;
#22823 = ORIENTED_EDGE ( 'NONE', *, *, #84128, .T. ) ;
#22822 = AXIS2_PLACEMENT_3D ( 'NONE', #57443, #37085, #2279 ) ;
#22824 = AXIS2_PLACEMENT_3D ( 'NONE', #60338, #36424, #105927 ) ;
#22825 = DIRECTION ( 'NONE',  ( 0.3543493200069162685, -0.000000000000000000, -0.9351131265310288487 ) ) ;
#22826 = VECTOR ( 'NONE', #49057, 1000.000000000000000 ) ;
#22827 = CARTESIAN_POINT ( 'NONE',  ( 31.82816939922330235, -14.24070752338414714, 4.000000000000000000 ) ) ;
#22828 = CARTESIAN_POINT ( 'NONE',  ( 38.99451991528749062, 28.92564299267965211, 4.000000000000000000 ) ) ;
#22829 = CONICAL_SURFACE ( 'NONE', #103862, 2.055000000000001048, 0.9599310885968758145 ) ;
#22830 = DIRECTION ( 'NONE',  ( -0.000000000000000000, -0.3543493200069152693, 0.9351131265310292928 ) ) ;
#22831 = DIRECTION ( 'NONE',  ( -0.7071067811865487940, 0.7071067811865463515, -0.000000000000000000 ) ) ;
#22833 = ORIENTED_EDGE ( 'NONE', *, *, #803, .T. ) ;
#22832 = CYLINDRICAL_SURFACE ( 'NONE', #116982, 2.500000000000000000 ) ;
#22834 = LINE ( 'NONE', #90260, #53056 ) ;
#22835 = LINE ( 'NONE', #43927, #112467 ) ;
#22836 = CARTESIAN_POINT ( 'NONE',  ( 17.39159235450332019, 3.061616997868380183E-16, -2.500000000000001332 ) ) ;
#22837 = AXIS2_PLACEMENT_3D ( 'NONE', #20309, #141395, #34087 ) ;
#22838 = DIRECTION ( 'NONE',  ( 1.000000000000000000, -0.000000000000000000, 0.000000000000000000 ) ) ;
#22839 = AXIS2_PLACEMENT_3D ( 'NONE', #5783, #50049, #98529 ) ;
#22840 = ORIENTED_EDGE ( 'NONE', *, *, #41276, .T. ) ;
#22841 = VERTEX_POINT ( 'NONE', #99138 ) ;
#22842 = CARTESIAN_POINT ( 'NONE',  ( 63.58376352523143993, -6.110000000000001208, -3.741295971395164515E-16 ) ) ;
#22843 = ADVANCED_FACE ( 'NONE', ( #142679 ), #21615, .F. ) ;
#22844 = VERTEX_POINT ( 'NONE', #33930 ) ;
#22845 = LINE ( 'NONE', #35935, #86979 ) ;
#22846 = ADVANCED_FACE ( 'NONE', ( #43371 ), #131090, .F. ) ;
#22847 = CARTESIAN_POINT ( 'NONE',  ( 2.510786437626908008, -27.52281430457053446, 5.000000000000000000 ) ) ;
#22848 = CARTESIAN_POINT ( 'NONE',  ( -8.816011393731004731, 28.73617430169781173, 5.000000000000000000 ) ) ;
#22849 = DIRECTION ( 'NONE',  ( -0.7071067811865486830, -0.7071067811865464625, 0.000000000000000000 ) ) ;
#22850 = CARTESIAN_POINT ( 'NONE',  ( -1.499999999999994449, -10.91253812416063873, 4.000000000000000000 ) ) ;
#22851 = VERTEX_POINT ( 'NONE', #110029 ) ;
#22852 = ORIENTED_EDGE ( 'NONE', *, *, #136880, .T. ) ;
#22853 = VECTOR ( 'NONE', #24928, 1000.000000000000227 ) ;
#22854 = DIRECTION ( 'NONE',  ( 0.000000000000000000, 1.000000000000000000, -0.000000000000000000 ) ) ;
#22855 = CARTESIAN_POINT ( 'NONE',  ( -17.54957349083946383, -3.269999989306286547, -35.77884719040818595 ) ) ;
#22856 = EDGE_CURVE ( 'NONE', #114476, #15110, #31777, .T. ) ;
#22857 = EDGE_CURVE ( 'NONE', #123401, #39039, #121617, .T. ) ;
#22858 = ORIENTED_EDGE ( 'NONE', *, *, #76935, .T. ) ;
#22859 = CARTESIAN_POINT ( 'NONE',  ( -27.29974487139158512, -27.71228299555225405, 4.000000000000000000 ) ) ;
#22860 = DIRECTION ( 'NONE',  ( 0.7071067811865487940, 0.7071067811865463515, 0.000000000000000000 ) ) ;
#22861 = CARTESIAN_POINT ( 'NONE',  ( -24.29974487139158867, -27.71228299555223273, 4.000000000000000000 ) ) ;
#22862 = ORIENTED_EDGE ( 'NONE', *, *, #64578, .T. ) ;
#22863 = ADVANCED_FACE ( 'NONE', ( #10013 ), #88311, .T. ) ;
#22864 = FACE_BOUND ( 'NONE', #18066, .T. ) ;
#22865 = ADVANCED_FACE ( 'NONE', ( #110723 ), #89034, .T. ) ;
#22866 = DIRECTION ( 'NONE',  ( -1.000000000000000000, 0.000000000000000000, 0.000000000000000000 ) ) ;
#22867 = CARTESIAN_POINT ( 'NONE',  ( 54.48921356237310221, -27.52281430457093236, 5.000000000000000000 ) ) ;
#22868 = CARTESIAN_POINT ( 'NONE',  ( -12.18398860626900060, 28.73617430169795739, 5.000000000000000000 ) ) ;
#22869 = DIRECTION ( 'NONE',  ( -0.7071067811865487940, 0.7071067811865463515, 0.000000000000000000 ) ) ;
#22870 = CARTESIAN_POINT ( 'NONE',  ( -39.48921356237310221, -27.52281430457082934, 5.000000000000000000 ) ) ;
#22871 = ORIENTED_EDGE ( 'NONE', *, *, #100271, .F. ) ;
#22872 = VERTEX_POINT ( 'NONE', #54971 ) ;
#22873 = CARTESIAN_POINT ( 'NONE',  ( 103.4537635252314516, -6.109999999999998543, -3.741295971395162543E-16 ) ) ;
#22874 = ORIENTED_EDGE ( 'NONE', *, *, #10903, .F. ) ;
#22875 = EDGE_CURVE ( 'NONE', #47092, #142281, #54277, .T. ) ;
#22876 = VERTEX_POINT ( 'NONE', #41948 ) ;
#22877 = DIRECTION ( 'NONE',  ( -0.6830127018922181881, 0.6830127018922202975, -0.2588190451025214056 ) ) ;
#22878 = EDGE_CURVE ( 'NONE', #28630, #32044, #107870, .T. ) ;
#22879 = CARTESIAN_POINT ( 'NONE',  ( 3.691639616203772789, 6.094999999999988205, -1.633150327867694651 ) ) ;
#22880 = CARTESIAN_POINT ( 'NONE',  ( 36.48921356237310221, -27.52281430457080802, 5.000000000000000000 ) ) ;
#22881 = VERTEX_POINT ( 'NONE', #44091 ) ;
#22882 = DIRECTION ( 'NONE',  ( -1.000000000000000000, -1.224606353822377258E-16, -0.000000000000000000 ) ) ;
#22883 = CARTESIAN_POINT ( 'NONE',  ( -1.256362331258242971E-13, -34.64999999999997726, 17.49210858042621908 ) ) ;
#22884 = VECTOR ( 'NONE', #42801, 1000.000000000000114 ) ;
#22885 = CARTESIAN_POINT ( 'NONE',  ( 8.999999999999936051, 4.931123077392133069, 4.000000000000000000 ) ) ;
#22886 = PRESENTATION_STYLE_ASSIGNMENT (( #102648 ) ) ;
#22888 = LINE ( 'NONE', #1148, #122226 ) ;
#22887 = DIRECTION ( 'NONE',  ( -0.3543493200069162685, -0.000000000000000000, -0.9351131265310288487 ) ) ;
#22889 = LINE ( 'NONE', #89607, #113262 ) ;
#22890 = EDGE_CURVE ( 'NONE', #97358, #50924, #9494, .T. ) ;
#22891 = VECTOR ( 'NONE', #104014, 999.9999999999998863 ) ;
#22892 = VECTOR ( 'NONE', #108345, 1000.000000000000000 ) ;
#22893 = CARTESIAN_POINT ( 'NONE',  ( -23.99999999999982947, -0.1606350220013114671, 4.664761815935120737 ) ) ;
#22894 = AXIS2_PLACEMENT_3D ( 'NONE', #99715, #34473, #142534 ) ;
#22895 = ORIENTED_EDGE ( 'NONE', *, *, #135225, .F. ) ;
#22896 = LINE ( 'NONE', #101198, #88967 ) ;
#22897 = CARTESIAN_POINT ( 'NONE',  ( 6.183988606268994381, 28.73617430169791476, 5.000000000000000000 ) ) ;
#22898 = AXIS2_PLACEMENT_3D ( 'NONE', #68082, #21675, #89089 ) ;
#22899 = EDGE_LOOP ( 'NONE', ( #80732, #129564, #133346, #101136 ) ) ;
#22900 = VERTEX_POINT ( 'NONE', #86163 ) ;
#22901 = ORIENTED_EDGE ( 'NONE', *, *, #55192, .F. ) ;
#22902 = CARTESIAN_POINT ( 'NONE',  ( 51.77126352523143993, 4.472830434245838482, 4.472830434245842035 ) ) ;
#22903 = ORIENTED_EDGE ( 'NONE', *, *, #89062, .T. ) ;
#22904 = VECTOR ( 'NONE', #103738, 1000.000000000000000 ) ;
#22905 = DIRECTION ( 'NONE',  ( 0.000000000000000000, 0.000000000000000000, 1.000000000000000000 ) ) ;
#22906 = EDGE_CURVE ( 'NONE', #52143, #46122, #33246, .T. ) ;
#22907 = CARTESIAN_POINT ( 'NONE',  ( 7.191639616203771013, 6.094999999999988205, -1.633150327867694651 ) ) ;
#22908 = CARTESIAN_POINT ( 'NONE',  ( 92.75043019189810423, 3.055000000000002824, -5.291415217122919401 ) ) ;
#22909 = DIRECTION ( 'NONE',  ( 0.3543493200069164351, 2.781805975412904658E-17, -0.9351131265310288487 ) ) ;
#22910 = ORIENTED_EDGE ( 'NONE', *, *, #57976, .T. ) ;
#22911 = CARTESIAN_POINT ( 'NONE',  ( -16.49999999999988276, 12.05218569542904206, 5.000000000000000000 ) ) ;
#22912 = VECTOR ( 'NONE', #21021, 1000.000000000000000 ) ;
#22913 = CARTESIAN_POINT ( 'NONE',  ( 0.000000000000000000, 0.000000000000000000, 5.000000000000000000 ) ) ;
#22914 = ORIENTED_EDGE ( 'NONE', *, *, #136476, .T. ) ;
#22915 = DIRECTION ( 'NONE',  ( -1.000000000000000000, 0.000000000000000000, 0.000000000000000000 ) ) ;
#22916 = DIRECTION ( 'NONE',  ( -0.3543493200069162685, -0.000000000000000000, -0.9351131265310288487 ) ) ;
#22917 = ORIENTED_EDGE ( 'NONE', *, *, #126818, .T. ) ;
#22918 = AXIS2_PLACEMENT_3D ( 'NONE', #65509, #19104, #108942 ) ;
#22919 = CARTESIAN_POINT ( 'NONE',  ( -8.999999999999937828, 4.384688058510551656, -7.090945410444704500 ) ) ;
#22920 = LINE ( 'NONE', #25992, #66050 ) ;
#22921 = VERTEX_POINT ( 'NONE', #130386 ) ;
#22922 = EDGE_LOOP ( 'NONE', ( #8284, #246, #33105, #38369 ) ) ;
#22923 = ORIENTED_EDGE ( 'NONE', *, *, #109533, .T. ) ;
#22924 = CARTESIAN_POINT ( 'NONE',  ( 122.7037635252314516, 6.109999999999998543, 1.122388791418548911E-15 ) ) ;
#22925 = CIRCLE ( 'NONE', #76269, 2.999999999999999556 ) ;
#22926 = AXIS2_PLACEMENT_3D ( 'NONE', #46041, #57630, #3204 ) ;
#22927 = LINE ( 'NONE', #54900, #5229 ) ;
#22928 = VECTOR ( 'NONE', #88259, 1000.000000000000114 ) ;
#22929 = CARTESIAN_POINT ( 'NONE',  ( 18.00548008471250583, 28.92564299267925776, 4.000000000000000000 ) ) ;
#22930 = CARTESIAN_POINT ( 'NONE',  ( 0.000000000000000000, 0.000000000000000000, 5.000000000000000000 ) ) ;
#22931 = VERTEX_POINT ( 'NONE', #63710 ) ;
#22932 = AXIS2_PLACEMENT_3D ( 'NONE', #28024, #128069, #84562 ) ;
#22933 = AXIS2_PLACEMENT_3D ( 'NONE', #4708, #62034, #27222 ) ;
#22934 = CARTESIAN_POINT ( 'NONE',  ( 9.312069808101886892, 7.934999999999993392, 2.126176841940951689 ) ) ;
#22935 = CARTESIAN_POINT ( 'NONE',  ( 0.000000000000000000, 0.000000000000000000, 8.094999999999991758 ) ) ;
#22936 = CARTESIAN_POINT ( 'NONE',  ( -34.92500000000001137, 9.691175483027018700, 9.749534648445560947 ) ) ;
#22937 = PLANE ( 'NONE',  #23527 ) ;
#22938 = EDGE_LOOP ( 'NONE', ( #93958, #2219, #9308, #81247 ) ) ;
#22939 = VERTEX_POINT ( 'NONE', #31079 ) ;
#22940 = EDGE_CURVE ( 'NONE', #96370, #115757, #75297, .T. ) ;
#22941 = ORIENTED_EDGE ( 'NONE', *, *, #30942, .F. ) ;
#22942 = PRESENTATION_STYLE_ASSIGNMENT (( #109983 ) ) ;
#22943 = UNCERTAINTY_MEASURE_WITH_UNIT (LENGTH_MEASURE( 1.000000000000000082E-05 ), #114451, 'distance_accuracy_value', 'NONE');
#22944 = MECHANICAL_DESIGN_GEOMETRIC_PRESENTATION_REPRESENTATION (  '', ( #76294 ), #36844 ) ;
#22945 = CARTESIAN_POINT ( 'NONE',  ( 3.183988606268992161, 28.73617430169789699, 5.000000000000000000 ) ) ;
#22946 = PLANE ( 'NONE',  #36688 ) ;
#22947 = CARTESIAN_POINT ( 'NONE',  ( 6.179508952642605912, 9.395989132568409730, 1.427142123928949013 ) ) ;
#22948 = DIRECTION ( 'NONE',  ( 0.000000000000000000, -1.000000000000000000, 0.000000000000000000 ) ) ;
#22949 = LINE ( 'NONE', #100566, #131307 ) ;
#22950 = CARTESIAN_POINT ( 'NONE',  ( 24.32816939922336630, -6.740707523384209310, 4.000000000000000000 ) ) ;
#22952 = ADVANCED_FACE ( 'NONE', ( #102030 ), #23759, .F. ) ;
#22951 = CARTESIAN_POINT ( 'NONE',  ( 8.994519915287490619, 28.92564299267944250, 4.000000000000000000 ) ) ;
#22953 = ORIENTED_EDGE ( 'NONE', *, *, #86387, .T. ) ;
#22954 = LINE ( 'NONE', #33887, #108909 ) ;
#22955 = ORIENTED_EDGE ( 'NONE', *, *, #79193, .F. ) ;
#22956 = B_SPLINE_CURVE_WITH_KNOTS ( 'NONE', 3,
 ( #133668, #13278, #45961, #101016 ),
 .UNSPECIFIED., .F., .F.,
 ( 4, 4 ),
 ( 0.003609336753060590763, 0.003809496093231039965 ),
 .UNSPECIFIED. ) ;
#22957 = CARTESIAN_POINT ( 'NONE',  ( 19.80437226529636163, -2.191939191560713152, -32.94353395994160394 ) ) ;
#22958 = ORIENTED_EDGE ( 'NONE', *, *, #52486, .F. ) ;
#22959 = CARTESIAN_POINT ( 'NONE',  ( -14.99999999999989519, -6.033600742197674727, 5.000000000000000000 ) ) ;
#22961 = VERTEX_POINT ( 'NONE', #124490 ) ;
#22960 = LINE ( 'NONE', #67230, #97407 ) ;
#22962 = EDGE_CURVE ( 'NONE', #127065, #104418, #31350, .T. ) ;
#22963 = DIRECTION ( 'NONE',  ( -0.7071067811865486830, -0.7071067811865464625, 0.000000000000000000 ) ) ;
#22964 = DIRECTION ( 'NONE',  ( -0.7071067811865486830, -0.7071067811865464625, 0.000000000000000000 ) ) ;
#22965 = ORIENTED_EDGE ( 'NONE', *, *, #134660, .T. ) ;
#22966 = EDGE_CURVE ( 'NONE', #19025, #20435, #125229, .T. ) ;
#22967 = CARTESIAN_POINT ( 'NONE',  ( 27.99999999999996803, -49.14999999999999147, 45.92499999999999005 ) ) ;
#22968 = VERTEX_POINT ( 'NONE', #69418 ) ;
#22969 = LINE ( 'NONE', #67236, #123222 ) ;
#22970 = VERTEX_POINT ( 'NONE', #37502 ) ;
#22971 = EDGE_CURVE ( 'NONE', #68934, #55692, #127640, .T. ) ;
#22972 = CARTESIAN_POINT ( 'NONE',  ( -38.99451991528749062, 28.92564299267965211, 4.000000000000000000 ) ) ;
#22973 = CARTESIAN_POINT ( 'NONE',  ( 116.3083603837962130, 7.949999999999997513, 2.130196079827431088 ) ) ;
#22974 = CARTESIAN_POINT ( 'NONE',  ( -14.99451991528749595, 28.92564299267948513, 4.000000000000000000 ) ) ;
#22975 = EDGE_CURVE ( 'NONE', #46898, #88378, #112896, .T. ) ;
#22976 = CARTESIAN_POINT ( 'NONE',  ( 156.1499999999997783, -49.14999999999999147, -34.92499999999975557 ) ) ;
#22977 = DIRECTION ( 'NONE',  ( 1.000000000000000000, 0.000000000000000000, 0.000000000000000000 ) ) ;
#22978 = CARTESIAN_POINT ( 'NONE',  ( 7.637717201596474048, 4.584330080086930965E-16, 0.000000000000000000 ) ) ;
#22979 = CARTESIAN_POINT ( 'NONE',  ( 16.04166666666666785, 3.047499999999993214, -5.278424836066146320 ) ) ;
#22980 = FACE_OUTER_BOUND ( 'NONE', #137132, .T. ) ;
#22981 = DIRECTION ( 'NONE',  ( 0.6830127018922180770, -0.6830127018922204085, -0.2588190451025213501 ) ) ;
#22982 = PLANE ( 'NONE',  #71007 ) ;
#22983 = ORIENTED_EDGE ( 'NONE', *, *, #19739, .T. ) ;
#22984 = ORIENTED_EDGE ( 'NONE', *, *, #64749, .F. ) ;
#22985 = EDGE_CURVE ( 'NONE', #110525, #108329, #135398, .T. ) ;
#22986 = CARTESIAN_POINT ( 'NONE',  ( -34.92500000000001137, 0.006123077391933379188, 4.000000000000000000 ) ) ;
#22987 = ORIENTED_EDGE ( 'NONE', *, *, #59123, .F. ) ;
#22988 = CARTESIAN_POINT ( 'NONE',  ( 95.81293019189807580, -1.637169565754159617, -6.110000000000001208 ) ) ;
#22989 = FACE_OUTER_BOUND ( 'NONE', #108834, .T. ) ;
#22990 = DIRECTION ( 'NONE',  ( 0.3543493200069162685, -0.000000000000000000, -0.9351131265310288487 ) ) ;
#22991 = CARTESIAN_POINT ( 'NONE',  ( 7.326124847093153925, 4.202752102959690472E-16, 0.000000000000000000 ) ) ;
#22992 = LINE ( 'NONE', #79617, #80321 ) ;
#22993 = VERTEX_POINT ( 'NONE', #57839 ) ;
#22995 = EDGE_CURVE ( 'NONE', #20866, #27961, #103428, .T. ) ;
#22994 = VECTOR ( 'NONE', #3144, 1000.000000000000000 ) ;
#22996 = VECTOR ( 'NONE', #13949, 999.9999999999998863 ) ;
#22997 = CARTESIAN_POINT ( 'NONE',  ( -34.92500000000001137, 2.816654386410402555, 4.500000000000000888 ) ) ;
#22998 = CARTESIAN_POINT ( 'NONE',  ( -34.49999999999975842, -13.53574439159936915, 4.994342998332166772 ) ) ;
#22999 = VECTOR ( 'NONE', #125827, 1000.000000000000000 ) ;
#23000 = FACE_OUTER_BOUND ( 'NONE', #124336, .T. ) ;
#23001 = CARTESIAN_POINT ( 'NONE',  ( -48.48921356237309510, -27.52281430457089328, 5.000000000000000000 ) ) ;
#23002 = SURFACE_STYLE_FILL_AREA ( #11410 ) ;
#23004 = ORIENTED_EDGE ( 'NONE', *, *, #73933, .F. ) ;
#23003 = LINE ( 'NONE', #10704, #28933 ) ;
#23005 = LINE ( 'NONE', #67278, #81662 ) ;
#23006 = EDGE_CURVE ( 'NONE', #22717, #41095, #81004, .T. ) ;
#23007 = LINE ( 'NONE', #58592, #1192 ) ;
#23008 = DIRECTION ( 'NONE',  ( 0.000000000000000000, 0.000000000000000000, 1.000000000000000000 ) ) ;
#23009 = EDGE_CURVE ( 'NONE', #67807, #88720, #113602, .T. ) ;
#23010 = CARTESIAN_POINT ( 'NONE',  ( 24.79289321881329045, -2.240707523384254163, 5.000000000000000000 ) ) ;
#23011 = AXIS2_PLACEMENT_3D ( 'NONE', #49250, #116614, #73136 ) ;
#23012 = CARTESIAN_POINT ( 'NONE',  ( -50.99451991528749062, 28.92564299267973738, 4.000000000000000000 ) ) ;
#23013 = ORIENTED_EDGE ( 'NONE', *, *, #108616, .F. ) ;
#23014 = ORIENTED_EDGE ( 'NONE', *, *, #91771, .F. ) ;
#23015 = ORIENTED_EDGE ( 'NONE', *, *, #73615, .T. ) ;
#23016 = CARTESIAN_POINT ( 'NONE',  ( 89.39626352523144703, 4.472830434245840259, -4.472830434245839371 ) ) ;
#23017 = AXIS2_PLACEMENT_3D ( 'NONE', #39402, #17606, #140143 ) ;
#23018 = ORIENTED_EDGE ( 'NONE', *, *, #36879, .F. ) ;
#23019 = DIRECTION ( 'NONE',  ( -0.6830127018922180770, -0.6830127018922204085, -0.2588190451025213501 ) ) ;
#23020 = EDGE_CURVE ( 'NONE', #54370, #81280, #101309, .T. ) ;
#23021 = DIRECTION ( 'NONE',  ( 0.000000000000000000, 0.000000000000000000, 1.000000000000000000 ) ) ;
#23022 = LINE ( 'NONE', #67294, #41071 ) ;
#23023 = CARTESIAN_POINT ( 'NONE',  ( 84.80836038379621300, 7.949999999999996625, 2.130196079827431088 ) ) ;
#23024 = VERTEX_POINT ( 'NONE', #1946 ) ;
#23025 = DIRECTION ( 'NONE',  ( 0.7071067811865486830, -0.7071067811865464625, -0.000000000000000000 ) ) ;
#23026 = PLANE ( 'NONE',  #21159 ) ;
#23027 = EDGE_CURVE ( 'NONE', #62199, #127411, #142465, .T. ) ;
#23028 = EDGE_CURVE ( 'NONE', #107481, #16142, #125209, .T. ) ;
#23029 = LINE ( 'NONE', #45571, #39511 ) ;
#23030 = VECTOR ( 'NONE', #73014, 1000.000000000000000 ) ;
#23031 = CARTESIAN_POINT ( 'NONE',  ( 87.84959685856476597, 6.109999999999996767, 1.637169565754163836 ) ) ;
#23032 = ORIENTED_EDGE ( 'NONE', *, *, #45579, .T. ) ;
#23033 = DIRECTION ( 'NONE',  ( 1.000000000000000000, -0.000000000000000000, -0.000000000000000000 ) ) ;
#23034 = CYLINDRICAL_SURFACE ( 'NONE', #118910, 2.500000000000000000 ) ;
#23035 = VECTOR ( 'NONE', #16831, 1000.000000000000227 ) ;
#23037 = ADVANCED_FACE ( 'NONE', ( #134684 ), #111468, .F. ) ;
#23036 = AXIS2_PLACEMENT_3D ( 'NONE', #89345, #142321, #132159 ) ;
#23038 = VECTOR ( 'NONE', #87017, 1000.000000000000000 ) ;
#23039 = VERTEX_POINT ( 'NONE', #106269 ) ;
#23040 = ORIENTED_EDGE ( 'NONE', *, *, #16286, .T. ) ;
#23041 = CARTESIAN_POINT ( 'NONE',  ( 6.489213562373093325, -27.52281430457059841, 5.000000000000000000 ) ) ;
#23042 = EDGE_CURVE ( 'NONE', #56720, #108519, #125932, .T. ) ;
#23043 =( NAMED_UNIT ( * ) SI_UNIT ( $, .STERADIAN. ) SOLID_ANGLE_UNIT ( ) );
#23044 = DIRECTION ( 'NONE',  ( -0.000000000000000000, 0.000000000000000000, 1.000000000000000000 ) ) ;
#23045 = VECTOR ( 'NONE', #35750, 1000.000000000000114 ) ;
#23046 = CARTESIAN_POINT ( 'NONE',  ( 3.225639847634963697, -48.88932940808382455, -39.16623080367948972 ) ) ;
#23047 = CARTESIAN_POINT ( 'NONE',  ( 0.000000000000000000, 0.000000000000000000, 5.000000000000000000 ) ) ;
#23048 = CARTESIAN_POINT ( 'NONE',  ( -25.39999999999996305, 0.000000000000000000, 2.500000000000000000 ) ) ;
#23049 = ORIENTED_EDGE ( 'NONE', *, *, #12363, .T. ) ;
#23050 = EDGE_LOOP ( 'NONE', ( #90265, #143149, #23952, #10437 ) ) ;
#23051 = EDGE_CURVE ( 'NONE', #94326, #62352, #104877, .T. ) ;
#23052 = CARTESIAN_POINT ( 'NONE',  ( 10.77958563595370833, 3.061616997868383634E-16, -2.500000000000000444 ) ) ;
#23053 = ORIENTED_EDGE ( 'NONE', *, *, #63175, .F. ) ;
#23054 = ORIENTED_EDGE ( 'NONE', *, *, #94600, .T. ) ;
#23055 = EDGE_CURVE ( 'NONE', #75784, #20082, #104404, .T. ) ;
#23056 = PLANE ( 'NONE',  #137746 ) ;
#23057 = ORIENTED_EDGE ( 'NONE', *, *, #90365, .T. ) ;
#23058 = DIRECTION ( 'NONE',  ( -0.7071067811865486830, -0.7071067811865464625, 0.000000000000000000 ) ) ;
#23059 = DIRECTION ( 'NONE',  ( 0.000000000000000000, 1.000000000000000000, 0.000000000000000000 ) ) ;
#23060 = CARTESIAN_POINT ( 'NONE',  ( 12.18398860626900060, 28.73617430169795739, 5.000000000000000000 ) ) ;
#23061 = DIRECTION ( 'NONE',  ( -0.6830127018922181881, 0.6830127018922202975, -0.2588190451025214056 ) ) ;
#23062 = DIRECTION ( 'NONE',  ( 0.000000000000000000, -1.091707662666338270E-16, 1.000000000000000000 ) ) ;
#23063 = VERTEX_POINT ( 'NONE', #116473 ) ;
#23064 = FILL_AREA_STYLE_COLOUR ( '', #74259 ) ;
#23065 = ORIENTED_EDGE ( 'NONE', *, *, #25019, .T. ) ;
#23066 = CARTESIAN_POINT ( 'NONE',  ( 26.40000000000000568, -17.48000000000005016, 34.92499999999998295 ) ) ;
#23067 = VERTEX_POINT ( 'NONE', #51231 ) ;
#23068 = CARTESIAN_POINT ( 'NONE',  ( 115.2875270504628986, 0.000000000000000000, -7.949999999999998401 ) ) ;
#23069 = VERTEX_POINT ( 'NONE', #137520 ) ;
#23070 = CARTESIAN_POINT ( 'NONE',  ( -45.29974487139158867, -27.71228299555237840, 4.000000000000000000 ) ) ;
#23071 = ORIENTED_EDGE ( 'NONE', *, *, #98556, .T. ) ;
#23072 = EDGE_LOOP ( 'NONE', ( #96524, #110093, #87214, #94847 ) ) ;
#23073 = ORIENTED_EDGE ( 'NONE', *, *, #136641, .F. ) ;
#23074 = ADVANCED_FACE ( 'NONE', ( #7690 ), #40369, .F. ) ;
#23075 = LINE ( 'NONE', #131883, #55895 ) ;
#23076 = CARTESIAN_POINT ( 'NONE',  ( -35.99451991528749772, 28.92564299267963079, 4.000000000000000000 ) ) ;
#23077 = LINE ( 'NONE', #102834, #88908 ) ;
#23078 = CARTESIAN_POINT ( 'NONE',  ( 121.6254301918981184, 5.291415217122919401, 3.055000000000002824 ) ) ;
#23079 = FACE_OUTER_BOUND ( 'NONE', #59637, .T. ) ;
#23080 = PLANE ( 'NONE',  #41292 ) ;
#23081 = LINE ( 'NONE', #65228, #11136 ) ;
#23082 = DIRECTION ( 'NONE',  ( 1.000000000000000000, 0.000000000000000000, 0.000000000000000000 ) ) ;
#23083 = DIRECTION ( 'NONE',  ( 0.6830127018922181881, 0.6830127018922202975, -0.2588190451025214056 ) ) ;
#23084 = ORIENTED_EDGE ( 'NONE', *, *, #23343, .F. ) ;
#23085 = CARTESIAN_POINT ( 'NONE',  ( 25.49999999999982947, -16.91253812416058011, 4.000000000000000000 ) ) ;
#23086 = LINE ( 'NONE', #48449, #119378 ) ;
#23087 = CARTESIAN_POINT ( 'NONE',  ( -11.99999999999990585, -12.41253812416062985, 4.000000000000000000 ) ) ;
#23088 = VERTEX_POINT ( 'NONE', #70850 ) ;
#23089 = ORIENTED_EDGE ( 'NONE', *, *, #79689, .F. ) ;
#23090 = ORIENTED_EDGE ( 'NONE', *, *, #141689, .F. ) ;
#23091 = CARTESIAN_POINT ( 'NONE',  ( 2.999999999999975131, -10.77435723561695191, -9.972017380717238311 ) ) ;
#23092 = VECTOR ( 'NONE', #102324, 999.9999999999998863 ) ;
#23093 = AXIS2_PLACEMENT_3D ( 'NONE', #13496, #124426, #79554 ) ;
#23094 = ORIENTED_EDGE ( 'NONE', *, *, #76790, .T. ) ;
#23095 = AXIS2_PLACEMENT_3D ( 'NONE', #27592, #116024, #72599 ) ;
#23097 = ORIENTED_EDGE ( 'NONE', *, *, #67451, .F. ) ;
#23096 = VECTOR ( 'NONE', #140953, 1000.000000000000000 ) ;
#23098 = CARTESIAN_POINT ( 'NONE',  ( 20.99999999999986144, 11.58746187583912324, 4.000000000000000000 ) ) ;
#23099 = DIRECTION ( 'NONE',  ( -0.7071067811865487940, 0.7071067811865463515, 0.000000000000000000 ) ) ;
#23100 = PLANE ( 'NONE',  #88942 ) ;
#23101 = PLANE ( 'NONE',  #20939 ) ;
#23102 = ORIENTED_EDGE ( 'NONE', *, *, #130098, .F. ) ;
#23103 = DIRECTION ( 'NONE',  ( 1.000000000000000000, 0.000000000000000000, 0.000000000000000000 ) ) ;
#23105 = ORIENTED_EDGE ( 'NONE', *, *, #51218, .T. ) ;
#23104 = VECTOR ( 'NONE', #42493, 1000.000000000000227 ) ;
#23106 = LINE ( 'NONE', #80407, #531 ) ;
#23107 = CARTESIAN_POINT ( 'NONE',  ( 18.73373647476854842, 5.808823158059036373, 5.808823158059032821 ) ) ;
#23108 = ORIENTED_EDGE ( 'NONE', *, *, #84922, .F. ) ;
#23109 = CARTESIAN_POINT ( 'NONE',  ( 85.37043019189812298, -3.055000000000001936, 5.291415217122918513 ) ) ;
#23110 = CARTESIAN_POINT ( 'NONE',  ( -34.49999999999975131, -17.56887692260763956, 4.000000000000000000 ) ) ;
#23111 = CARTESIAN_POINT ( 'NONE',  ( 97.93336038379622721, 2.130196079827431532, -7.949999999999996625 ) ) ;
#23112 = ORIENTED_EDGE ( 'NONE', *, *, #62804, .F. ) ;
#23113 = VERTEX_POINT ( 'NONE', #51944 ) ;
#23114 = ORIENTED_EDGE ( 'NONE', *, *, #369, .F. ) ;
#23116 = AXIS2_PLACEMENT_3D ( 'NONE', #23357, #36397, #25497 ) ;
#23115 = DIRECTION ( 'NONE',  ( 0.7071067811865487940, -0.7071067811865463515, 0.000000000000000000 ) ) ;
#23117 = DIRECTION ( 'NONE',  ( -0.7071067811865486830, -0.7071067811865464625, 0.000000000000000000 ) ) ;
#23118 = CARTESIAN_POINT ( 'NONE',  ( 0.000000000000000000, 0.000000000000000000, 5.000000000000000000 ) ) ;
#23119 = CARTESIAN_POINT ( 'NONE',  ( 14.99451991528749595, 28.92564299267948513, 4.000000000000000000 ) ) ;
#23120 = FACE_OUTER_BOUND ( 'NONE', #110235, .T. ) ;
#23121 = VERTEX_POINT ( 'NONE', #93990 ) ;
#23122 = CARTESIAN_POINT ( 'NONE',  ( 25.39999999999999858, -18.48000000000005372, 33.92499999999998295 ) ) ;
#23123 = AXIS2_PLACEMENT_3D ( 'NONE', #56804, #78517, #135754 ) ;
#23124 = EDGE_CURVE ( 'NONE', #83273, #26933, #117162, .T. ) ;
#23125 = CARTESIAN_POINT ( 'NONE',  ( -0.005480084712502889671, 28.92564299267938210, 4.000000000000000000 ) ) ;
#23127 = EDGE_CURVE ( 'NONE', #86507, #88273, #27299, .T. ) ;
#23126 = DIRECTION ( 'NONE',  ( 0.6830127018922180770, -0.6830127018922204085, -0.2588190451025213501 ) ) ;
#23128 = EDGE_CURVE ( 'NONE', #85852, #137066, #138225, .T. ) ;
#23129 = VERTEX_POINT ( 'NONE', #17162 ) ;
#23130 = DIRECTION ( 'NONE',  ( 0.7071067811865487940, 0.7071067811865463515, 0.000000000000000000 ) ) ;
#23132 = VECTOR ( 'NONE', #41380, 1000.000000000000000 ) ;
#23131 = DIRECTION ( 'NONE',  ( -0.6830127018922180770, -0.6830127018922204085, -0.2588190451025213501 ) ) ;
#23133 = ORIENTED_EDGE ( 'NONE', *, *, #133855, .F. ) ;
#23134 = ADVANCED_FACE ( 'NONE', ( #18547 ), #28041, .T. ) ;
#23136 = VERTEX_POINT ( 'NONE', #41051 ) ;
#23135 = FACE_OUTER_BOUND ( 'NONE', #37640, .T. ) ;
#23137 = ORIENTED_EDGE ( 'NONE', *, *, #42389, .F. ) ;
#23138 = EDGE_CURVE ( 'NONE', #132741, #116545, #114999, .T. ) ;
#23139 = EDGE_CURVE ( 'NONE', #101337, #1886, #59965, .T. ) ;
#23140 = VECTOR ( 'NONE', #121635, 1000.000000000000000 ) ;
#23141 = CARTESIAN_POINT ( 'NONE',  ( -14.38161509397995630, -2.240707523384260824, 13.37739548510242749 ) ) ;
#23142 = VECTOR ( 'NONE', #55326, 1000.000000000000000 ) ;
#23143 = FACE_OUTER_BOUND ( 'NONE', #141221, .T. ) ;
#23144 = ORIENTED_EDGE ( 'NONE', *, *, #39848, .F. ) ;
#23145 = CARTESIAN_POINT ( 'NONE',  ( 66.48921356237309510, -27.52281430457101763, 5.000000000000000000 ) ) ;
#23146 = UNCERTAINTY_MEASURE_WITH_UNIT (LENGTH_MEASURE( 1.000000000000000082E-05 ), #105479, 'distance_accuracy_value', 'NONE');
#23147 = EDGE_CURVE ( 'NONE', #101509, #92497, #38913, .T. ) ;
#23148 = EDGE_CURVE ( 'NONE', #103780, #3304, #72306, .T. ) ;
#23149 = FACE_OUTER_BOUND ( 'NONE', #114739, .T. ) ;
#23150 = DIRECTION ( 'NONE',  ( 0.000000000000000000, 0.000000000000000000, 1.000000000000000000 ) ) ;
#23151 = DIRECTION ( 'NONE',  ( 1.000000000000000000, 0.000000000000000000, 0.000000000000000000 ) ) ;
#23152 = COLOUR_RGB ( '', 0.66274510, 0.83137255, 0.94901961) ;
#23153 = CARTESIAN_POINT ( 'NONE',  ( 2.816011393730999401, 28.73617430169785436, 5.000000000000000000 ) ) ;
#23154 = DIRECTION ( 'NONE',  ( 0.6830127018922180770, -0.6830127018922204085, -0.2588190451025213501 ) ) ;
#23155 = EDGE_CURVE ( 'NONE', #74550, #34938, #83135, .T. ) ;
#23156 = CARTESIAN_POINT ( 'NONE',  ( 17.81601139373099940, 28.73617430169775133, 5.000000000000000000 ) ) ;
#23157 = DIRECTION ( 'NONE',  ( 0.7071067811865486830, -0.7071067811865464625, -0.000000000000000000 ) ) ;
#23158 = PLANE ( 'NONE',  #27510 ) ;
#23160 = VECTOR ( 'NONE', #53896, 1000.000000000000000 ) ;
#23159 = CARTESIAN_POINT ( 'NONE',  ( 24.18706980810188867, -2.126176841940956130, 7.934999999999991616 ) ) ;
#23161 = CARTESIAN_POINT ( 'NONE',  ( 2.603736474768552966, 5.808823158059035485, 5.808823158059032821 ) ) ;
#23162 = CARTESIAN_POINT ( 'NONE',  ( -19.05000000000000071, 3.174999999999997158, 0.000000000000000000 ) ) ;
#23163 = CARTESIAN_POINT ( 'NONE',  ( 110.2291666666666714, 7.950000000000001954, -2.130196079827421762 ) ) ;
#23164 = PLANE ( 'NONE',  #77825 ) ;
#23165 = VERTEX_POINT ( 'NONE', #28763 ) ;
#23166 = ORIENTED_EDGE ( 'NONE', *, *, #75569, .F. ) ;
#23168 = ADVANCED_FACE ( 'NONE', ( #61427 ), #39670, .T. ) ;
#23167 = CARTESIAN_POINT ( 'NONE',  ( 102.6458333333333144, 2.130196079827431976, -7.949999999999999289 ) ) ;
#23169 = EDGE_LOOP ( 'NONE', ( #77960, #58458, #75038, #82049 ) ) ;
#23170 = VERTEX_POINT ( 'NONE', #20711 ) ;
#23171 = ORIENTED_EDGE ( 'NONE', *, *, #63981, .F. ) ;
#23172 = CARTESIAN_POINT ( 'NONE',  ( 3.299744871391591339, -27.71228299555208352, 4.000000000000000000 ) ) ;
#23173 = DIRECTION ( 'NONE',  ( -0.7071067811865486830, 0.7071067811865464625, 0.000000000000000000 ) ) ;
#23174 = VECTOR ( 'NONE', #67745, 1000.000000000000000 ) ;
#23175 = CARTESIAN_POINT ( 'NONE',  ( 11.74866626111222878, 8.548044547423961248, 4.146786111629948479 ) ) ;
#23176 = VERTEX_POINT ( 'NONE', #54111 ) ;
#23177 = DIRECTION ( 'NONE',  ( 0.3543493200069162685, -0.000000000000000000, -0.9351131265310288487 ) ) ;
#23178 = LINE ( 'NONE', #80471, #76572 ) ;
#23179 = DIRECTION ( 'NONE',  ( 0.6830127018922180770, -0.6830127018922204085, -0.2588190451025213501 ) ) ;
#23180 = ORIENTED_EDGE ( 'NONE', *, *, #129461, .F. ) ;
#23181 = CARTESIAN_POINT ( 'NONE',  ( 127.5162635252314658, -4.472830434245838482, 4.472830434245838482 ) ) ;
#23182 = LINE ( 'NONE', #123272, #86698 ) ;
#23183 = CARTESIAN_POINT ( 'NONE',  ( 32.18753812416031224, -22.22500000000000142, 4.000000000000000000 ) ) ;
#23184 = EDGE_CURVE ( 'NONE', #68994, #129006, #131640, .T. ) ;
#23185 = DIRECTION ( 'NONE',  ( -0.7071067811865487940, 0.7071067811865463515, 0.000000000000000000 ) ) ;
#23186 = AXIS2_PLACEMENT_3D ( 'NONE', #38882, #59244, #106242 ) ;
#23187 = DIRECTION ( 'NONE',  ( 0.000000000000000000, 1.301042606982605074E-16, -1.000000000000000000 ) ) ;
#23188 = LINE ( 'NONE', #26086, #105517 ) ;
#23189 = CLOSED_SHELL ( 'NONE', ( #137798, #11692, #104368, #45731, #100110, #8352, #14703, #25783, #51710, #103740, #11894, #92745, #16823, #137321, #79630, #134169, #40307, #125559, #67396, #9068, #3197, #129681, #103579, #98799, #37983, #19569, #107477, #84254, #19901, #53463, #113555, #27937, #133919, #21845, #63546, #22024, #29646, #21954, #140473, #142697, #119004, #46534, #6057, #33935, #87011, #118981, #85619, #65659, #47955, #121513, #100649, #97828, #135757, #26954, #139418, #50673, #63932, #60469, #63042, #98236, #7337, #32686, #93114, #24209, #54145, #89178, #126437, #136590, #85296, #49188, #113335, #67253, #53506, #79120, #38240, #127478, #71703, #126664, #13841, #86902, #47980, #112944, #101907, #67390, #126988, #41661, #43653, #84133, #54431, #71218, #82724, #107695, #96883, #100043, #50891, #31601, #18662, #104134, #96064, #34683, #45477, #41188, #141355, #106102, #101431, #73909, #102651, #55180, #60721, #142224, #68439, #8866, #112362, #117843, #111602, #107454, #112826, #67884, #68156, #57544, #128145, #79090, #69774, #60906, #67202, #122774, #42543, #113197, #138443, #68728, #137325, #99743, #137026, #2629, #120918, #43461, #121057, #73641, #18126, #54665, #51331, #24583, #1325, #38417, #15239, #36998, #116105, #126268, #8918, #92076, #19006, #126348, #140556, #24359, #129391, #113413, #63511, #43668, #38809, #81807, #104288, #105630, #110083, #117766, #112876, #86064, #82611, #141582, #113101, #47822, #33290, #20135, #82138, #101917, #49174, #51328, #86887, #12527, #72720, #29715, #15769, #52512, #125203, #29272, #58968, #15578, #14202, #88301, #42028, #14463, #91201, #46152, #34128, #88822, #95151, #29557, #14698, #6395, #108026, #4303, #46173, #67125, #34139, #42594, #32227, #80525, #128249, #74586, #16570, #4484, #139672, #114582, #22561, #68029, #114826, #49063, #70211, #27065, #130048, #129873, #57166, #76602, #135346, #356, #117976, #26320, #129376, #72830, #34846, #36149, #7170, #123257, #68845, #130256, #88767, #80559, #77664, #61878, #98736, #38249, #129254, #104510, #12536, #46068, #26775, #69232, #39259, #10624, #129431, #30936, #90985, #113593, #62179, #74881, #86762, #49489, #106061, #76012, #93551, #100794, #26877, #135677, #101236, #80646, #65053, #37495, #100808, #60292, #44673, #2229, #4442, #24062, #3634, #27486, #135651, #17889, #82020, #29378, #114840, #78706, #119103, #63381, #62140, #95570, #105380, #138772, #67588, #77407, #38817, #123068, #73805, #93500, #98206, #70398, #104078, #134090, #38233, #4613, #55293, #99270, #44517, #93416, #106816, #124341, #34077, #57565, #63585, #109088, #38734, #109398, #2766, #139929, #109540, #128460, #39419, #56199, #124867, #3504, #31660, #75583, #18404, #104154, #133716, #27997, #134118, #110608, #7447, #68425, #132104, #109619, #58928, #32060, #73478, #87577, #69085, #130277, #43099, #129021, #33314, #112095, #80387, #67290, #95053, #4211, #103066, #75906, #6848, #64183, #125017, #10974, #58783, #34831, #51403, #35181, #101885, #4024, #5653, #127596, #82271, #118245, #59463, #55309, #113540, #74339, #57327, #92096, #9637, #24528, #122722, #70065, #17207, #112972, #90957, #72516, #3563, #122534, #90451, #82005, #96611, #80807, #18939, #35997, #45512, #106354, #136154, #25474, #63082, #100561, #84194, #62394, #106880, #111482, #63422, #19562, #48134, #5344, #71333, #85253, #23767, #137738, #49368, #103328, #17144, #82479, #3646, #139499, #104682, #48407, #97848, #70551, #79019, #31742, #96472, #47037, #85853, #78124, #32203, #140652, #9794, #125609, #121541, #58565, #130408, #32016, #119247, #133182, #126811, #36984, #88209, #117902, #62854, #32323, #60771, #78079, #130248, #116355, #4175, #109105, #28158, #25235, #92204, #21494, #58639, #59831, #41460, #65245, #117190, #77129, #16481, #14213, #59716, #94236, #31931, #85532, #90051, #87035, #45468, #66824, #140256, #127192, #89818, #66997, #71227, #64618, #81518, #68162, #111450, #94722, #124965, #94778, #123388, #126507, #23845, #69371, #128164, #19979, #97546, #6809, #129316, #44554, #77729, #64748, #14692, #69851, #26329, #126029, #88185, #104, #47187, #85230, #124167, #74524, #131373, #137510, #124356, #38416, #64116, #131748, #120047, #77400, #75558, #16015, #119123, #113701, #87144, #49886, #38531, #21545, #11906, #138246, #91040, #78883, #55630, #131689, #11542, #77104, #66556, #91019, #19695, #5209, #122818, #63501, #108102, #37713, #96299, #21554, #118500, #137117, #17493, #101147, #134047, #14529, #58104, #93411, #22150, #117256, #142814, #45552, #133573, #99219, #109077, #127461, #58602, #46759, #45847, #76433, #80347, #74500, #16795, #1123, #68396, #100836, #34494, #140394, #80002, #96552, #70889, #33833, #65322, #76156, #68749, #78426, #61113, #130531, #32835, #35009, #32247, #104500, #41723, #126801, #123553, #47141, #17588, #50942, #28627, #109961, #80170, #141601, #119782, #126638, #99544, #124028, #42160, #37554, #59186, #111986, #24754, #47372, #109324, #95122, #81919, #72177, #109258, #120038, #38145, #42454, #4935, #40408, #105030, #24298, #6530, #85733, #78378, #126931, #54401, #84454, #111316, #6247, #9267, #121252, #112755, #41727, #104274, #89731, #84017, #87705, #55285, #81305, #63610, #93493, #111163, #124890, #7929, #23134, #48494, #16280, #10715, #20070, #32434, #107951, #109966, #100516, #84912, #28939, #91046, #68065, #69932, #32002, #105263, #10912, #87550, #84751, #83666, #1973, #57027, #129262, #8623, #135683, #25039, #30318, #122368, #126151, #52858, #30450, #52577, #41529, #108900, #2865, #3044, #99414, #23894, #5920, #111260, #37452, #28494, #103931, #9487, #41078, #52977, #23282, #53714, #1446, #24880, #90886, #28982, #134490, #36316, #136247, #33233, #59115, #113365, #68452, #115348, #22865, #119542, #43202, #120043, #45491, #1743, #127511, #85461, #137626, #13031, #19340, #119449, #2787, #19453, #126019, #66849, #118749, #79220, #68108, #112594, #56503, #86100, #58349, #45304, #15294, #67484, #129283, #122699, #51117, #45329, #143186, #31800, #39090, #75256, #119114, #57445, #124317, #113090, #112728, #111912, #36209, #41031, #21038, #101769, #35643, #5543, #116803, #100337, #64402, #136885, #12929, #55942, #138970, #10083, #6559, #9892, #133134, #51630, #141683, #29869, #123078, #70822, #36016, #100988, #29149, #91030, #85192, #3280, #15140, #49141, #90502, #30935, #22809, #142557, #69528, #80518, #140619, #100550, #129590, #19678, #122937, #76092, #22952, #74956, #61022, #128779, #54880, #29680, #116948, #128250, #129886, #14339, #116189, #69476, #37431, #130683, #99447, #122091, #76776, #75430, #24343, #73341, #84588, #101298, #2378, #95450, #43111, #30860, #82900, #119862, #95504, #137703, #134179, #88366, #21654, #29221, #110467, #42248, #12914, #55157, #17018, #125417, #42561, #42980, #93782, #6111, #110161, #36782, #103364, #32731, #26962, #37067, #117559, #79390, #41846, #4998, #22163, #109931, #80462, #12272, #60049, #84604, #82928, #1901, #22729, #133288, #78674, #57174, #101788, #31844, #92877, #90441, #59596, #101531, #45196, #91277, #53844, #56242, #39900, #3178, #106350, #53478, #57110, #90646, #71488, #88558, #24174, #89952, #62345, #33690, #28362, #102461, #4809, #134393, #12590, #724, #76758, #6019, #93897, #88081, #125972, #49842, #111738, #44427, #12232, #106907, #84084, #44792, #25922, #93071, #142216, #115447, #67604, #132262, #93118, #106894, #103444, #3530, #78097, #131166, #79009, #83127, #117149, #10428, #13872, #130092, #100730, #99730, #12783, #47592, #100737, #130631, #135175, #94447, #54684, #99354, #128771, #19922, #53039, #36336, #108506, #17664, #25523, #9420, #58815, #84192, #61059, #114477, #136263, #49336, #91328, #80372, #51038, #98480, #55531, #50875, #116257, #11887, #135456, #94965, #61891, #65605, #65857, #68165, #61414, #35992, #2971, #84403, #79700, #134947, #95244, #138600, #99281, #92592, #98128, #128951, #82315, #31326, #32726, #3940, #98250, #48443, #78352, #141902, #85750, #57106, #127651, #38256, #21559, #24800, #94887, #94343, #127955, #138760, #1405, #35397, #27280, #7271, #27968, #98401, #62728, #60197, #74668, #83407, #46687, #75649, #120210, #126171, #100288, #120135, #45823, #74237, #3450, #132077, #1047, #31639, #81211, #104196, #66445, #52516, #22068, #52647, #52821, #28295, #113270, #112254, #97385, #139174, #109805, #127669, #92336, #90141, #11798, #39791, #51879, #98004, #98305, #84134, #16108, #114607, #5846, #44318, #63329, #5762, #31202, #51638, #102178, #125799, #61047, #7533, #23857, #138140, #19731, #51212, #95880, #2894, #126648, #7278, #114034, #106516, #87677, #34901, #17049, #90841, #142653, #133367, #16672, #70217, #135334, #113255, #47201, #88998, #88865, #113721, #32739, #98971, #21896, #61014, #113307, #105896, #137309, #23875, #67481, #125839, #97645, #110237, #33059, #7021, #14152, #47656, #104957, #40130, #97672, #130237, #42629, #131455, #117208, #60836, #129222, #54852, #63975, #15311, #28425, #2493, #105134, #31713, #40627, #80654, #10275, #54309, #24183, #87835, #38063, #14193, #30663, #27657, #104384, #5120, #63291, #41171, #139719, #56545, #44860, #4153, #31417, #137428, #121681, #36323, #39361, #39071, #97616, #5988, #141261, #20107, #130868, #71979, #66189, #76452, #42883, #127250, #67978, #31023, #102717, #15216, #130381, #72822, #98179, #139051, #139113, #138279, #25155, #65450, #107288, #110748, #31282, #115693, #100172, #16093, #67748, #47836, #114055, #43695, #75690, #27845, #24552, #109812, #59530, #129412, #7348, #126608, #115054, #40242, #996, #131070, #64419, #117535, #11389, #136715, #117123, #103563, #30956, #89167, #141383, #8541, #47401, #106523, #42691, #50887, #3388, #119533, #53186, #105065, #135665, #61803, #1794, #139812, #78236, #60085, #50303, #104527, #87239, #139553, #46833, #63660, #49098, #1125, #83864, #8267, #43898, #62867, #109381, #906, #62438, #135179, #68742, #3714, #98364, #87999, #27323, #89975, #133270, #98937, #17154, #141604, #26472, #1895, #45939, #14827, #104216, #91160, #79384, #122521, #33728, #126419, #17862, #123419, #19589, #131743, #153, #64295, #90131, #93343, #126578, #115143, #1719, #28945, #20095, #93927, #117096, #96454, #50427, #2230, #121859, #126304, #19656, #141570, #29493, #134163, #106272, #37475, #70371, #53657, #115270, #68330, #85783, #64867, #106039, #10249, #81270, #19345, #14601, #8194, #65839, #42214, #128593, #5186, #37195, #90493, #124720, #126049, #75563, #117286, #94579, #120886, #70192, #102559, #69419, #19050, #138502, #24507, #34179, #112757, #25913, #29967, #89391, #96169, #6943, #61262, #35485, #103015, #87208, #46970, #5458, #100761, #94035, #82863, #109384, #10451, #10038, #116028, #76394, #137589, #107965, #70221, #4348, #13892, #28142, #124095, #95129, #130586, #112335, #64173, #74233, #134907, #59154, #70374, #24686, #124263, #43994, #140383, #126071, #2164, #79915, #123620, #133531, #124851, #130973, #3499, #129551, #92100, #117633, #5470, #3175, #28125, #52493, #135800, #110232, #87730, #125322, #32924, #18201, #132318, #14176, #46315, #81009, #112005, #20076, #33176, #76395, #69534, #143495, #33456, #20374, #8927, #106848, #89842, #97835, #142659, #4626, #131363, #75828, #7029, #138975, #31693, #24695, #138130, #26319, #55622, #132569, #45250, #7438, #105639, #108924, #115337, #37259, #127182, #99521, #96984, #116856, #133894, #119031, #125442, #105475, #37446, #39109, #64504, #15394, #64285, #130578, #61852, #72027, #111391, #100547, #106340, #21565, #25847, #12404, #29057, #136498, #109168, #97702, #12808, #17297, #34744, #25960, #62419, #137338, #100636, #64401, #38, #82123, #85068, #128676, #136012, #61359, #131193, #139886, #131214, #45386, #132657, #116136, #96862, #1587, #109278, #131303, #128480, #133797, #59574, #99970, #103587, #15283, #42944, #100467, #88632, #34365, #77041, #130759, #65231, #110857, #68747, #121522, #98695, #53968, #113580, #114367, #6933, #44937, #76514, #58113, #113502, #98354, #70253, #95711, #4201, #27697, #87502, #55273, #48795, #117949, #18960, #62918, #91440, #6438, #41307, #47869, #26174, #65475, #130473, #121518, #141167, #60756, #96387, #15036, #29636, #1425, #67287, #14337, #5671, #33393, #115516, #97309, #16879, #138123, #61633, #134961, #37503, #1310, #18731, #21198, #50776, #53034, #125182, #89324, #138293, #115935, #57100, #65895, #28936, #140819, #4556, #72251, #80491, #54888, #29478, #60987, #59102, #108720, #46325, #44016, #28477, #52053, #63509, #27586, #15284, #131051, #123097, #82327, #18252, #76410, #72354, #92998, #102921, #122553, #99302, #34808, #60, #7878, #137610, #112937, #779, #17809, #1081, #69907, #22750, #61644, #81679, #96352, #38448, #32256, #95041, #100670, #61352, #19111, #22033, #96643, #20205, #74172, #76146, #98970, #89991, #24345, #36966, #42740, #45191, #80257, #17684, #121715, #19060, #58283, #1065, #3, #67090, #55825, #107845, #39491, #78738, #106946, #99500, #110246, #111402, #16260, #123935, #23329, #1591, #45586, #6437, #132112, #19507, #123099, #112150, #29893, #140205, #69184, #133046, #119694, #23435, #17240, #51850, #22508, #10140, #74992, #133081, #38191, #89381, #86535, #86626, #87646, #134521, #68736, #124232, #83783, #10882, #25194, #114409, #54434, #98863, #96806, #141611, #80855, #84957, #114695, #101488, #77118, #89616, #118069, #127130, #83605, #94082, #87987, #5280, #28975, #108969, #54997, #100138, #35120, #78303, #87549, #104851, #90468, #2597, #84502, #107108, #80140, #137779, #102582, #104033, #16293, #8263, #50549, #100790, #91844, #25128, #141018, #139430, #66335, #125495, #10641, #50271, #39660, #116104, #85555, #86019, #52916, #50866, #56161, #541, #41572, #21099, #34533, #25669, #110931, #53102, #123943, #73985, #117743, #100684, #134471, #49784, #84827, #85317, #761, #9929, #138579, #87104, #58063, #141799, #18001, #120237, #83025, #59541, #22322, #132854, #124538, #109174, #92058, #73927, #114890, #2564, #67178, #118130, #61098, #129915, #71701, #65954, #122071, #140111, #49643, #106321, #119705, #18934, #62994, #109853, #24230, #21779, #94270, #68599, #11509, #1055, #101894, #122565, #97892, #69923, #59232, #2388, #54204, #47399, #44716, #78893, #73877, #51931, #43369, #9150, #78652, #107793, #116560, #95842, #48716, #11603, #63993, #40196, #125625, #61108, #39338, #129938, #85573, #125571, #28792, #61962, #22340, #47133, #110070, #28778, #25268, #120787, #93064, #50588, #123283, #127790, #141285, #39737, #18461, #100365, #102286, #140486, #103218, #55995, #15461, #133990, #49719, #82990, #78319, #28932, #89897, #45885, #122418, #50690, #21795, #133021, #56313, #111904, #4640, #26493, #54040, #121809, #128741, #65422, #4255, #35316, #70493, #72437, #14397, #70442, #85056, #57484, #15153, #98025, #35883, #66129, #109555, #14248, #139440, #96894, #127904, #7362, #74871, #3115, #81632, #32073, #32967, #123879, #42616, #135247, #114690, #7990, #119430, #23823, #141552, #100839, #15189, #139092, #120504, #78387, #130671, #105552, #56132, #35247, #140715, #9713, #54866, #37166, #138526, #2694, #49820, #99250, #121594, #11362, #42259, #76829, #73255, #30425, #122160, #92230, #24846, #125085, #91782, #137799, #133478, #52036, #31268, #103056, #66446, #15969, #13238, #93915, #32791, #53687, #8531, #66658, #67359, #26287, #35853, #20519, #116316, #73815, #50738, #120113, #32201, #30209, #142988, #37153, #128312, #58123, #1056, #40398, #117206, #114983, #12688, #67850, #4119, #109662, #124456, #22376, #67223, #133078, #16588, #25308, #104960, #73810, #40716, #108126, #55927, #66329, #2603, #68923, #118160, #18935, #136776, #63668, #115043, #130945, #27819, #27547, #141412, #133520, #30700, #56303, #134365, #126782, #140310, #141510, #143013, #114201, #54962, #81538, #142813, #20304, #18820, #10082, #3061, #37801, #9812, #27096, #90665, #106943, #47677, #65233, #134351, #118627, #127128, #121508, #90094, #41597, #108358, #49718, #48993, #78283, #130672, #114376, #3744, #72571, #125155, #131912, #27235, #16688, #17461, #128842, #127613, #7762, #67192, #25884, #40887, #107798, #1530, #129992, #83472, #46196, #117600, #106278, #61358, #17477, #84655, #31231, #33212, #137457, #60244, #57305, #51270, #86859, #27942, #51939, #118463, #120042, #35491, #74872, #77834, #31070, #69866, #4496, #40437, #66750, #84331, #136869, #23074, #110250, #134078, #80936, #20272, #4335, #44405, #30390, #61355, #3065, #131369, #42717, #118733, #4813, #105252, #132929, #35755, #29749, #41263, #143101, #70473, #116000, #122766, #56627, #20214, #30523, #103050, #75280, #139523, #127607, #84267, #64169, #42036, #111831, #32732, #27317, #78200, #103213, #4381, #136990, #119989, #51682, #116004, #81986, #110701, #71501, #82411, #49715, #68727, #86674, #105203, #129078, #140279, #55694, #105840, #32207, #117291, #19032, #54944, #74503, #80267, #79671, #2340, #113884, #100324, #79268, #114618, #83606, #94818, #2150, #94094, #50551, #26625, #22699, #118067, #128598, #14067, #75512, #29960, #32449, #120133, #47324, #15667, #65326, #109736, #102258, #115163, #135101, #127664, #134541, #18290, #84278, #38242, #60492, #45957, #116990, #77382, #28911, #5545, #143507, #141348, #23901, #136569, #109821, #78030, #124584, #106748, #424, #121923, #3381, #106199, #91211, #132090, #17151, #16459, #56311, #81894, #22263, #39722, #139047, #79464, #18098, #133206, #47417, #31508, #16655, #950, #48760, #51592, #30312, #32187, #128296, #78233, #65940, #121867, #32874, #56439, #139711, #79049, #6213, #93220, #88895, #115817, #69288, #6627, #107111, #91423, #139959, #30988, #38597, #76773, #38881, #115603, #103684, #114086, #64799, #70661, #141000, #18743, #71146, #29542, #103826, #4579, #138168, #33389, #16154, #21925, #74022, #114276, #112112, #87808, #63354, #28736, #17769, #97289, #11978, #102141, #85283, #81006, #46780, #48402, #1629, #114387, #142715, #98024, #57570, #83737, #91581, #5885, #36560, #39686, #45153, #44503, #110868, #119522, #128616, #25631, #32578, #71438, #39602, #1067, #90066, #44640, #82312, #47483, #26807, #76382, #131784, #79605, #133054, #17201, #123195, #127598, #13553, #62516, #57575, #78732, #64331, #67410, #59869, #18070, #131717, #57181, #118452, #122060, #45297, #28485, #115377, #49290, #82945, #93703, #7660, #75568, #100578, #105882, #112432, #62607, #722, #95109, #48149, #101352, #88847, #94072, #120823, #58777, #120865, #135583, #64970, #52659, #123777, #9362, #24814, #47344, #91368, #2898, #13222, #18330, #61196, #118502, #128795, #35839, #16603, #96676, #107324, #28599, #28301, #98960, #24884, #84714, #58945, #106693, #77159, #2698, #131553, #38082, #6804, #76048, #52589, #33847, #113354, #93225, #71348, #25680, #140741, #85705, #101092, #96379, #117468, #69074, #137967, #60075, #98506, #16961, #29945, #62232, #122382, #53903, #67573, #23455, #123735, #54266, #21812, #596, #43752, #95096, #9077, #14411, #10575, #140061, #120396, #24829, #45070, #127680, #44127, #39415, #55356, #101696, #51385, #25853, #5516, #73328, #71503, #47820, #139527, #79567, #124510, #74326, #56769, #17906, #38094, #32793, #77560, #112400, #60809, #97949, #30881, #29511, #91798, #74642, #135959, #5675, #85587, #122851, #101158, #63167, #5572, #66557, #36622, #134766, #29136, #122208, #25176, #129547, #69347, #41667, #42497, #123675, #53330, #18366, #108677, #40798, #96201, #33866, #52604, #6611, #99128, #35137, #5664, #98647, #85887, #110073, #45036, #95282, #34765, #115175, #45213, #82113, #29433, #115325, #119589, #35400, #63759, #141931, #114867, #117449, #26391, #132049, #75074, #105492, #490, #82981, #3085, #121278, #140994, #24822, #118586, #81821, #64302, #44772, #57922, #19730, #46109, #37787, #68098, #36499, #8160, #101069, #92569, #131179, #78927, #3527, #81359, #69891, #40017, #138212, #76626, #22420, #124682, #101815, #137596, #41137, #12846, #85858, #62335, #94191, #70565, #70994, #40235, #11283, #114178, #31870, #125357, #81075, #15320, #60831, #73446, #89690, #51568, #82476, #31718, #128297, #33240, #23912, #121583, #93292, #27764, #133970, #140135, #80330, #139822, #123200, #139548, #6320, #99818, #49263, #108956, #26222, #90880, #90198, #35515, #111248, #6165, #4624, #103508, #48572, #104561, #119566, #12441, #37568, #10303, #92774, #52133, #15811, #69281, #100896, #92459, #128673, #91653, #141360, #133024, #8340, #109363, #107649, #136954, #101618, #105771, #38704, #66971, #142574, #56153, #109978, #41023, #2042, #64370, #23202, #8579, #68262, #80210, #4465, #115799, #65003, #9951, #111864, #68103, #63840, #18777, #55647, #114990, #47926, #88188, #118412, #105757, #42966, #8642, #95722, #90534, #53749, #141750, #90087, #7685, #65682, #97177, #12399, #25311, #117896, #127773, #45763, #104611, #104793, #124346, #58775, #8783, #48758, #56218, #82445, #85521, #39172, #85966, #81464, #133547, #115329, #56124, #42058, #89858, #47228, #117260, #18532, #136081, #110534, #114324, #24721, #127808, #106990, #77554, #132188, #119252, #123305, #113211, #113688, #45313, #94500, #107497, #118491, #67416, #40140, #42582, #47077, #128748, #2012, #19545, #5592, #133981, #42678, #21750, #39245, #23267, #115161, #82217, #7369, #47932, #67614, #38027, #98905, #98747, #42859, #72541, #97491, #125859, #31095, #47846, #18283, #83918, #98986, #17307, #31785, #81465, #82897, #74143, #120769, #43572, #80206, #54054, #133660, #87991, #106681, #98455, #81240, #5909, #14757, #106461, #136636, #136859, #2217, #67212, #30282, #29280, #36009, #40874, #45666, #37504, #67782, #96235, #51977, #10701, #29385, #99292, #51887, #17962, #74731, #81344, #9992, #138936, #77967, #54827, #137073, #66613, #130003, #115382, #24966, #53447, #29437, #86715, #55524, #34962, #25684, #16940, #93699, #40091, #2018, #103424, #125334, #27342, #111534, #931, #16456, #77470, #6178, #3400, #58423, #103416, #125380, #49878, #89976, #3142, #114261, #117990, #21732, #109584, #140808, #59952, #40361, #102180, #27419, #13357, #40243, #31566, #58317, #43523, #140196, #55774, #119177, #88530, #58985, #89450, #2086, #16463, #104181, #50860, #5038, #22217, #131741, #133725, #91429, #34033, #101095, #28588, #139364, #86646, #6818, #24043, #72759, #122175, #61522, #140538, #1318, #117342, #15804, #129183, #84576, #14093, #128239, #38423, #44811, #85108, #61829, #114186, #12657, #62148, #48988, #60069, #143005, #54349, #43248, #92974, #139248, #104856, #20532, #102884, #95525, #127462, #26045, #18865, #124278, #93805, #60178, #51104, #97694, #91281, #18946, #17244, #92598, #125029, #66463, #128834, #42906, #77757, #141921, #20920, #48399, #114497, #111473, #80408, #111357, #66955, #21518, #61442, #8604, #22582, #92136, #65294, #17528, #96846, #59663, #44754, #93682, #138588, #86797, #119528, #35367, #76082, #130501, #94210, #22046, #20268, #39535, #86479, #128925, #15192, #1681, #68137, #3082, #34122, #115002, #16130, #72670, #64933, #82697, #118908, #119256, #124971, #125794, #77502, #71683, #115646, #123838, #87186, #11746, #37934, #109087, #71809, #24731, #98687, #100483, #62830, #12549, #22843, #98492, #15124, #54409, #44747, #119793, #34390, #49501, #128149, #138424, #80117, #109303, #30990, #7457, #92874, #125129, #69621, #54969, #124699, #47627, #36648, #24562, #95475, #90473, #55977, #28147, #70104, #116892, #58292, #22054, #84938, #93723, #114328, #78657, #17904, #122388, #136597, #84149, #37627, #28360, #137679, #114673, #96533, #17510, #1117, #11721, #48551, #5313, #133830, #117916, #142040, #114664, #61254, #22456, #88363, #106605, #82773, #80425, #50230, #48077, #39697, #21436, #49201, #58881, #25676, #27399, #96554, #64313, #76108, #85260, #117953, #98064, #62194, #8753, #104121, #18163, #106084, #96969, #56330, #139766, #1842, #23438, #124005, #109499, #57320, #32866, #226, #35101, #85049, #31408, #102698, #83272, #50046, #13216, #45836, #84546, #63214, #112872, #76666, #55700, #93976, #11681, #66026, #137095, #16972, #37890, #50101, #77863, #26325, #127653, #5188, #64581, #7124, #31850, #75011, #133155, #142820, #95074, #127795, #37695, #101310, #103817, #61682, #23243, #5256, #136493, #62132, #134358, #118618, #39774, #31390, #13164, #136307, #123580, #30614, #138959, #71549, #133873, #40979, #58325, #84512, #119470, #12542, #76688, #29122, #83787, #67950, #9732, #9770, #37908, #92116, #142567, #98996, #87669, #75988, #72309, #116180, #54090, #108406, #133735, #121599, #4167, #105811, #37415, #107402, #126593, #73645, #12626, #98311, #76588, #44907, #55583, #86330, #52707, #42211, #135265, #90996, #76260, #45003, #40081, #9500, #143389, #75319, #132933, #30050, #135783, #135405, #44207, #121225, #22732, #1258, #58651, #5734, #2236, #83814, #39516, #110588, #86825, #81502, #37275, #104003, #41081, #49027, #86733, #87028, #29161, #38535, #10980, #78995, #129539, #122878, #141175, #84763, #4173, #30714, #6259, #57992, #10829, #85842, #135815, #106669, #21608, #5200, #6096, #77889, #50366, #60552, #109159, #65130, #133379, #129081, #137317, #27233, #55493, #41975, #49582, #13666, #3313, #101004, #84741, #33055, #101770, #110112, #33070, #41614, #70756, #20956, #109333, #94301, #79199, #87829, #12728, #4107, #132949, #53421, #37759, #78022, #63505, #119884, #8381, #83451, #43632, #61105, #86654, #116333, #70869, #55984, #125529, #13080, #66212, #97381, #63856, #11867, #8094, #12253, #83996, #35897, #136127, #80791, #45368, #42109, #29464, #138508, #140320, #130226, #86261, #58588, #105734, #125971, #54770, #73829, #49663, #121973, #121534, #132790, #136832, #142365, #134320, #31129, #105944, #47407, #56948, #2440, #87714, #22453, #122697, #69935, #3128, #31386, #37338, #82425, #5638, #90656, #129724, #57390, #94542, #133351, #19995, #47304, #142932, #130430, #58293, #48460, #69744, #57828, #123084, #43803, #106486, #8759, #54588, #82370, #128088, #66608, #104673, #50523, #93224, #2588, #124919, #15924, #28634, #27640, #59745, #66306, #6663, #103663, #54727, #18368, #112555, #24026, #120218, #41384, #64321, #54774, #29144, #36490, #26344, #9240, #135790, #139597, #117945, #100665, #142221, #10896, #127107, #22234, #36441, #140560, #138638, #56384, #65812, #126738, #51811, #122943, #93360, #96032, #110530, #78668, #12618, #13680, #75417, #134691, #107561, #139948, #62730, #85565, #101798, #86845, #15615, #80823, #35462, #72685, #90304, #138349, #38133, #121205, #92635, #90732, #62187, #108540, #127784, #114767, #46036, #31960, #132916, #66151, #141072, #141551, #23808, #71054, #65407, #63790, #56115, #82087, #26618, #65116, #75572, #71188, #77909, #89837, #142571, #6853, #30504, #85468, #12417, #30651, #73893, #45121, #1155, #78720, #10764, #15443, #132495, #119094, #124648, #8765, #135702, #134891, #55398, #28120, #105823, #28275, #61530, #54388, #102328, #92898, #8009, #140846, #50518, #113685, #130055, #92577, #99627, #9074, #20612, #52745, #19285, #88955, #15915, #43767, #28437, #51068, #67052, #96504, #74806, #2377, #107159, #104519, #140059, #135985, #32549, #60613, #45396, #117032, #73122, #24633, #107906, #97026, #81826, #73962, #15631, #18984, #126415, #114225, #60463, #37080, #53271, #6156, #6314, #124440, #100463, #28481, #75883, #36774, #85611, #86689, #123716, #39970, #25488, #83156, #84784, #86199, #115081, #41389, #22002, #71073, #31741, #104367, #75814, #142283, #76300, #36081, #116313, #95132, #119646, #72870, #34399, #47249, #87020, #126209, #65467, #51497, #83412, #29654, #7587, #2206, #55503, #85093, #82634, #107489, #89037, #21070, #114338, #123588, #111577, #86298, #109913, #109924, #68260, #62492, #70926, #6336, #61129, #126141, #51699, #37005, #49072, #131948, #133664, #80677, #15298, #121855, #35783, #26812, #109452, #66566, #92317, #110749, #42379, #64884, #36462, #8438, #97681, #66909, #13344, #62689, #41045, #103046, #57813, #142704, #51445, #56510, #87719, #136162, #88101, #78274, #6997, #82952, #95901, #60109, #123889, #18732, #132352, #80684, #15567, #96528, #65423, #110721, #69408, #75142, #82647, #61978, #139507, #7486, #13810, #91712, #62512, #44294, #33348, #96796, #48452, #27756, #12944, #2303, #98914, #34750, #8955, #42865, #55923, #9070, #143252, #30805, #66107, #140077, #8877, #90027, #34364, #51975, #3553, #45595, #98807, #93564, #68109, #100119, #68557, #24853, #100626, #137427, #89787, #139234, #28666, #49803, #53268, #99017, #5471, #108012, #6726, #87770, #31059, #10117, #39641, #52986, #74770, #83537, #129270, #105863, #11073, #104917, #8496, #50728, #64898, #105450, #6445, #35524, #15580, #26693, #27044, #22846, #30894, #3681, #129583, #115047, #38609, #108181, #4052, #113390, #39631, #17164, #83274, #46289, #41912, #101375, #118655, #18924, #104672, #79849, #139944, #28944, #90157, #59946, #52040, #24672, #41898, #136423, #63945, #102979, #119276, #74779, #41904, #15674, #5084, #106449, #3492, #98328, #114709, #59315, #86348, #56827, #5658, #18756, #137804, #97832, #111068, #83313, #119355, #86741, #40316, #84292, #56072, #55369, #97384, #47479, #25793, #105315, #40762, #23665, #69102, #39748, #111039, #80052, #114361, #8153, #95082, #3228, #82487, #63924, #97925, #112811, #60116, #55264, #140096, #10253, #38377, #94328, #26081, #125878, #66407, #74830, #74425, #22183, #51421, #119171, #65874, #22550, #106177, #8320, #67084, #79136, #84982, #119363, #130222, #63717, #73453, #48300, #66396, #101125, #139720, #92087, #109672, #21820, #83011, #90510, #106631, #138419, #4336, #23226, #57119, #18074, #68384, #50146, #128130, #33405, #113642, #78364, #87930, #118104, #134115, #71663, #135313, #88832, #35379, #69970, #21211, #136126, #115454, #81408, #35945, #96186, #139376, #131713, #123432, #27580, #112416, #15809, #37636, #71978, #32588, #2411, #11082, #99977, #100252, #104886, #117802, #57052, #54706, #51515, #76214, #32713, #90161, #7822, #56483, #76207, #119939, #114513, #30261, #141078, #39252, #1958, #138435, #128032, #7642, #25726, #134467, #133634, #13332, #51260, #8424, #84305, #97807, #26870, #36359, #45593, #111344, #140534, #68936, #26173, #38781 ) ) ;
#23190 = LINE ( 'NONE', #24641, #5849 ) ;
#23191 = DIRECTION ( 'NONE',  ( -1.000000000000000000, -1.224606353822377258E-16, -0.000000000000000000 ) ) ;
#23192 = EDGE_LOOP ( 'NONE', ( #6510, #60783, #68050, #126474, #95522, #20256 ) ) ;
#23193 = ORIENTED_EDGE ( 'NONE', *, *, #69469, .T. ) ;
#23194 = CARTESIAN_POINT ( 'NONE',  ( 123.5212635252314470, -4.472830434245839371, -4.472830434245840259 ) ) ;
#23195 = VERTEX_POINT ( 'NONE', #96816 ) ;
#23196 = EDGE_CURVE ( 'NONE', #77143, #90786, #83656, .T. ) ;
#23197 = CARTESIAN_POINT ( 'NONE',  ( 9.183988606268997046, 28.73617430169793607, 5.000000000000000000 ) ) ;
#23198 = DIRECTION ( 'NONE',  ( 0.000000000000000000, -0.9976538855070753442, -0.06845965770171351383 ) ) ;
#23199 = LINE ( 'NONE', #45038, #109177 ) ;
#23200 = LINE ( 'NONE', #108064, #102098 ) ;
#23202 = ADVANCED_FACE ( 'NONE', ( #19299 ), #98297, .F. ) ;
#23201 = VECTOR ( 'NONE', #17873, 1000.000000000000000 ) ;
#23203 = AXIS2_PLACEMENT_3D ( 'NONE', #4903, #140457, #104237 ) ;
#23204 = CARTESIAN_POINT ( 'NONE',  ( 110.7454301918981088, -5.291415217122918513, -3.055000000000000160 ) ) ;
#23205 = VERTEX_POINT ( 'NONE', #375 ) ;
#23206 = EDGE_CURVE ( 'NONE', #59816, #86810, #109158, .T. ) ;
#23207 = VERTEX_POINT ( 'NONE', #141063 ) ;
#23208 = DIRECTION ( 'NONE',  ( 0.7071067811865486830, -0.7071067811865464625, -0.000000000000000000 ) ) ;
#23209 = VECTOR ( 'NONE', #48458, 1000.000000000000000 ) ;
#23210 = VECTOR ( 'NONE', #131222, 1000.000000000000000 ) ;
#23211 = VECTOR ( 'NONE', #122271, 1000.000000000000227 ) ;
#23212 = VECTOR ( 'NONE', #82120, 1000.000000000000000 ) ;
#23213 = CARTESIAN_POINT ( 'NONE',  ( -12.70710678118644665, -9.740707523384180888, 5.000000000000000000 ) ) ;
#23214 = EDGE_CURVE ( 'NONE', #8442, #22844, #132382, .T. ) ;
#23215 = VECTOR ( 'NONE', #115084, 1000.000000000000000 ) ;
#23216 = ORIENTED_EDGE ( 'NONE', *, *, #72244, .F. ) ;
#23217 = EDGE_LOOP ( 'NONE', ( #78449, #4011, #28326, #18829, #32888, #43917, #111614, #132500, #29513, #29326, #117246, #64612, #89420, #61446, #76501, #105657, #71211, #12917, #15098, #29704, #56676, #86288 ) ) ;
#23218 = CARTESIAN_POINT ( 'NONE',  ( 35.58376352523143282, -6.110000000000001208, -3.741295971395164515E-16 ) ) ;
#23219 = VERTEX_POINT ( 'NONE', #87422 ) ;
#23220 = DIRECTION ( 'NONE',  ( -1.000000000000000000, -0.000000000000000000, -0.000000000000000000 ) ) ;
#23221 = CARTESIAN_POINT ( 'NONE',  ( 1.087903141435219379, 6.871911579029515771, 3.967499999999989146 ) ) ;
#23222 = CIRCLE ( 'NONE', #78839, 2.500000000000000888 ) ;
#23223 = EDGE_CURVE ( 'NONE', #102488, #124605, #142525, .T. ) ;
#23224 = CARTESIAN_POINT ( 'NONE',  ( 33.45376352523145158, -6.109999999999998543, -3.741295971395162543E-16 ) ) ;
#23225 = EDGE_LOOP ( 'NONE', ( #99212, #95349, #78138, #140570 ) ) ;
#23226 = ADVANCED_FACE ( 'NONE', ( #21446 ), #110558, .F. ) ;
#23227 = CARTESIAN_POINT ( 'NONE',  ( -29.29298673570674794, -21.74070752338405299, 4.999753212805210012 ) ) ;
#23228 = VERTEX_POINT ( 'NONE', #108399 ) ;
#23229 = ORIENTED_EDGE ( 'NONE', *, *, #43030, .F. ) ;
#23230 = AXIS2_PLACEMENT_3D ( 'NONE', #4229, #4970, #92021 ) ;
#23231 = VERTEX_POINT ( 'NONE', #86716 ) ;
#23232 = AXIS2_PLACEMENT_3D ( 'NONE', #32539, #31119, #9296 ) ;
#23233 = VECTOR ( 'NONE', #113856, 1000.000000000000000 ) ;
#23234 = DIRECTION ( 'NONE',  ( -0.7071067811865486830, -0.7071067811865464625, 0.000000000000000000 ) ) ;
#23235 = EDGE_CURVE ( 'NONE', #35520, #128274, #41772, .T. ) ;
#23236 = ORIENTED_EDGE ( 'NONE', *, *, #101781, .F. ) ;
#23237 = CARTESIAN_POINT ( 'NONE',  ( 33.48921356237309510, -27.52281430457078670, 5.000000000000000000 ) ) ;
#23238 = VECTOR ( 'NONE', #51581, 1000.000000000000000 ) ;
#23239 = CARTESIAN_POINT ( 'NONE',  ( 6.066782984417857350, 3.061616997868382648E-16, -2.500000000000000444 ) ) ;
#23240 =( NAMED_UNIT ( * ) SI_UNIT ( $, .STERADIAN. ) SOLID_ANGLE_UNIT ( ) );
#23241 = VECTOR ( 'NONE', #42286, 999.9999999999998863 ) ;
#23242 = LINE ( 'NONE', #131320, #130067 ) ;
#23243 = ADVANCED_FACE ( 'NONE', ( #33076 ), #53347, .F. ) ;
#23244 = FACE_BOUND ( 'NONE', #133518, .T. ) ;
#23245 = VERTEX_POINT ( 'NONE', #8378 ) ;
#23246 = CARTESIAN_POINT ( 'NONE',  ( 0.000000000000000000, 0.000000000000000000, 5.000000000000000000 ) ) ;
#23247 = DIRECTION ( 'NONE',  ( -0.000000000000000000, 0.000000000000000000, 1.000000000000000000 ) ) ;
#23248 = VECTOR ( 'NONE', #52739, 1000.000000000000000 ) ;
#23249 = DIRECTION ( 'NONE',  ( -0.7071067811865487940, 0.7071067811865463515, 0.000000000000000000 ) ) ;
#23250 = PLANE ( 'NONE',  #90210 ) ;
#23251 = ORIENTED_EDGE ( 'NONE', *, *, #79310, .T. ) ;
#23252 = CARTESIAN_POINT ( 'NONE',  ( -7.140000000000001457, -60.26999999999998892, -12.10072711459627293 ) ) ;
#23253 = VERTEX_POINT ( 'NONE', #22132 ) ;
#23254 = ORIENTED_EDGE ( 'NONE', *, *, #89629, .T. ) ;
#23255 = ORIENTED_EDGE ( 'NONE', *, *, #109265, .T. ) ;
#23256 = EDGE_CURVE ( 'NONE', #82657, #79834, #63556, .T. ) ;
#23257 = CARTESIAN_POINT ( 'NONE',  ( 45.41209685856478728, 5.291415217122921177, -3.054999999999994831 ) ) ;
#23258 = ORIENTED_EDGE ( 'NONE', *, *, #47475, .F. ) ;
#23259 = VECTOR ( 'NONE', #79401, 1000.000000000000000 ) ;
#23260 = DIRECTION ( 'NONE',  ( 0.6830127018922181881, 0.6830127018922202975, -0.2588190451025214056 ) ) ;
#23261 = CARTESIAN_POINT ( 'NONE',  ( 14.74000000000000021, -2.055000000000000160, 0.000000000000000000 ) ) ;
#23262 = VERTEX_POINT ( 'NONE', #85251 ) ;
#23263 = LINE ( 'NONE', #132073, #37574 ) ;
#23265 = LINE ( 'NONE', #64, #138475 ) ;
#23264 = VECTOR ( 'NONE', #44844, 999.9999999999998863 ) ;
#23266 = ADVANCED_FACE ( 'NONE', ( #99703 ), #85984, .F. ) ;
#23267 = ADVANCED_FACE ( 'NONE', ( #75140 ), #130219, .F. ) ;
#23268 = DIRECTION ( 'NONE',  ( -1.000000000000000000, -1.224606353822377258E-16, -0.000000000000000000 ) ) ;
#23269 = DIRECTION ( 'NONE',  ( 2.110369192185896011E-16, -1.000000000000000000, 0.000000000000000000 ) ) ;
#23270 = CARTESIAN_POINT ( 'NONE',  ( -65.99451991528749772, 28.92564299267984396, 4.000000000000000000 ) ) ;
#23271 = PLANE ( 'NONE',  #125791 ) ;
#23272 = ORIENTED_EDGE ( 'NONE', *, *, #14416, .F. ) ;
#23273 = ORIENTED_EDGE ( 'NONE', *, *, #21916, .F. ) ;
#23274 = VERTEX_POINT ( 'NONE', #74414 ) ;
#23275 = VECTOR ( 'NONE', #67386, 1000.000000000000227 ) ;
#23276 = ORIENTED_EDGE ( 'NONE', *, *, #87257, .F. ) ;
#23277 = DIRECTION ( 'NONE',  ( -0.7071067811865487940, 0.7071067811865463515, -0.000000000000000000 ) ) ;
#23278 = DIRECTION ( 'NONE',  ( 0.7071067811865487940, 0.7071067811865463515, 0.000000000000000000 ) ) ;
#23279 = ORIENTED_EDGE ( 'NONE', *, *, #77901, .T. ) ;
#23280 = VERTEX_POINT ( 'NONE', #119306 ) ;
#23281 = CARTESIAN_POINT ( 'NONE',  ( 159.7320121765528711, 26.96999999999993847, -34.92499999999998295 ) ) ;
#23282 = ADVANCED_FACE ( 'NONE', ( #118602 ), #141814, .T. ) ;
#23283 = LINE ( 'NONE', #22558, #122671 ) ;
#23284 = ORIENTED_EDGE ( 'NONE', *, *, #106707, .T. ) ;
#23285 = DIRECTION ( 'NONE',  ( -0.6830127018922181881, 0.6830127018922202975, -0.2588190451025214056 ) ) ;
#23286 = VECTOR ( 'NONE', #90047, 1000.000000000000227 ) ;
#23287 = AXIS2_PLACEMENT_3D ( 'NONE', #97102, #62402, #73977 ) ;
#23288 = CARTESIAN_POINT ( 'NONE',  ( 22.88901570796818774, -1.420450978533076558, 4.272001239691295638 ) ) ;
#23289 = CARTESIAN_POINT ( 'NONE',  ( 24.56706980810189123, 2.126176841940952134, -7.934999999999993392 ) ) ;
#23290 = FACE_OUTER_BOUND ( 'NONE', #120183, .T. ) ;
#23291 = VERTEX_POINT ( 'NONE', #77976 ) ;
#23293 = LINE ( 'NONE', #80577, #96199 ) ;
#23292 = CARTESIAN_POINT ( 'NONE',  ( 110.8912635252314658, -4.472830434245839371, -4.472830434245839371 ) ) ;
#23294 = DIRECTION ( 'NONE',  ( -0.7071067811865486830, -0.7071067811865464625, 0.000000000000000000 ) ) ;
#23295 = CYLINDRICAL_SURFACE ( 'NONE', #32658, 4.000000000000000000 ) ;
#23296 = CARTESIAN_POINT ( 'NONE',  ( -45.29974487139158867, -27.71228299555237840, 4.000000000000000000 ) ) ;
#23298 = ORIENTED_EDGE ( 'NONE', *, *, #64749, .T. ) ;
#23297 = DIRECTION ( 'NONE',  ( 0.7071067811865487940, -0.7071067811865463515, 0.000000000000000000 ) ) ;
#23299 = DIRECTION ( 'NONE',  ( 0.6830127018922180770, -0.6830127018922204085, -0.2588190451025213501 ) ) ;
#23300 = ORIENTED_EDGE ( 'NONE', *, *, #120715, .T. ) ;
#23301 = DIRECTION ( 'NONE',  ( -0.3543493200069163240, 0.000000000000000000, -0.9351131265310288487 ) ) ;
#23302 = VECTOR ( 'NONE', #80580, 1000.000000000000000 ) ;
#23303 = DIRECTION ( 'NONE',  ( 1.000000000000000000, 0.000000000000000000, 0.000000000000000000 ) ) ;
#23304 = LINE ( 'NONE', #102345, #128202 ) ;
#23306 = EDGE_LOOP ( 'NONE', ( #47, #64919, #117252, #122097 ) ) ;
#23305 =( BOUNDED_CURVE ( )  B_SPLINE_CURVE ( 3, ( #41392, #131267, #120344, #110204 ),
 .UNSPECIFIED., .F., .F. ) 
 B_SPLINE_CURVE_WITH_KNOTS ( ( 4, 4 ),
 ( 4.407062196515976638, 4.453802039120700940 ),
 .UNSPECIFIED. ) 
 CURVE ( )  GEOMETRIC_REPRESENTATION_ITEM ( )  RATIONAL_B_SPLINE_CURVE ( ( 1.000000000000000000, 0.9998179572116046021, 0.9998179572116046021, 1.000000000000000000 ) ) 
 REPRESENTATION_ITEM ( '' )  );
#23307 = VECTOR ( 'NONE', #10765, 1000.000000000000000 ) ;
#23308 = VECTOR ( 'NONE', #32911, 999.9999999999998863 ) ;
#23309 = CARTESIAN_POINT ( 'NONE',  ( -26.99451991528749417, 28.92564299267956685, 4.000000000000000000 ) ) ;
#23310 = CARTESIAN_POINT ( 'NONE',  ( 15.65467068707222076, 3.061616997868383634E-16, -2.500000000000000444 ) ) ;
#23311 = ORIENTED_EDGE ( 'NONE', *, *, #115035, .F. ) ;
#23312 = VECTOR ( 'NONE', #13145, 999.9999999999998863 ) ;
#23313 = VECTOR ( 'NONE', #17284, 1000.000000000000000 ) ;
#23314 = VECTOR ( 'NONE', #62065, 1000.000000000000227 ) ;
#23315 = VECTOR ( 'NONE', #20354, 1000.000000000000000 ) ;
#23316 =( BOUNDED_CURVE ( )  B_SPLINE_CURVE ( 3, ( #68711, #71557, #102758, #81744 ),
 .UNSPECIFIED., .F., .T. ) 
 B_SPLINE_CURVE_WITH_KNOTS ( ( 4, 4 ),
 ( 5.920967161967927161, 7.341195215986642708 ),
 .UNSPECIFIED. ) 
 CURVE ( )  GEOMETRIC_REPRESENTATION_ITEM ( )  RATIONAL_B_SPLINE_CURVE ( ( 1.000000000000000000, 0.8388583629366603844, 0.8388583629366603844, 1.000000000000000000 ) ) 
 REPRESENTATION_ITEM ( '' )  );
#23317 = DIRECTION ( 'NONE',  ( -0.7071067811865487940, 0.7071067811865463515, 0.000000000000000000 ) ) ;
#23319 = VERTEX_POINT ( 'NONE', #48740 ) ;
#23318 = VECTOR ( 'NONE', #65619, 1000.000000000000000 ) ;
#23320 = CARTESIAN_POINT ( 'NONE',  ( 33.48921356237309510, -27.52281430457078670, 5.000000000000000000 ) ) ;
#23322 = ORIENTED_EDGE ( 'NONE', *, *, #12154, .F. ) ;
#23321 = CARTESIAN_POINT ( 'NONE',  ( 15.49238828748955576, 4.584330080086930965E-16, 0.000000000000000000 ) ) ;
#23323 = EDGE_CURVE ( 'NONE', #111354, #15103, #136437, .T. ) ;
#23324 = ORIENTED_EDGE ( 'NONE', *, *, #66320, .T. ) ;
#23325 = CARTESIAN_POINT ( 'NONE',  ( 2.602316007518551189, 13.59879521490819165, -24.48217750605332910 ) ) ;
#23326 = CONICAL_SURFACE ( 'NONE', #127561, 2.055000000000000604, 0.9599310885968764806 ) ;
#23327 = CARTESIAN_POINT ( 'NONE',  ( -4.499999999999968914, 13.56627193232214523, -10.57019076586069772 ) ) ;
#23328 = ORIENTED_EDGE ( 'NONE', *, *, #132683, .T. ) ;
#23329 = ADVANCED_FACE ( 'NONE', ( #71217 ), #81391, .F. ) ;
#23330 = DIRECTION ( 'NONE',  ( 0.7071067811865487940, 0.7071067811865463515, -0.000000000000000000 ) ) ;
#23331 = EDGE_CURVE ( 'NONE', #45528, #114150, #100436, .T. ) ;
#23332 = EDGE_CURVE ( 'NONE', #54652, #94433, #3750, .T. ) ;
#23333 = CARTESIAN_POINT ( 'NONE',  ( 11.99451991528749417, 28.92564299267946382, 4.000000000000000000 ) ) ;
#23334 = EDGE_CURVE ( 'NONE', #27882, #108415, #137179, .T. ) ;
#23335 = EDGE_LOOP ( 'NONE', ( #116460, #90751, #101462, #119209 ) ) ;
#23336 = AXIS2_PLACEMENT_3D ( 'NONE', #93697, #139377, #40060 ) ;
#23337 = FACE_OUTER_BOUND ( 'NONE', #135922, .T. ) ;
#23338 = EDGE_CURVE ( 'NONE', #82772, #69799, #16052, .T. ) ;
#23339 = DIRECTION ( 'NONE',  ( 0.7071067811865487940, 0.7071067811865463515, 0.000000000000000000 ) ) ;
#23340 = PLANE ( 'NONE',  #72554 ) ;
#23341 = VECTOR ( 'NONE', #45497, 1000.000000000000114 ) ;
#23342 = CARTESIAN_POINT ( 'NONE',  ( 126.3365768546761956, -7.119864409971977004, -0.03876453820169215719 ) ) ;
#23343 = EDGE_CURVE ( 'NONE', #33303, #100766, #93669, .T. ) ;
#23344 = CARTESIAN_POINT ( 'NONE',  ( 129.1416937171295558, -2.130196079827424871, -7.949999999999999289 ) ) ;
#23345 = LINE ( 'NONE', #67618, #46614 ) ;
#23346 = EDGE_LOOP ( 'NONE', ( #117946, #19477, #120978 ) ) ;
#23347 = AXIS2_PLACEMENT_3D ( 'NONE', #73391, #96510, #141486 ) ;
#23348 = ORIENTED_EDGE ( 'NONE', *, *, #113999, .T. ) ;
#23349 = ORIENTED_EDGE ( 'NONE', *, *, #130879, .F. ) ;
#23351 = EDGE_CURVE ( 'NONE', #88704, #125103, #71940, .T. ) ;
#23350 = SURFACE_STYLE_USAGE ( .BOTH. , #31395 ) ;
#23352 = AXIS2_PLACEMENT_3D ( 'NONE', #11074, #33608, #93494 ) ;
#23353 = ORIENTED_EDGE ( 'NONE', *, *, #107961, .T. ) ;
#23354 = ORIENTED_EDGE ( 'NONE', *, *, #103718, .T. ) ;
#23355 = ORIENTED_EDGE ( 'NONE', *, *, #105669, .F. ) ;
#23356 = CARTESIAN_POINT ( 'NONE',  ( 1.494327302228996235, -1.524194347291654372, -6.429405139856394946 ) ) ;
#23357 = CARTESIAN_POINT ( 'NONE',  ( -54.18398860626899705, 28.73617430169825226, 5.000000000000000000 ) ) ;
#23358 = VECTOR ( 'NONE', #87902, 1000.000000000000227 ) ;
#23359 = ORIENTED_EDGE ( 'NONE', *, *, #79504, .T. ) ;
#23360 = CARTESIAN_POINT ( 'NONE',  ( 48.18398860626899705, 28.73617430169820608, 5.000000000000000000 ) ) ;
#23361 = CARTESIAN_POINT ( 'NONE',  ( -20.99451991528748707, 28.92564299267952777, 4.000000000000000000 ) ) ;
#23362 = EDGE_CURVE ( 'NONE', #122791, #31140, #18822, .T. ) ;
#23363 = LINE ( 'NONE', #34995, #104182 ) ;
#23364 = DIRECTION ( 'NONE',  ( -0.7071067811865487940, 0.7071067811865463515, -0.000000000000000000 ) ) ;
#23365 = CARTESIAN_POINT ( 'NONE',  ( 122.6462635252314328, -4.472830434245840259, 4.472830434245839371 ) ) ;
#23366 = COLOUR_RGB ( '', 0.72549020, 0.75294118, 0.79215686) ;
#23367 = EDGE_LOOP ( 'NONE', ( #143116, #88131, #80266, #46485 ) ) ;
#23368 = DIRECTION ( 'NONE',  ( -0.000000000000000000, -0.3543493200069152693, 0.9351131265310292928 ) ) ;
#23369 = DIRECTION ( 'NONE',  ( 0.7071067811865487940, -0.7071067811865463515, 0.000000000000000000 ) ) ;
#23370 = CARTESIAN_POINT ( 'NONE',  ( 19.82816939922339117, 9.759292476615614831, 4.000000000000000000 ) ) ;
#23371 = CARTESIAN_POINT ( 'NONE',  ( 29.99451991528749417, 28.92564299267958816, 4.000000000000000000 ) ) ;
#23372 = EDGE_CURVE ( 'NONE', #112760, #14379, #69808, .T. ) ;
#23373 = DIRECTION ( 'NONE',  ( -1.000000000000000000, -0.000000000000000000, -0.000000000000000000 ) ) ;
#23374 = CARTESIAN_POINT ( 'NONE',  ( 11.62000000000000099, 2.055000000000001492, 0.000000000000000000 ) ) ;
#23375 = CARTESIAN_POINT ( 'NONE',  ( 48.20419371712955581, -6.884901960086285300, -3.975000000000000089 ) ) ;
#23376 = DIRECTION ( 'NONE',  ( -0.000000000000000000, -0.3543493200069152693, 0.9351131265310292928 ) ) ;
#23377 = DIRECTION ( 'NONE',  ( -0.3543493200069162685, -0.000000000000000000, -0.9351131265310288487 ) ) ;
#23378 = AXIS2_PLACEMENT_3D ( 'NONE', #63597, #9880, #62874 ) ;
#23379 = ORIENTED_EDGE ( 'NONE', *, *, #21397, .T. ) ;
#23380 = EDGE_LOOP ( 'NONE', ( #142296, #68291, #9932, #116399 ) ) ;
#23381 = CARTESIAN_POINT ( 'NONE',  ( 45.04166666666665719, -3.975000000000002753, 6.884901960086286188 ) ) ;
#23382 = FACE_OUTER_BOUND ( 'NONE', #13189, .T. ) ;
#23383 = VECTOR ( 'NONE', #92550, 1000.000000000000000 ) ;
#23384 = FACE_OUTER_BOUND ( 'NONE', #19910, .T. ) ;
#23385 = ORIENTED_EDGE ( 'NONE', *, *, #899, .F. ) ;
#23386 = AXIS2_PLACEMENT_3D ( 'NONE', #1900, #78815, #23706 ) ;
#23387 = FACE_OUTER_BOUND ( 'NONE', #54695, .T. ) ;
#23388 = CARTESIAN_POINT ( 'NONE',  ( 36.18398860626899705, 28.73617430169812437, 5.000000000000000000 ) ) ;
#23389 = CARTESIAN_POINT ( 'NONE',  ( 34.56293019189810423, 1.637169565754157174, 6.110000000000002984 ) ) ;
#23390 = VERTEX_POINT ( 'NONE', #34458 ) ;
#23391 = EDGE_CURVE ( 'NONE', #136547, #4967, #67096, .T. ) ;
#23392 = LINE ( 'NONE', #109699, #140506 ) ;
#23393 = ORIENTED_EDGE ( 'NONE', *, *, #26639, .T. ) ;
#23394 = ORIENTED_EDGE ( 'NONE', *, *, #76592, .F. ) ;
#23395 = DIRECTION ( 'NONE',  ( -1.000000000000000000, -0.000000000000000000, -0.000000000000000000 ) ) ;
#23396 = LINE ( 'NONE', #113995, #133391 ) ;
#23398 = EDGE_CURVE ( 'NONE', #68247, #61017, #78680, .T. ) ;
#23397 = FILL_AREA_STYLE ('',( #22656 ) ) ;
#23399 = LINE ( 'NONE', #111862, #62601 ) ;
#23400 = ORIENTED_EDGE ( 'NONE', *, *, #24979, .T. ) ;
#23401 = LINE ( 'NONE', #88694, #44184 ) ;
#23402 = ORIENTED_EDGE ( 'NONE', *, *, #42208, .T. ) ;
#23403 = LINE ( 'NONE', #113267, #58679 ) ;
#23404 = DIRECTION ( 'NONE',  ( -0.7071067811865486830, -0.7071067811865464625, 0.000000000000000000 ) ) ;
#23405 = PLANE ( 'NONE',  #19936 ) ;
#23406 = CARTESIAN_POINT ( 'NONE',  ( -16.50229999999999819, 3.130000000000007887, 0.000000000000000000 ) ) ;
#23407 = PLANE ( 'NONE',  #129598 ) ;
#23408 = VECTOR ( 'NONE', #36244, 1000.000000000000000 ) ;
#23409 = LINE ( 'NONE', #45913, #48486 ) ;
#23410 = EDGE_CURVE ( 'NONE', #1311, #83494, #28577, .T. ) ;
#23411 = ORIENTED_EDGE ( 'NONE', *, *, #134833, .T. ) ;
#23412 = PLANE ( 'NONE',  #40740 ) ;
#23413 = CARTESIAN_POINT ( 'NONE',  ( 57.51626352523144448, -4.472830434245839371, 4.472830434245839371 ) ) ;
#23414 = CARTESIAN_POINT ( 'NONE',  ( 4.828169399223495084, -2.240707523384264377, 4.000000000000000000 ) ) ;
#23415 = ADVANCED_FACE ( 'NONE', ( #5189 ), #58956, .T. ) ;
#23416 = FACE_OUTER_BOUND ( 'NONE', #7301, .T. ) ;
#23417 = DIRECTION ( 'NONE',  ( 0.000000000000000000, -1.000000000000000000, 0.000000000000000000 ) ) ;
#23418 = ORIENTED_EDGE ( 'NONE', *, *, #52187, .F. ) ;
#23419 = CARTESIAN_POINT ( 'NONE',  ( 0.000000000000000000, 0.000000000000000000, 0.000000000000000000 ) ) ;
#23421 = VECTOR ( 'NONE', #23873, 1000.000000000000000 ) ;
#23420 =( LENGTH_UNIT ( ) NAMED_UNIT ( * ) SI_UNIT ( .MILLI., .METRE. ) );
#23422 = EDGE_LOOP ( 'NONE', ( #97008, #112478, #94156, #66685, #90258 ) ) ;
#23423 = VECTOR ( 'NONE', #106904, 1000.000000000000000 ) ;
#23424 = AXIS2_PLACEMENT_3D ( 'NONE', #38595, #37160, #103808 ) ;
#23425 = ADVANCED_FACE ( 'NONE', ( #92944 ), #125328, .T. ) ;
#23426 = DIRECTION ( 'NONE',  ( 0.3543493200069162685, -0.000000000000000000, -0.9351131265310288487 ) ) ;
#23427 = VERTEX_POINT ( 'NONE', #37877 ) ;
#23428 = CARTESIAN_POINT ( 'NONE',  ( 34.49999999999976552, 7.464255608400424791, 4.994342998332163219 ) ) ;
#23429 = FACE_OUTER_BOUND ( 'NONE', #130491, .T. ) ;
#23430 = VECTOR ( 'NONE', #23889, 1000.000000000000000 ) ;
#23431 = AXIS2_PLACEMENT_3D ( 'NONE', #26413, #40170, #93091 ) ;
#23432 = VECTOR ( 'NONE', #45735, 999.9999999999998863 ) ;
#23433 = VECTOR ( 'NONE', #71301, 1000.000000000000000 ) ;
#23434 = CARTESIAN_POINT ( 'NONE',  ( 30.70710678118632941, -9.740707523384177335, 5.000000000000000000 ) ) ;
#23435 = ADVANCED_FACE ( 'NONE', ( #49482 ), #38568, .F. ) ;
#23436 = FACE_BOUND ( 'NONE', #81848, .T. ) ;
#23437 = LINE ( 'NONE', #122753, #38657 ) ;
#23438 = ADVANCED_FACE ( 'NONE', ( #133089 ), #96473, .F. ) ;
#23439 = DIRECTION ( 'NONE',  ( 0.7071067811865486830, -0.7071067811865464625, -0.000000000000000000 ) ) ;
#23441 = DIRECTION ( 'NONE',  ( 0.000000000000000000, 0.000000000000000000, 1.000000000000000000 ) ) ;
#23440 = VECTOR ( 'NONE', #127914, 1000.000000000000000 ) ;
#23443 = ORIENTED_EDGE ( 'NONE', *, *, #133759, .T. ) ;
#23442 = LINE ( 'NONE', #90875, #85222 ) ;
#23444 = DIRECTION ( 'NONE',  ( 0.7071067811865487940, -0.7071067811865463515, 0.000000000000000000 ) ) ;
#23445 = VERTEX_POINT ( 'NONE', #83516 ) ;
#23446 = ADVANCED_FACE ( 'NONE', ( #39291 ), #118969, .F. ) ;
#23447 = ORIENTED_EDGE ( 'NONE', *, *, #121990, .T. ) ;
#23448 = CARTESIAN_POINT ( 'NONE',  ( 76.18293019189810877, -1.637169565754158951, -6.109999999999998543 ) ) ;
#23449 = EDGE_LOOP ( 'NONE', ( #79154, #66222, #64491, #68703, #25856 ) ) ;
#23450 = LINE ( 'NONE', #44541, #12902 ) ;
#23451 = AXIS2_PLACEMENT_3D ( 'NONE', #59488, #136298, #94216 ) ;
#23452 = DIRECTION ( 'NONE',  ( 0.000000000000000000, 0.000000000000000000, -1.000000000000000000 ) ) ;
#23453 = VERTEX_POINT ( 'NONE', #95067 ) ;
#23454 = DIRECTION ( 'NONE',  ( 0.7071067811865487940, -0.7071067811865463515, 0.000000000000000000 ) ) ;
#23455 = ADVANCED_FACE ( 'NONE', ( #29813 ), #127732, .F. ) ;
#23456 = CIRCLE ( 'NONE', #104482, 2.500000000000000444 ) ;
#23457 = CARTESIAN_POINT ( 'NONE',  ( 122.4791666666666714, -7.950000000000000178, 2.130196079827424427 ) ) ;
#23458 = AXIS2_PLACEMENT_3D ( 'NONE', #127544, #128966, #6417 ) ;
#23459 = EDGE_CURVE ( 'NONE', #132715, #98945, #18198, .T. ) ;
#23460 = FACE_OUTER_BOUND ( 'NONE', #4259, .T. ) ;
#23461 = CARTESIAN_POINT ( 'NONE',  ( -34.42500000000000426, 10.54139925780190801, 5.000000000000000000 ) ) ;
#23463 = DIRECTION ( 'NONE',  ( -0.7071067811865487940, 0.7071067811865463515, -0.000000000000000000 ) ) ;
#23462 = LINE ( 'NONE', #66986, #101380 ) ;
#23464 = VECTOR ( 'NONE', #73423, 1000.000000000000000 ) ;
#23465 = DIRECTION ( 'NONE',  ( 0.000000000000000000, 0.000000000000000000, 1.000000000000000000 ) ) ;
#23466 = DIRECTION ( 'NONE',  ( 0.6830127018922180770, -0.6830127018922204085, -0.2588190451025213501 ) ) ;
#23467 = VERTEX_POINT ( 'NONE', #8050 ) ;
#23468 = EDGE_LOOP ( 'NONE', ( #135492, #32814, #95797, #17863 ) ) ;
#23469 = AXIS2_PLACEMENT_3D ( 'NONE', #143367, #22981, #111451 ) ;
#23470 = DIRECTION ( 'NONE',  ( 0.000000000000000000, 0.000000000000000000, -1.000000000000000000 ) ) ;
#23471 =( NAMED_UNIT ( * ) PLANE_ANGLE_UNIT ( ) SI_UNIT ( $, .RADIAN. ) );
#23472 = ORIENTED_EDGE ( 'NONE', *, *, #101844, .T. ) ;
#23473 = ORIENTED_EDGE ( 'NONE', *, *, #10903, .T. ) ;
#23474 = ORIENTED_EDGE ( 'NONE', *, *, #66907, .F. ) ;
#23475 = VECTOR ( 'NONE', #10158, 1000.000000000000000 ) ;
#23476 = EDGE_CURVE ( 'NONE', #24896, #64028, #84244, .T. ) ;
#23477 = APPLICATION_CONTEXT ( 'automotive_design' ) ;
#23478 = CARTESIAN_POINT ( 'NONE',  ( 29.89626352523142927, 4.472830434245840259, -4.472830434245838482 ) ) ;
#23479 = VERTEX_POINT ( 'NONE', #74793 ) ;
#23480 = LINE ( 'NONE', #2415, #23174 ) ;
#23481 = CARTESIAN_POINT ( 'NONE',  ( 89.62086038379622721, -6.884901960086286188, 3.974999999999997424 ) ) ;
#23482 = CARTESIAN_POINT ( 'NONE',  ( 32.42080628287043709, 3.047499999999997655, 5.278424836066143655 ) ) ;
#23483 = CARTESIAN_POINT ( 'NONE',  ( 19.28515664589288292, 1.196650378695338635, -30.59010235425024860 ) ) ;
#23484 = ORIENTED_EDGE ( 'NONE', *, *, #24859, .F. ) ;
#23485 = DIRECTION ( 'NONE',  ( 0.000000000000000000, 1.000000000000000000, 0.000000000000000000 ) ) ;
#23486 = CARTESIAN_POINT ( 'NONE',  ( -17.39060256275758221, -2.561874075326514788, 4.636692559446314199 ) ) ;
#23487 = VECTOR ( 'NONE', #22484, 1000.000000000000000 ) ;
#23488 = CARTESIAN_POINT ( 'NONE',  ( -71.99451991528749772, 28.92564299267988304, 4.000000000000000000 ) ) ;
#23490 = ORIENTED_EDGE ( 'NONE', *, *, #127884, .T. ) ;
#23489 = PLANE ( 'NONE',  #109654 ) ;
#23491 = AXIS2_PLACEMENT_3D ( 'NONE', #121576, #67218, #502 ) ;
#23492 = VERTEX_POINT ( 'NONE', #52285 ) ;
#23493 = FACE_OUTER_BOUND ( 'NONE', #141649, .T. ) ;
#23494 = LINE ( 'NONE', #123564, #7470 ) ;
#23495 = DIRECTION ( 'NONE',  ( -0.000000000000000000, 0.000000000000000000, 1.000000000000000000 ) ) ;
#23496 = EDGE_LOOP ( 'NONE', ( #46636, #8377, #22534, #85133, #58555 ) ) ;
#23497 = SURFACE_SIDE_STYLE ('',( #14034 ) ) ;
#23498 = ORIENTED_EDGE ( 'NONE', *, *, #86853, .F. ) ;
#23499 = VECTOR ( 'NONE', #38044, 1000.000000000000000 ) ;
#23500 =( NAMED_UNIT ( * ) SI_UNIT ( $, .STERADIAN. ) SOLID_ANGLE_UNIT ( ) );
#23501 = CARTESIAN_POINT ( 'NONE',  ( 6.938893903907228378E-15, -22.06887692260758627, 4.000000000000000000 ) ) ;
#23502 = CARTESIAN_POINT ( 'NONE',  ( -3.489213562373097322, -27.52281430457057709, 5.000000000000000000 ) ) ;
#23503 = VECTOR ( 'NONE', #106574, 1000.000000000000000 ) ;
#23504 = CARTESIAN_POINT ( 'NONE',  ( -34.42500000000001137, -0.02281430457058350458, 5.000000000000000000 ) ) ;
#23505 = DIRECTION ( 'NONE',  ( -0.7071067811865487940, 0.7071067811865463515, -0.000000000000000000 ) ) ;
#23507 = EDGE_CURVE ( 'NONE', #67994, #123638, #117522, .T. ) ;
#23506 = DIRECTION ( 'NONE',  ( -0.3543493200069162685, -0.000000000000000000, -0.9351131265310288487 ) ) ;
#23508 = CARTESIAN_POINT ( 'NONE',  ( -34.92500000000001137, 22.22500000000000142, 4.000000000000000000 ) ) ;
#23509 = DIRECTION ( 'NONE',  ( -0.7071067811865487940, -0.7071067811865463515, -0.000000000000000000 ) ) ;
#23510 = VERTEX_POINT ( 'NONE', #51600 ) ;
#23511 = EDGE_LOOP ( 'NONE', ( #5596, #45703, #41920, #84206 ) ) ;
#23512 = AXIS2_PLACEMENT_3D ( 'NONE', #3910, #61255, #49646 ) ;
#23513 = CARTESIAN_POINT ( 'NONE',  ( -0.3281693992235289459, 14.25929247661557042, 4.000000000000000000 ) ) ;
#23514 =( BOUNDED_CURVE ( )  B_SPLINE_CURVE ( 3, ( #103990, #140234, #38773, #30017 ),
 .UNSPECIFIED., .F., .T. ) 
 B_SPLINE_CURVE_WITH_KNOTS ( ( 4, 4 ),
 ( 4.350170835173025274, 4.500739107949256912 ),
 .UNSPECIFIED. ) 
 CURVE ( )  GEOMETRIC_REPRESENTATION_ITEM ( )  RATIONAL_B_SPLINE_CURVE ( ( 1.000000000000000000, 0.9981116584018945304, 0.9981116584018945304, 1.000000000000000000 ) ) 
 REPRESENTATION_ITEM ( '' )  );
#23515 = CYLINDRICAL_SURFACE ( 'NONE', #25025, 0.5000000000000004441 ) ;
#23516 = EDGE_CURVE ( 'NONE', #66688, #40407, #136909, .T. ) ;
#23517 = VERTEX_POINT ( 'NONE', #18949 ) ;
#23518 = CARTESIAN_POINT ( 'NONE',  ( 22.25000000000000000, 0.000000000000000000, 0.000000000000000000 ) ) ;
#23519 = CARTESIAN_POINT ( 'NONE',  ( -15.48921356237309510, -27.52281430457066236, 5.000000000000000000 ) ) ;
#23520 = LINE ( 'NONE', #13342, #139371 ) ;
#23521 = EDGE_CURVE ( 'NONE', #16006, #84048, #63211, .T. ) ;
#23522 = ORIENTED_EDGE ( 'NONE', *, *, #54209, .T. ) ;
#23523 = CARTESIAN_POINT ( 'NONE',  ( 12.51280225271498736, -2.499999999999999112, 0.000000000000000000 ) ) ;
#23524 = LINE ( 'NONE', #22086, #7154 ) ;
#23525 = EDGE_CURVE ( 'NONE', #72338, #128631, #86368, .T. ) ;
#23526 = DIRECTION ( 'NONE',  ( 0.000000000000000000, -1.091707662666338270E-16, 1.000000000000000000 ) ) ;
#23527 = AXIS2_PLACEMENT_3D ( 'NONE', #1199, #111400, #102695 ) ;
#23528 = CARTESIAN_POINT ( 'NONE',  ( 29.29289321881324781, 17.25929247661554200, 5.000000000000000000 ) ) ;
#23529 = EDGE_CURVE ( 'NONE', #110079, #445, #8732, .T. ) ;
#23530 = CARTESIAN_POINT ( 'NONE',  ( 57.80793019189810877, -6.109999999999999432, 1.637169565754158507 ) ) ;
#23531 = CARTESIAN_POINT ( 'NONE',  ( 26.99999999999980815, -8.151047557385048492, -8.977947279169864458 ) ) ;
#23532 = AXIS2_PLACEMENT_3D ( 'NONE', #27174, #40236, #103997 ) ;
#23533 = LINE ( 'NONE', #77245, #127491 ) ;
#23534 = DIRECTION ( 'NONE',  ( -0.7071067811865486830, 0.7071067811865464625, 0.000000000000000000 ) ) ;
#23535 = ORIENTED_EDGE ( 'NONE', *, *, #108964, .T. ) ;
#23536 = EDGE_CURVE ( 'NONE', #90132, #111726, #119656, .T. ) ;
#23537 = CARTESIAN_POINT ( 'NONE',  ( 10.37159235450332062, 2.500000000000001332, 0.000000000000000000 ) ) ;
#23538 = ORIENTED_EDGE ( 'NONE', *, *, #102250, .F. ) ;
#23539 =( GEOMETRIC_REPRESENTATION_CONTEXT ( 3 ) GLOBAL_UNCERTAINTY_ASSIGNED_CONTEXT ( ( #25863 ) ) GLOBAL_UNIT_ASSIGNED_CONTEXT ( ( #97692, #20113, #86115 ) ) REPRESENTATION_CONTEXT ( 'NONE', 'WORKASPACE' ) );
#23540 = VECTOR ( 'NONE', #99129, 1000.000000000000000 ) ;
#23541 = CARTESIAN_POINT ( 'NONE',  ( 7.499999999999949374, 12.05218569542904561, 5.000000000000000000 ) ) ;
#23542 = VECTOR ( 'NONE', #120765, 1000.000000000000000 ) ;
#23543 = CIRCLE ( 'NONE', #30492, 6.349999999999999645 ) ;
#23544 = CARTESIAN_POINT ( 'NONE',  ( -12.18398860626900060, 28.73617430169795739, 5.000000000000000000 ) ) ;
#23545 = DIRECTION ( 'NONE',  ( -0.3543493200069162685, -0.000000000000000000, -0.9351131265310288487 ) ) ;
#23546 = EDGE_CURVE ( 'NONE', #80500, #123836, #138604, .T. ) ;
#23547 = CARTESIAN_POINT ( 'NONE',  ( -35.99451991528749772, 28.92564299267963079, 4.000000000000000000 ) ) ;
#23548 = ADVANCED_FACE ( 'NONE', ( #21807 ), #129985, .T. ) ;
#23549 = DIRECTION ( 'NONE',  ( 0.000000000000000000, 0.000000000000000000, 1.000000000000000000 ) ) ;
#23550 = CYLINDRICAL_SURFACE ( 'NONE', #126409, 0.5000000000000004441 ) ;
#23551 = EDGE_LOOP ( 'NONE', ( #80888, #27220, #41014, #78092 ) ) ;
#23552 = ORIENTED_EDGE ( 'NONE', *, *, #117463, .T. ) ;
#23553 = DIRECTION ( 'NONE',  ( -0.000000000000000000, -0.3543493200069152693, 0.9351131265310292928 ) ) ;
#23554 = DIRECTION ( 'NONE',  ( -0.6830127018922181881, 0.6830127018922202975, -0.2588190451025214056 ) ) ;
#23555 = CARTESIAN_POINT ( 'NONE',  ( 0.000000000000000000, 0.000000000000000000, 5.000000000000000000 ) ) ;
#23556 = EDGE_CURVE ( 'NONE', #23783, #77634, #55160, .T. ) ;
#23557 = CARTESIAN_POINT ( 'NONE',  ( 16.08747294953710849, -6.094999999999989981, 3.732111120401553285E-16 ) ) ;
#23558 = CARTESIAN_POINT ( 'NONE',  ( 78.24586038379621300, 3.974999999999996980, 6.884901960086287964 ) ) ;
#23559 = CARTESIAN_POINT ( 'NONE',  ( 17.50183651486032943, -17.24070752338410628, 8.407044977365183414 ) ) ;
#23560 = DIRECTION ( 'NONE',  ( 2.496005001405478586E-15, 1.000000000000000000, -0.000000000000000000 ) ) ;
#23561 = ORIENTED_EDGE ( 'NONE', *, *, #140594, .T. ) ;
#23562 = CARTESIAN_POINT ( 'NONE',  ( 71.72916666666667140, 7.950000000000001954, -2.130196079827421762 ) ) ;
#23563 = LINE ( 'NONE', #67831, #93237 ) ;
#23564 = CARTESIAN_POINT ( 'NONE',  ( -66.48921356237309510, -27.52281430457101763, 5.000000000000000000 ) ) ;
#23565 = CARTESIAN_POINT ( 'NONE',  ( -6.183988606268994381, 28.73617430169791476, 5.000000000000000000 ) ) ;
#23566 = EDGE_CURVE ( 'NONE', #28263, #142286, #44297, .T. ) ;
#23567 = ORIENTED_EDGE ( 'NONE', *, *, #109809, .F. ) ;
#23568 = AXIS2_PLACEMENT_3D ( 'NONE', #141883, #67914, #14185 ) ;
#23569 = DIRECTION ( 'NONE',  ( 0.7071067811865487940, -0.7071067811865463515, 0.000000000000000000 ) ) ;
#23570 = CARTESIAN_POINT ( 'NONE',  ( 7.600000000000009415, 0.000000000000000000, 0.000000000000000000 ) ) ;
#23571 = CARTESIAN_POINT ( 'NONE',  ( 64.16709685856476142, -3.055000000000000160, -5.291415217122921177 ) ) ;
#23572 = AXIS2_PLACEMENT_3D ( 'NONE', #84148, #51499, #19560 ) ;
#23573 = EDGE_CURVE ( 'NONE', #73841, #65308, #97945, .T. ) ;
#23574 = ORIENTED_EDGE ( 'NONE', *, *, #89215, .F. ) ;
#23575 = ORIENTED_EDGE ( 'NONE', *, *, #132041, .F. ) ;
#23576 = VECTOR ( 'NONE', #29103, 1000.000000000000000 ) ;
#23577 = CARTESIAN_POINT ( 'NONE',  ( -23.29289321881329755, -6.740707523384218192, 5.000000000000000000 ) ) ;
#23578 = DIRECTION ( 'NONE',  ( -0.7071067811865487940, 0.7071067811865463515, 0.000000000000000000 ) ) ;
#23579 = CARTESIAN_POINT ( 'NONE',  ( 12.18398860626900060, 28.73617430169795739, 5.000000000000000000 ) ) ;
#23580 = FACE_OUTER_BOUND ( 'NONE', #121217, .T. ) ;
#23582 = EDGE_LOOP ( 'NONE', ( #107551, #79467, #82377, #38533 ) ) ;
#23581 = LINE ( 'NONE', #1780, #68489 ) ;
#23583 = DIRECTION ( 'NONE',  ( -0.7071067811865487940, 0.7071067811865463515, -0.000000000000000000 ) ) ;
#23584 = CARTESIAN_POINT ( 'NONE',  ( -0.005480084712502889671, 28.92564299267938210, 4.000000000000000000 ) ) ;
#23585 = LINE ( 'NONE', #133098, #70342 ) ;
#23586 = AXIS2_PLACEMENT_3D ( 'NONE', #32205, #130829, #63438 ) ;
#23587 = DIRECTION ( 'NONE',  ( 0.7071067811865486830, -0.7071067811865464625, -0.000000000000000000 ) ) ;
#23588 = ORIENTED_EDGE ( 'NONE', *, *, #25508, .F. ) ;
#23589 = EDGE_CURVE ( 'NONE', #14142, #71472, #110217, .T. ) ;
#23590 = VERTEX_POINT ( 'NONE', #76197 ) ;
#23591 = CARTESIAN_POINT ( 'NONE',  ( 53.37543019189811133, -5.291415217122920289, -3.055000000000001492 ) ) ;
#23592 = ORIENTED_EDGE ( 'NONE', *, *, #11709, .F. ) ;
#23593 = LINE ( 'NONE', #56277, #22083 ) ;
#23594 = DIRECTION ( 'NONE',  ( 0.7071067811865486830, -0.7071067811865464625, -0.000000000000000000 ) ) ;
#23595 = LINE ( 'NONE', #77307, #54881 ) ;
#23596 = EDGE_CURVE ( 'NONE', #42879, #108448, #120358, .T. ) ;
#23597 = VECTOR ( 'NONE', #94711, 999.9999999999998863 ) ;
#23598 = FACE_OUTER_BOUND ( 'NONE', #130932, .T. ) ;
#23599 = CARTESIAN_POINT ( 'NONE',  ( 5.816011393731002066, 28.73617430169783304, 5.000000000000000000 ) ) ;
#23600 = VERTEX_POINT ( 'NONE', #12344 ) ;
#23601 = ORIENTED_EDGE ( 'NONE', *, *, #127305, .F. ) ;
#23602 = VECTOR ( 'NONE', #119784, 1000.000000000000000 ) ;
#23603 = DIRECTION ( 'NONE',  ( 0.000000000000000000, -1.000000000000000000, 0.000000000000000000 ) ) ;
#23604 = CARTESIAN_POINT ( 'NONE',  ( -19.93618820135884562, -3.270000000000008900, -36.39086428169088094 ) ) ;
#23605 = ORIENTED_EDGE ( 'NONE', *, *, #141115, .F. ) ;
#23606 = EDGE_CURVE ( 'NONE', #138104, #121, #142182, .T. ) ;
#23607 = FACE_OUTER_BOUND ( 'NONE', #133321, .T. ) ;
#23608 = CARTESIAN_POINT ( 'NONE',  ( -24.79289321881328334, 12.75929247661558463, 5.000000000000000000 ) ) ;
#23609 = VECTOR ( 'NONE', #139448, 1000.000000000000000 ) ;
#23610 = ORIENTED_EDGE ( 'NONE', *, *, #28044, .F. ) ;
#23611 = EDGE_CURVE ( 'NONE', #87888, #64475, #56632, .T. ) ;
#23612 = FACE_BOUND ( 'NONE', #73677, .T. ) ;
#23613 = DIRECTION ( 'NONE',  ( 0.7071067811865487940, 0.7071067811865463515, 0.000000000000000000 ) ) ;
#23614 = PLANE ( 'NONE',  #79144 ) ;
#23615 = DIRECTION ( 'NONE',  ( 0.7071067811865487940, -0.7071067811865463515, 0.000000000000000000 ) ) ;
#23616 = VECTOR ( 'NONE', #78133, 999.9999999999998863 ) ;
#23617 = DIRECTION ( 'NONE',  ( 0.7071067811865487940, 0.7071067811865463515, 0.000000000000000000 ) ) ;
#23618 = LINE ( 'NONE', #132432, #136903 ) ;
#23619 = CARTESIAN_POINT ( 'NONE',  ( 94.86850992298124652, -53.48000000000006082, 7.939999999998056168 ) ) ;
#23620 = ORIENTED_EDGE ( 'NONE', *, *, #49553, .F. ) ;
#23621 = ORIENTED_EDGE ( 'NONE', *, *, #56613, .T. ) ;
#23622 = CARTESIAN_POINT ( 'NONE',  ( 106.3704301918981230, -3.055000000000001492, 5.291415217122917625 ) ) ;
#23623 = VERTEX_POINT ( 'NONE', #108775 ) ;
#23624 = CARTESIAN_POINT ( 'NONE',  ( 69.29974487139159578, -27.71228299555254537, 4.000000000000000000 ) ) ;
#23625 = EDGE_LOOP ( 'NONE', ( #83972, #64722, #84187, #82173 ) ) ;
#23626 = DIRECTION ( 'NONE',  ( -0.000000000000000000, -0.3543493200069152693, 0.9351131265310292928 ) ) ;
#23627 = VECTOR ( 'NONE', #59063, 999.9999999999998863 ) ;
#23628 =( GEOMETRIC_REPRESENTATION_CONTEXT ( 3 ) GLOBAL_UNCERTAINTY_ASSIGNED_CONTEXT ( ( #14246 ) ) GLOBAL_UNIT_ASSIGNED_CONTEXT ( ( #5974, #84999, #29892 ) ) REPRESENTATION_CONTEXT ( 'NONE', 'WORKASPACE' ) );
#23629 = AXIS2_PLACEMENT_3D ( 'NONE', #86198, #120949, #130426 ) ;
#23630 = DIRECTION ( 'NONE',  ( -1.000000000000000000, -1.224606353822377258E-16, -0.000000000000000000 ) ) ;
#23631 = VECTOR ( 'NONE', #54198, 1000.000000000000000 ) ;
#23632 = AXIS2_PLACEMENT_3D ( 'NONE', #46691, #100998, #89417 ) ;
#23633 = FACE_OUTER_BOUND ( 'NONE', #48634, .T. ) ;
#23634 = ORIENTED_EDGE ( 'NONE', *, *, #72112, .F. ) ;
#23635 = CARTESIAN_POINT ( 'NONE',  ( -25.08567745463940213, 22.22500000000000142, 8.728487125628603849 ) ) ;
#23636 = LINE ( 'NONE', #44731, #5591 ) ;
#23637 = EDGE_CURVE ( 'NONE', #6676, #45046, #31970, .T. ) ;
#23638 = DIRECTION ( 'NONE',  ( -0.000000000000000000, -0.3543493200069152693, 0.9351131265310292928 ) ) ;
#23639 = DIRECTION ( 'NONE',  ( 0.7071067811865487940, 0.7071067811865463515, 0.000000000000000000 ) ) ;
#23641 = CARTESIAN_POINT ( 'NONE',  ( -10.49999999999992895, 14.14708470758590408, -0.5283514160166316032 ) ) ;
#23640 = DIRECTION ( 'NONE',  ( 0.7071067811865486830, -0.7071067811865464625, -0.000000000000000000 ) ) ;
#23642 = DIRECTION ( 'NONE',  ( 0.6830127018922181881, 0.6830127018922202975, -0.2588190451025214056 ) ) ;
#23643 = AXIS2_PLACEMENT_3D ( 'NONE', #128597, #83695, #65520 ) ;
#23644 = AXIS2_PLACEMENT_3D ( 'NONE', #106247, #40343, #87400 ) ;
#23645 = AXIS2_PLACEMENT_3D ( 'NONE', #129326, #52484, #117711 ) ;
#23646 = DIRECTION ( 'NONE',  ( 0.000000000000000000, 0.000000000000000000, -1.000000000000000000 ) ) ;
#23647 = ORIENTED_EDGE ( 'NONE', *, *, #113987, .T. ) ;
#23648 = LINE ( 'NONE', #133151, #123650 ) ;
#23649 = CARTESIAN_POINT ( 'NONE',  ( 66.18398860626901126, 28.73617430169833753, 5.000000000000000000 ) ) ;
#23650 = ORIENTED_EDGE ( 'NONE', *, *, #133980, .T. ) ;
#23651 = EDGE_CURVE ( 'NONE', #49245, #69087, #87780, .T. ) ;
#23652 = VERTEX_POINT ( 'NONE', #122532 ) ;
#23653 = EDGE_CURVE ( 'NONE', #134939, #126282, #79083, .T. ) ;
#23654 = ORIENTED_EDGE ( 'NONE', *, *, #135523, .F. ) ;
#23655 = CARTESIAN_POINT ( 'NONE',  ( 57.31293019189810423, -1.637169565754159617, -6.110000000000001208 ) ) ;
#23656 = ORIENTED_EDGE ( 'NONE', *, *, #88915, .T. ) ;
#23657 = CARTESIAN_POINT ( 'NONE',  ( -32.99999999999976552, -1.447814304570818500, 5.000000000000000000 ) ) ;
#23658 = CARTESIAN_POINT ( 'NONE',  ( 5.733306282870439752, -6.094999999999989981, -1.633150327867689100 ) ) ;
#23659 = CARTESIAN_POINT ( 'NONE',  ( 89.97959685856477563, 6.109999999999999432, 1.637169565754164280 ) ) ;
#23660 = EDGE_LOOP ( 'NONE', ( #71624, #140277, #117546, #22585 ) ) ;
#23661 = ORIENTED_EDGE ( 'NONE', *, *, #3010, .F. ) ;
#23662 = DIRECTION ( 'NONE',  ( -1.000000000000000000, -1.224606353822377258E-16, -0.000000000000000000 ) ) ;
#23663 = CARTESIAN_POINT ( 'NONE',  ( 184.1500000000000057, -57.15000000000009095, 34.92499999999998295 ) ) ;
#23664 = ORIENTED_EDGE ( 'NONE', *, *, #109523, .T. ) ;
#23665 = ADVANCED_FACE ( 'NONE', ( #65348 ), #76937, .F. ) ;
#23666 = DIRECTION ( 'NONE',  ( -0.7071067811865486830, -0.7071067811865464625, -0.000000000000000000 ) ) ;
#23667 = CIRCLE ( 'NONE', #95379, 2.500000000000000888 ) ;
#23668 = DIRECTION ( 'NONE',  ( 0.000000000000000000, 0.000000000000000000, 1.000000000000000000 ) ) ;
#23669 = DIRECTION ( 'NONE',  ( 0.6830127018922181881, 0.6830127018922202975, -0.2588190451025214056 ) ) ;
#23670 = VERTEX_POINT ( 'NONE', #54466 ) ;
#23671 = VECTOR ( 'NONE', #27001, 1000.000000000000000 ) ;
#23672 = DIRECTION ( 'NONE',  ( 0.7071067811865487940, -0.7071067811865463515, 0.000000000000000000 ) ) ;
#23673 = ORIENTED_EDGE ( 'NONE', *, *, #5775, .F. ) ;
#23674 = VECTOR ( 'NONE', #123898, 1000.000000000000000 ) ;
#23675 = ORIENTED_EDGE ( 'NONE', *, *, #143448, .T. ) ;
#23676 = EDGE_LOOP ( 'NONE', ( #62354, #1657, #80835, #2162, #119567, #85141 ) ) ;
#23677 = DIRECTION ( 'NONE',  ( 0.6830127018922181881, 0.6830127018922202975, -0.2588190451025214056 ) ) ;
#23678 = VECTOR ( 'NONE', #120927, 1000.000000000000000 ) ;
#23679 = PLANE ( 'NONE',  #97769 ) ;
#23680 = DIRECTION ( 'NONE',  ( -0.6830127018922180770, -0.6830127018922204085, -0.2588190451025213501 ) ) ;
#23681 = CARTESIAN_POINT ( 'NONE',  ( 152.4000000000000057, 7.919999999999947526, 16.57229999999999137 ) ) ;
#23682 = CARTESIAN_POINT ( 'NONE',  ( -1.171830600776468945, 18.75929247661553134, 4.000000000000000000 ) ) ;
#23683 = ORIENTED_EDGE ( 'NONE', *, *, #58939, .T. ) ;
#23684 = VECTOR ( 'NONE', #22541, 999.9999999999998863 ) ;
#23685 = CARTESIAN_POINT ( 'NONE',  ( 54.18398860626899705, 28.73617430169825226, 5.000000000000000000 ) ) ;
#23686 = CARTESIAN_POINT ( 'NONE',  ( 16.74956980810188867, 3.967499999999998916, 6.871911579029510442 ) ) ;
#23687 = DIRECTION ( 'NONE',  ( -0.3543493200069162685, -0.000000000000000000, -0.9351131265310288487 ) ) ;
#23688 = EDGE_CURVE ( 'NONE', #115745, #4418, #43559, .T. ) ;
#23689 = CARTESIAN_POINT ( 'NONE',  ( 0.000000000000000000, 0.000000000000000000, 5.000000000000000000 ) ) ;
#23690 = CARTESIAN_POINT ( 'NONE',  ( -6.183988606268994381, 28.73617430169791476, 5.000000000000000000 ) ) ;
#23691 = ORIENTED_EDGE ( 'NONE', *, *, #137850, .T. ) ;
#23692 = ADVANCED_FACE ( 'NONE', ( #88511 ), #21214, .T. ) ;
#23693 = ORIENTED_EDGE ( 'NONE', *, *, #98453, .T. ) ;
#23694 = AXIS2_PLACEMENT_3D ( 'NONE', #109899, #54825, #122924 ) ;
#23695 = VERTEX_POINT ( 'NONE', #121108 ) ;
#23696 = SURFACE_SIDE_STYLE ('',( #14244 ) ) ;
#23697 = CARTESIAN_POINT ( 'NONE',  ( -20.99999999999985079, -4.068876922607771895, 4.000000000000000000 ) ) ;
#23698 = DIRECTION ( 'NONE',  ( -0.6830127018922181881, 0.6830127018922202975, -0.2588190451025214056 ) ) ;
#23699 = DIRECTION ( 'NONE',  ( 0.6830127018922181881, 0.6830127018922202975, -0.2588190451025214056 ) ) ;
#23700 = EDGE_CURVE ( 'NONE', #127570, #19214, #100090, .T. ) ;
#23702 = EDGE_CURVE ( 'NONE', #83048, #122228, #23199, .T. ) ;
#23701 = CARTESIAN_POINT ( 'NONE',  ( 10.03591437549700771, 8.432637487761468265, -4.375000000000003553 ) ) ;
#23703 = CARTESIAN_POINT ( 'NONE',  ( 60.18398860626900415, 28.73617430169829490, 5.000000000000000000 ) ) ;
#23704 = LINE ( 'NONE', #46210, #52545 ) ;
#23705 = DIRECTION ( 'NONE',  ( 0.7071067811865487940, 0.7071067811865463515, 0.000000000000000000 ) ) ;
#23706 = DIRECTION ( 'NONE',  ( -0.7071067811865486830, -0.7071067811865464625, 0.000000000000000000 ) ) ;
#23707 = ORIENTED_EDGE ( 'NONE', *, *, #94300, .F. ) ;
#23708 = PLANE ( 'NONE',  #76584 ) ;
#23709 = AXIS2_PLACEMENT_3D ( 'NONE', #68152, #22422, #55092 ) ;
#23710 = ORIENTED_EDGE ( 'NONE', *, *, #92408, .F. ) ;
#23711 = CARTESIAN_POINT ( 'NONE',  ( 16.73810023419144954, 0.1001526995030668499, -33.96747071225524905 ) ) ;
#23712 = VERTEX_POINT ( 'NONE', #34125 ) ;
#23713 = DIRECTION ( 'NONE',  ( -0.6830127018922181881, 0.6830127018922202975, -0.2588190451025214056 ) ) ;
#23715 = ORIENTED_EDGE ( 'NONE', *, *, #41148, .T. ) ;
#23714 = LINE ( 'NONE', #67985, #27892 ) ;
#23716 = EDGE_CURVE ( 'NONE', #13610, #136798, #111678, .T. ) ;
#23717 = EDGE_CURVE ( 'NONE', #35748, #50158, #69625, .T. ) ;
#23718 = PLANE ( 'NONE',  #132910 ) ;
#23719 = VERTEX_POINT ( 'NONE', #71043 ) ;
#23720 = DIRECTION ( 'NONE',  ( -0.7071067811865487940, 0.7071067811865463515, 0.000000000000000000 ) ) ;
#23722 = ORIENTED_EDGE ( 'NONE', *, *, #30900, .F. ) ;
#23721 = VECTOR ( 'NONE', #23373, 1000.000000000000000 ) ;
#23723 = DIRECTION ( 'NONE',  ( 0.000000000000000000, 1.000000000000000000, 0.000000000000000000 ) ) ;
#23724 = ORIENTED_EDGE ( 'NONE', *, *, #51989, .F. ) ;
#23725 = DIRECTION ( 'NONE',  ( -0.7071067811865487940, 0.7071067811865463515, -0.000000000000000000 ) ) ;
#23726 = EDGE_CURVE ( 'NONE', #47652, #130156, #81203, .T. ) ;
#23727 = CARTESIAN_POINT ( 'NONE',  ( 107.5583603837962414, -7.949999999999997513, -2.130196079827425759 ) ) ;
#23728 = DIRECTION ( 'NONE',  ( 0.000000000000000000, -0.000000000000000000, -1.000000000000000000 ) ) ;
#23729 = DIRECTION ( 'NONE',  ( 0.000000000000000000, -1.000000000000000000, 0.000000000000000000 ) ) ;
#23730 = ORIENTED_EDGE ( 'NONE', *, *, #132629, .T. ) ;
#23731 = CARTESIAN_POINT ( 'NONE',  ( -10.17183060077639745, -14.24070752338413648, 4.000000000000000000 ) ) ;
#23732 = CARTESIAN_POINT ( 'NONE',  ( 26.18753812416034421, -22.22500000000000142, 4.000000000000000000 ) ) ;
#23733 = DIRECTION ( 'NONE',  ( 0.7071067811865486830, -0.7071067811865464625, -0.000000000000000000 ) ) ;
#23734 = CARTESIAN_POINT ( 'NONE',  ( 10.35416666666666430, 1.633150327867695095, 6.094999999999988205 ) ) ;
#23735 = CARTESIAN_POINT ( 'NONE',  ( 23.60373647476854941, 5.808823158059035485, 5.808823158059032821 ) ) ;
#23737 = EDGE_CURVE ( 'NONE', #28591, #136607, #15873, .T. ) ;
#23736 = VECTOR ( 'NONE', #104276, 1000.000000000000000 ) ;
#23738 = AXIS2_PLACEMENT_3D ( 'NONE', #143487, #121021, #21718 ) ;
#23740 = DIRECTION ( 'NONE',  ( 0.6830127018922180770, -0.6830127018922204085, -0.2588190451025213501 ) ) ;
#23739 = VECTOR ( 'NONE', #20564, 1000.000000000000000 ) ;
#23741 = CARTESIAN_POINT ( 'NONE',  ( 0.1161069444170876042, 0.3999999999999995781, 2.220360628129161906 ) ) ;
#23742 = ORIENTED_EDGE ( 'NONE', *, *, #63225, .F. ) ;
#23743 =( BOUNDED_CURVE ( )  B_SPLINE_CURVE ( 3, ( #73854, #27470, #39831, #18729 ),
 .UNSPECIFIED., .F., .F. ) 
 B_SPLINE_CURVE_WITH_KNOTS ( ( 4, 4 ),
 ( 5.143245962375958769, 6.645403452391247079 ),
 .UNSPECIFIED. ) 
 CURVE ( )  GEOMETRIC_REPRESENTATION_ITEM ( )  RATIONAL_B_SPLINE_CURVE ( ( 1.000000000000000000, 0.8206354192515226131, 0.8206354192515226131, 1.000000000000000000 ) ) 
 REPRESENTATION_ITEM ( '' )  );
#23744 = VERTEX_POINT ( 'NONE', #92754 ) ;
#23745 = VECTOR ( 'NONE', #3838, 1000.000000000000000 ) ;
#23746 = LINE ( 'NONE', #68013, #72333 ) ;
#23747 = ORIENTED_EDGE ( 'NONE', *, *, #25486, .F. ) ;
#23748 = CARTESIAN_POINT ( 'NONE',  ( 94.93793019189810423, -6.110000000000001208, 1.637169565754158951 ) ) ;
#23749 = LINE ( 'NONE', #89711, #61629 ) ;
#23750 = LINE ( 'NONE', #2688, #115730 ) ;
#23751 =( GEOMETRIC_REPRESENTATION_CONTEXT ( 3 ) GLOBAL_UNCERTAINTY_ASSIGNED_CONTEXT ( ( #54918 ) ) GLOBAL_UNIT_ASSIGNED_CONTEXT ( ( #50873, #60342, #64599 ) ) REPRESENTATION_CONTEXT ( 'NONE', 'WORKASPACE' ) );
#23752 = EDGE_CURVE ( 'NONE', #97758, #116142, #38397, .T. ) ;
#23754 = AXIS2_PLACEMENT_3D ( 'NONE', #10347, #11038, #11766 ) ;
#23753 = LINE ( 'NONE', #68020, #7579 ) ;
#23755 = COLOUR_RGB ( '', 0.31764706, 0.68627451, 0.89019608) ;
#23756 = CARTESIAN_POINT ( 'NONE',  ( 32.99999999999977973, 20.96639925780204905, 5.000000000000000000 ) ) ;
#23757 = EDGE_LOOP ( 'NONE', ( #112666, #125837, #18940, #79920 ) ) ;
#23758 = CARTESIAN_POINT ( 'NONE',  ( -12.29974487139158512, -27.71228299555214747, 4.000000000000000000 ) ) ;
#23759 = PLANE ( 'NONE',  #115983 ) ;
#23760 = CARTESIAN_POINT ( 'NONE',  ( -17.27718569542927796, -21.72500000000000142, 5.000000000000000000 ) ) ;
#23761 = ORIENTED_EDGE ( 'NONE', *, *, #117550, .F. ) ;
#23762 = CARTESIAN_POINT ( 'NONE',  ( -69.48921356237309510, -27.52281430457103895, 5.000000000000000000 ) ) ;
#23765 = VERTEX_POINT ( 'NONE', #113809 ) ;
#23764 = EDGE_CURVE ( 'NONE', #97802, #118711, #57322, .T. ) ;
#23763 = DIRECTION ( 'NONE',  ( -0.000000000000000000, 0.3543493200069153248, 0.9351131265310292928 ) ) ;
#23766 = SURFACE_STYLE_USAGE ( .BOTH. , #10706 ) ;
#23767 = ADVANCED_FACE ( 'NONE', ( #4999 ), #25362, .T. ) ;
#23768 = CARTESIAN_POINT ( 'NONE',  ( 101.2875270504628986, 0.000000000000000000, -7.949999999999998401 ) ) ;
#23769 = DIRECTION ( 'NONE',  ( -0.7071067811865486830, -0.7071067811865464625, 0.000000000000000000 ) ) ;
#23770 = CARTESIAN_POINT ( 'NONE',  ( -54.18398860626899705, 28.73617430169825226, 5.000000000000000000 ) ) ;
#23771 = LINE ( 'NONE', #10711, #23678 ) ;
#23772 = ORIENTED_EDGE ( 'NONE', *, *, #107140, .F. ) ;
#23773 = EDGE_CURVE ( 'NONE', #76159, #103631, #104618, .T. ) ;
#23774 = VERTEX_POINT ( 'NONE', #137722 ) ;
#23775 = ORIENTED_EDGE ( 'NONE', *, *, #31725, .T. ) ;
#23776 = CARTESIAN_POINT ( 'NONE',  ( 93.47959685856474721, 6.109999999999999432, 1.637169565754164280 ) ) ;
#23777 = VECTOR ( 'NONE', #2463, 999.9999999999998863 ) ;
#23778 = ORIENTED_EDGE ( 'NONE', *, *, #9826, .F. ) ;
#23779 = CARTESIAN_POINT ( 'NONE',  ( -3.707106781186512823, -9.740707523384184441, 5.000000000000000000 ) ) ;
#23780 = CARTESIAN_POINT ( 'NONE',  ( 14.27159235450332098, 3.061616997868378211E-16, -2.500000000000001332 ) ) ;
#23781 = CARTESIAN_POINT ( 'NONE',  ( 26.99999999999981171, 2.342191155542478587, -5.001666872980147893 ) ) ;
#23782 = DIRECTION ( 'NONE',  ( -0.6830127018922181881, 0.6830127018922202975, -0.2588190451025214056 ) ) ;
#23783 = VERTEX_POINT ( 'NONE', #90653 ) ;
#23784 = CARTESIAN_POINT ( 'NONE',  ( 103.2291666666666714, 7.950000000000001954, -2.130196079827421762 ) ) ;
#23785 = DIRECTION ( 'NONE',  ( -0.6830127018922180770, -0.6830127018922204085, -0.2588190451025213501 ) ) ;
#23786 = CIRCLE ( 'NONE', #46914, 2.999999999999999112 ) ;
#23787 = CARTESIAN_POINT ( 'NONE',  ( -17.16347128873440298, 15.75929247661555799, 9.299976744542879814 ) ) ;
#23788 = CARTESIAN_POINT ( 'NONE',  ( 84.34959685856478018, 6.109999999999996767, 1.637169565754163836 ) ) ;
#23789 = ORIENTED_EDGE ( 'NONE', *, *, #55586, .T. ) ;
#23790 =( GEOMETRIC_REPRESENTATION_CONTEXT ( 3 ) GLOBAL_UNCERTAINTY_ASSIGNED_CONTEXT ( ( #98274 ) ) GLOBAL_UNIT_ASSIGNED_CONTEXT ( ( #2621, #4718, #3328 ) ) REPRESENTATION_CONTEXT ( 'NONE', 'WORKASPACE' ) );
#23791 = CARTESIAN_POINT ( 'NONE',  ( 42.29974487139158157, -27.71228299555235708, 4.000000000000000000 ) ) ;
#23793 = AXIS2_PLACEMENT_3D ( 'NONE', #62645, #32143, #98811 ) ;
#23792 = CARTESIAN_POINT ( 'NONE',  ( -12.48921356237309155, -27.52281430457064104, 5.000000000000000000 ) ) ;
#23794 = ORIENTED_EDGE ( 'NONE', *, *, #10112, .F. ) ;
#23795 = EDGE_LOOP ( 'NONE', ( #12849, #103597, #54630, #64230, #7410 ) ) ;
#23796 = DIRECTION ( 'NONE',  ( -0.000000000000000000, 0.000000000000000000, 1.000000000000000000 ) ) ;
#23797 = CARTESIAN_POINT ( 'NONE',  ( -20.99999999999984368, -4.447814304570784749, 5.000000000000000000 ) ) ;
#23798 = CARTESIAN_POINT ( 'NONE',  ( 20.62956980810188412, -3.967499999999998028, -6.871911579029511330 ) ) ;
#23799 = LINE ( 'NONE', #1987, #104449 ) ;
#23800 = LINE ( 'NONE', #113646, #89578 ) ;
#23801 = CARTESIAN_POINT ( 'NONE',  ( 4.499999999999965361, 15.43112307739203182, 4.000000000000000000 ) ) ;
#23802 = CARTESIAN_POINT ( 'NONE',  ( -34.82816939922327748, 15.75929247661556332, 4.000000000000000000 ) ) ;
#23803 = FILL_AREA_STYLE_COLOUR ( '', #63104 ) ;
#23804 = ORIENTED_EDGE ( 'NONE', *, *, #137652, .F. ) ;
#23805 = ORIENTED_EDGE ( 'NONE', *, *, #73933, .T. ) ;
#23806 = CARTESIAN_POINT ( 'NONE',  ( 10.35416666666666607, 1.633150327867685103, 6.094999999999992646 ) ) ;
#23807 = VERTEX_POINT ( 'NONE', #91373 ) ;
#23808 = ADVANCED_FACE ( 'NONE', ( #47190 ), #35582, .F. ) ;
#23809 = ORIENTED_EDGE ( 'NONE', *, *, #14061, .F. ) ;
#23810 = AXIS2_PLACEMENT_3D ( 'NONE', #49514, #15375, #61799 ) ;
#23811 = AXIS2_PLACEMENT_3D ( 'NONE', #130928, #18531, #141049 ) ;
#23812 = FACE_OUTER_BOUND ( 'NONE', #122641, .T. ) ;
#23813 = ORIENTED_EDGE ( 'NONE', *, *, #77932, .T. ) ;
#23814 = PLANE ( 'NONE',  #11197 ) ;
#23815 = LINE ( 'NONE', #14360, #47192 ) ;
#23816 = B_SPLINE_CURVE_WITH_KNOTS ( 'NONE', 3,
 ( #105595, #59994, #92585, #136822 ),
 .UNSPECIFIED., .F., .F.,
 ( 4, 4 ),
 ( 0.000000000000000000, 0.001115544020566860712 ),
 .UNSPECIFIED. ) ;
#23817 = DIRECTION ( 'NONE',  ( -0.7071067811865487940, 0.7071067811865463515, -0.000000000000000000 ) ) ;
#23818 = VECTOR ( 'NONE', #116503, 1000.000000000000000 ) ;
#23819 = CARTESIAN_POINT ( 'NONE',  ( -15.48921356237309510, -27.52281430457066236, 5.000000000000000000 ) ) ;
#23820 = ORIENTED_EDGE ( 'NONE', *, *, #20725, .T. ) ;
#23821 = DIRECTION ( 'NONE',  ( 0.7071067811865486830, -0.7071067811865464625, -0.000000000000000000 ) ) ;
#23822 = ORIENTED_EDGE ( 'NONE', *, *, #97081, .F. ) ;
#23823 = ADVANCED_FACE ( 'NONE', ( #134886 ), #126125, .F. ) ;
#23824 = DIRECTION ( 'NONE',  ( 0.000000000000000000, 0.000000000000000000, -1.000000000000000000 ) ) ;
#23825 = ORIENTED_EDGE ( 'NONE', *, *, #38940, .T. ) ;
#23826 = DIRECTION ( 'NONE',  ( -0.000000000000000000, 0.000000000000000000, 1.000000000000000000 ) ) ;
#23827 = ORIENTED_EDGE ( 'NONE', *, *, #11058, .T. ) ;
#23829 = EDGE_CURVE ( 'NONE', #20167, #103522, #26799, .T. ) ;
#23828 = DIRECTION ( 'NONE',  ( 0.7071067811865486830, -0.7071067811865464625, -0.000000000000000000 ) ) ;
#23830 = VERTEX_POINT ( 'NONE', #135584 ) ;
#23831 = VERTEX_POINT ( 'NONE', #58780 ) ;
#23832 = COLOUR_RGB ( '', 0.31764706, 0.68627451, 0.89019608) ;
#23833 = VERTEX_POINT ( 'NONE', #93488 ) ;
#23834 = CARTESIAN_POINT ( 'NONE',  ( 6.639999999999984581, -40.29840020119762301, 19.55137198191483350 ) ) ;
#23835 = DIRECTION ( 'NONE',  ( 0.000000000000000000, -1.000000000000000000, 0.000000000000000000 ) ) ;
#23836 = DIRECTION ( 'NONE',  ( 0.7071067811865487940, 0.7071067811865463515, 0.000000000000000000 ) ) ;
#23837 = CARTESIAN_POINT ( 'NONE',  ( 114.1879301918981042, 6.110000000000002984, -1.637169565754156730 ) ) ;
#23838 = DIRECTION ( 'NONE',  ( 0.3543493200069162685, -0.000000000000000000, -0.9351131265310288487 ) ) ;
#23839 = EDGE_CURVE ( 'NONE', #98820, #106359, #102944, .T. ) ;
#23840 = DIRECTION ( 'NONE',  ( 0.7071067811865486830, -0.7071067811865464625, -0.000000000000000000 ) ) ;
#23841 = PLANE ( 'NONE',  #29684 ) ;
#23842 = AXIS2_PLACEMENT_3D ( 'NONE', #126383, #94464, #138717 ) ;
#23843 = DIRECTION ( 'NONE',  ( -0.6830127018922181881, 0.6830127018922202975, -0.2588190451025214056 ) ) ;
#23844 = VECTOR ( 'NONE', #81304, 1000.000000000000227 ) ;
#23845 = ADVANCED_FACE ( 'NONE', ( #126805 ), #68217, .T. ) ;
#23846 = VECTOR ( 'NONE', #2771, 1000.000000000000227 ) ;
#23847 = DIRECTION ( 'NONE',  ( 0.000000000000000000, -1.000000000000000000, 0.000000000000000000 ) ) ;
#23848 = ORIENTED_EDGE ( 'NONE', *, *, #9039, .T. ) ;
#23849 = CARTESIAN_POINT ( 'NONE',  ( -11.99999999999992006, 7.007997736742436423, -8.085015511992141413 ) ) ;
#23850 = LINE ( 'NONE', #12942, #47629 ) ;
#23851 = CARTESIAN_POINT ( 'NONE',  ( -30.29974487139158867, -27.71228299555227537, 4.000000000000000000 ) ) ;
#23852 = ORIENTED_EDGE ( 'NONE', *, *, #38303, .F. ) ;
#23853 = ORIENTED_EDGE ( 'NONE', *, *, #26376, .T. ) ;
#23854 = VECTOR ( 'NONE', #107115, 1000.000000000000000 ) ;
#23855 = AXIS2_PLACEMENT_3D ( 'NONE', #12730, #122942, #70031 ) ;
#23856 = CARTESIAN_POINT ( 'NONE',  ( 8.031592354503320763, -2.500000000000000000, 3.061616997868384127E-16 ) ) ;
#23857 = ADVANCED_FACE ( 'NONE', ( #112394 ), #13753, .F. ) ;
#23858 = ORIENTED_EDGE ( 'NONE', *, *, #9643, .F. ) ;
#23859 = ORIENTED_EDGE ( 'NONE', *, *, #50507, .F. ) ;
#23860 = CARTESIAN_POINT ( 'NONE',  ( -28.49999999999980815, -4.796895815301044586, -3.611700055028748579 ) ) ;
#23861 = CARTESIAN_POINT ( 'NONE',  ( 13.46247294953710494, -7.464222240803106570E-16, -6.094999999999989981 ) ) ;
#23862 = CARTESIAN_POINT ( 'NONE',  ( 0.000000000000000000, 0.000000000000000000, 5.000000000000000000 ) ) ;
#23863 = DIRECTION ( 'NONE',  ( -0.7071067811865487940, 0.7071067811865463515, -0.000000000000000000 ) ) ;
#23864 = ORIENTED_EDGE ( 'NONE', *, *, #59219, .T. ) ;
#23865 = CARTESIAN_POINT ( 'NONE',  ( 0.2569208697893817228, -2.055000000000000160, 0.000000000000000000 ) ) ;
#23866 = ORIENTED_EDGE ( 'NONE', *, *, #66290, .F. ) ;
#23867 = LINE ( 'NONE', #68821, #12131 ) ;
#23868 = VECTOR ( 'NONE', #40836, 999.9999999999998863 ) ;
#23869 = CARTESIAN_POINT ( 'NONE',  ( 21.21290314143522338, 3.967499999999992699, -6.871911579029513994 ) ) ;
#23870 = ORIENTED_EDGE ( 'NONE', *, *, #109184, .T. ) ;
#23871 = CARTESIAN_POINT ( 'NONE',  ( 82.01626352523142316, -4.472830434245839371, 4.472830434245839371 ) ) ;
#23872 = CARTESIAN_POINT ( 'NONE',  ( 3.250000000000000000, 0.000000000000000000, 0.000000000000000000 ) ) ;
#23873 = DIRECTION ( 'NONE',  ( -0.7071067811865486830, -0.7071067811865464625, 0.000000000000000000 ) ) ;
#23874 = VERTEX_POINT ( 'NONE', #92043 ) ;
#23875 = ADVANCED_FACE ( 'NONE', ( #36956 ), #26098, .F. ) ;
#23876 = ORIENTED_EDGE ( 'NONE', *, *, #102805, .F. ) ;
#23877 = ORIENTED_EDGE ( 'NONE', *, *, #82813, .F. ) ;
#23878 = CARTESIAN_POINT ( 'NONE',  ( 72.48921356237309510, -27.52281430457106026, 5.000000000000000000 ) ) ;
#23879 = CARTESIAN_POINT ( 'NONE',  ( 0.000000000000000000, 0.000000000000000000, 5.000000000000000000 ) ) ;
#23880 = CARTESIAN_POINT ( 'NONE',  ( -27.51665438641025574, 22.22500000000000142, 4.500000000000000888 ) ) ;
#23881 = CARTESIAN_POINT ( 'NONE',  ( -42.18398860626899705, 28.73617430169816700, 5.000000000000000000 ) ) ;
#23882 = DIRECTION ( 'NONE',  ( 0.7071067811865486830, -0.7071067811865464625, -0.000000000000000000 ) ) ;
#23883 = ORIENTED_EDGE ( 'NONE', *, *, #122040, .F. ) ;
#23884 = VECTOR ( 'NONE', #55056, 1000.000000000000000 ) ;
#23885 = EDGE_CURVE ( 'NONE', #121977, #27100, #27490, .T. ) ;
#23886 = EDGE_CURVE ( 'NONE', #94004, #125681, #5249, .T. ) ;
#23887 = DIRECTION ( 'NONE',  ( 0.7071067811865487940, 0.7071067811865463515, 0.000000000000000000 ) ) ;
#23888 = PRESENTATION_LAYER_ASSIGNMENT (  '', '', ( #58615 ) ) ;
#23889 = DIRECTION ( 'NONE',  ( 0.7071067811865487940, 0.7071067811865463515, -0.000000000000000000 ) ) ;
#23890 = DIRECTION ( 'NONE',  ( -1.000000000000000000, -1.224606353822377258E-16, -0.000000000000000000 ) ) ;
#23891 = ORIENTED_EDGE ( 'NONE', *, *, #43145, .F. ) ;
#23892 = DIRECTION ( 'NONE',  ( -1.000000000000000000, -0.000000000000000000, -0.000000000000000000 ) ) ;
#23894 = ADVANCED_FACE ( 'NONE', ( #139149 ), #52117, .T. ) ;
#23893 = DIRECTION ( 'NONE',  ( 0.7071067811865487940, -0.7071067811865463515, 0.000000000000000000 ) ) ;
#23895 = ORIENTED_EDGE ( 'NONE', *, *, #8974, .F. ) ;
#23896 = VECTOR ( 'NONE', #112824, 1000.000000000000227 ) ;
#23898 = ORIENTED_EDGE ( 'NONE', *, *, #107842, .T. ) ;
#23897 =( NAMED_UNIT ( * ) SI_UNIT ( $, .STERADIAN. ) SOLID_ANGLE_UNIT ( ) );
#23900 = ORIENTED_EDGE ( 'NONE', *, *, #35720, .T. ) ;
#23899 = EDGE_CURVE ( 'NONE', #128651, #87872, #139871, .T. ) ;
#23901 = ADVANCED_FACE ( 'NONE', ( #96300 ), #72495, .F. ) ;
#23902 = DIRECTION ( 'NONE',  ( -0.7071067811865486830, 0.7071067811865464625, 0.000000000000000000 ) ) ;
#23903 = CARTESIAN_POINT ( 'NONE',  ( -1.499999999999989120, 18.05218569542898521, 5.000000000000000000 ) ) ;
#23904 = VERTEX_POINT ( 'NONE', #128268 ) ;
#23905 = CARTESIAN_POINT ( 'NONE',  ( 5.999999999999956479, 12.83542986846997813, -1.025386466790383810 ) ) ;
#23906 = ORIENTED_EDGE ( 'NONE', *, *, #23829, .F. ) ;
#23907 = VECTOR ( 'NONE', #113020, 1000.000000000000227 ) ;
#23908 = CARTESIAN_POINT ( 'NONE',  ( -10.17183060077639389, -8.240707523384200428, 4.000000000000000000 ) ) ;
#23909 = CARTESIAN_POINT ( 'NONE',  ( -63.18398860626900415, 28.73617430169831621, 5.000000000000000000 ) ) ;
#23911 = VECTOR ( 'NONE', #66332, 1000.000000000000000 ) ;
#23910 = DIRECTION ( 'NONE',  ( -0.7071067811865486830, 0.7071067811865464625, -0.000000000000000000 ) ) ;
#23912 = ADVANCED_FACE ( 'NONE', ( #94885 ), #7879, .F. ) ;
#23913 = CARTESIAN_POINT ( 'NONE',  ( 47.18336038379622721, -2.130196079827426203, 7.949999999999996625 ) ) ;
#23914 = FACE_OUTER_BOUND ( 'NONE', #6668, .T. ) ;
#23915 = FACE_OUTER_BOUND ( 'NONE', #29153, .T. ) ;
#23916 = CARTESIAN_POINT ( 'NONE',  ( 13.49999999999991473, 1.030536316426525989, -5.498701923753829490 ) ) ;
#23917 = FACE_OUTER_BOUND ( 'NONE', #97376, .T. ) ;
#23918 = CARTESIAN_POINT ( 'NONE',  ( 21.41623647476855652, -7.934999999999990727, 4.858786175617117713E-16 ) ) ;
#23919 = CARTESIAN_POINT ( 'NONE',  ( 0.4162364747685527444, -7.934999999999990727, 4.858786175617117713E-16 ) ) ;
#23920 = VECTOR ( 'NONE', #35905, 1000.000000000000000 ) ;
#23921 = PLANE ( 'NONE',  #6564 ) ;
#23922 = EDGE_CURVE ( 'NONE', #29089, #2906, #86182, .T. ) ;
#23923 = CARTESIAN_POINT ( 'NONE',  ( -14.29289321881335439, 17.25929247661554200, 5.000000000000000000 ) ) ;
#23924 = PLANE ( 'NONE',  #75545 ) ;
#23925 = VERTEX_POINT ( 'NONE', #39849 ) ;
#23926 = EDGE_LOOP ( 'NONE', ( #347, #130375, #132994, #47429 ) ) ;
#23927 = CARTESIAN_POINT ( 'NONE',  ( 92.72916666666664298, 7.950000000000001954, -2.130196079827421762 ) ) ;
#23928 = VERTEX_POINT ( 'NONE', #71756 ) ;
#23929 = EDGE_LOOP ( 'NONE', ( #98168, #32572, #31518, #56574 ) ) ;
#23930 = ORIENTED_EDGE ( 'NONE', *, *, #42551, .T. ) ;
#23931 = CARTESIAN_POINT ( 'NONE',  ( 12.40000000000000213, 9.521314400968980422E-16, 0.000000000000000000 ) ) ;
#23932 = DIRECTION ( 'NONE',  ( -0.3543493200069162685, -0.000000000000000000, -0.9351131265310288487 ) ) ;
#23933 = VECTOR ( 'NONE', #25083, 1000.000000000000000 ) ;
#23934 = PLANE ( 'NONE',  #75535 ) ;
#23935 = VERTEX_POINT ( 'NONE', #62299 ) ;
#23936 = FACE_OUTER_BOUND ( 'NONE', #85454, .T. ) ;
#23937 = CARTESIAN_POINT ( 'NONE',  ( -30.79289321881324071, -14.24070752338413826, 5.000000000000000000 ) ) ;
#23938 = CARTESIAN_POINT ( 'NONE',  ( -34.92500000000001137, 22.22500000000000142, 4.000000000000000000 ) ) ;
#23939 = DIRECTION ( 'NONE',  ( 0.000000000000000000, -1.000000000000000000, 0.000000000000000000 ) ) ;
#23940 = VERTEX_POINT ( 'NONE', #63027 ) ;
#23941 = DIRECTION ( 'NONE',  ( 1.000000000000000000, 0.000000000000000000, 0.000000000000000000 ) ) ;
#23942 = DIRECTION ( 'NONE',  ( -0.6830127018922181881, 0.6830127018922202975, -0.2588190451025214056 ) ) ;
#23944 = VECTOR ( 'NONE', #30918, 1000.000000000000000 ) ;
#23943 = DIRECTION ( 'NONE',  ( -0.6830127018922181881, 0.6830127018922202975, -0.2588190451025214056 ) ) ;
#23945 = CARTESIAN_POINT ( 'NONE',  ( 26.99999999999998579, 4.092321363584886740, 6.547056572790977746 ) ) ;
#23946 = CARTESIAN_POINT ( 'NONE',  ( 8.811592354503320124, 3.061616997868378211E-16, -2.500000000000001332 ) ) ;
#23947 = FACE_OUTER_BOUND ( 'NONE', #24959, .T. ) ;
#23948 = DIRECTION ( 'NONE',  ( -1.000000000000000000, -0.000000000000000000, -0.000000000000000000 ) ) ;
#23949 = DIRECTION ( 'NONE',  ( 0.6830127018922181881, 0.6830127018922202975, -0.2588190451025214056 ) ) ;
#23950 = EDGE_CURVE ( 'NONE', #59256, #67860, #106459, .T. ) ;
#23951 = EDGE_CURVE ( 'NONE', #16172, #104226, #127538, .T. ) ;
#23952 = ORIENTED_EDGE ( 'NONE', *, *, #121994, .T. ) ;
#23953 = ORIENTED_EDGE ( 'NONE', *, *, #115671, .F. ) ;
#23954 = CARTESIAN_POINT ( 'NONE',  ( 124.1045968585647756, 1.637169565754164946, -6.109999999999999432 ) ) ;
#23955 = ORIENTED_EDGE ( 'NONE', *, *, #24429, .F. ) ;
#23956 = DIRECTION ( 'NONE',  ( -0.7071067811865486830, 0.7071067811865464625, 0.000000000000000000 ) ) ;
#23957 = VECTOR ( 'NONE', #39965, 1000.000000000000000 ) ;
#23958 = DIRECTION ( 'NONE',  ( -0.7071067811865487940, 0.7071067811865463515, -0.000000000000000000 ) ) ;
#23959 = DIRECTION ( 'NONE',  ( 0.000000000000000000, 1.000000000000000000, 0.000000000000000000 ) ) ;
#23960 = PLANE ( 'NONE',  #125270 ) ;
#23961 = CARTESIAN_POINT ( 'NONE',  ( 115.9954301918981230, 5.291415217122916737, 3.055000000000001936 ) ) ;
#23962 = VERTEX_POINT ( 'NONE', #105753 ) ;
#23963 = VERTEX_POINT ( 'NONE', #41232 ) ;
#23964 = VECTOR ( 'NONE', #128534, 1000.000000000000000 ) ;
#23965 = DIRECTION ( 'NONE',  ( 0.7071067811865487940, 0.7071067811865463515, 0.000000000000000000 ) ) ;
#23966 = ORIENTED_EDGE ( 'NONE', *, *, #42956, .F. ) ;
#23967 = ORIENTED_EDGE ( 'NONE', *, *, #79843, .F. ) ;
#23968 = ORIENTED_EDGE ( 'NONE', *, *, #100533, .F. ) ;
#23969 = CARTESIAN_POINT ( 'NONE',  ( -11.99999999999991651, -16.60178936734449806, 0.8616154019347220805 ) ) ;
#23970 = SURFACE_STYLE_FILL_AREA ( #47892 ) ;
#23971 = AXIS2_PLACEMENT_3D ( 'NONE', #91918, #53795, #65395 ) ;
#23972 = AXIS2_PLACEMENT_3D ( 'NONE', #4952, #48509, #92711 ) ;
#23973 = CARTESIAN_POINT ( 'NONE',  ( 28.34959685856477662, 6.109999999999996767, 1.637169565754163836 ) ) ;
#23974 = ORIENTED_EDGE ( 'NONE', *, *, #2211, .T. ) ;
#23975 = EDGE_LOOP ( 'NONE', ( #59627, #125479, #68697, #16819 ) ) ;
#23976 = CARTESIAN_POINT ( 'NONE',  ( -24.18398860626899705, 28.73617430169804265, 5.000000000000000000 ) ) ;
#23977 = ORIENTED_EDGE ( 'NONE', *, *, #121392, .F. ) ;
#23978 = VERTEX_POINT ( 'NONE', #28233 ) ;
#23979 = ORIENTED_EDGE ( 'NONE', *, *, #80572, .F. ) ;
#23980 = VECTOR ( 'NONE', #99606, 1000.000000000000000 ) ;
#23981 = DIRECTION ( 'NONE',  ( -0.000000000000000000, -0.000000000000000000, 1.000000000000000000 ) ) ;
#23982 = DIRECTION ( 'NONE',  ( 0.000000000000000000, 0.9647414015272168797, -0.2631995976047484254 ) ) ;
#23983 = ORIENTED_EDGE ( 'NONE', *, *, #97510, .F. ) ;
#23984 = AXIS2_PLACEMENT_3D ( 'NONE', #47902, #136297, #71074 ) ;
#23985 = DIRECTION ( 'NONE',  ( -0.7071067811865486830, -0.7071067811865464625, -0.000000000000000000 ) ) ;
#23986 = CARTESIAN_POINT ( 'NONE',  ( 36.18398860626899705, 28.73617430169812437, 5.000000000000000000 ) ) ;
#23987 = FILL_AREA_STYLE_COLOUR ( '', #120063 ) ;
#23988 = VECTOR ( 'NONE', #57598, 1000.000000000000000 ) ;
#23989 = EDGE_CURVE ( 'NONE', #4323, #86268, #51422, .T. ) ;
#23990 = FACE_BOUND ( 'NONE', #86776, .T. ) ;
#23991 = ORIENTED_EDGE ( 'NONE', *, *, #126923, .F. ) ;
#23992 = FACE_OUTER_BOUND ( 'NONE', #74875, .T. ) ;
#23993 = EDGE_CURVE ( 'NONE', #128576, #36198, #118795, .T. ) ;
#23995 = ADVANCED_FACE ( 'NONE', ( #63735 ), #132501, .T. ) ;
#23994 = CARTESIAN_POINT ( 'NONE',  ( 0.000000000000000000, 0.000000000000000000, 5.000000000000000000 ) ) ;
#23996 = CARTESIAN_POINT ( 'NONE',  ( 20.99451991528748707, 28.92564299267952777, 4.000000000000000000 ) ) ;
#23997 = DIRECTION ( 'NONE',  ( -0.7071067811865487940, 0.7071067811865463515, -0.000000000000000000 ) ) ;
#23998 = VERTEX_POINT ( 'NONE', #141257 ) ;
#23999 = DIRECTION ( 'NONE',  ( -0.7071067811865486830, -0.7071067811865464625, 0.000000000000000000 ) ) ;
#24000 = ORIENTED_EDGE ( 'NONE', *, *, #9486, .F. ) ;
#24001 = ORIENTED_EDGE ( 'NONE', *, *, #94727, .F. ) ;
#24002 = ORIENTED_EDGE ( 'NONE', *, *, #43553, .T. ) ;
#24004 = EDGE_CURVE ( 'NONE', #81446, #19388, #41968, .T. ) ;
#24003 = AXIS2_PLACEMENT_3D ( 'NONE', #17046, #70740, #38800 ) ;
#24005 = EDGE_CURVE ( 'NONE', #98543, #69474, #98478, .T. ) ;
#24006 = CARTESIAN_POINT ( 'NONE',  ( 47.01626352523143737, -4.472830434245838482, 4.472830434245838482 ) ) ;
#24008 = ORIENTED_EDGE ( 'NONE', *, *, #51351, .F. ) ;
#24007 = CIRCLE ( 'NONE', #86524, 2.500000000000000888 ) ;
#24009 = DIRECTION ( 'NONE',  ( 0.6830127018922180770, -0.6830127018922204085, -0.2588190451025213501 ) ) ;
#24010 = CARTESIAN_POINT ( 'NONE',  ( -26.18650864602345507, -15.74070752338411694, 8.904080028139002678 ) ) ;
#24011 = EDGE_CURVE ( 'NONE', #138592, #672, #78340, .T. ) ;
#24012 = ORIENTED_EDGE ( 'NONE', *, *, #142972, .F. ) ;
#24013 = CARTESIAN_POINT ( 'NONE',  ( -34.42500000000001137, -10.45860074219788416, 5.000000000000000000 ) ) ;
#24014 = STYLED_ITEM ( 'NONE', ( #76738 ), #32375 ) ;
#24015 = EDGE_CURVE ( 'NONE', #58244, #113958, #132578, .T. ) ;
#24016 = DIRECTION ( 'NONE',  ( -1.000000000000000000, -1.224606353822377258E-16, -0.000000000000000000 ) ) ;
#24017 = DIRECTION ( 'NONE',  ( 0.7071067811865487940, 0.7071067811865463515, -0.000000000000000000 ) ) ;
#24018 = DIRECTION ( 'NONE',  ( -0.000000000000000000, 1.000000000000000000, 0.000000000000000000 ) ) ;
#24019 = CARTESIAN_POINT ( 'NONE',  ( 30.70710678118633652, -6.740707523384211086, 5.000000000000000000 ) ) ;
#24020 = ORIENTED_EDGE ( 'NONE', *, *, #26078, .F. ) ;
#24021 = ORIENTED_EDGE ( 'NONE', *, *, #124420, .T. ) ;
#24023 = ORIENTED_EDGE ( 'NONE', *, *, #130808, .T. ) ;
#24022 = VECTOR ( 'NONE', #43838, 999.9999999999998863 ) ;
#24024 = VERTEX_POINT ( 'NONE', #54297 ) ;
#24025 = DIRECTION ( 'NONE',  ( -0.7071067811865487940, 0.7071067811865463515, -0.000000000000000000 ) ) ;
#24026 = ADVANCED_FACE ( 'NONE', ( #43395 ), #97762, .F. ) ;
#24027 = EDGE_LOOP ( 'NONE', ( #80558, #123746, #94746, #141359 ) ) ;
#24028 = ORIENTED_EDGE ( 'NONE', *, *, #22971, .T. ) ;
#24029 = CARTESIAN_POINT ( 'NONE',  ( -30.47512612785027031, 14.25929247661557397, 9.797011795316567628 ) ) ;
#24030 = DIRECTION ( 'NONE',  ( 1.000000000000000000, 0.000000000000000000, 0.000000000000000000 ) ) ;
#24031 = VECTOR ( 'NONE', #138431, 999.9999999999998863 ) ;
#24032 = ORIENTED_EDGE ( 'NONE', *, *, #57447, .F. ) ;
#24033 = LINE ( 'NONE', #45111, #34811 ) ;
#24034 = EDGE_CURVE ( 'NONE', #90786, #71989, #33957, .T. ) ;
#24035 = DIRECTION ( 'NONE',  ( -0.7071067811865487940, 0.7071067811865463515, 0.000000000000000000 ) ) ;
#24036 = CARTESIAN_POINT ( 'NONE',  ( 23.10873647476855552, -5.808823158059033709, 5.808823158059035485 ) ) ;
#24037 = CARTESIAN_POINT ( 'NONE',  ( -27.48921356237309155, -27.52281430457074762, 5.000000000000000000 ) ) ;
#24038 = ORIENTED_EDGE ( 'NONE', *, *, #76899, .F. ) ;
#24040 = DIRECTION ( 'NONE',  ( -0.000000000000000000, 0.000000000000000000, 1.000000000000000000 ) ) ;
#24039 = CARTESIAN_POINT ( 'NONE',  ( 106.3704301918981230, -3.055000000000001936, 5.291415217122918513 ) ) ;
#24041 = DIRECTION ( 'NONE',  ( -0.6830127018922181881, 0.6830127018922202975, -0.2588190451025214056 ) ) ;
#24042 = LINE ( 'NONE', #90745, #97505 ) ;
#24043 = ADVANCED_FACE ( 'NONE', ( #22310 ), #76759, .F. ) ;
#24044 = ORIENTED_EDGE ( 'NONE', *, *, #65956, .F. ) ;
#24045 = LINE ( 'NONE', #55249, #10215 ) ;
#24047 = EDGE_LOOP ( 'NONE', ( #137875, #80734, #38618, #42768 ) ) ;
#24046 = FACE_OUTER_BOUND ( 'NONE', #72030, .T. ) ;
#24048 = DIRECTION ( 'NONE',  ( -0.000000000000000000, -0.3543493200069152693, 0.9351131265310292928 ) ) ;
#24049 = VERTEX_POINT ( 'NONE', #143407 ) ;
#24050 = PLANE ( 'NONE',  #128430 ) ;
#24051 = CARTESIAN_POINT ( 'NONE',  ( -18.00548008471250583, 28.92564299267925776, 4.000000000000000000 ) ) ;
#24052 = DIRECTION ( 'NONE',  ( 0.7071067811865486830, -0.7071067811865464625, -0.000000000000000000 ) ) ;
#24054 = EDGE_LOOP ( 'NONE', ( #99732, #66513, #110720, #72403, #63448, #106302 ) ) ;
#24053 = AXIS2_PLACEMENT_3D ( 'NONE', #15727, #49152, #5597 ) ;
#24055 = EDGE_CURVE ( 'NONE', #135397, #46535, #31099, .T. ) ;
#24056 = CARTESIAN_POINT ( 'NONE',  ( 56.09683561313698874, -51.20434817233912383, 36.87500513592860329 ) ) ;
#24057 = EDGE_CURVE ( 'NONE', #102448, #93966, #45569, .T. ) ;
#24058 = CARTESIAN_POINT ( 'NONE',  ( 26.99999999999981526, -16.60178936734445543, 0.8616154019348096771 ) ) ;
#24059 = CARTESIAN_POINT ( 'NONE',  ( 1.499999999999997780, 10.08746187583914633, 4.000000000000000000 ) ) ;
#24060 = EDGE_LOOP ( 'NONE', ( #76698, #78115, #20601, #70455 ) ) ;
#24062 = ADVANCED_FACE ( 'NONE', ( #20177 ), #21641, .T. ) ;
#24061 = CARTESIAN_POINT ( 'NONE',  ( -57.18398860626899705, 28.73617430169827358, 5.000000000000000000 ) ) ;
#24063 = VERTEX_POINT ( 'NONE', #86900 ) ;
#24064 = CARTESIAN_POINT ( 'NONE',  ( 25.19159235450331735, 9.902892378096218942E-16, 0.000000000000000000 ) ) ;
#24066 = VERTEX_POINT ( 'NONE', #55711 ) ;
#24065 = DIRECTION ( 'NONE',  ( -1.000000000000000000, -1.224606353822377258E-16, -0.000000000000000000 ) ) ;
#24067 = VERTEX_POINT ( 'NONE', #575 ) ;
#24068 = CARTESIAN_POINT ( 'NONE',  ( 17.69516080050994589, 4.375290223488867980, -29.58855600362791449 ) ) ;
#24069 = CARTESIAN_POINT ( 'NONE',  ( -34.92500000000001137, 22.22500000000000142, 4.000000000000000000 ) ) ;
#24070 = VECTOR ( 'NONE', #119898, 1000.000000000000000 ) ;
#24071 = ORIENTED_EDGE ( 'NONE', *, *, #57413, .F. ) ;
#24072 = CARTESIAN_POINT ( 'NONE',  ( 11.99451991528749417, 28.92564299267946382, 4.000000000000000000 ) ) ;
#24073 = AXIS2_PLACEMENT_3D ( 'NONE', #2307, #122684, #23369 ) ;
#24074 = CARTESIAN_POINT ( 'NONE',  ( 72.18398860626899705, 28.73617430169837661, 5.000000000000000000 ) ) ;
#24075 = PLANE ( 'NONE',  #26018 ) ;
#24076 = ORIENTED_EDGE ( 'NONE', *, *, #89113, .F. ) ;
#24077 = EDGE_CURVE ( 'NONE', #22612, #22841, #133276, .T. ) ;
#24078 = CARTESIAN_POINT ( 'NONE',  ( -21.48921356237309155, -27.52281430457070499, 5.000000000000000000 ) ) ;
#24079 = PLANE ( 'NONE',  #104524 ) ;
#24080 = FACE_OUTER_BOUND ( 'NONE', #140654, .T. ) ;
#24081 = DIRECTION ( 'NONE',  ( 0.6830127018922181881, 0.6830127018922202975, -0.2588190451025214056 ) ) ;
#24082 = CARTESIAN_POINT ( 'NONE',  ( 125.6129489383715736, -4.459058803571000595, 6.473095785633507404 ) ) ;
#24083 = EDGE_CURVE ( 'NONE', #45596, #97154, #30551, .T. ) ;
#24084 = VECTOR ( 'NONE', #92300, 1000.000000000000114 ) ;
#24085 = FACE_OUTER_BOUND ( 'NONE', #51856, .T. ) ;
#24086 = ORIENTED_EDGE ( 'NONE', *, *, #117102, .T. ) ;
#24087 = ORIENTED_EDGE ( 'NONE', *, *, #136770, .T. ) ;
#24088 = ORIENTED_EDGE ( 'NONE', *, *, #82858, .F. ) ;
#24089 = CARTESIAN_POINT ( 'NONE',  ( -25.64175702458845052, 15.75929247661555799, 19.34181609438705607 ) ) ;
#24090 = EDGE_LOOP ( 'NONE', ( #73838, #93627, #101612 ) ) ;
#24091 = VECTOR ( 'NONE', #107306, 999.9999999999998863 ) ;
#24092 = VERTEX_POINT ( 'NONE', #99161 ) ;
#24093 = ORIENTED_EDGE ( 'NONE', *, *, #104016, .F. ) ;
#24094 = LINE ( 'NONE', #111059, #10863 ) ;
#24095 = LINE ( 'NONE', #58920, #57863 ) ;
#24096 = ORIENTED_EDGE ( 'NONE', *, *, #84863, .T. ) ;
#24097 = DIRECTION ( 'NONE',  ( 1.000000000000000000, 1.224606353822377258E-16, 0.000000000000000000 ) ) ;
#24099 = VECTOR ( 'NONE', #111035, 1000.000000000000000 ) ;
#24098 = DIRECTION ( 'NONE',  ( -1.000000000000000000, -0.000000000000000000, -0.000000000000000000 ) ) ;
#24100 = DIRECTION ( 'NONE',  ( 0.7071067811865486830, -0.7071067811865464625, -0.000000000000000000 ) ) ;
#24101 = PRESENTATION_LAYER_ASSIGNMENT (  '', '', ( #112067 ) ) ;
#24102 = CARTESIAN_POINT ( 'NONE',  ( -1.499999999999987566, 5.696342897626511359, -7.587980461218403860 ) ) ;
#24103 = CARTESIAN_POINT ( 'NONE',  ( 125.4170968585647756, 3.054999999999998828, 5.291415217122922066 ) ) ;
#24104 = ORIENTED_EDGE ( 'NONE', *, *, #58313, .T. ) ;
#24105 = EDGE_CURVE ( 'NONE', #107639, #127483, #89056, .T. ) ;
#24106 = DIRECTION ( 'NONE',  ( -0.6830127018922180770, -0.6830127018922204085, -0.2588190451025213501 ) ) ;
#24107 = DIRECTION ( 'NONE',  ( -1.000000000000000000, -0.000000000000000000, -0.000000000000000000 ) ) ;
#24108 = LINE ( 'NONE', #79955, #62183 ) ;
#24109 = CARTESIAN_POINT ( 'NONE',  ( -19.05000000000000071, 3.174999999999997158, 4.000000000000000000 ) ) ;
#24110 = DIRECTION ( 'NONE',  ( -0.000000000000000000, -0.3543493200069152693, 0.9351131265310292928 ) ) ;
#24111 = DIRECTION ( 'NONE',  ( 0.000000000000000000, 1.000000000000000000, -0.000000000000000000 ) ) ;
#24112 = VECTOR ( 'NONE', #68438, 1000.000000000000000 ) ;
#24113 = CARTESIAN_POINT ( 'NONE',  ( 51.26669371712954160, -7.949999999999999289, 2.130196079827424427 ) ) ;
#24114 = FACE_OUTER_BOUND ( 'NONE', #43275, .T. ) ;
#24115 = VECTOR ( 'NONE', #74148, 1000.000000000000227 ) ;
#24116 = DIRECTION ( 'NONE',  ( -0.3543493200069162685, -0.000000000000000000, -0.9351131265310288487 ) ) ;
#24117 = ORIENTED_EDGE ( 'NONE', *, *, #107966, .T. ) ;
#24118 = EDGE_LOOP ( 'NONE', ( #74263, #6428, #30308, #126804 ) ) ;
#24119 = CARTESIAN_POINT ( 'NONE',  ( 47.81249999999999289, 5.819803920172571310, 5.819803920172575751 ) ) ;
#24120 = DIRECTION ( 'NONE',  ( 1.000000000000000000, 0.000000000000000000, 0.000000000000000000 ) ) ;
#24121 = DIRECTION ( 'NONE',  ( -1.734723475976806848E-16, 1.000000000000000000, 0.000000000000000000 ) ) ;
#24122 = ORIENTED_EDGE ( 'NONE', *, *, #26113, .T. ) ;
#24123 = CARTESIAN_POINT ( 'NONE',  ( 30.48921356237309510, -27.52281430457076894, 5.000000000000000000 ) ) ;
#24124 = DIRECTION ( 'NONE',  ( -0.000000000000000000, 0.000000000000000000, 1.000000000000000000 ) ) ;
#24125 = EDGE_CURVE ( 'NONE', #137134, #5098, #67298, .T. ) ;
#24126 = CARTESIAN_POINT ( 'NONE',  ( 39.66709685856477563, -3.055000000000000160, -5.291415217122921177 ) ) ;
#24127 = ORIENTED_EDGE ( 'NONE', *, *, #11913, .T. ) ;
#24128 = DIRECTION ( 'NONE',  ( 0.7071067811865486830, -0.7071067811865464625, -0.000000000000000000 ) ) ;
#24129 = VERTEX_POINT ( 'NONE', #130413 ) ;
#24130 = CIRCLE ( 'NONE', #135291, 2.055000000000001048 ) ;
#24131 = DIRECTION ( 'NONE',  ( 0.000000000000000000, 0.000000000000000000, 1.000000000000000000 ) ) ;
#24132 = DIRECTION ( 'NONE',  ( 0.3543493200069162685, -0.000000000000000000, -0.9351131265310288487 ) ) ;
#24133 =( LENGTH_UNIT ( ) NAMED_UNIT ( * ) SI_UNIT ( .MILLI., .METRE. ) );
#24134 = CARTESIAN_POINT ( 'NONE',  ( -14.99999999999990230, 7.559798855135676732, 4.979909187984716823 ) ) ;
#24135 = ORIENTED_EDGE ( 'NONE', *, *, #102451, .T. ) ;
#24136 = EDGE_CURVE ( 'NONE', #40570, #98769, #75320, .T. ) ;
#24137 = LINE ( 'NONE', #113265, #69653 ) ;
#24138 = ORIENTED_EDGE ( 'NONE', *, *, #132025, .F. ) ;
#24139 = FACE_OUTER_BOUND ( 'NONE', #26337, .T. ) ;
#24140 = DIRECTION ( 'NONE',  ( -0.7071067811865486830, -0.7071067811865464625, 0.000000000000000000 ) ) ;
#24141 = CARTESIAN_POINT ( 'NONE',  ( -34.92500000000001137, -21.72500000000000142, 0.4999999999999995559 ) ) ;
#24142 = DIRECTION ( 'NONE',  ( -0.7071067811865487940, 0.7071067811865463515, -0.000000000000000000 ) ) ;
#24143 = DIRECTION ( 'NONE',  ( -0.7071067811865486830, -0.7071067811865464625, 0.000000000000000000 ) ) ;
#24144 = VERTEX_POINT ( 'NONE', #112228 ) ;
#24145 = LINE ( 'NONE', #35773, #84706 ) ;
#24146 = CARTESIAN_POINT ( 'NONE',  ( 56.49543019189812298, 5.291415217122916737, 3.055000000000001936 ) ) ;
#24147 = CARTESIAN_POINT ( 'NONE',  ( -7.214984197241858688, -3.740707523384244837, 15.76143240460122286 ) ) ;
#24148 = DIRECTION ( 'NONE',  ( 0.6830127018922180770, -0.6830127018922204085, -0.2588190451025213501 ) ) ;
#24150 = VERTEX_POINT ( 'NONE', #125957 ) ;
#24149 = FACE_OUTER_BOUND ( 'NONE', #16320, .T. ) ;
#24151 = ORIENTED_EDGE ( 'NONE', *, *, #129904, .T. ) ;
#24152 = CARTESIAN_POINT ( 'NONE',  ( 59.99451991528749772, 28.92564299267980132, 4.000000000000000000 ) ) ;
#24153 = EDGE_LOOP ( 'NONE', ( #104201, #51159, #34849, #135520 ) ) ;
#24154 = VECTOR ( 'NONE', #20409, 1000.000000000000000 ) ;
#24155 = CARTESIAN_POINT ( 'NONE',  ( 34.89822658805448441, 22.27000000000000668, -9.118343482381657594 ) ) ;
#24156 = VERTEX_POINT ( 'NONE', #81763 ) ;
#24157 = FACE_OUTER_BOUND ( 'NONE', #45501, .T. ) ;
#24159 = EDGE_CURVE ( 'NONE', #56636, #60449, #70874, .T. ) ;
#24158 = LINE ( 'NONE', #45929, #131301 ) ;
#24160 = CARTESIAN_POINT ( 'NONE',  ( -33.18398860626899705, 28.73617430169810305, 5.000000000000000000 ) ) ;
#24161 = DIRECTION ( 'NONE',  ( -0.3543493200069162685, -0.000000000000000000, -0.9351131265310288487 ) ) ;
#24162 = FACE_BOUND ( 'NONE', #52009, .T. ) ;
#24163 = DIRECTION ( 'NONE',  ( -0.6830127018922181881, 0.6830127018922202975, -0.2588190451025214056 ) ) ;
#24165 = EDGE_CURVE ( 'NONE', #14419, #39873, #46282, .T. ) ;
#24164 = ADVANCED_FACE ( 'NONE', ( #14321 ), #25983, .T. ) ;
#24166 = EDGE_CURVE ( 'NONE', #113805, #78627, #109274, .T. ) ;
#24167 = DIRECTION ( 'NONE',  ( 0.6830127018922181881, 0.6830127018922202975, -0.2588190451025214056 ) ) ;
#24168 = LINE ( 'NONE', #78557, #126825 ) ;
#24170 = ORIENTED_EDGE ( 'NONE', *, *, #42522, .T. ) ;
#24169 = DIRECTION ( 'NONE',  ( -0.6830127018922180770, -0.6830127018922204085, -0.2588190451025213501 ) ) ;
#24171 = AXIS2_PLACEMENT_3D ( 'NONE', #137960, #113320, #92280 ) ;
#24172 = DIRECTION ( 'NONE',  ( -0.000000000000000000, 0.000000000000000000, 1.000000000000000000 ) ) ;
#24173 = ORIENTED_EDGE ( 'NONE', *, *, #98334, .F. ) ;
#24174 = ADVANCED_FACE ( 'NONE', ( #92578 ), #57160, .F. ) ;
#24175 = EDGE_CURVE ( 'NONE', #83448, #12339, #134710, .T. ) ;
#24176 = VECTOR ( 'NONE', #8030, 1000.000000000000227 ) ;
#24177 = ORIENTED_EDGE ( 'NONE', *, *, #11337, .F. ) ;
#24178 = CARTESIAN_POINT ( 'NONE',  ( 79.39126352523146579, -4.472830434245838482, -4.472830434245838482 ) ) ;
#24179 = ORIENTED_EDGE ( 'NONE', *, *, #46665, .F. ) ;
#24180 = EDGE_CURVE ( 'NONE', #102725, #93151, #87827, .T. ) ;
#24181 = CARTESIAN_POINT ( 'NONE',  ( 11.99999999999991651, -15.03360074219758324, 5.000000000000000000 ) ) ;
#24182 = VECTOR ( 'NONE', #43013, 1000.000000000000000 ) ;
#24183 = ADVANCED_FACE ( 'NONE', ( #59986 ), #104155, .F. ) ;
#24184 = ORIENTED_EDGE ( 'NONE', *, *, #106030, .T. ) ;
#24185 = DIRECTION ( 'NONE',  ( 0.6830127018922181881, 0.6830127018922202975, -0.2588190451025214056 ) ) ;
#24186 = EDGE_CURVE ( 'NONE', #8228, #93313, #13583, .T. ) ;
#24187 =( BOUNDED_CURVE ( )  B_SPLINE_CURVE ( 3, ( #142581, #133148, #43273, #33825 ),
 .UNSPECIFIED., .F., .F. ) 
 B_SPLINE_CURVE_WITH_KNOTS ( ( 4, 4 ),
 ( 1.901594255663605182, 1.933014472006542306 ),
 .UNSPECIFIED. ) 
 CURVE ( )  GEOMETRIC_REPRESENTATION_ITEM ( )  RATIONAL_B_SPLINE_CURVE ( ( 1.000000000000000000, 0.9999177325257868620, 0.9999177325257868620, 1.000000000000000000 ) ) 
 REPRESENTATION_ITEM ( '' )  );
#24188 = CARTESIAN_POINT ( 'NONE',  ( -39.18398860626899705, 28.73617430169814568, 5.000000000000000000 ) ) ;
#24189 = EDGE_CURVE ( 'NONE', #92779, #57095, #2724, .T. ) ;
#24190 = CARTESIAN_POINT ( 'NONE',  ( 8.510786437626906675, -27.52281430457049183, 5.000000000000000000 ) ) ;
#24191 = VECTOR ( 'NONE', #35324, 1000.000000000000000 ) ;
#24192 = CARTESIAN_POINT ( 'NONE',  ( 6.874395825605885690, -40.07226884389044130, 19.48967909493512352 ) ) ;
#24194 = PLANE ( 'NONE',  #38007 ) ;
#24193 = PLANE ( 'NONE',  #69019 ) ;
#24195 = CARTESIAN_POINT ( 'NONE',  ( 27.29974487139158512, -27.71228299555225405, 4.000000000000000000 ) ) ;
#24196 = PLANE ( 'NONE',  #81005 ) ;
#24197 = EDGE_LOOP ( 'NONE', ( #109550, #66485, #91576, #128104 ) ) ;
#24198 = ORIENTED_EDGE ( 'NONE', *, *, #133712, .F. ) ;
#24199 = CARTESIAN_POINT ( 'NONE',  ( 25.00442415654155681, 3.591886032380943838, 4.000000000000000000 ) ) ;
#24200 =( BOUNDED_CURVE ( )  B_SPLINE_CURVE ( 3, ( #83223, #70938, #94077, #36161 ),
 .UNSPECIFIED., .F., .T. ) 
 B_SPLINE_CURVE_WITH_KNOTS ( ( 4, 4 ),
 ( 4.350170835173027939, 4.500739107949266682 ),
 .UNSPECIFIED. ) 
 CURVE ( )  GEOMETRIC_REPRESENTATION_ITEM ( )  RATIONAL_B_SPLINE_CURVE ( ( 1.000000000000000000, 0.9981116584018943083, 0.9981116584018943083, 1.000000000000000000 ) ) 
 REPRESENTATION_ITEM ( '' )  );
#24201 = FACE_OUTER_BOUND ( 'NONE', #111150, .T. ) ;
#24202 = ORIENTED_EDGE ( 'NONE', *, *, #94224, .T. ) ;
#24203 = EDGE_CURVE ( 'NONE', #23833, #32348, #119157, .T. ) ;
#24204 = ORIENTED_EDGE ( 'NONE', *, *, #137850, .F. ) ;
#24205 = VERTEX_POINT ( 'NONE', #25188 ) ;
#24206 = DIRECTION ( 'NONE',  ( 1.000000000000000000, 0.000000000000000000, 0.000000000000000000 ) ) ;
#24207 = ORIENTED_EDGE ( 'NONE', *, *, #143397, .T. ) ;
#24208 = LINE ( 'NONE', #33675, #6907 ) ;
#24209 = ADVANCED_FACE ( 'NONE', ( #48380 ), #69444, .T. ) ;
#24210 = VECTOR ( 'NONE', #137600, 1000.000000000000000 ) ;
#24211 = CARTESIAN_POINT ( 'NONE',  ( 42.07919371712954870, 3.975000000000002753, -6.884901960086283523 ) ) ;
#24212 =( GEOMETRIC_REPRESENTATION_CONTEXT ( 3 ) GLOBAL_UNCERTAINTY_ASSIGNED_CONTEXT ( ( #124631 ) ) GLOBAL_UNIT_ASSIGNED_CONTEXT ( ( #79181, #98732, #134981 ) ) REPRESENTATION_CONTEXT ( 'NONE', 'WORKASPACE' ) );
#24213 = CARTESIAN_POINT ( 'NONE',  ( 3.275403141435220267, -2.126176841940958351, -7.934999999999989839 ) ) ;
#24214 = VECTOR ( 'NONE', #49219, 1000.000000000000000 ) ;
#24215 = FACE_OUTER_BOUND ( 'NONE', #127300, .T. ) ;
#24216 = ORIENTED_EDGE ( 'NONE', *, *, #39775, .F. ) ;
#24217 = VECTOR ( 'NONE', #118827, 1000.000000000000000 ) ;
#24218 = LINE ( 'NONE', #14019, #131441 ) ;
#24219 = LINE ( 'NONE', #124939, #39714 ) ;
#24220 = CARTESIAN_POINT ( 'NONE',  ( -15.70710678118642711, -6.740707523384211086, 5.000000000000000000 ) ) ;
#24222 = ORIENTED_EDGE ( 'NONE', *, *, #142388, .T. ) ;
#24221 = CARTESIAN_POINT ( 'NONE',  ( -19.39656807105345848, -14.24070752338412937, 19.24067776001721342 ) ) ;
#24223 = ORIENTED_EDGE ( 'NONE', *, *, #106454, .T. ) ;
#24224 = DIRECTION ( 'NONE',  ( 1.000000000000000000, 0.000000000000000000, 0.000000000000000000 ) ) ;
#24225 = CARTESIAN_POINT ( 'NONE',  ( -31.49999999999977973, 0.4497235411627178991, -5.599840258123613523 ) ) ;
#24226 = ORIENTED_EDGE ( 'NONE', *, *, #54493, .F. ) ;
#24227 =( NAMED_UNIT ( * ) PLANE_ANGLE_UNIT ( ) SI_UNIT ( $, .RADIAN. ) );
#24228 = EDGE_CURVE ( 'NONE', #114524, #96272, #102666, .T. ) ;
#24229 = PLANE ( 'NONE',  #110408 ) ;
#24230 = ADVANCED_FACE ( 'NONE', ( #133964 ), #137547, .F. ) ;
#24231 = CARTESIAN_POINT ( 'NONE',  ( 1.146006882977912644, -0.4000000000000003553, 2.166563419957292513 ) ) ;
#24232 = DIRECTION ( 'NONE',  ( -1.000000000000000000, -0.000000000000000000, -0.000000000000000000 ) ) ;
#24233 = FACE_OUTER_BOUND ( 'NONE', #108436, .T. ) ;
#24234 = CARTESIAN_POINT ( 'NONE',  ( 54.48921356237310221, -27.52281430457093236, 5.000000000000000000 ) ) ;
#24235 = LINE ( 'NONE', #111967, #86402 ) ;
#24236 = EDGE_CURVE ( 'NONE', #21831, #42023, #128790, .T. ) ;
#24237 = CARTESIAN_POINT ( 'NONE',  ( -23.99999999999982592, 17.58746187583906107, 4.000000000000000000 ) ) ;
#24238 = CARTESIAN_POINT ( 'NONE',  ( 34.49999999999975842, 16.77039438581782349, 0.4657186855306942319 ) ) ;
#24239 = CARTESIAN_POINT ( 'NONE',  ( -30.33010218547246950, 17.25929247661554555, 19.83885114516078474 ) ) ;
#24240 = EDGE_LOOP ( 'NONE', ( #51513, #62975, #33531, #91148 ) ) ;
#24241 = ORIENTED_EDGE ( 'NONE', *, *, #72179, .F. ) ;
#24242 = CARTESIAN_POINT ( 'NONE',  ( -26.99999999999980460, 8.587461875839162317, 4.000000000000000000 ) ) ;
#24243 = CARTESIAN_POINT ( 'NONE',  ( -32.99999999999977263, -10.77435723561698566, -9.972017380717154822 ) ) ;
#24244 = CARTESIAN_POINT ( 'NONE',  ( -0.1670968585647805704, -3.967499999999994476, 6.871911579029513106 ) ) ;
#24245 = DIRECTION ( 'NONE',  ( 0.7071067811865486830, -0.7071067811865464625, -0.000000000000000000 ) ) ;
#24246 = ORIENTED_EDGE ( 'NONE', *, *, #82734, .F. ) ;
#24247 = DIRECTION ( 'NONE',  ( 2.781805975412905274E-17, -0.3543493200069152138, 0.9351131265310292928 ) ) ;
#24248 = LINE ( 'NONE', #101797, #85325 ) ;
#24249 = DIRECTION ( 'NONE',  ( -0.6830127018922181881, 0.6830127018922202975, -0.2588190451025214056 ) ) ;
#24250 = EDGE_LOOP ( 'NONE', ( #96209, #45193, #2320, #131019, #102936 ) ) ;
#24251 = EDGE_CURVE ( 'NONE', #76457, #65481, #6964, .T. ) ;
#24252 = DIRECTION ( 'NONE',  ( 0.7071067811865487940, 0.7071067811865463515, 0.000000000000000000 ) ) ;
#24253 = LINE ( 'NONE', #133040, #114104 ) ;
#24254 = CARTESIAN_POINT ( 'NONE',  ( 53.72459685856478018, -1.637169565754161171, 6.109999999999998543 ) ) ;
#24255 = VECTOR ( 'NONE', #86953, 999.9999999999998863 ) ;
#24256 = CARTESIAN_POINT ( 'NONE',  ( 14.99451991528749595, 28.92564299267948513, 4.000000000000000000 ) ) ;
#24257 = CARTESIAN_POINT ( 'NONE',  ( -9.792893218813391698, 9.759292476615618384, 5.000000000000000000 ) ) ;
#24258 = CARTESIAN_POINT ( 'NONE',  ( -34.49999999999976552, -14.94567065516890558, 4.994342998332162331 ) ) ;
#24259 = EDGE_CURVE ( 'NONE', #63418, #9731, #93314, .T. ) ;
#24260 = VERTEX_POINT ( 'NONE', #107036 ) ;
#24261 = ORIENTED_EDGE ( 'NONE', *, *, #99136, .F. ) ;
#24262 = CARTESIAN_POINT ( 'NONE',  ( -21.29974487139158512, -27.71228299555221142, 4.000000000000000000 ) ) ;
#24263 = DIRECTION ( 'NONE',  ( 0.000000000000000000, 0.000000000000000000, 1.000000000000000000 ) ) ;
#24264 = CARTESIAN_POINT ( 'NONE',  ( -0.4892135623730947680, -27.52281430457055578, 5.000000000000000000 ) ) ;
#24265 = CARTESIAN_POINT ( 'NONE',  ( 1.249915061292911078, 0.4000000000000001887, -2.317232259782045833 ) ) ;
#24266 = EDGE_CURVE ( 'NONE', #119390, #115334, #82451, .T. ) ;
#24267 = DIRECTION ( 'NONE',  ( -0.000000000000000000, 0.000000000000000000, 1.000000000000000000 ) ) ;
#24268 = DIRECTION ( 'NONE',  ( 0.000000000000000000, 0.000000000000000000, 1.000000000000000000 ) ) ;
#24269 = ORIENTED_EDGE ( 'NONE', *, *, #130272, .F. ) ;
#24270 = ORIENTED_EDGE ( 'NONE', *, *, #346, .T. ) ;
#24271 = CARTESIAN_POINT ( 'NONE',  ( -8.999999999999921840, -16.06887692260765377, 4.000000000000000000 ) ) ;
#24272 = CARTESIAN_POINT ( 'NONE',  ( 27.00000000000000355, -4.083527258847093222, -4.862849486279972488 ) ) ;
#24273 = UNCERTAINTY_MEASURE_WITH_UNIT (LENGTH_MEASURE( 1.000000000000000082E-05 ), #31307, 'distance_accuracy_value', 'NONE');
#24274 = DIRECTION ( 'NONE',  ( 0.3543493200069162685, -0.000000000000000000, -0.9351131265310288487 ) ) ;
#24275 = CARTESIAN_POINT ( 'NONE',  ( 72.85002705046289861, -5.819803920172572198, -5.819803920172572198 ) ) ;
#24276 = PLANE ( 'NONE',  #106515 ) ;
#24277 = VECTOR ( 'NONE', #123809, 1000.000000000000000 ) ;
#24278 = EDGE_CURVE ( 'NONE', #34100, #50218, #104899, .T. ) ;
#24279 = DIRECTION ( 'NONE',  ( 0.7071067811865487940, 0.7071067811865463515, -0.000000000000000000 ) ) ;
#24280 = ORIENTED_EDGE ( 'NONE', *, *, #104473, .F. ) ;
#24281 = CARTESIAN_POINT ( 'NONE',  ( 70.41666666666665719, -6.884901960086287076, -3.975000000000000977 ) ) ;
#24282 = CARTESIAN_POINT ( 'NONE',  ( -15.18398860626900237, 28.73617430169797871, 5.000000000000000000 ) ) ;
#24283 = STYLED_ITEM ( 'NONE', ( #106285 ), #90553 ) ;
#24284 = DIRECTION ( 'NONE',  ( -0.7071067811865486830, -0.7071067811865464625, 0.000000000000000000 ) ) ;
#24285 = DIRECTION ( 'NONE',  ( -0.7071067811865486830, -0.7071067811865464625, 0.000000000000000000 ) ) ;
#24286 = ORIENTED_EDGE ( 'NONE', *, *, #134834, .F. ) ;
#24287 = EDGE_CURVE ( 'NONE', #54574, #92154, #17860, .T. ) ;
#24288 = FACE_OUTER_BOUND ( 'NONE', #49017, .T. ) ;
#24289 = EDGE_CURVE ( 'NONE', #31140, #109534, #83157, .T. ) ;
#24290 = PRESENTATION_LAYER_ASSIGNMENT (  '', '', ( #65920 ) ) ;
#24291 = CARTESIAN_POINT ( 'NONE',  ( 16.82816939922341604, 18.75929247661552424, 4.000000000000000000 ) ) ;
#24292 = CARTESIAN_POINT ( 'NONE',  ( 63.14626352523143282, -4.472830434245840259, 4.472830434245839371 ) ) ;
#24293 = ORIENTED_EDGE ( 'NONE', *, *, #48422, .T. ) ;
#24294 = ORIENTED_EDGE ( 'NONE', *, *, #57740, .T. ) ;
#24295 = LINE ( 'NONE', #68541, #29162 ) ;
#24296 = SURFACE_SIDE_STYLE ('',( #79446 ) ) ;
#24297 = CARTESIAN_POINT ( 'NONE',  ( 44.31249999999999289, 5.819803920172571310, 5.819803920172576639 ) ) ;
#24298 = ADVANCED_FACE ( 'NONE', ( #49122 ), #41074, .T. ) ;
#24299 = CARTESIAN_POINT ( 'NONE',  ( -29.75830541574794808, 0.7592924766157173044, 14.37146558664989904 ) ) ;
#24301 = ORIENTED_EDGE ( 'NONE', *, *, #11779, .T. ) ;
#24300 = LINE ( 'NONE', #81568, #126303 ) ;
#24302 = CARTESIAN_POINT ( 'NONE',  ( -20.29289321881331176, -18.74070752338409562, 5.000000000000000000 ) ) ;
#24303 = CARTESIAN_POINT ( 'NONE',  ( -2.018447346356678995, 18.75929247661552424, 20.33588619593443170 ) ) ;
#24304 = DIRECTION ( 'NONE',  ( 0.000000000000000000, -1.000000000000000000, 0.000000000000000000 ) ) ;
#24305 = DIRECTION ( 'NONE',  ( -0.000000000000000000, 0.000000000000000000, 1.000000000000000000 ) ) ;
#24306 = EDGE_LOOP ( 'NONE', ( #19472, #76371, #111926, #22409 ) ) ;
#24307 =( GEOMETRIC_REPRESENTATION_CONTEXT ( 3 ) GLOBAL_UNCERTAINTY_ASSIGNED_CONTEXT ( ( #37444 ) ) GLOBAL_UNIT_ASSIGNED_CONTEXT ( ( #33711, #79382, #122838 ) ) REPRESENTATION_CONTEXT ( 'NONE', 'WORKASPACE' ) );
#24308 = ORIENTED_EDGE ( 'NONE', *, *, #105117, .T. ) ;
#24309 = CARTESIAN_POINT ( 'NONE',  ( 52.93793019189809002, -6.110000000000001208, 1.637169565754158951 ) ) ;
#24310 = CIRCLE ( 'NONE', #126239, 0.5000000000000004441 ) ;
#24311 = VECTOR ( 'NONE', #33854, 1000.000000000000000 ) ;
#24312 = ORIENTED_EDGE ( 'NONE', *, *, #5812, .F. ) ;
#24313 = VECTOR ( 'NONE', #2001, 1000.000000000000000 ) ;
#24314 = CARTESIAN_POINT ( 'NONE',  ( -29.99999999999979750, 14.87792677143805520, -11.06722581663446903 ) ) ;
#24315 = DIRECTION ( 'NONE',  ( -0.7071067811865487940, 0.7071067811865463515, -0.000000000000000000 ) ) ;
#24316 = FACE_OUTER_BOUND ( 'NONE', #65157, .T. ) ;
#24317 = CARTESIAN_POINT ( 'NONE',  ( 15.78162688292483473, 21.74787736706806029, 4.999607392498049308 ) ) ;
#24318 = DIRECTION ( 'NONE',  ( -0.6830127018922180770, -0.6830127018922204085, -0.2588190451025213501 ) ) ;
#24319 = EDGE_LOOP ( 'NONE', ( #66076, #22965, #52344, #97397 ) ) ;
#24320 = ORIENTED_EDGE ( 'NONE', *, *, #39790, .F. ) ;
#24321 = DIRECTION ( 'NONE',  ( -0.3543493200069162685, -0.000000000000000000, -0.9351131265310288487 ) ) ;
#24322 = CARTESIAN_POINT ( 'NONE',  ( -16.77039577548053728, -0.01029060706347190504, -34.06785180161139692 ) ) ;
#24323 = ORIENTED_EDGE ( 'NONE', *, *, #59393, .T. ) ;
#24324 = LINE ( 'NONE', #26468, #109247 ) ;
#24325 = CARTESIAN_POINT ( 'NONE',  ( -34.92500000000001137, -6.183345613589518841, 4.500000000000000888 ) ) ;
#24326 = FACE_OUTER_BOUND ( 'NONE', #22454, .T. ) ;
#24327 = VERTEX_POINT ( 'NONE', #28789 ) ;
#24328 = FACE_BOUND ( 'NONE', #64160, .T. ) ;
#24329 = DIRECTION ( 'NONE',  ( 0.000000000000000000, -1.000000000000000000, 0.000000000000000000 ) ) ;
#24330 = CARTESIAN_POINT ( 'NONE',  ( -21.48921356237309155, -27.52281430457070499, 5.000000000000000000 ) ) ;
#24331 = DIRECTION ( 'NONE',  ( -0.7071067811865486830, -0.7071067811865464625, -0.000000000000000000 ) ) ;
#24332 = DIRECTION ( 'NONE',  ( -0.7071067811865486830, -0.7071067811865464625, 0.000000000000000000 ) ) ;
#24333 = DIRECTION ( 'NONE',  ( 0.7071067811865486830, -0.7071067811865464625, -0.000000000000000000 ) ) ;
#24334 = DIRECTION ( 'NONE',  ( 1.000000000000000000, 0.000000000000000000, 0.000000000000000000 ) ) ;
#24335 = ORIENTED_EDGE ( 'NONE', *, *, #126321, .T. ) ;
#24336 = EDGE_CURVE ( 'NONE', #86181, #2775, #51966, .T. ) ;
#24337 = ORIENTED_EDGE ( 'NONE', *, *, #88831, .T. ) ;
#24338 = CARTESIAN_POINT ( 'NONE',  ( 101.2662635252314374, 4.472830434245838482, -4.472830434245837594 ) ) ;
#24339 = ORIENTED_EDGE ( 'NONE', *, *, #8369, .T. ) ;
#24340 = EDGE_CURVE ( 'NONE', #73530, #114745, #17185, .T. ) ;
#24341 = LINE ( 'NONE', #91058, #129949 ) ;
#24342 = ORIENTED_EDGE ( 'NONE', *, *, #40425, .F. ) ;
#24343 = ADVANCED_FACE ( 'NONE', ( #96145 ), #106289, .F. ) ;
#24344 = DIRECTION ( 'NONE',  ( -0.000000000000000000, 0.3543493200069153248, 0.9351131265310292928 ) ) ;
#24345 = ADVANCED_FACE ( 'NONE', ( #84595 ), #29470, .F. ) ;
#24346 = DIRECTION ( 'NONE',  ( -0.7071067811865486830, -0.7071067811865464625, -0.000000000000000000 ) ) ;
#24347 = DIRECTION ( 'NONE',  ( -0.7071067811865487940, 0.7071067811865463515, -0.000000000000000000 ) ) ;
#24348 = ORIENTED_EDGE ( 'NONE', *, *, #93283, .T. ) ;
#24349 = CARTESIAN_POINT ( 'NONE',  ( 9.279999999999999361, 9.521314400968980422E-16, 0.000000000000000000 ) ) ;
#24350 = LINE ( 'NONE', #2574, #70953 ) ;
#24351 = EDGE_CURVE ( 'NONE', #8640, #50635, #107739, .T. ) ;
#24352 = FILL_AREA_STYLE_COLOUR ( '', #82855 ) ;
#24353 = CARTESIAN_POINT ( 'NONE',  ( -15.51665438641034989, 22.22500000000000142, 4.500000000000000888 ) ) ;
#24354 = DIRECTION ( 'NONE',  ( -0.3543493200069162685, -0.000000000000000000, -0.9351131265310288487 ) ) ;
#24355 = CARTESIAN_POINT ( 'NONE',  ( 13.63753812416088707, 22.22500000000000142, 4.000000000000000000 ) ) ;
#24356 = ORIENTED_EDGE ( 'NONE', *, *, #86841, .T. ) ;
#24357 = CARTESIAN_POINT ( 'NONE',  ( 16.49999999999988276, -10.04351517176476527, -1.623559851933785714 ) ) ;
#24358 = LINE ( 'NONE', #1153, #62781 ) ;
#24359 = ADVANCED_FACE ( 'NONE', ( #16437 ), #94011, .T. ) ;
#24360 = ORIENTED_EDGE ( 'NONE', *, *, #4311, .T. ) ;
#24361 = ORIENTED_EDGE ( 'NONE', *, *, #4451, .F. ) ;
#24362 = EDGE_CURVE ( 'NONE', #65251, #20682, #116495, .T. ) ;
#24363 = ORIENTED_EDGE ( 'NONE', *, *, #101901, .T. ) ;
#24364 = CARTESIAN_POINT ( 'NONE',  ( 50.02126352523143282, -4.472830434245838482, -4.472830434245840259 ) ) ;
#24365 = EDGE_LOOP ( 'NONE', ( #111901, #2692, #141057, #108066 ) ) ;
#24367 = EDGE_CURVE ( 'NONE', #42968, #29293, #39675, .T. ) ;
#24366 =( BOUNDED_CURVE ( )  B_SPLINE_CURVE ( 3, ( #33569, #22618, #66885, #112522 ),
 .UNSPECIFIED., .F., .T. ) 
 B_SPLINE_CURVE_WITH_KNOTS ( ( 4, 4 ),
 ( 2.001653308786151442, 3.503810798801451742 ),
 .UNSPECIFIED. ) 
 CURVE ( )  GEOMETRIC_REPRESENTATION_ITEM ( )  RATIONAL_B_SPLINE_CURVE ( ( 1.000000000000000000, 0.8206354192515199486, 0.8206354192515199486, 1.000000000000000000 ) ) 
 REPRESENTATION_ITEM ( '' )  );
#24368 = DIRECTION ( 'NONE',  ( 0.6830127018922181881, 0.6830127018922202975, -0.2588190451025214056 ) ) ;
#24369 = VECTOR ( 'NONE', #85807, 1000.000000000000000 ) ;
#24370 = CARTESIAN_POINT ( 'NONE',  ( 6.170806282870438864, -3.047499999999997211, -5.278424836066143655 ) ) ;
#24371 = CARTESIAN_POINT ( 'NONE',  ( 87.50043019189810423, -3.055000000000002380, 5.291415217122920289 ) ) ;
#24372 = CARTESIAN_POINT ( 'NONE',  ( -29.99999999999978328, 1.552185695429149304, 5.000000000000000000 ) ) ;
#24373 = ORIENTED_EDGE ( 'NONE', *, *, #33298, .F. ) ;
#24374 =( GEOMETRIC_REPRESENTATION_CONTEXT ( 3 ) GLOBAL_UNCERTAINTY_ASSIGNED_CONTEXT ( ( #133064 ) ) GLOBAL_UNIT_ASSIGNED_CONTEXT ( ( #114168, #125045, #125781 ) ) REPRESENTATION_CONTEXT ( 'NONE', 'WORKASPACE' ) );
#24375 = CARTESIAN_POINT ( 'NONE',  ( 21.29974487139158512, -27.71228299555221142, 4.000000000000000000 ) ) ;
#24376 = EDGE_LOOP ( 'NONE', ( #8779, #8893, #140460, #72393 ) ) ;
#24377 = CARTESIAN_POINT ( 'NONE',  ( 30.18398860626900060, 28.73617430169808173, 5.000000000000000000 ) ) ;
#24378 = DIRECTION ( 'NONE',  ( 0.3543493200069163240, -0.000000000000000000, 0.9351131265310288487 ) ) ;
#24379 = VERTEX_POINT ( 'NONE', #122183 ) ;
#24380 = FACE_OUTER_BOUND ( 'NONE', #116533, .T. ) ;
#24381 = CARTESIAN_POINT ( 'NONE',  ( -16.49999999999988276, 13.56627193232213102, -10.57019076586072259 ) ) ;
#24382 = CARTESIAN_POINT ( 'NONE',  ( 126.4954301918981230, 5.291415217122917625, 3.055000000000002380 ) ) ;
#24383 = ORIENTED_EDGE ( 'NONE', *, *, #128484, .F. ) ;
#24384 = DIRECTION ( 'NONE',  ( 0.7071067811865486830, -0.7071067811865464625, -0.000000000000000000 ) ) ;
#24385 = AXIS2_PLACEMENT_3D ( 'NONE', #69576, #26046, #37650 ) ;
#24386 = ORIENTED_EDGE ( 'NONE', *, *, #74648, .F. ) ;
#24387 = ORIENTED_EDGE ( 'NONE', *, *, #43077, .T. ) ;
#24388 = VERTEX_POINT ( 'NONE', #99007 ) ;
#24389 = EDGE_CURVE ( 'NONE', #101006, #90591, #30932, .T. ) ;
#24390 = CARTESIAN_POINT ( 'NONE',  ( 16.30000000000000071, 2.055000000000001492, 0.000000000000000000 ) ) ;
#24391 = DIRECTION ( 'NONE',  ( 0.000000000000000000, -1.000000000000000000, 0.000000000000000000 ) ) ;
#24392 = DIRECTION ( 'NONE',  ( -0.6830127018922181881, 0.6830127018922202975, -0.2588190451025214056 ) ) ;
#24393 = LINE ( 'NONE', #3333, #92831 ) ;
#24394 = VERTEX_POINT ( 'NONE', #8399 ) ;
#24395 = SURFACE_STYLE_USAGE ( .BOTH. , #46192 ) ;
#24396 = EDGE_CURVE ( 'NONE', #69437, #98488, #22155, .T. ) ;
#24397 = VECTOR ( 'NONE', #57309, 1000.000000000000000 ) ;
#24398 = CARTESIAN_POINT ( 'NONE',  ( 26.22873647476855652, 5.808823158059031044, -5.808823158059038150 ) ) ;
#24399 = LINE ( 'NONE', #68646, #106391 ) ;
#24400 = VECTOR ( 'NONE', #133426, 1000.000000000000000 ) ;
#24401 = LINE ( 'NONE', #100549, #76130 ) ;
#24402 = VECTOR ( 'NONE', #13291, 1000.000000000000227 ) ;
#24403 = LINE ( 'NONE', #14240, #35151 ) ;
#24404 = ORIENTED_EDGE ( 'NONE', *, *, #15741, .F. ) ;
#24405 = ORIENTED_EDGE ( 'NONE', *, *, #62800, .F. ) ;
#24406 = EDGE_CURVE ( 'NONE', #103560, #74147, #121481, .T. ) ;
#24407 = ORIENTED_EDGE ( 'NONE', *, *, #101070, .T. ) ;
#24408 =( NAMED_UNIT ( * ) SI_UNIT ( $, .STERADIAN. ) SOLID_ANGLE_UNIT ( ) );
#24409 = CARTESIAN_POINT ( 'NONE',  ( 57.14583333333332860, 2.130196079827431976, -7.949999999999998401 ) ) ;
#24410 = UNCERTAINTY_MEASURE_WITH_UNIT (LENGTH_MEASURE( 1.000000000000000082E-05 ), #34609, 'distance_accuracy_value', 'NONE');
#24411 = PRESENTATION_LAYER_ASSIGNMENT (  '', '', ( #12908 ) ) ;
#24412 = CARTESIAN_POINT ( 'NONE',  ( 0.000000000000000000, 0.000000000000000000, 5.000000000000000000 ) ) ;
#24413 = DIRECTION ( 'NONE',  ( -0.7071067811865487940, 0.7071067811865463515, -0.000000000000000000 ) ) ;
#24414 = CARTESIAN_POINT ( 'NONE',  ( 7.650458736803186888, 8.843704551814687065, 3.473947073368465421 ) ) ;
#24415 = PLANE ( 'NONE',  #110900 ) ;
#24416 = DIRECTION ( 'NONE',  ( 0.7071067811865486830, -0.7071067811865464625, -0.000000000000000000 ) ) ;
#24417 = EDGE_CURVE ( 'NONE', #106976, #69406, #130963, .T. ) ;
#24418 = CARTESIAN_POINT ( 'NONE',  ( 19.49999999999987921, 13.56627193232217188, -10.57019076586064266 ) ) ;
#24419 = LINE ( 'NONE', #68665, #62951 ) ;
#24420 = CARTESIAN_POINT ( 'NONE',  ( 6.940000000000001279, -2.055000000000000160, 0.000000000000000000 ) ) ;
#24421 = ORIENTED_EDGE ( 'NONE', *, *, #113073, .F. ) ;
#24422 = DIRECTION ( 'NONE',  ( 0.7071067811865487940, 0.7071067811865463515, -0.000000000000000000 ) ) ;
#24423 = ORIENTED_EDGE ( 'NONE', *, *, #27960, .T. ) ;
#24424 = FACE_OUTER_BOUND ( 'NONE', #98997, .T. ) ;
#24426 = VERTEX_POINT ( 'NONE', #32349 ) ;
#24425 = CARTESIAN_POINT ( 'NONE',  ( 18.70701326429291456, -21.74070752338405654, 4.999753212805210012 ) ) ;
#24427 = EDGE_CURVE ( 'NONE', #87614, #51304, #83959, .T. ) ;
#24428 = DIRECTION ( 'NONE',  ( -0.7071067811865487940, 0.7071067811865463515, -0.000000000000000000 ) ) ;
#24429 = EDGE_CURVE ( 'NONE', #5483, #37692, #31635, .T. ) ;
#24430 = ORIENTED_EDGE ( 'NONE', *, *, #32868, .T. ) ;
#24431 = DIRECTION ( 'NONE',  ( 0.3543493200069162685, -0.000000000000000000, -0.9351131265310288487 ) ) ;
#24432 = EDGE_LOOP ( 'NONE', ( #136582, #64651, #135205, #133382 ) ) ;
#24433 = DIRECTION ( 'NONE',  ( -0.6830127018922181881, 0.6830127018922202975, -0.2588190451025214056 ) ) ;
#24434 = VERTEX_POINT ( 'NONE', #53372 ) ;
#24435 = CARTESIAN_POINT ( 'NONE',  ( 45.29974487139158867, -27.71228299555237840, 4.000000000000000000 ) ) ;
#24436 = CARTESIAN_POINT ( 'NONE',  ( 105.6625270504628844, 7.949999999999998401, 1.460391307983218338E-15 ) ) ;
#24437 = LINE ( 'NONE', #68685, #64865 ) ;
#24438 = CARTESIAN_POINT ( 'NONE',  ( 36.18398860626899705, 28.73617430169812437, 5.000000000000000000 ) ) ;
#24439 = EDGE_LOOP ( 'NONE', ( #121271, #140270, #44785, #114858 ) ) ;
#24440 = DIRECTION ( 'NONE',  ( 0.6830127018922180770, -0.6830127018922204085, -0.2588190451025213501 ) ) ;
#24441 = CARTESIAN_POINT ( 'NONE',  ( 0.4892135623730947680, -27.52281430457055578, 5.000000000000000000 ) ) ;
#24442 = CARTESIAN_POINT ( 'NONE',  ( 12.18398860626900060, 28.73617430169795739, 5.000000000000000000 ) ) ;
#24443 = CARTESIAN_POINT ( 'NONE',  ( 15.31250000000000000, -4.461849672132299993, -4.461849672132299105 ) ) ;
#24444 = CARTESIAN_POINT ( 'NONE',  ( 25.06206980810188512, -7.934999999999990727, -2.126176841940955242 ) ) ;
#24445 = CARTESIAN_POINT ( 'NONE',  ( -12.48921356237309155, -27.52281430457064104, 5.000000000000000000 ) ) ;
#24446 = DIRECTION ( 'NONE',  ( 0.6830127018922180770, -0.6830127018922204085, -0.2588190451025213501 ) ) ;
#24447 = ORIENTED_EDGE ( 'NONE', *, *, #26988, .T. ) ;
#24448 = EDGE_CURVE ( 'NONE', #141174, #6489, #130245, .T. ) ;
#24449 = DIRECTION ( 'NONE',  ( -0.7071067811865486830, -0.7071067811865464625, -0.000000000000000000 ) ) ;
#24450 = ORIENTED_EDGE ( 'NONE', *, *, #132450, .T. ) ;
#24451 = EDGE_CURVE ( 'NONE', #41816, #113815, #143243, .T. ) ;
#24452 = CARTESIAN_POINT ( 'NONE',  ( 90.85459685856477563, -1.637169565754161615, 6.110000000000000320 ) ) ;
#24453 = DIRECTION ( 'NONE',  ( -0.7071067811865486830, 0.7071067811865464625, 0.000000000000000000 ) ) ;
#24454 = CARTESIAN_POINT ( 'NONE',  ( 17.84878961325748037, 2.500000000000000444, 0.000000000000000000 ) ) ;
#24455 = CARTESIAN_POINT ( 'NONE',  ( 126.6671759105392567, -47.13357697190492246, -36.34567044387053869 ) ) ;
#24456 = VERTEX_POINT ( 'NONE', #75167 ) ;
#24457 = CARTESIAN_POINT ( 'NONE',  ( -14.99451991528749595, 28.92564299267948513, 4.000000000000000000 ) ) ;
#24458 = CARTESIAN_POINT ( 'NONE',  ( 2.277185695429367662, -21.72499999999999432, 5.000000000000000000 ) ) ;
#24459 = DIRECTION ( 'NONE',  ( 0.000000000000000000, -1.000000000000000000, 0.000000000000000000 ) ) ;
#24460 = EDGE_CURVE ( 'NONE', #51050, #74995, #52656, .T. ) ;
#24461 = ORIENTED_EDGE ( 'NONE', *, *, #51679, .F. ) ;
#24462 = DIRECTION ( 'NONE',  ( 0.7071067811865486830, -0.7071067811865464625, -0.000000000000000000 ) ) ;
#24463 = EDGE_CURVE ( 'NONE', #82613, #92516, #9103, .T. ) ;
#24464 = FACE_OUTER_BOUND ( 'NONE', #112111, .T. ) ;
#24466 = VERTEX_POINT ( 'NONE', #33100 ) ;
#24465 = DIRECTION ( 'NONE',  ( -1.000000000000000000, 0.000000000000000000, 0.000000000000000000 ) ) ;
#24467 = CARTESIAN_POINT ( 'NONE',  ( 34.92499999999998295, -16.29806943317885271, 4.500000000000000888 ) ) ;
#24468 = CARTESIAN_POINT ( 'NONE',  ( 101.5791937171295558, 3.975000000000002753, -6.884901960086283523 ) ) ;
#24469 = CARTESIAN_POINT ( 'NONE',  ( 14.51078643762690490, -27.52281430457045275, 5.000000000000000000 ) ) ;
#24470 = DIRECTION ( 'NONE',  ( -0.7071067811865487940, 0.7071067811865463515, -0.000000000000000000 ) ) ;
#24471 = CARTESIAN_POINT ( 'NONE',  ( 8.292893218813407685, -3.740707523384241728, 5.000000000000000000 ) ) ;
#24472 = EDGE_LOOP ( 'NONE', ( #82351, #53951, #140450, #26125 ) ) ;
#24473 = VECTOR ( 'NONE', #40555, 1000.000000000000000 ) ;
#24474 = EDGE_LOOP ( 'NONE', ( #64671, #128686, #4711, #130771 ) ) ;
#24475 = VERTEX_POINT ( 'NONE', #78004 ) ;
#24476 = CARTESIAN_POINT ( 'NONE',  ( 82.83376352523144703, 6.110000000000001208, 1.122388791418549305E-15 ) ) ;
#24477 = ORIENTED_EDGE ( 'NONE', *, *, #132966, .F. ) ;
#24478 = VECTOR ( 'NONE', #55528, 1000.000000000000000 ) ;
#24479 = CARTESIAN_POINT ( 'NONE',  ( -22.17183060077631396, 18.75929247661552779, 4.000000000000000000 ) ) ;
#24480 = DIRECTION ( 'NONE',  ( -0.000000000000000000, -0.3543493200069152693, 0.9351131265310292928 ) ) ;
#24481 = LINE ( 'NONE', #68732, #54957 ) ;
#24482 = CARTESIAN_POINT ( 'NONE',  ( 25.39999999999999858, 0.000000000000000000, 6.094999999999989093 ) ) ;
#24483 = ORIENTED_EDGE ( 'NONE', *, *, #86189, .F. ) ;
#24484 = EDGE_CURVE ( 'NONE', #20411, #83949, #141838, .T. ) ;
#24485 = DIRECTION ( 'NONE',  ( -0.7071067811865486830, -0.7071067811865464625, -0.000000000000000000 ) ) ;
#24486 = LINE ( 'NONE', #112923, #130036 ) ;
#24487 = CARTESIAN_POINT ( 'NONE',  ( 23.99451991528749062, 28.92564299267954908, 4.000000000000000000 ) ) ;
#24488 = CARTESIAN_POINT ( 'NONE',  ( 73.41209685856478018, 5.291415217122921177, -3.054999999999994831 ) ) ;
#24489 = ORIENTED_EDGE ( 'NONE', *, *, #55465, .T. ) ;
#24490 = CARTESIAN_POINT ( 'NONE',  ( -18.48921356237309510, -27.52281430457068367, 5.000000000000000000 ) ) ;
#24491 = LINE ( 'NONE', #91219, #14504 ) ;
#24492 = ORIENTED_EDGE ( 'NONE', *, *, #60227, .T. ) ;
#24493 = ORIENTED_EDGE ( 'NONE', *, *, #68463, .T. ) ;
#24494 = CARTESIAN_POINT ( 'NONE',  ( 0.000000000000000000, 21.72500000000000142, 4.500000000000000888 ) ) ;
#24495 = DIRECTION ( 'NONE',  ( 0.000000000000000000, 0.000000000000000000, 1.000000000000000000 ) ) ;
#24496 = PLANE ( 'NONE',  #60514 ) ;
#24497 = DIRECTION ( 'NONE',  ( 0.7071067811865486830, -0.7071067811865464625, -0.000000000000000000 ) ) ;
#24498 = AXIS2_PLACEMENT_3D ( 'NONE', #37512, #81747, #50515 ) ;
#24499 = CARTESIAN_POINT ( 'NONE',  ( 30.70710678118633297, 8.259292476615637923, 5.000000000000000000 ) ) ;
#24500 = FACE_OUTER_BOUND ( 'NONE', #130732, .T. ) ;
#24501 =( NAMED_UNIT ( * ) PLANE_ANGLE_UNIT ( ) SI_UNIT ( $, .RADIAN. ) );
#24503 = EDGE_CURVE ( 'NONE', #98842, #75802, #67120, .T. ) ;
#24502 = VECTOR ( 'NONE', #6601, 1000.000000000000227 ) ;
#24504 = ORIENTED_EDGE ( 'NONE', *, *, #56229, .F. ) ;
#24506 = ORIENTED_EDGE ( 'NONE', *, *, #89045, .T. ) ;
#24505 = AXIS2_PLACEMENT_3D ( 'NONE', #9711, #18422, #61996 ) ;
#24507 = ADVANCED_FACE ( 'NONE', ( #120022 ), #110586, .F. ) ;
#24508 =( GEOMETRIC_REPRESENTATION_CONTEXT ( 3 ) GLOBAL_UNCERTAINTY_ASSIGNED_CONTEXT ( ( #24598 ) ) GLOBAL_UNIT_ASSIGNED_CONTEXT ( ( #71202, #7322, #127716 ) ) REPRESENTATION_CONTEXT ( 'NONE', 'WORKASPACE' ) );
#24509 = DIRECTION ( 'NONE',  ( 1.000000000000000000, 0.000000000000000000, 0.000000000000000000 ) ) ;
#24510 = ORIENTED_EDGE ( 'NONE', *, *, #72587, .F. ) ;
#24511 = ORIENTED_EDGE ( 'NONE', *, *, #78689, .F. ) ;
#24512 = VECTOR ( 'NONE', #107836, 1000.000000000000227 ) ;
#24513 = EDGE_CURVE ( 'NONE', #20118, #76695, #9864, .T. ) ;
#24514 = EDGE_CURVE ( 'NONE', #103671, #8470, #98326, .T. ) ;
#24515 = LINE ( 'NONE', #4120, #24313 ) ;
#24516 = ORIENTED_EDGE ( 'NONE', *, *, #18148, .F. ) ;
#24517 = DIRECTION ( 'NONE',  ( -1.000000000000000000, -1.224606353822377258E-16, -0.000000000000000000 ) ) ;
#24518 = DIRECTION ( 'NONE',  ( -0.7071067811865486830, -0.7071067811865464625, 0.000000000000000000 ) ) ;
#24519 = CARTESIAN_POINT ( 'NONE',  ( -20.99999999999985079, -6.108550654416979420, -3.114665004255016356 ) ) ;
#24520 = DIRECTION ( 'NONE',  ( -0.7071067811865486830, -0.7071067811865464625, -0.000000000000000000 ) ) ;
#24521 = ORIENTED_EDGE ( 'NONE', *, *, #71587, .F. ) ;
#24522 = CARTESIAN_POINT ( 'NONE',  ( 9.328169399223463998, -21.74070752338406365, 4.000000000000000000 ) ) ;
#24523 = EDGE_CURVE ( 'NONE', #77379, #9354, #142547, .T. ) ;
#24524 = ORIENTED_EDGE ( 'NONE', *, *, #11433, .T. ) ;
#24525 = DIRECTION ( 'NONE',  ( -0.000000000000000000, 0.000000000000000000, 1.000000000000000000 ) ) ;
#24526 = ORIENTED_EDGE ( 'NONE', *, *, #114676, .F. ) ;
#24527 = DIRECTION ( 'NONE',  ( -0.7071067811865487940, 0.7071067811865463515, -0.000000000000000000 ) ) ;
#24528 = ADVANCED_FACE ( 'NONE', ( #87451 ), #76589, .T. ) ;
#24529 = ORIENTED_EDGE ( 'NONE', *, *, #104545, .T. ) ;
#24530 = CARTESIAN_POINT ( 'NONE',  ( 6.160000000000001030, 2.055000000000001492, 0.000000000000000000 ) ) ;
#24531 = VERTEX_POINT ( 'NONE', #80861 ) ;
#24532 = VERTEX_POINT ( 'NONE', #103287 ) ;
#24533 = ORIENTED_EDGE ( 'NONE', *, *, #23124, .F. ) ;
#24534 = EDGE_CURVE ( 'NONE', #42223, #55852, #20068, .T. ) ;
#24535 = LINE ( 'NONE', #90523, #14147 ) ;
#24536 = CARTESIAN_POINT ( 'NONE',  ( 1.179999999999999272, 9.043340090917736163, 6.750000000000000888 ) ) ;
#24537 = CARTESIAN_POINT ( 'NONE',  ( 12.43680103220821742, -12.74070752338415069, 9.898150129686346332 ) ) ;
#24538 = CARTESIAN_POINT ( 'NONE',  ( 2.999999999999977351, -21.84840872380824095, 2.849755605029614447 ) ) ;
#24539 = CARTESIAN_POINT ( 'NONE',  ( 119.0004301918981184, -3.055000000000002380, 5.291415217122920289 ) ) ;
#24540 = PLANE ( 'NONE',  #72931 ) ;
#24541 = DIRECTION ( 'NONE',  ( -0.7071067811865486830, -0.7071067811865464625, 0.000000000000000000 ) ) ;
#24542 = DIRECTION ( 'NONE',  ( -0.7071067811865486830, -0.7071067811865464625, 0.000000000000000000 ) ) ;
#24543 = EDGE_CURVE ( 'NONE', #68447, #89873, #114176, .T. ) ;
#24544 = VECTOR ( 'NONE', #57296, 1000.000000000000000 ) ;
#24545 = CARTESIAN_POINT ( 'NONE',  ( 34.78501580275788996, -3.740707523384241728, 15.76143240460132411 ) ) ;
#24546 = FACE_OUTER_BOUND ( 'NONE', #62524, .T. ) ;
#24547 = ORIENTED_EDGE ( 'NONE', *, *, #120485, .F. ) ;
#24548 = LINE ( 'NONE', #23849, #57329 ) ;
#24549 = CARTESIAN_POINT ( 'NONE',  ( 0.000000000000000000, 0.000000000000000000, 5.000000000000000000 ) ) ;
#24550 = ORIENTED_EDGE ( 'NONE', *, *, #91788, .F. ) ;
#24551 = ORIENTED_EDGE ( 'NONE', *, *, #8883, .T. ) ;
#24552 = ADVANCED_FACE ( 'NONE', ( #100464 ), #125051, .F. ) ;
#24553 = LINE ( 'NONE', #14399, #37994 ) ;
#24554 = EDGE_LOOP ( 'NONE', ( #61711, #92279, #100762, #87674 ) ) ;
#24555 = CARTESIAN_POINT ( 'NONE',  ( -11.99999999999990763, 1.552185695429147527, 5.000000000000000000 ) ) ;
#24556 = DIRECTION ( 'NONE',  ( 0.7071067811865487940, -0.7071067811865463515, 0.000000000000000000 ) ) ;
#24557 = DIRECTION ( 'NONE',  ( 0.000000000000000000, 0.000000000000000000, 1.000000000000000000 ) ) ;
#24558 = DIRECTION ( 'NONE',  ( -0.7071067811865486830, -0.7071067811865464625, -0.000000000000000000 ) ) ;
#24559 = CARTESIAN_POINT ( 'NONE',  ( 0.000000000000000000, 0.000000000000000000, 5.000000000000000000 ) ) ;
#24560 = EDGE_CURVE ( 'NONE', #109980, #131513, #125648, .T. ) ;
#24561 = ORIENTED_EDGE ( 'NONE', *, *, #5312, .T. ) ;
#24562 = ADVANCED_FACE ( 'NONE', ( #135933 ), #56981, .F. ) ;
#24563 = FACE_OUTER_BOUND ( 'NONE', #39992, .T. ) ;
#24564 = ORIENTED_EDGE ( 'NONE', *, *, #90718, .F. ) ;
#24565 = CARTESIAN_POINT ( 'NONE',  ( -32.99451991528749062, 28.92564299267960948, 4.000000000000000000 ) ) ;
#24566 = EDGE_CURVE ( 'NONE', #63744, #140742, #14140, .T. ) ;
#24567 = AXIS2_PLACEMENT_3D ( 'NONE', #72540, #116702, #61639 ) ;
#24568 = CARTESIAN_POINT ( 'NONE',  ( 32.44206980810188412, 7.934999999999993392, 2.126176841940951689 ) ) ;
#24569 = ORIENTED_EDGE ( 'NONE', *, *, #28321, .T. ) ;
#24570 = CARTESIAN_POINT ( 'NONE',  ( 6.516654386410396071, 22.22500000000000142, 4.500000000000000888 ) ) ;
#24571 = VECTOR ( 'NONE', #50015, 1000.000000000000000 ) ;
#24572 = CARTESIAN_POINT ( 'NONE',  ( 24.18398860626899705, 28.73617430169804265, 5.000000000000000000 ) ) ;
#24573 = ORIENTED_EDGE ( 'NONE', *, *, #15161, .F. ) ;
#24574 = EDGE_LOOP ( 'NONE', ( #35144, #44229, #26867, #52487 ) ) ;
#24575 = ORIENTED_EDGE ( 'NONE', *, *, #4901, .F. ) ;
#24576 = DIRECTION ( 'NONE',  ( -0.7071067811865486830, -0.7071067811865464625, -0.000000000000000000 ) ) ;
#24577 = DIRECTION ( 'NONE',  ( 0.7071067811865487940, 0.7071067811865463515, 0.000000000000000000 ) ) ;
#24578 = CARTESIAN_POINT ( 'NONE',  ( -54.48921356237310221, -27.52281430457093236, 5.000000000000000000 ) ) ;
#24579 = LINE ( 'NONE', #77570, #42731 ) ;
#24581 = ORIENTED_EDGE ( 'NONE', *, *, #56708, .F. ) ;
#24580 =( BOUNDED_CURVE ( )  B_SPLINE_CURVE ( 3, ( #83651, #16180, #60472, #127858 ),
 .UNSPECIFIED., .F., .F. ) 
 B_SPLINE_CURVE_WITH_KNOTS ( ( 4, 4 ),
 ( 4.350170835173026163, 4.500739107949264906 ),
 .UNSPECIFIED. ) 
 CURVE ( )  GEOMETRIC_REPRESENTATION_ITEM ( )  RATIONAL_B_SPLINE_CURVE ( ( 1.000000000000000000, 0.9981116584018943083, 0.9981116584018943083, 1.000000000000000000 ) ) 
 REPRESENTATION_ITEM ( '' )  );
#24582 = VECTOR ( 'NONE', #41548, 1000.000000000000000 ) ;
#24583 = ADVANCED_FACE ( 'NONE', ( #58433 ), #35941, .T. ) ;
#24584 = LINE ( 'NONE', #66683, #132233 ) ;
#24585 = FACE_OUTER_BOUND ( 'NONE', #37691, .T. ) ;
#24586 = ORIENTED_EDGE ( 'NONE', *, *, #61936, .T. ) ;
#24587 = DIRECTION ( 'NONE',  ( -0.7071067811865486830, -0.7071067811865464625, 0.000000000000000000 ) ) ;
#24588 = EDGE_LOOP ( 'NONE', ( #109728, #43109, #132825, #124586, #71597, #58637 ) ) ;
#24590 = VERTEX_POINT ( 'NONE', #48213 ) ;
#24589 = DIRECTION ( 'NONE',  ( 0.7071067811865487940, -0.7071067811865463515, 0.000000000000000000 ) ) ;
#24591 = VECTOR ( 'NONE', #124516, 1000.000000000000000 ) ;
#24592 = ORIENTED_EDGE ( 'NONE', *, *, #117460, .F. ) ;
#24593 = EDGE_CURVE ( 'NONE', #82088, #48470, #91710, .T. ) ;
#24594 = DIRECTION ( 'NONE',  ( -0.3543493200069162685, -0.000000000000000000, -0.9351131265310288487 ) ) ;
#24595 = DIRECTION ( 'NONE',  ( -0.6830127018922180770, -0.6830127018922204085, -0.2588190451025213501 ) ) ;
#24596 = ORIENTED_EDGE ( 'NONE', *, *, #1175, .T. ) ;
#24597 = DIRECTION ( 'NONE',  ( -0.000000000000000000, -0.3543493200069152693, 0.9351131265310292928 ) ) ;
#24598 = UNCERTAINTY_MEASURE_WITH_UNIT (LENGTH_MEASURE( 1.000000000000000082E-05 ), #71202, 'distance_accuracy_value', 'NONE');
#24599 = ORIENTED_EDGE ( 'NONE', *, *, #51089, .T. ) ;
#24600 = VECTOR ( 'NONE', #90848, 1000.000000000000000 ) ;
#24601 = VECTOR ( 'NONE', #98835, 1000.000000000000000 ) ;
#24602 = DIRECTION ( 'NONE',  ( 0.7071067811865487940, 0.7071067811865463515, 0.000000000000000000 ) ) ;
#24603 = DIRECTION ( 'NONE',  ( -1.000000000000000000, -1.224606353822377258E-16, -0.000000000000000000 ) ) ;
#24604 = VECTOR ( 'NONE', #23965, 999.9999999999998863 ) ;
#24605 = FACE_OUTER_BOUND ( 'NONE', #112233, .T. ) ;
#24606 = CARTESIAN_POINT ( 'NONE',  ( -14.99999999999989875, 12.83542986846996214, -1.025386466790335183 ) ) ;
#24607 = DIRECTION ( 'NONE',  ( 0.000000000000000000, 1.000000000000000000, 0.000000000000000000 ) ) ;
#24609 = EDGE_CURVE ( 'NONE', #7076, #110736, #70011, .T. ) ;
#24608 = LINE ( 'NONE', #22442, #44547 ) ;
#24610 = DIRECTION ( 'NONE',  ( 0.6830127018922180770, -0.6830127018922204085, -0.2588190451025213501 ) ) ;
#24611 = CARTESIAN_POINT ( 'NONE',  ( -8.648657329869978142E-14, -34.64999999999997726, -39.50000000000000000 ) ) ;
#24612 = CARTESIAN_POINT ( 'NONE',  ( 22.29123647476855652, -9.717572351234235426E-16, -7.934999999999990727 ) ) ;
#24613 = CARTESIAN_POINT ( 'NONE',  ( 1.145403141435219263, -2.126176841940958351, -7.934999999999988951 ) ) ;
#24614 = DIRECTION ( 'NONE',  ( -0.000000000000000000, 0.000000000000000000, 1.000000000000000000 ) ) ;
#24615 = AXIS2_PLACEMENT_3D ( 'NONE', #65303, #89866, #31233 ) ;
#24616 = CARTESIAN_POINT ( 'NONE',  ( 6.229065384000522343, 3.821174125832445049E-16, 0.000000000000000000 ) ) ;
#24617 = DIRECTION ( 'NONE',  ( -0.000000000000000000, 0.000000000000000000, 1.000000000000000000 ) ) ;
#24618 = ORIENTED_EDGE ( 'NONE', *, *, #44709, .T. ) ;
#24619 = EDGE_LOOP ( 'NONE', ( #35962, #66651, #131137, #587 ) ) ;
#24620 = CARTESIAN_POINT ( 'NONE',  ( 94.47916666666664298, -7.950000000000001066, 2.130196079827424427 ) ) ;
#24621 = VERTEX_POINT ( 'NONE', #3937 ) ;
#24622 = ORIENTED_EDGE ( 'NONE', *, *, #51399, .F. ) ;
#24623 = EDGE_CURVE ( 'NONE', #79589, #32976, #67722, .T. ) ;
#24624 = ORIENTED_EDGE ( 'NONE', *, *, #6013, .F. ) ;
#24625 = DIRECTION ( 'NONE',  ( 0.7071067811865486830, -0.7071067811865464625, -0.000000000000000000 ) ) ;
#24626 = CARTESIAN_POINT ( 'NONE',  ( 88.79166666666665719, 3.975000000000003642, -6.884901960086285300 ) ) ;
#24627 = CARTESIAN_POINT ( 'NONE',  ( 14.70014206744062690, 9.500065425788731588, 0.2867161110784761102 ) ) ;
#24628 = ORIENTED_EDGE ( 'NONE', *, *, #122970, .F. ) ;
#24629 = CARTESIAN_POINT ( 'NONE',  ( -34.49999999999975842, -19.91253812416055879, 4.000000000000000000 ) ) ;
#24630 = DIRECTION ( 'NONE',  ( -0.000000000000000000, 0.000000000000000000, 1.000000000000000000 ) ) ;
#24631 = DIRECTION ( 'NONE',  ( -0.7071067811865486830, -0.7071067811865464625, 0.000000000000000000 ) ) ;
#24632 = CARTESIAN_POINT ( 'NONE',  ( 125.7873552745503503, 0.9952826964532990317, -7.614395392956494923 ) ) ;
#24633 = ADVANCED_FACE ( 'NONE', ( #81586 ), #125789, .F. ) ;
#24634 = CARTESIAN_POINT ( 'NONE',  ( 128.2454301918981230, -5.291415217122918513, -3.055000000000000160 ) ) ;
#24635 = EDGE_CURVE ( 'NONE', #61603, #135652, #11998, .T. ) ;
#24636 = CARTESIAN_POINT ( 'NONE',  ( 7.499999999999961808, -20.94781430457061333, 5.000000000000000000 ) ) ;
#24637 = CARTESIAN_POINT ( 'NONE',  ( 0.000000000000000000, 0.000000000000000000, 5.000000000000000000 ) ) ;
#24638 = DIRECTION ( 'NONE',  ( 0.000000000000000000, 0.000000000000000000, 1.000000000000000000 ) ) ;
#24639 = DIRECTION ( 'NONE',  ( -0.7071067811865486830, -0.7071067811865464625, -0.000000000000000000 ) ) ;
#24640 = CARTESIAN_POINT ( 'NONE',  ( 18.06011071044008887, -9.740707523384184441, 10.89222023123376637 ) ) ;
#24641 = CARTESIAN_POINT ( 'NONE',  ( 0.000000000000000000, -14.29000000000013593, 12.69999999999954632 ) ) ;
#24642 = VERTEX_POINT ( 'NONE', #79470 ) ;
#24643 = ORIENTED_EDGE ( 'NONE', *, *, #11504, .F. ) ;
#24644 = CARTESIAN_POINT ( 'NONE',  ( 112.1462635252314328, -4.472830434245840259, 4.472830434245839371 ) ) ;
#24645 = VECTOR ( 'NONE', #38305, 1000.000000000000000 ) ;
#24646 = VERTEX_POINT ( 'NONE', #67871 ) ;
#24647 = EDGE_CURVE ( 'NONE', #142592, #47990, #46101, .T. ) ;
#24648 = CARTESIAN_POINT ( 'NONE',  ( 99.14583333333334281, 2.130196079827470168, -7.949999999999977973 ) ) ;
#24649 =( GEOMETRIC_REPRESENTATION_CONTEXT ( 3 ) GLOBAL_UNCERTAINTY_ASSIGNED_CONTEXT ( ( #47480 ) ) GLOBAL_UNIT_ASSIGNED_CONTEXT ( ( #9837, #92205, #132378 ) ) REPRESENTATION_CONTEXT ( 'NONE', 'WORKASPACE' ) );
#24650 = SURFACE_STYLE_FILL_AREA ( #34841 ) ;
#24651 = EDGE_CURVE ( 'NONE', #101509, #63240, #89572, .T. ) ;
#24652 = CARTESIAN_POINT ( 'NONE',  ( -26.16347128873434258, 15.75929247661555443, 9.299976744542860274 ) ) ;
#24653 = FACE_OUTER_BOUND ( 'NONE', #128890, .T. ) ;
#24654 = CARTESIAN_POINT ( 'NONE',  ( 117.8912635252314516, -4.472830434245839371, -4.472830434245839371 ) ) ;
#24655 = ORIENTED_EDGE ( 'NONE', *, *, #10182, .F. ) ;
#24656 = ORIENTED_EDGE ( 'NONE', *, *, #59710, .F. ) ;
#24657 = DIRECTION ( 'NONE',  ( 0.000000000000000000, 0.000000000000000000, -1.000000000000000000 ) ) ;
#24658 = VECTOR ( 'NONE', #76524, 1000.000000000000000 ) ;
#24659 = EDGE_CURVE ( 'NONE', #41224, #6884, #46845, .T. ) ;
#24660 = FACE_OUTER_BOUND ( 'NONE', #103978, .T. ) ;
#24661 = VERTEX_POINT ( 'NONE', #13413 ) ;
#24662 = VERTEX_POINT ( 'NONE', #91032 ) ;
#24663 = ORIENTED_EDGE ( 'NONE', *, *, #142448, .F. ) ;
#24664 = LINE ( 'NONE', #113822, #127867 ) ;
#24665 = CARTESIAN_POINT ( 'NONE',  ( 0.9420698081018860082, 7.934999999999992504, 2.126176841940951689 ) ) ;
#24666 = VECTOR ( 'NONE', #88927, 1000.000000000000000 ) ;
#24667 = B_SPLINE_CURVE_WITH_KNOTS ( 'NONE', 3,
 ( #48532, #81178, #134128, #113056 ),
 .UNSPECIFIED., .F., .F.,
 ( 4, 4 ),
 ( 0.001163520961193752548, 0.001596196080316615801 ),
 .UNSPECIFIED. ) ;
#24668 = CARTESIAN_POINT ( 'NONE',  ( 31.55793019189810522, 6.110000000000000320, -1.637169565754156064 ) ) ;
#24669 = ORIENTED_EDGE ( 'NONE', *, *, #55004, .F. ) ;
#24670 = AXIS2_PLACEMENT_3D ( 'NONE', #35422, #34680, #24495 ) ;
#24671 = VERTEX_POINT ( 'NONE', #40225 ) ;
#24672 = ADVANCED_FACE ( 'NONE', ( #94550 ), #84439, .F. ) ;
#24673 = LINE ( 'NONE', #59484, #15456 ) ;
#24674 = ORIENTED_EDGE ( 'NONE', *, *, #1920, .T. ) ;
#24675 = ORIENTED_EDGE ( 'NONE', *, *, #35226, .T. ) ;
#24676 = EDGE_LOOP ( 'NONE', ( #63927, #137795, #19708, #93918 ) ) ;
#24677 = ADVANCED_FACE ( 'NONE', ( #72150 ), #95276, .T. ) ;
#24678 = EDGE_CURVE ( 'NONE', #143427, #116147, #29305, .T. ) ;
#24679 = CARTESIAN_POINT ( 'NONE',  ( 15.48921356237309510, -27.52281430457066236, 5.000000000000000000 ) ) ;
#24680 = CARTESIAN_POINT ( 'NONE',  ( 0.000000000000000000, -21.72500000000000142, 0.000000000000000000 ) ) ;
#24681 = CARTESIAN_POINT ( 'NONE',  ( 24.56840764549667355, 9.139736423841732040E-16, 0.000000000000000000 ) ) ;
#24682 = VERTEX_POINT ( 'NONE', #6088 ) ;
#24683 = CARTESIAN_POINT ( 'NONE',  ( 5.999999999999950262, -22.22500000000000853, 4.412002311790033104 ) ) ;
#24684 = CIRCLE ( 'NONE', #105686, 2.500000000000000444 ) ;
#24685 = DIRECTION ( 'NONE',  ( -0.7071067811865486830, -0.7071067811865464625, 0.000000000000000000 ) ) ;
#24686 = ADVANCED_FACE ( 'NONE', ( #82291 ), #38766, .F. ) ;
#24687 = FACE_BOUND ( 'NONE', #54559, .T. ) ;
#24689 = FACE_BOUND ( 'NONE', #21002, .T. ) ;
#24688 = AXIS2_PLACEMENT_3D ( 'NONE', #51798, #121308, #75682 ) ;
#24690 = EDGE_CURVE ( 'NONE', #28705, #37784, #4636, .T. ) ;
#24691 = ORIENTED_EDGE ( 'NONE', *, *, #50913, .T. ) ;
#24692 = CARTESIAN_POINT ( 'NONE',  ( 184.1500000000000057, -43.14999999999999147, 40.92499999999998295 ) ) ;
#24693 = CARTESIAN_POINT ( 'NONE',  ( 3.730677800976791136, -52.14999999999999147, 40.92499999999998295 ) ) ;
#24694 = DIRECTION ( 'NONE',  ( 1.000000000000000000, 0.000000000000000000, 0.000000000000000000 ) ) ;
#24695 = ADVANCED_FACE ( 'NONE', ( #103987 ), #17697, .F. ) ;
#24696 = ORIENTED_EDGE ( 'NONE', *, *, #80401, .T. ) ;
#24697 = LINE ( 'NONE', #4301, #18040 ) ;
#24698 = ORIENTED_EDGE ( 'NONE', *, *, #33045, .F. ) ;
#24699 = VERTEX_POINT ( 'NONE', #117710 ) ;
#24700 = VECTOR ( 'NONE', #54139, 999.9999999999998863 ) ;
#24701 = ORIENTED_EDGE ( 'NONE', *, *, #5743, .F. ) ;
#24702 = VECTOR ( 'NONE', #96498, 1000.000000000000000 ) ;
#24703 = VECTOR ( 'NONE', #72304, 1000.000000000000000 ) ;
#24704 = CARTESIAN_POINT ( 'NONE',  ( 39.14126352523145158, 4.472830434245835818, 4.472830434245840259 ) ) ;
#24705 = EDGE_CURVE ( 'NONE', #129502, #4418, #61968, .T. ) ;
#24706 = VERTEX_POINT ( 'NONE', #27162 ) ;
#24707 = EDGE_CURVE ( 'NONE', #109252, #62370, #114861, .T. ) ;
#24708 = DIRECTION ( 'NONE',  ( 1.000000000000000000, 1.224606353822377258E-16, 0.000000000000000000 ) ) ;
#24709 = DIRECTION ( 'NONE',  ( -1.000000000000000000, -0.000000000000000000, -0.000000000000000000 ) ) ;
#24710 = ORIENTED_EDGE ( 'NONE', *, *, #137724, .T. ) ;
#24711 = FILL_AREA_STYLE_COLOUR ( '', #95401 ) ;
#24712 = CARTESIAN_POINT ( 'NONE',  ( -31.17183060077625356, 21.75929247661549581, 4.000000000000000000 ) ) ;
#24713 = AXIS2_PLACEMENT_3D ( 'NONE', #44074, #36748, #57824 ) ;
#24714 = EDGE_CURVE ( 'NONE', #73986, #13719, #117434, .T. ) ;
#24715 = DIRECTION ( 'NONE',  ( 1.000000000000000000, 3.115803279706882722E-16, 0.000000000000000000 ) ) ;
#24716 = CARTESIAN_POINT ( 'NONE',  ( 30.70710678118632941, -18.74070752338409207, 5.000000000000000000 ) ) ;
#24717 = DIRECTION ( 'NONE',  ( -0.7071067811865487940, 0.7071067811865463515, -0.000000000000000000 ) ) ;
#24718 = DIRECTION ( 'NONE',  ( -0.7071067811865486830, -0.7071067811865464625, 0.000000000000000000 ) ) ;
#24719 = VERTEX_POINT ( 'NONE', #39496 ) ;
#24720 = VERTEX_POINT ( 'NONE', #18401 ) ;
#24722 = ORIENTED_EDGE ( 'NONE', *, *, #2904, .T. ) ;
#24721 = ADVANCED_FACE ( 'NONE', ( #83730 ), #73547, .F. ) ;
#24723 = ORIENTED_EDGE ( 'NONE', *, *, #104739, .T. ) ;
#24724 = CARTESIAN_POINT ( 'NONE',  ( 21.62762920772360786, 8.558752285115851066, 4.000000000000000000 ) ) ;
#24725 = VERTEX_POINT ( 'NONE', #51801 ) ;
#24726 = ORIENTED_EDGE ( 'NONE', *, *, #30605, .F. ) ;
#24727 = FACE_OUTER_BOUND ( 'NONE', #15466, .T. ) ;
#24728 = CARTESIAN_POINT ( 'NONE',  ( 34.82816939922328459, 12.75929247661558996, 4.000000000000000000 ) ) ;
#24729 = EDGE_LOOP ( 'NONE', ( #4254, #138901, #38874, #65835 ) ) ;
#24731 = ADVANCED_FACE ( 'NONE', ( #27879 ), #95985, .F. ) ;
#24730 = VECTOR ( 'NONE', #58494, 1000.000000000000000 ) ;
#24732 = PLANE ( 'NONE',  #60383 ) ;
#24733 = VERTEX_POINT ( 'NONE', #60553 ) ;
#24734 = CARTESIAN_POINT ( 'NONE',  ( 14.39532882439692862, 4.202752102959690472E-16, 0.000000000000000000 ) ) ;
#24735 = EDGE_CURVE ( 'NONE', #68652, #2255, #40911, .T. ) ;
#24736 = CARTESIAN_POINT ( 'NONE',  ( 26.17123647476855908, 0.000000000000000000, 7.934999999999990727 ) ) ;
#24737 = VECTOR ( 'NONE', #27874, 1000.000000000000000 ) ;
#24738 = PLANE ( 'NONE',  #92393 ) ;
#24739 = ORIENTED_EDGE ( 'NONE', *, *, #57916, .T. ) ;
#24741 = CARTESIAN_POINT ( 'NONE',  ( 9.792893218813391698, 15.75929247661555976, 5.000000000000000000 ) ) ;
#24740 = CARTESIAN_POINT ( 'NONE',  ( 112.7870968585647802, 3.054999999999997939, 5.291415217122920289 ) ) ;
#24742 =( BOUNDED_CURVE ( )  B_SPLINE_CURVE ( 3, ( #83747, #29316, #136651, #4657 ),
 .UNSPECIFIED., .F., .T. ) 
 B_SPLINE_CURVE_WITH_KNOTS ( ( 4, 4 ),
 ( 1.901594255663616728, 1.933014472006574280 ),
 .UNSPECIFIED. ) 
 CURVE ( )  GEOMETRIC_REPRESENTATION_ITEM ( )  RATIONAL_B_SPLINE_CURVE ( ( 1.000000000000000000, 0.9999177325257867510, 0.9999177325257867510, 1.000000000000000000 ) ) 
 REPRESENTATION_ITEM ( '' )  );
#24743 = DIRECTION ( 'NONE',  ( 0.6830127018922181881, 0.6830127018922202975, -0.2588190451025214056 ) ) ;
#24744 = CARTESIAN_POINT ( 'NONE',  ( -22.49999999999984368, 21.43112307739195899, 4.000000000000000000 ) ) ;
#24745 = ORIENTED_EDGE ( 'NONE', *, *, #21542, .F. ) ;
#24746 = LINE ( 'NONE', #43648, #26384 ) ;
#24748 = EDGE_LOOP ( 'NONE', ( #44816, #77947, #87247, #10735, #10628, #2405 ) ) ;
#24747 = CARTESIAN_POINT ( 'NONE',  ( -23.99451991528749062, 28.92564299267954908, 4.000000000000000000 ) ) ;
#24749 = PRESENTATION_LAYER_ASSIGNMENT (  '', '', ( #17696 ) ) ;
#24750 = DIRECTION ( 'NONE',  ( 1.000000000000000000, 0.000000000000000000, 0.000000000000000000 ) ) ;
#24751 = ORIENTED_EDGE ( 'NONE', *, *, #99589, .T. ) ;
#24752 = FACE_OUTER_BOUND ( 'NONE', #138791, .T. ) ;
#24754 = ADVANCED_FACE ( 'NONE', ( #28623 ), #129325, .T. ) ;
#24753 = LINE ( 'NONE', #35680, #135661 ) ;
#24755 = CARTESIAN_POINT ( 'NONE',  ( -24.18398860626899705, 28.73617430169804265, 5.000000000000000000 ) ) ;
#24756 = CARTESIAN_POINT ( 'NONE',  ( -12.69999999999998153, 0.000000000000000000, 0.000000000000000000 ) ) ;
#24757 = ORIENTED_EDGE ( 'NONE', *, *, #56337, .T. ) ;
#24758 = LINE ( 'NONE', #112489, #122354 ) ;
#24759 = LINE ( 'NONE', #111025, #27999 ) ;
#24760 = CYLINDRICAL_SURFACE ( 'NONE', #118492, 5.968999999999998529 ) ;
#24761 = VECTOR ( 'NONE', #121079, 1000.000000000000000 ) ;
#24762 = ORIENTED_EDGE ( 'NONE', *, *, #74947, .T. ) ;
#24763 = CARTESIAN_POINT ( 'NONE',  ( 14.99999999999989875, 2.342191155542461267, -5.001666872980119471 ) ) ;
#24764 = ORIENTED_EDGE ( 'NONE', *, *, #20831, .T. ) ;
#24765 = VECTOR ( 'NONE', #117379, 1000.000000000000000 ) ;
#24767 = ORIENTED_EDGE ( 'NONE', *, *, #72494, .F. ) ;
#24766 = LINE ( 'NONE', #93604, #37101 ) ;
#24768 = EDGE_LOOP ( 'NONE', ( #53099, #116561, #25080 ) ) ;
#24769 = CARTESIAN_POINT ( 'NONE',  ( 7.166003870700648370, 12.55858695562843330, -25.25459431962041634 ) ) ;
#24770 = CARTESIAN_POINT ( 'NONE',  ( 30.79289321881324781, 9.759292476615627265, 5.000000000000000000 ) ) ;
#24771 = ORIENTED_EDGE ( 'NONE', *, *, #15946, .T. ) ;
#24772 = VECTOR ( 'NONE', #114569, 999.9999999999998863 ) ;
#24773 = CARTESIAN_POINT ( 'NONE',  ( 12.18398860626900060, 28.73617430169795739, 5.000000000000000000 ) ) ;
#24774 = ORIENTED_EDGE ( 'NONE', *, *, #35547, .T. ) ;
#24775 = CARTESIAN_POINT ( 'NONE',  ( -24.12147316337132352, -20.24070752338407786, 7.412974875817845977 ) ) ;
#24776 = ADVANCED_FACE ( 'NONE', ( #138080 ), #32172, .T. ) ;
#24777 = DIRECTION ( 'NONE',  ( 0.3543493200069162685, -0.000000000000000000, -0.9351131265310288487 ) ) ;
#24778 = CARTESIAN_POINT ( 'NONE',  ( 104.2500000000000000, -9.735942053221458872E-16, 7.950000000000000178 ) ) ;
#24779 = CARTESIAN_POINT ( 'NONE',  ( 36.48921356237310221, -27.52281430457080802, 5.000000000000000000 ) ) ;
#24780 = CARTESIAN_POINT ( 'NONE',  ( 126.3673795226528682, -7.080845498744676725, -0.3407821965100499839 ) ) ;
#24781 = DIRECTION ( 'NONE',  ( 0.3543493200069162685, -0.000000000000000000, -0.9351131265310288487 ) ) ;
#24782 = ORIENTED_EDGE ( 'NONE', *, *, #74786, .T. ) ;
#24783 = EDGE_LOOP ( 'NONE', ( #122449, #74990, #58078, #111229 ) ) ;
#24785 = EDGE_CURVE ( 'NONE', #23453, #93248, #118590, .T. ) ;
#24784 = EDGE_LOOP ( 'NONE', ( #1330, #54795, #91454, #104250 ) ) ;
#24786 = CARTESIAN_POINT ( 'NONE',  ( 122.7708333333333286, -7.949999999999999289, -2.130196079827426203 ) ) ;
#24787 = ORIENTED_EDGE ( 'NONE', *, *, #113327, .F. ) ;
#24788 = ORIENTED_EDGE ( 'NONE', *, *, #97316, .F. ) ;
#24789 = ORIENTED_EDGE ( 'NONE', *, *, #24560, .F. ) ;
#24790 = CARTESIAN_POINT ( 'NONE',  ( 0.2168868938212059061, -7.334364015408722182, 2.940725648025187766 ) ) ;
#24791 = CARTESIAN_POINT ( 'NONE',  ( -60.29974487139158867, -27.71228299555248142, 4.000000000000000000 ) ) ;
#24792 = EDGE_LOOP ( 'NONE', ( #39357, #33755, #123387, #72207 ) ) ;
#24793 = DIRECTION ( 'NONE',  ( -0.000000000000000000, 0.3543493200069153248, 0.9351131265310292928 ) ) ;
#24794 = CARTESIAN_POINT ( 'NONE',  ( 18.70710678118641468, -9.740707523384177335, 5.000000000000000000 ) ) ;
#24795 = EDGE_CURVE ( 'NONE', #110391, #43579, #10397, .T. ) ;
#24796 = FACE_OUTER_BOUND ( 'NONE', #81252, .T. ) ;
#24797 = VECTOR ( 'NONE', #111879, 1000.000000000000000 ) ;
#24798 = LINE ( 'NONE', #2301, #83568 ) ;
#24799 = CARTESIAN_POINT ( 'NONE',  ( 118.5629301918981042, 1.637169565754157174, 6.110000000000002984 ) ) ;
#24800 = ADVANCED_FACE ( 'NONE', ( #209 ), #32916, .F. ) ;
#24801 = ORIENTED_EDGE ( 'NONE', *, *, #79162, .F. ) ;
#24802 = LINE ( 'NONE', #12493, #69659 ) ;
#24803 = CARTESIAN_POINT ( 'NONE',  ( -51.48921356237309510, -27.52281430457091460, 5.000000000000000000 ) ) ;
#24804 = CARTESIAN_POINT ( 'NONE',  ( 6.183988606268994381, 28.73617430169791476, 5.000000000000000000 ) ) ;
#24805 = LINE ( 'NONE', #102402, #71391 ) ;
#24806 = LINE ( 'NONE', #115346, #82257 ) ;
#24807 = EDGE_CURVE ( 'NONE', #107783, #2199, #110416, .T. ) ;
#24808 = AXIS2_PLACEMENT_3D ( 'NONE', #41620, #108264, #53961 ) ;
#24809 = DIRECTION ( 'NONE',  ( -0.7071067811865486830, -0.7071067811865464625, 0.000000000000000000 ) ) ;
#24810 = DIRECTION ( 'NONE',  ( 0.5735764363510448272, -0.8191520442889927978, 1.003171929053526103E-16 ) ) ;
#24812 = EDGE_CURVE ( 'NONE', #57387, #136867, #118449, .T. ) ;
#24811 = VECTOR ( 'NONE', #120958, 1000.000000000000227 ) ;
#24814 = ADVANCED_FACE ( 'NONE', ( #43069 ), #108988, .F. ) ;
#24813 = CARTESIAN_POINT ( 'NONE',  ( 44.12086038379622721, -6.884901960086286188, 3.974999999999997424 ) ) ;
#24815 = LINE ( 'NONE', #66901, #120837 ) ;
#24816 = VECTOR ( 'NONE', #10199, 999.9999999999998863 ) ;
#24817 = CARTESIAN_POINT ( 'NONE',  ( 15.48921356237309510, -27.52281430457066236, 5.000000000000000000 ) ) ;
#24818 = ORIENTED_EDGE ( 'NONE', *, *, #46441, .F. ) ;
#24819 = ORIENTED_EDGE ( 'NONE', *, *, #54793, .T. ) ;
#24820 = CARTESIAN_POINT ( 'NONE',  ( 37.02083333333332149, 7.949999999999999289, 2.130196079827431532 ) ) ;
#24821 = VERTEX_POINT ( 'NONE', #99542 ) ;
#24822 = ADVANCED_FACE ( 'NONE', ( #142376 ), #11092, .F. ) ;
#24823 = CARTESIAN_POINT ( 'NONE',  ( 11.51078643762690490, -27.52281430457047406, 5.000000000000000000 ) ) ;
#24824 = AXIS2_PLACEMENT_3D ( 'NONE', #102040, #89728, #47006 ) ;
#24825 = VECTOR ( 'NONE', #61942, 1000.000000000000227 ) ;
#24826 = EDGE_LOOP ( 'NONE', ( #19906, #90876, #83230, #124829, #66858, #44857, #32174, #94810, #11706, #13472, #6778, #137535, #129058, #23040, #1703, #103612, #107448, #29737, #27327, #31153, #85027, #32216, #111106, #54212, #30347, #97092, #35556, #47882, #15222, #32773, #35666, #66403, #25892, #135592, #140142, #141247, #56332, #112819, #75625, #10544, #65313, #139754, #11477, #32261, #104541, #45613, #24674, #12592, #14813, #129991, #121483, #80789, #8407, #110097, #61779, #110023, #138499, #18135, #119506, #131579, #107451, #77975, #13204, #52, #57985, #113303 ) ) ;
#24827 = DIRECTION ( 'NONE',  ( 0.000000000000000000, -1.000000000000000000, 0.000000000000000000 ) ) ;
#24828 = LINE ( 'NONE', #111093, #46888 ) ;
#24829 = ADVANCED_FACE ( 'NONE', ( #131489 ), #140913, .F. ) ;
#24830 = CARTESIAN_POINT ( 'NONE',  ( 35.58376352523143282, -6.110000000000001208, -3.741295971395164515E-16 ) ) ;
#24831 = ORIENTED_EDGE ( 'NONE', *, *, #76517, .F. ) ;
#24832 = DIRECTION ( 'NONE',  ( 2.781805975412905890E-17, -0.3543493200069152693, 0.9351131265310292928 ) ) ;
#24833 = VERTEX_POINT ( 'NONE', #120567 ) ;
#24834 = CARTESIAN_POINT ( 'NONE',  ( 8.999999999999934275, 19.55218569542897100, 5.000000000000000000 ) ) ;
#24835 = EDGE_CURVE ( 'NONE', #98296, #5341, #143070, .T. ) ;
#24836 = CARTESIAN_POINT ( 'NONE',  ( 21.59770000000000678, 3.130000000000007887, -2.396719511207313368E-16 ) ) ;
#24837 = DIRECTION ( 'NONE',  ( -0.6830127018922180770, -0.6830127018922204085, -0.2588190451025213501 ) ) ;
#24838 = DIRECTION ( 'NONE',  ( 0.6830127018922180770, -0.6830127018922204085, -0.2588190451025213501 ) ) ;
#24839 = EDGE_LOOP ( 'NONE', ( #52875, #93709, #109898, #83200 ) ) ;
#24840 = PLANE ( 'NONE',  #23352 ) ;
#24841 = ORIENTED_EDGE ( 'NONE', *, *, #27571, .F. ) ;
#24842 = CARTESIAN_POINT ( 'NONE',  ( 0.000000000000000000, 9.913515839097813477E-16, -8.094999999999991758 ) ) ;
#24843 = LINE ( 'NONE', #1625, #2222 ) ;
#24844 = DIRECTION ( 'NONE',  ( 0.3543493200069162685, -0.000000000000000000, -0.9351131265310288487 ) ) ;
#24845 = CIRCLE ( 'NONE', #96521, 2.500000000000000444 ) ;
#24846 = ADVANCED_FACE ( 'NONE', ( #64812 ), #53194, .F. ) ;
#24847 = CARTESIAN_POINT ( 'NONE',  ( 57.29974487139158157, -27.71228299555246011, 4.000000000000000000 ) ) ;
#24848 = CARTESIAN_POINT ( 'NONE',  ( -30.12147316337128800, -20.24070752338407431, 7.412974875817861076 ) ) ;
#24849 = VECTOR ( 'NONE', #75255, 1000.000000000000000 ) ;
#24850 = LINE ( 'NONE', #84088, #87091 ) ;
#24851 = CARTESIAN_POINT ( 'NONE',  ( 61.30793019189810877, -6.109999999999998543, 1.637169565754158063 ) ) ;
#24852 = LINE ( 'NONE', #122005, #9305 ) ;
#24853 = ADVANCED_FACE ( 'NONE', ( #130063 ), #21297, .F. ) ;
#24854 = LINE ( 'NONE', #69098, #38688 ) ;
#24855 = ORIENTED_EDGE ( 'NONE', *, *, #70977, .T. ) ;
#24856 = ORIENTED_EDGE ( 'NONE', *, *, #118944, .T. ) ;
#24857 = CARTESIAN_POINT ( 'NONE',  ( 15.85005128541015118, -8.240707523384193323, 17.25253755692242663 ) ) ;
#24858 = VERTEX_POINT ( 'NONE', #54654 ) ;
#24859 = EDGE_CURVE ( 'NONE', #71177, #59824, #43762, .T. ) ;
#24860 = EDGE_CURVE ( 'NONE', #125463, #35816, #63411, .T. ) ;
#24861 = CARTESIAN_POINT ( 'NONE',  ( -63.18398860626900415, 28.73617430169831621, 5.000000000000000000 ) ) ;
#24862 = ORIENTED_EDGE ( 'NONE', *, *, #37969, .T. ) ;
#24863 = DIRECTION ( 'NONE',  ( -1.000000000000000000, -1.192622389734054877E-16, 0.000000000000000000 ) ) ;
#24864 = AXIS2_PLACEMENT_3D ( 'NONE', #139116, #48525, #105039 ) ;
#24865 = EDGE_CURVE ( 'NONE', #65337, #23121, #64547, .T. ) ;
#24866 = FACE_OUTER_BOUND ( 'NONE', #38042, .T. ) ;
#24867 = FACE_BOUND ( 'NONE', #60484, .T. ) ;
#24868 = EDGE_CURVE ( 'NONE', #97631, #28308, #119167, .T. ) ;
#24869 = CARTESIAN_POINT ( 'NONE',  ( 34.42500000000002558, -22.26999999999999247, -37.00000000000000000 ) ) ;
#24870 = CARTESIAN_POINT ( 'NONE',  ( 0.000000000000000000, 0.000000000000000000, 5.000000000000000000 ) ) ;
#24872 = ORIENTED_EDGE ( 'NONE', *, *, #117840, .T. ) ;
#24871 = DIRECTION ( 'NONE',  ( -0.7071067811865486830, -0.7071067811865464625, 0.000000000000000000 ) ) ;
#24873 = VERTEX_POINT ( 'NONE', #133636 ) ;
#24874 = DIRECTION ( 'NONE',  ( -0.000000000000000000, 0.000000000000000000, 1.000000000000000000 ) ) ;
#24875 = EDGE_LOOP ( 'NONE', ( #63111, #78593, #113323, #10872, #54122 ) ) ;
#24876 = ORIENTED_EDGE ( 'NONE', *, *, #15736, .T. ) ;
#24877 = CARTESIAN_POINT ( 'NONE',  ( 75.30793019189810877, -6.109999999999998543, 1.637169565754158507 ) ) ;
#24878 = ORIENTED_EDGE ( 'NONE', *, *, #119415, .T. ) ;
#24879 = CIRCLE ( 'NONE', #98963, 9.000000000000001776 ) ;
#24880 = ADVANCED_FACE ( 'NONE', ( #1642 ), #89406, .T. ) ;
#24881 = FACE_OUTER_BOUND ( 'NONE', #10172, .T. ) ;
#24882 = VERTEX_POINT ( 'NONE', #14701 ) ;
#24883 = CARTESIAN_POINT ( 'NONE',  ( 1.516262732464673135, 2.500000000000000888, 3.061616997868384127E-16 ) ) ;
#24884 = ADVANCED_FACE ( 'NONE', ( #11814 ), #111881, .F. ) ;
#24885 = DIRECTION ( 'NONE',  ( 0.6830127018922181881, 0.6830127018922202975, -0.2588190451025214056 ) ) ;
#24886 = DIRECTION ( 'NONE',  ( -0.7071067811865486830, -0.7071067811865464625, 0.000000000000000000 ) ) ;
#24887 = DIRECTION ( 'NONE',  ( -1.000000000000000000, -0.000000000000000000, -0.000000000000000000 ) ) ;
#24888 = DIRECTION ( 'NONE',  ( -0.7071067811865487940, 0.7071067811865463515, -0.000000000000000000 ) ) ;
#24889 = DIRECTION ( 'NONE',  ( -0.3543493200069162685, -0.000000000000000000, -0.9351131265310288487 ) ) ;
#24890 = ORIENTED_EDGE ( 'NONE', *, *, #20739, .T. ) ;
#24891 = ORIENTED_EDGE ( 'NONE', *, *, #105358, .F. ) ;
#24892 = DIRECTION ( 'NONE',  ( -2.781805975412905890E-17, 0.3543493200069152693, 0.9351131265310292928 ) ) ;
#24894 = DIRECTION ( 'NONE',  ( -0.7071067811865486830, 0.7071067811865464625, 0.000000000000000000 ) ) ;
#24893 = AXIS2_PLACEMENT_3D ( 'NONE', #68112, #135481, #114414 ) ;
#24895 = ORIENTED_EDGE ( 'NONE', *, *, #121383, .T. ) ;
#24896 = VERTEX_POINT ( 'NONE', #35780 ) ;
#24898 = EDGE_LOOP ( 'NONE', ( #122667, #93359, #83336, #2161 ) ) ;
#24897 = VECTOR ( 'NONE', #16273, 1000.000000000000000 ) ;
#24899 = CARTESIAN_POINT ( 'NONE',  ( 25.08376352523143638, -6.110000000000001208, -3.741295971395164515E-16 ) ) ;
#24900 = EDGE_LOOP ( 'NONE', ( #100331, #45757, #104997, #109498 ) ) ;
#24901 = LINE ( 'NONE', #32971, #141265 ) ;
#24902 = VECTOR ( 'NONE', #39894, 1000.000000000000000 ) ;
#24903 = AXIS2_PLACEMENT_3D ( 'NONE', #138650, #14716, #27727 ) ;
#24904 = EDGE_CURVE ( 'NONE', #115656, #127118, #56101, .T. ) ;
#24905 = VECTOR ( 'NONE', #117871, 1000.000000000000000 ) ;
#24906 = CARTESIAN_POINT ( 'NONE',  ( 0.3587364747685527488, 5.808823158059031044, -5.808823158059038150 ) ) ;
#24907 = LINE ( 'NONE', #14017, #10156 ) ;
#24908 = ORIENTED_EDGE ( 'NONE', *, *, #113493, .F. ) ;
#24909 = LINE ( 'NONE', #134412, #68955 ) ;
#24910 = DIRECTION ( 'NONE',  ( -0.000000000000000000, 0.000000000000000000, 1.000000000000000000 ) ) ;
#24911 = VECTOR ( 'NONE', #98322, 1000.000000000000000 ) ;
#24912 = PLANE ( 'NONE',  #91478 ) ;
#24914 = VERTEX_POINT ( 'NONE', #13959 ) ;
#24913 = DIRECTION ( 'NONE',  ( -0.000000000000000000, -0.3543493200069152693, 0.9351131265310292928 ) ) ;
#24915 = EDGE_LOOP ( 'NONE', ( #134550, #8420, #63874, #102184 ) ) ;
#24916 = PLANE ( 'NONE',  #93542 ) ;
#24917 = LINE ( 'NONE', #126372, #37623 ) ;
#24918 = CARTESIAN_POINT ( 'NONE',  ( 10.49999999999993250, 3.073033219394637250, -6.593910359670946519 ) ) ;
#24919 = ORIENTED_EDGE ( 'NONE', *, *, #24367, .F. ) ;
#24920 = PLANE ( 'NONE',  #3897 ) ;
#24921 = CARTESIAN_POINT ( 'NONE',  ( 28.12499999999999645, -7.950000000000000178, -4.867971026610729436E-16 ) ) ;
#24922 = PLANE ( 'NONE',  #100394 ) ;
#24923 = ORIENTED_EDGE ( 'NONE', *, *, #11600, .T. ) ;
#24924 = DIRECTION ( 'NONE',  ( 4.681814790819592407E-17, 0.3543493200069153248, 0.9351131265310292928 ) ) ;
#24925 = CARTESIAN_POINT ( 'NONE',  ( 34.92500000000002558, -21.76999999999999247, -37.00000000000000000 ) ) ;
#24926 = FACE_OUTER_BOUND ( 'NONE', #105562, .T. ) ;
#24927 = CARTESIAN_POINT ( 'NONE',  ( -42.48921356237308800, -27.52281430457085065, 5.000000000000000000 ) ) ;
#24928 = DIRECTION ( 'NONE',  ( -0.3543493200069162685, -0.000000000000000000, -0.9351131265310288487 ) ) ;
#24929 = ORIENTED_EDGE ( 'NONE', *, *, #27127, .F. ) ;
#24930 = ORIENTED_EDGE ( 'NONE', *, *, #99993, .T. ) ;
#24931 = AXIS2_PLACEMENT_3D ( 'NONE', #79508, #48246, #15570 ) ;
#24932 = FACE_OUTER_BOUND ( 'NONE', #29897, .T. ) ;
#24933 = CARTESIAN_POINT ( 'NONE',  ( 52.26932219902319332, -49.14999999999999147, -40.92499999999998295 ) ) ;
#24934 = CARTESIAN_POINT ( 'NONE',  ( 65.55836038379622721, -7.949999999999996625, -2.130196079827426203 ) ) ;
#24935 = CARTESIAN_POINT ( 'NONE',  ( 22.49999999999984723, -9.462702396500988655, -9.474982329943564707 ) ) ;
#24936 = DIRECTION ( 'NONE',  ( 0.7071067811865487940, -0.7071067811865463515, 0.000000000000000000 ) ) ;
#24937 = CARTESIAN_POINT ( 'NONE',  ( 16.17183060077636014, 15.75929247661555443, 4.000000000000000000 ) ) ;
#24938 = ORIENTED_EDGE ( 'NONE', *, *, #107182, .F. ) ;
#24939 = CARTESIAN_POINT ( 'NONE',  ( 47.03752705046289151, -9.735942053221456900E-16, 7.949999999999998401 ) ) ;
#24940 = DIRECTION ( 'NONE',  ( -0.7071067811865486830, 0.7071067811865464625, 0.000000000000000000 ) ) ;
#24941 = CARTESIAN_POINT ( 'NONE',  ( 52.55793019189811588, 6.110000000000001208, -1.637169565754156286 ) ) ;
#24942 = CARTESIAN_POINT ( 'NONE',  ( 54.18398860626899705, 28.73617430169825226, 5.000000000000000000 ) ) ;
#24943 = CARTESIAN_POINT ( 'NONE',  ( 7.251592354503322291, 3.061616997868379197E-16, -2.500000000000001332 ) ) ;
#24944 = LINE ( 'NONE', #135191, #100 ) ;
#24945 = ORIENTED_EDGE ( 'NONE', *, *, #40546, .F. ) ;
#24946 = CARTESIAN_POINT ( 'NONE',  ( 19.17183060077634593, 18.75929247661552779, 4.000000000000000000 ) ) ;
#24947 = EDGE_LOOP ( 'NONE', ( #29701, #23112, #105287, #88007 ) ) ;
#24948 = CYLINDRICAL_SURFACE ( 'NONE', #77862, 2.500000000000000000 ) ;
#24949 = DIRECTION ( 'NONE',  ( -0.7071067811865486830, -0.7071067811865464625, 0.000000000000000000 ) ) ;
#24951 = ADVANCED_FACE ( 'NONE', ( #102449 ), #34312, .T. ) ;
#24950 = DIRECTION ( 'NONE',  ( -0.7071067811865487940, 0.7071067811865463515, 0.000000000000000000 ) ) ;
#24952 = EDGE_CURVE ( 'NONE', #114916, #115494, #100294, .T. ) ;
#24953 = DIRECTION ( 'NONE',  ( -0.7071067811865486830, -0.7071067811865464625, 0.000000000000000000 ) ) ;
#24954 = DIRECTION ( 'NONE',  ( -0.6830127018922180770, -0.6830127018922204085, -0.2588190451025213501 ) ) ;
#24955 = DIRECTION ( 'NONE',  ( 0.6830127018922181881, 0.6830127018922202975, -0.2588190451025214056 ) ) ;
#24956 = EDGE_CURVE ( 'NONE', #20512, #122084, #112589, .T. ) ;
#24957 = ADVANCED_FACE ( 'NONE', ( #3101 ), #123380, .T. ) ;
#24958 = VERTEX_POINT ( 'NONE', #122010 ) ;
#24959 = EDGE_LOOP ( 'NONE', ( #51243, #76106, #78357, #5440 ) ) ;
#24960 = CARTESIAN_POINT ( 'NONE',  ( -6.299744871391586898, -27.71228299555210484, 4.000000000000000000 ) ) ;
#24961 = DIRECTION ( 'NONE',  ( -0.7071067811865487940, 0.7071067811865463515, 0.000000000000000000 ) ) ;
#24962 = CARTESIAN_POINT ( 'NONE',  ( 15.49238828748955576, 4.584330080086930965E-16, 0.000000000000000000 ) ) ;
#24963 = FACE_OUTER_BOUND ( 'NONE', #32107, .T. ) ;
#24964 = EDGE_CURVE ( 'NONE', #63769, #131639, #48059, .T. ) ;
#24966 = ADVANCED_FACE ( 'NONE', ( #80688 ), #101703, .F. ) ;
#24965 = CARTESIAN_POINT ( 'NONE',  ( 79.70419371712955581, -6.884901960086285300, -3.975000000000000089 ) ) ;
#24967 = DIRECTION ( 'NONE',  ( -0.7071067811865486830, -0.7071067811865464625, -0.000000000000000000 ) ) ;
#24968 = DIRECTION ( 'NONE',  ( -0.7071067811865487940, 0.7071067811865463515, 0.000000000000000000 ) ) ;
#24969 = ORIENTED_EDGE ( 'NONE', *, *, #141668, .T. ) ;
#24970 = AXIS2_PLACEMENT_3D ( 'NONE', #142910, #87811, #10932 ) ;
#24971 = CARTESIAN_POINT ( 'NONE',  ( 74.79166666666667140, 3.975000000000003642, -6.884901960086285300 ) ) ;
#24972 = FACE_OUTER_BOUND ( 'NONE', #35502, .T. ) ;
#24973 = ADVANCED_FACE ( 'NONE', ( #45229 ), #132947, .T. ) ;
#24974 = CARTESIAN_POINT ( 'NONE',  ( -34.47516574401893052, -1.509482387884379939, 4.998110765256835286 ) ) ;
#24975 = CYLINDRICAL_SURFACE ( 'NONE', #14973, 2.500000000000000444 ) ;
#24976 = EDGE_CURVE ( 'NONE', #101876, #109461, #83358, .T. ) ;
#24977 = ORIENTED_EDGE ( 'NONE', *, *, #18314, .T. ) ;
#24978 = LINE ( 'NONE', #26433, #18985 ) ;
#24979 = EDGE_CURVE ( 'NONE', #78390, #4806, #67693, .T. ) ;
#24980 = AXIS2_PLACEMENT_3D ( 'NONE', #142333, #76351, #120518 ) ;
#24981 = CARTESIAN_POINT ( 'NONE',  ( 14.81601139373099585, 28.73617430169776910, 5.000000000000000000 ) ) ;
#24982 = CARTESIAN_POINT ( 'NONE',  ( 65.62543019189810423, 5.291415217122919401, 3.055000000000002824 ) ) ;
#24983 = CARTESIAN_POINT ( 'NONE',  ( -34.49999999999976552, 13.46425560840034841, 4.994342998332165884 ) ) ;
#24984 = ORIENTED_EDGE ( 'NONE', *, *, #79741, .F. ) ;
#24985 = ORIENTED_EDGE ( 'NONE', *, *, #18063, .F. ) ;
#24986 = AXIS2_PLACEMENT_3D ( 'NONE', #59197, #103351, #3999 ) ;
#24987 = CARTESIAN_POINT ( 'NONE',  ( -78.48921356237309510, -27.52281430457109934, 5.000000000000000000 ) ) ;
#24988 = EDGE_CURVE ( 'NONE', #8455, #111687, #134356, .T. ) ;
#24989 = DIRECTION ( 'NONE',  ( -0.6830127018922181881, 0.6830127018922202975, -0.2588190451025214056 ) ) ;
#24990 = VECTOR ( 'NONE', #11106, 1000.000000000000227 ) ;
#24991 = DIRECTION ( 'NONE',  ( -0.000000000000000000, -0.3543493200069152693, 0.9351131265310292928 ) ) ;
#24992 = CARTESIAN_POINT ( 'NONE',  ( -48.18398860626899705, 28.73617430169820608, 5.000000000000000000 ) ) ;
#24994 = VERTEX_POINT ( 'NONE', #135093 ) ;
#24993 = CARTESIAN_POINT ( 'NONE',  ( 55.56056557994608625, -52.00875322212550600, 39.86617647058822200 ) ) ;
#24995 = DIRECTION ( 'NONE',  ( 0.7071067811865487940, 0.7071067811865463515, 0.000000000000000000 ) ) ;
#24996 = LINE ( 'NONE', #23584, #45350 ) ;
#24997 = FACE_OUTER_BOUND ( 'NONE', #72765, .T. ) ;
#24998 = EDGE_CURVE ( 'NONE', #39797, #134968, #123498, .T. ) ;
#24999 = VECTOR ( 'NONE', #15737, 1000.000000000000000 ) ;
#25000 = DIRECTION ( 'NONE',  ( -0.7071067811865487940, 0.7071067811865463515, 0.000000000000000000 ) ) ;
#25001 = AXIS2_PLACEMENT_3D ( 'NONE', #2773, #2020, #46332 ) ;
#25002 = ORIENTED_EDGE ( 'NONE', *, *, #35830, .T. ) ;
#25003 = ORIENTED_EDGE ( 'NONE', *, *, #3823, .T. ) ;
#25004 = CARTESIAN_POINT ( 'NONE',  ( 52.20876352523143282, -7.482591942790329030E-16, 6.110000000000001208 ) ) ;
#25005 = ORIENTED_EDGE ( 'NONE', *, *, #91434, .F. ) ;
#25006 = PLANE ( 'NONE',  #40637 ) ;
#25007 = LINE ( 'NONE', #110580, #98933 ) ;
#25008 = LINE ( 'NONE', #22848, #133628 ) ;
#25009 = EDGE_CURVE ( 'NONE', #8977, #98083, #77826, .T. ) ;
#25010 = DIRECTION ( 'NONE',  ( 0.7071067811865487940, -0.7071067811865463515, 0.000000000000000000 ) ) ;
#25011 = DIRECTION ( 'NONE',  ( 0.000000000000000000, -1.000000000000000000, 0.000000000000000000 ) ) ;
#25012 = ORIENTED_EDGE ( 'NONE', *, *, #69124, .F. ) ;
#25013 = VERTEX_POINT ( 'NONE', #17539 ) ;
#25014 = CARTESIAN_POINT ( 'NONE',  ( 45.18398860626900415, 28.73617430169818832, 5.000000000000000000 ) ) ;
#25015 = SURFACE_SIDE_STYLE ('',( #1116 ) ) ;
#25016 = EDGE_CURVE ( 'NONE', #108338, #86073, #26299, .T. ) ;
#25017 = ORIENTED_EDGE ( 'NONE', *, *, #84533, .F. ) ;
#25019 = EDGE_CURVE ( 'NONE', #120738, #84062, #61123, .T. ) ;
#25018 = ORIENTED_EDGE ( 'NONE', *, *, #36282, .T. ) ;
#25020 = CARTESIAN_POINT ( 'NONE',  ( 111.7875270504628986, 0.000000000000000000, -7.949999999999998401 ) ) ;
#25021 = CARTESIAN_POINT ( 'NONE',  ( -18.48921356237309510, -27.52281430457068367, 5.000000000000000000 ) ) ;
#25023 = EDGE_CURVE ( 'NONE', #37506, #14791, #138633, .T. ) ;
#25022 =( BOUNDED_CURVE ( )  B_SPLINE_CURVE ( 3, ( #141529, #129935, #85692, #30640 ),
 .UNSPECIFIED., .F., .T. ) 
 B_SPLINE_CURVE_WITH_KNOTS ( ( 4, 4 ),
 ( 2.001653308786163876, 3.503810798801451742 ),
 .UNSPECIFIED. ) 
 CURVE ( )  GEOMETRIC_REPRESENTATION_ITEM ( )  RATIONAL_B_SPLINE_CURVE ( ( 1.000000000000000000, 0.8206354192515226131, 0.8206354192515226131, 1.000000000000000000 ) ) 
 REPRESENTATION_ITEM ( '' )  );
#25024 = ORIENTED_EDGE ( 'NONE', *, *, #143287, .T. ) ;
#25026 = EDGE_CURVE ( 'NONE', #35802, #126591, #116144, .T. ) ;
#25025 = AXIS2_PLACEMENT_3D ( 'NONE', #135174, #123590, #14056 ) ;
#25027 = FACE_BOUND ( 'NONE', #10582, .T. ) ;
#25028 = CARTESIAN_POINT ( 'NONE',  ( 0.2569208697893814453, 4.202752102959690472E-16, 0.000000000000000000 ) ) ;
#25029 = FACE_OUTER_BOUND ( 'NONE', #79229, .T. ) ;
#25030 = DIRECTION ( 'NONE',  ( 1.000000000000000000, 0.000000000000000000, 0.000000000000000000 ) ) ;
#25031 = AXIS2_PLACEMENT_3D ( 'NONE', #29006, #20241, #130475 ) ;
#25032 = DIRECTION ( 'NONE',  ( 0.3543493200069162685, -0.000000000000000000, -0.9351131265310288487 ) ) ;
#25033 = LINE ( 'NONE', #98167, #104176 ) ;
#25034 = DIRECTION ( 'NONE',  ( -0.4788050402068163014, -0.3207663868634366144, 0.8172237505916754019 ) ) ;
#25035 = VERTEX_POINT ( 'NONE', #27707 ) ;
#25036 = ORIENTED_EDGE ( 'NONE', *, *, #61925, .T. ) ;
#25037 = CARTESIAN_POINT ( 'NONE',  ( 107.3912635252314516, -4.472830434245838482, -4.472830434245838482 ) ) ;
#25038 = ORIENTED_EDGE ( 'NONE', *, *, #91759, .T. ) ;
#25039 = ADVANCED_FACE ( 'NONE', ( #103812 ), #126314, .T. ) ;
#25040 = CARTESIAN_POINT ( 'NONE',  ( -11.51078643762690490, -27.52281430457047406, 5.000000000000000000 ) ) ;
#25041 = ORIENTED_EDGE ( 'NONE', *, *, #45473, .F. ) ;
#25042 = CARTESIAN_POINT ( 'NONE',  ( 14.99451991528749595, 28.92564299267948513, 4.000000000000000000 ) ) ;
#25043 = VECTOR ( 'NONE', #131167, 1000.000000000000000 ) ;
#25044 = DIRECTION ( 'NONE',  ( -0.000000000000000000, 0.3543493200069153248, 0.9351131265310292928 ) ) ;
#25045 = AXIS2_PLACEMENT_3D ( 'NONE', #33725, #109829, #67050 ) ;
#25046 = CARTESIAN_POINT ( 'NONE',  ( 4.499999999999962697, -1.592773361805368992, -6.492772025301240646 ) ) ;
#25047 = VERTEX_POINT ( 'NONE', #114703 ) ;
#25048 = CARTESIAN_POINT ( 'NONE',  ( 10.49999999999992539, 13.56627193232215767, -10.57019076586066397 ) ) ;
#25049 = FACE_OUTER_BOUND ( 'NONE', #120188, .T. ) ;
#25050 = CARTESIAN_POINT ( 'NONE',  ( 25.40000000000000568, 7.872929591417200612, 1.072287140687521179 ) ) ;
#25051 = CARTESIAN_POINT ( 'NONE',  ( 67.50000000000000000, 0.000000000000000000, -7.950000000000000178 ) ) ;
#25052 = LINE ( 'NONE', #135290, #36889 ) ;
#25053 = DIRECTION ( 'NONE',  ( -0.000000000000000000, -0.3543493200069152693, 0.9351131265310292928 ) ) ;
#25054 = VERTEX_POINT ( 'NONE', #105273 ) ;
#25055 = CARTESIAN_POINT ( 'NONE',  ( -11.99999999999991651, -13.06887692260767686, 4.000000000000000000 ) ) ;
#25056 = CARTESIAN_POINT ( 'NONE',  ( 18.48921356237309510, -27.52281430457068367, 5.000000000000000000 ) ) ;
#25057 = ORIENTED_EDGE ( 'NONE', *, *, #134251, .F. ) ;
#25058 = EDGE_CURVE ( 'NONE', #31872, #104365, #5924, .T. ) ;
#25059 = VERTEX_POINT ( 'NONE', #82833 ) ;
#25060 = VERTEX_POINT ( 'NONE', #50908 ) ;
#25061 = CARTESIAN_POINT ( 'NONE',  ( 53.95876352523143282, 0.000000000000000000, -6.110000000000001208 ) ) ;
#25062 = ORIENTED_EDGE ( 'NONE', *, *, #63698, .T. ) ;
#25063 = CARTESIAN_POINT ( 'NONE',  ( 2.670806282870439308, -3.047499999999997211, -5.278424836066143655 ) ) ;
#25064 = VECTOR ( 'NONE', #22712, 1000.000000000000227 ) ;
#25065 = CARTESIAN_POINT ( 'NONE',  ( 92.31293019189810423, -1.637169565754159617, -6.110000000000001208 ) ) ;
#25066 = LINE ( 'NONE', #123714, #56480 ) ;
#25067 = EDGE_LOOP ( 'NONE', ( #86892, #114399, #64679, #38504 ) ) ;
#25068 = CARTESIAN_POINT ( 'NONE',  ( 30.48921356237309510, -27.52281430457076894, 5.000000000000000000 ) ) ;
#25069 = ORIENTED_EDGE ( 'NONE', *, *, #94390, .F. ) ;
#25070 = DIRECTION ( 'NONE',  ( 0.7071067811865487940, 0.7071067811865463515, 0.000000000000000000 ) ) ;
#25071 = CARTESIAN_POINT ( 'NONE',  ( 25.82816939922334853, 9.759292476615621936, 4.000000000000000000 ) ) ;
#25072 = VERTEX_POINT ( 'NONE', #71244 ) ;
#25073 = EDGE_CURVE ( 'NONE', #86413, #91617, #137921, .T. ) ;
#25074 = FILL_AREA_STYLE_COLOUR ( '', #32882 ) ;
#25075 = FACE_OUTER_BOUND ( 'NONE', #37120, .T. ) ;
#25076 = DIRECTION ( 'NONE',  ( 0.7071067811865486830, -0.7071067811865464625, -0.000000000000000000 ) ) ;
#25077 = VERTEX_POINT ( 'NONE', #115389 ) ;
#25078 = EDGE_CURVE ( 'NONE', #30236, #74065, #60377, .T. ) ;
#25079 = VECTOR ( 'NONE', #3680, 999.9999999999998863 ) ;
#25080 = ORIENTED_EDGE ( 'NONE', *, *, #63935, .T. ) ;
#25081 = VERTEX_POINT ( 'NONE', #94388 ) ;
#25082 = EDGE_LOOP ( 'NONE', ( #82192, #118040, #4137, #6144, #70178, #59676 ) ) ;
#25083 = DIRECTION ( 'NONE',  ( -0.7071067811865486830, -0.7071067811865464625, 0.000000000000000000 ) ) ;
#25084 = VECTOR ( 'NONE', #63063, 1000.000000000000114 ) ;
#25085 = VECTOR ( 'NONE', #54386, 1000.000000000000000 ) ;
#25086 = CARTESIAN_POINT ( 'NONE',  ( 4.171830600776445408, -8.240707523384198652, 4.000000000000000000 ) ) ;
#25087 = VECTOR ( 'NONE', #46113, 1000.000000000000227 ) ;
#25088 = CARTESIAN_POINT ( 'NONE',  ( 3.489213562373097322, -27.52281430457057709, 5.000000000000000000 ) ) ;
#25089 = DIRECTION ( 'NONE',  ( 0.3543493200069162685, -0.000000000000000000, -0.9351131265310288487 ) ) ;
#25090 = EDGE_CURVE ( 'NONE', #3994, #137018, #134973, .T. ) ;
#25091 = VECTOR ( 'NONE', #67210, 999.9999999999998863 ) ;
#25092 = DIRECTION ( 'NONE',  ( 0.000000000000000000, -1.000000000000000000, 0.000000000000000000 ) ) ;
#25093 = VERTEX_POINT ( 'NONE', #83550 ) ;
#25094 = VECTOR ( 'NONE', #37023, 1000.000000000000000 ) ;
#25095 = VECTOR ( 'NONE', #103909, 999.9999999999998863 ) ;
#25096 = DIRECTION ( 'NONE',  ( 0.7071067811865487940, 0.7071067811865463515, -0.000000000000000000 ) ) ;
#25097 = CARTESIAN_POINT ( 'NONE',  ( 25.06206980810188512, -7.934999999999991616, -2.126176841940955242 ) ) ;
#25098 = LINE ( 'NONE', #57066, #36987 ) ;
#25099 = DIRECTION ( 'NONE',  ( -0.000000000000000000, -0.3543493200069152693, 0.9351131265310292928 ) ) ;
#25100 = DIRECTION ( 'NONE',  ( 0.7071067811865487940, 0.7071067811865463515, 0.000000000000000000 ) ) ;
#25101 = ORIENTED_EDGE ( 'NONE', *, *, #92101, .F. ) ;
#25102 = ORIENTED_EDGE ( 'NONE', *, *, #26008, .F. ) ;
#25103 = VERTEX_POINT ( 'NONE', #127757 ) ;
#25104 = DIRECTION ( 'NONE',  ( 0.000000000000000000, 0.000000000000000000, -1.000000000000000000 ) ) ;
#25105 = CARTESIAN_POINT ( 'NONE',  ( 95.30836038379619879, 7.949999999999996625, 2.130196079827431088 ) ) ;
#25106 = VECTOR ( 'NONE', #101615, 1000.000000000000000 ) ;
#25107 = LINE ( 'NONE', #71499, #56729 ) ;
#25108 = CARTESIAN_POINT ( 'NONE',  ( 0.000000000000000000, 0.000000000000000000, 5.000000000000000000 ) ) ;
#25109 = LINE ( 'NONE', #56380, #22301 ) ;
#25111 = CARTESIAN_POINT ( 'NONE',  ( 152.4000000000000057, 7.919999999999947526, -16.42230000000006029 ) ) ;
#25110 = STYLED_ITEM ( 'NONE', ( #99861 ), #95688 ) ;
#25112 = CARTESIAN_POINT ( 'NONE',  ( 42.29974487139158157, -27.71228299555235708, 4.000000000000000000 ) ) ;
#25113 = PLANE ( 'NONE',  #106828 ) ;
#25114 = CARTESIAN_POINT ( 'NONE',  ( -5.510786437626906675, -27.52281430457051314, 5.000000000000000000 ) ) ;
#25115 = DIRECTION ( 'NONE',  ( 0.7071067811865487940, 0.7071067811865463515, 0.000000000000000000 ) ) ;
#25116 = EDGE_LOOP ( 'NONE', ( #56668, #139399, #112357, #5395 ) ) ;
#25117 = VECTOR ( 'NONE', #28907, 1000.000000000000000 ) ;
#25118 = EDGE_CURVE ( 'NONE', #26316, #50236, #28446, .T. ) ;
#25119 = CARTESIAN_POINT ( 'NONE',  ( 16.95443293193746115, -0.6982307342378247794, -35.09649380009672370 ) ) ;
#25120 = ORIENTED_EDGE ( 'NONE', *, *, #120253, .T. ) ;
#25121 = VECTOR ( 'NONE', #67606, 1000.000000000000000 ) ;
#25122 =( GEOMETRIC_REPRESENTATION_CONTEXT ( 3 ) GLOBAL_UNCERTAINTY_ASSIGNED_CONTEXT ( ( #48891 ) ) GLOBAL_UNIT_ASSIGNED_CONTEXT ( ( #35470, #99978, #66641 ) ) REPRESENTATION_CONTEXT ( 'NONE', 'WORKASPACE' ) );
#25123 = CARTESIAN_POINT ( 'NONE',  ( 2.671830600776446740, -21.74070752338405654, 4.000000000000000000 ) ) ;
#25125 = ORIENTED_EDGE ( 'NONE', *, *, #137968, .F. ) ;
#25124 = DIRECTION ( 'NONE',  ( -1.000000000000000000, 4.083240884147117807E-14, 0.000000000000000000 ) ) ;
#25126 = CARTESIAN_POINT ( 'NONE',  ( 2.999999999999999112, -43.14999999999999147, 40.92499999999998295 ) ) ;
#25127 = DIRECTION ( 'NONE',  ( -0.3543493200069162685, -0.000000000000000000, -0.9351131265310288487 ) ) ;
#25128 = ADVANCED_FACE ( 'NONE', ( #104556 ), #116863, .F. ) ;
#25129 = ORIENTED_EDGE ( 'NONE', *, *, #108815, .F. ) ;
#25130 = DIRECTION ( 'NONE',  ( -0.000000000000000000, -0.3543493200069152693, 0.9351131265310292928 ) ) ;
#25131 = VERTEX_POINT ( 'NONE', #48770 ) ;
#25132 = PLANE ( 'NONE',  #25814 ) ;
#25133 = ORIENTED_EDGE ( 'NONE', *, *, #47590, .F. ) ;
#25134 = VECTOR ( 'NONE', #2851, 1000.000000000000000 ) ;
#25135 = CARTESIAN_POINT ( 'NONE',  ( 11.99999999999992184, 7.552185695429091794, 5.000000000000000000 ) ) ;
#25136 = EDGE_CURVE ( 'NONE', #5782, #20512, #139370, .T. ) ;
#25138 = ADVANCED_FACE ( 'NONE', ( #125620 ), #134559, .T. ) ;
#25137 = CARTESIAN_POINT ( 'NONE',  ( 107.8500270504629128, -5.819803920172572198, -5.819803920172572198 ) ) ;
#25139 = FACE_OUTER_BOUND ( 'NONE', #102674, .T. ) ;
#25140 = DIRECTION ( 'NONE',  ( 0.3543493200069162685, -0.000000000000000000, -0.9351131265310288487 ) ) ;
#25142 = EDGE_CURVE ( 'NONE', #112149, #46262, #66443, .T. ) ;
#25141 = ORIENTED_EDGE ( 'NONE', *, *, #72034, .F. ) ;
#25143 = PLANE ( 'NONE',  #9831 ) ;
#25144 = DIRECTION ( 'NONE',  ( 0.7071067811865487940, 0.7071067811865463515, 0.000000000000000000 ) ) ;
#25145 = EDGE_CURVE ( 'NONE', #96120, #102869, #2566, .T. ) ;
#25146 = LINE ( 'NONE', #36743, #13737 ) ;
#25147 = CARTESIAN_POINT ( 'NONE',  ( 21.87500000000000355, -6.094999999999989981, 3.732111120401553285E-16 ) ) ;
#25148 = CARTESIAN_POINT ( 'NONE',  ( 25.20790314143522082, -6.871911579029513106, -3.967499999999993587 ) ) ;
#25149 = VECTOR ( 'NONE', #135852, 1000.000000000000227 ) ;
#25151 = EDGE_CURVE ( 'NONE', #9218, #135984, #40087, .T. ) ;
#25150 = CARTESIAN_POINT ( 'NONE',  ( 17.99451991528748351, 28.92564299267950645, 4.000000000000000000 ) ) ;
#25152 = VERTEX_POINT ( 'NONE', #33128 ) ;
#25153 = AXIS2_PLACEMENT_3D ( 'NONE', #116253, #29233, #52409 ) ;
#25154 = DIRECTION ( 'NONE',  ( 0.7071067811865487940, 0.7071067811865463515, 0.000000000000000000 ) ) ;
#25156 = ORIENTED_EDGE ( 'NONE', *, *, #20587, .F. ) ;
#25155 = ADVANCED_FACE ( 'NONE', ( #101905 ), #78737, .F. ) ;
#25157 = CARTESIAN_POINT ( 'NONE',  ( 96.25043019189810423, 3.055000000000002824, -5.291415217122919401 ) ) ;
#25158 = PLANE ( 'NONE',  #22240 ) ;
#25159 = DIRECTION ( 'NONE',  ( 0.7071067811865486830, -0.7071067811865464625, -0.000000000000000000 ) ) ;
#25160 = FACE_OUTER_BOUND ( 'NONE', #1957, .T. ) ;
#25161 = PLANE ( 'NONE',  #15460 ) ;
#25162 = ORIENTED_EDGE ( 'NONE', *, *, #25985, .T. ) ;
#25163 = CARTESIAN_POINT ( 'NONE',  ( 2.292986735706931345, -21.74070752338405654, 4.999753212805221558 ) ) ;
#25164 = EDGE_CURVE ( 'NONE', #13056, #14650, #35965, .T. ) ;
#25165 = CARTESIAN_POINT ( 'NONE',  ( -7.940000000000001279, -35.14999999999999147, -10.00000000000000178 ) ) ;
#25166 = ORIENTED_EDGE ( 'NONE', *, *, #85, .T. ) ;
#25167 = ADVANCED_FACE ( 'NONE', ( #68591 ), #65551, .T. ) ;
#25168 = CARTESIAN_POINT ( 'NONE',  ( -34.92500000000001137, 22.22500000000000142, 4.000000000000000000 ) ) ;
#25169 = DIRECTION ( 'NONE',  ( -0.7071067811865487940, 0.7071067811865463515, 0.000000000000000000 ) ) ;
#25171 = EDGE_LOOP ( 'NONE', ( #22941, #122946, #96168, #131733 ) ) ;
#25170 = LINE ( 'NONE', #91857, #26650 ) ;
#25172 = LINE ( 'NONE', #69427, #136585 ) ;
#25173 = CARTESIAN_POINT ( 'NONE',  ( 102.0166937171295558, 7.950000000000000178, -2.130196079827421318 ) ) ;
#25174 = DIRECTION ( 'NONE',  ( 0.3543493200069162685, -0.000000000000000000, -0.9351131265310288487 ) ) ;
#25175 = DIRECTION ( 'NONE',  ( 0.7071067811865487940, 0.7071067811865463515, 0.000000000000000000 ) ) ;
#25176 = ADVANCED_FACE ( 'NONE', ( #46873 ), #99757, .F. ) ;
#25177 = CARTESIAN_POINT ( 'NONE',  ( -1.499999999999990008, 15.05218569542901186, 5.000000000000000000 ) ) ;
#25178 = ORIENTED_EDGE ( 'NONE', *, *, #137923, .T. ) ;
#25179 = ORIENTED_EDGE ( 'NONE', *, *, #83294, .F. ) ;
#25180 = VERTEX_POINT ( 'NONE', #133827 ) ;
#25181 = CARTESIAN_POINT ( 'NONE',  ( 84.72959685856476142, -6.110000000000000320, -1.637169565754161393 ) ) ;
#25182 = ORIENTED_EDGE ( 'NONE', *, *, #133464, .F. ) ;
#25183 = DIRECTION ( 'NONE',  ( -8.673617379884034239E-17, 1.000000000000000000, 0.000000000000000000 ) ) ;
#25184 = CARTESIAN_POINT ( 'NONE',  ( 0.000000000000000000, 0.000000000000000000, 10.00000000000000000 ) ) ;
#25185 = DIRECTION ( 'NONE',  ( -0.6830127018922180770, -0.6830127018922204085, -0.2588190451025213501 ) ) ;
#25186 = LINE ( 'NONE', #47017, #112567 ) ;
#25187 = ORIENTED_EDGE ( 'NONE', *, *, #108086, .T. ) ;
#25188 = CARTESIAN_POINT ( 'NONE',  ( 23.78840764549667597, -2.499999999999996003, 0.000000000000000000 ) ) ;
#25189 = DIRECTION ( 'NONE',  ( 0.000000000000000000, -1.000000000000000000, 0.000000000000000000 ) ) ;
#25190 = CARTESIAN_POINT ( 'NONE',  ( -26.99999999999979394, 2.587461875839214720, 4.000000000000000000 ) ) ;
#25191 = CARTESIAN_POINT ( 'NONE',  ( 79.09959685856478018, -6.109999999999997655, -1.637169565754160283 ) ) ;
#25192 = EDGE_LOOP ( 'NONE', ( #34503, #42118, #95635, #37396 ) ) ;
#25193 = FACE_OUTER_BOUND ( 'NONE', #6787, .T. ) ;
#25194 = ADVANCED_FACE ( 'NONE', ( #79498 ), #44725, .F. ) ;
#25195 = DIRECTION ( 'NONE',  ( 0.000000000000000000, -0.3543493200069152138, 0.9351131265310292928 ) ) ;
#25196 = CARTESIAN_POINT ( 'NONE',  ( 2.671830600776451181, -15.74070752338412760, 4.000000000000000000 ) ) ;
#25197 = COLOUR_RGB ( '', 0.40784314, 0.44705882, 0.49803922) ;
#25198 = AXIS2_PLACEMENT_3D ( 'NONE', #130162, #43862, #141004 ) ;
#25199 = VECTOR ( 'NONE', #49518, 1000.000000000000000 ) ;
#25200 = EDGE_LOOP ( 'NONE', ( #125486, #2996, #136169, #125836 ) ) ;
#25201 = ORIENTED_EDGE ( 'NONE', *, *, #45542, .F. ) ;
#25202 = VECTOR ( 'NONE', #32557, 1000.000000000000000 ) ;
#25203 = DIRECTION ( 'NONE',  ( 0.7071067811865487940, 0.7071067811865463515, 0.000000000000000000 ) ) ;
#25204 = LINE ( 'NONE', #123126, #40832 ) ;
#25205 = CARTESIAN_POINT ( 'NONE',  ( 25.39999999999999858, 7.796566843815467607, 1.475727091950665537 ) ) ;
#25206 = DIRECTION ( 'NONE',  ( 0.3543493200069162685, -0.000000000000000000, -0.9351131265310288487 ) ) ;
#25207 = VECTOR ( 'NONE', #119548, 1000.000000000000000 ) ;
#25208 = STYLED_ITEM ( 'NONE', ( #111796 ), #139027 ) ;
#25210 = EDGE_CURVE ( 'NONE', #49508, #11167, #122209, .T. ) ;
#25209 =( BOUNDED_CURVE ( )  B_SPLINE_CURVE ( 3, ( #74025, #108037, #76169, #129101 ),
 .UNSPECIFIED., .F., .T. ) 
 B_SPLINE_CURVE_WITH_KNOTS ( ( 4, 4 ),
 ( 3.995629653766868294, 4.163580865291857336 ),
 .UNSPECIFIED. ) 
 CURVE ( )  GEOMETRIC_REPRESENTATION_ITEM ( )  RATIONAL_B_SPLINE_CURVE ( ( 1.000000000000000000, 0.9976507469244647597, 0.9976507469244647597, 1.000000000000000000 ) ) 
 REPRESENTATION_ITEM ( '' )  );
#25211 = CARTESIAN_POINT ( 'NONE',  ( 0.000000000000000000, 0.000000000000000000, 5.000000000000000000 ) ) ;
#25212 = DIRECTION ( 'NONE',  ( -0.7071067811865487940, 0.7071067811865463515, 0.000000000000000000 ) ) ;
#25213 = VERTEX_POINT ( 'NONE', #91060 ) ;
#25214 = ORIENTED_EDGE ( 'NONE', *, *, #80067, .F. ) ;
#25215 = CARTESIAN_POINT ( 'NONE',  ( 10.06250000000000000, 4.461849672132300881, 4.461849672132299105 ) ) ;
#25217 = EDGE_LOOP ( 'NONE', ( #111195, #59292, #134518, #110623 ) ) ;
#25216 = EDGE_CURVE ( 'NONE', #28316, #48874, #99030, .T. ) ;
#25218 = ORIENTED_EDGE ( 'NONE', *, *, #40487, .T. ) ;
#25219 = CONICAL_SURFACE ( 'NONE', #36812, 9.524999999999991473, 1.029744258676653645 ) ;
#25220 = CIRCLE ( 'NONE', #48311, 1.898649999999994842 ) ;
#25221 = CARTESIAN_POINT ( 'NONE',  ( 26.90840764549667696, 9.139736423841732040E-16, 0.000000000000000000 ) ) ;
#25222 = VERTEX_POINT ( 'NONE', #45420 ) ;
#25223 = CARTESIAN_POINT ( 'NONE',  ( 12.29974487139158512, -27.71228299555214747, 4.000000000000000000 ) ) ;
#25224 = CARTESIAN_POINT ( 'NONE',  ( 10.49999999999992539, 4.466399257802213363, 5.000000000000000000 ) ) ;
#25225 = EDGE_CURVE ( 'NONE', #95357, #99199, #143264, .T. ) ;
#25226 = CARTESIAN_POINT ( 'NONE',  ( -8.999999999999937828, 12.25461709320620507, -10.07315571508699392 ) ) ;
#25227 = AXIS2_PLACEMENT_3D ( 'NONE', #14122, #1782, #135235 ) ;
#25228 = LINE ( 'NONE', #81069, #81554 ) ;
#25229 = ORIENTED_EDGE ( 'NONE', *, *, #620, .F. ) ;
#25230 = VECTOR ( 'NONE', #74931, 1000.000000000000227 ) ;
#25231 = DIRECTION ( 'NONE',  ( -0.6830127018922180770, -0.6830127018922204085, -0.2588190451025213501 ) ) ;
#25232 = FACE_OUTER_BOUND ( 'NONE', #454, .T. ) ;
#25233 = ORIENTED_EDGE ( 'NONE', *, *, #29375, .F. ) ;
#25235 = ADVANCED_FACE ( 'NONE', ( #77342 ), #88919, .T. ) ;
#25234 = CARTESIAN_POINT ( 'NONE',  ( 36.48921356237310221, -27.52281430457080802, 5.000000000000000000 ) ) ;
#25236 = EDGE_LOOP ( 'NONE', ( #17195, #3429, #11412, #2916 ) ) ;
#25237 = EDGE_LOOP ( 'NONE', ( #110238, #33276, #40216, #71620 ) ) ;
#25238 = DIRECTION ( 'NONE',  ( -0.7071067811865486830, -0.7071067811865464625, -0.000000000000000000 ) ) ;
#25239 = ORIENTED_EDGE ( 'NONE', *, *, #76703, .T. ) ;
#25240 = EDGE_LOOP ( 'NONE', ( #119371, #65109, #15226, #85292 ) ) ;
#25242 = AXIS2_PLACEMENT_3D ( 'NONE', #134663, #136060, #112879 ) ;
#25241 = CARTESIAN_POINT ( 'NONE',  ( 2.139447441471317379, 4.584330080086930965E-16, 0.000000000000000000 ) ) ;
#25243 = EDGE_LOOP ( 'NONE', ( #114226, #4020, #78800, #69540 ) ) ;
#25244 = VECTOR ( 'NONE', #73929, 1000.000000000000000 ) ;
#25245 = CARTESIAN_POINT ( 'NONE',  ( 6.328169399223485314, -9.740707523384182664, 4.000000000000000000 ) ) ;
#25246 = CARTESIAN_POINT ( 'NONE',  ( -36.48921356237310221, -27.52281430457080802, 5.000000000000000000 ) ) ;
#25247 = DIRECTION ( 'NONE',  ( -0.6830127018922181881, 0.6830127018922202975, -0.2588190451025214056 ) ) ;
#25248 = CARTESIAN_POINT ( 'NONE',  ( 115.9379301918980900, -6.110000000000001208, 1.637169565754158951 ) ) ;
#25249 = DIRECTION ( 'NONE',  ( 1.318980745116185161E-16, -1.000000000000000000, 0.000000000000000000 ) ) ;
#25250 = EDGE_CURVE ( 'NONE', #134254, #54031, #112086, .T. ) ;
#25251 = DIRECTION ( 'NONE',  ( 0.000000000000000000, 0.000000000000000000, -1.000000000000000000 ) ) ;
#25252 = CARTESIAN_POINT ( 'NONE',  ( 6.489213562373093325, -27.52281430457059841, 5.000000000000000000 ) ) ;
#25253 = PRESENTATION_STYLE_ASSIGNMENT (( #100159 ) ) ;
#25254 = VECTOR ( 'NONE', #96330, 1000.000000000000000 ) ;
#25255 = CARTESIAN_POINT ( 'NONE',  ( -21.48921356237309155, -27.52281430457070499, 5.000000000000000000 ) ) ;
#25256 = DIRECTION ( 'NONE',  ( -0.7071067811865487940, 0.7071067811865463515, -0.000000000000000000 ) ) ;
#25257 = VERTEX_POINT ( 'NONE', #425 ) ;
#25258 = EDGE_CURVE ( 'NONE', #111297, #98615, #67147, .T. ) ;
#25259 = DIRECTION ( 'NONE',  ( -0.000000000000000000, 0.000000000000000000, 1.000000000000000000 ) ) ;
#25260 = DIRECTION ( 'NONE',  ( -0.000000000000000000, 0.000000000000000000, 1.000000000000000000 ) ) ;
#25261 = ORIENTED_EDGE ( 'NONE', *, *, #105948, .T. ) ;
#25262 = ORIENTED_EDGE ( 'NONE', *, *, #131237, .F. ) ;
#25263 = CARTESIAN_POINT ( 'NONE',  ( 27.29974487139158512, -27.71228299555225405, 4.000000000000000000 ) ) ;
#25264 = ORIENTED_EDGE ( 'NONE', *, *, #40477, .T. ) ;
#25265 = DIRECTION ( 'NONE',  ( 0.7071067811865487940, 0.7071067811865463515, 0.000000000000000000 ) ) ;
#25266 = DIRECTION ( 'NONE',  ( 0.3543493200069163240, 0.000000000000000000, -0.9351131265310288487 ) ) ;
#25267 = CARTESIAN_POINT ( 'NONE',  ( 7.566871997512529369, -21.74070752338406365, 6.915939825044055134 ) ) ;
#25268 = ADVANCED_FACE ( 'NONE', ( #12023 ), #56312, .F. ) ;
#25269 = DIRECTION ( 'NONE',  ( 0.7071067811865487940, 0.7071067811865463515, -0.000000000000000000 ) ) ;
#25270 = ORIENTED_EDGE ( 'NONE', *, *, #18276, .T. ) ;
#25271 = DIRECTION ( 'NONE',  ( -0.6830127018922181881, 0.6830127018922202975, -0.2588190451025214056 ) ) ;
#25272 = ORIENTED_EDGE ( 'NONE', *, *, #138161, .F. ) ;
#25274 = CARTESIAN_POINT ( 'NONE',  ( 29.99999999999979039, -15.03360074219758857, 5.000000000000000000 ) ) ;
#25273 = PRODUCT_RELATED_PRODUCT_CATEGORY ( 'part', '', ( #140743 ) ) ;
#25275 = CARTESIAN_POINT ( 'NONE',  ( 28.35873647476855197, 5.808823158059031044, -5.808823158059038150 ) ) ;
#25276 = EDGE_LOOP ( 'NONE', ( #26407, #65884, #6597, #77732 ) ) ;
#25277 = DIRECTION ( 'NONE',  ( 0.7071067811865486830, -0.7071067811865464625, -0.000000000000000000 ) ) ;
#25278 = LINE ( 'NONE', #3505, #14101 ) ;
#25279 = EDGE_LOOP ( 'NONE', ( #9278, #1510, #21821, #115037 ) ) ;
#25280 = EDGE_LOOP ( 'NONE', ( #75509, #67601, #83168 ) ) ;
#25281 = VERTEX_POINT ( 'NONE', #38797 ) ;
#25282 = CARTESIAN_POINT ( 'NONE',  ( 24.87999999999999901, -2.055000000000000160, 0.000000000000000000 ) ) ;
#25283 = DIRECTION ( 'NONE',  ( 0.3543493200069162685, -0.000000000000000000, -0.9351131265310288487 ) ) ;
#25284 = CARTESIAN_POINT ( 'NONE',  ( 57.18398860626899705, 28.73617430169827358, 5.000000000000000000 ) ) ;
#25285 = DIRECTION ( 'NONE',  ( 0.000000000000000000, -1.000000000000000000, 0.000000000000000000 ) ) ;
#25286 = ORIENTED_EDGE ( 'NONE', *, *, #41528, .T. ) ;
#25287 = CARTESIAN_POINT ( 'NONE',  ( -34.17183060077622514, 0.7592924766157138627, 4.000000000000000000 ) ) ;
#25288 = DIRECTION ( 'NONE',  ( 0.000000000000000000, 0.000000000000000000, -1.000000000000000000 ) ) ;
#25289 = CARTESIAN_POINT ( 'NONE',  ( -30.48921356237309510, -27.52281430457076894, 5.000000000000000000 ) ) ;
#25290 = FACE_OUTER_BOUND ( 'NONE', #13023, .T. ) ;
#25291 = ORIENTED_EDGE ( 'NONE', *, *, #74796, .F. ) ;
#25292 = AXIS2_PLACEMENT_3D ( 'NONE', #111936, #101029, #24206 ) ;
#25293 = VECTOR ( 'NONE', #38691, 1000.000000000000000 ) ;
#25294 = VECTOR ( 'NONE', #18389, 1000.000000000000114 ) ;
#25295 = DIRECTION ( 'NONE',  ( 0.7071067811865487940, 0.7071067811865463515, 0.000000000000000000 ) ) ;
#25296 = ORIENTED_EDGE ( 'NONE', *, *, #51502, .T. ) ;
#25297 = VECTOR ( 'NONE', #80363, 1000.000000000000227 ) ;
#25299 = EDGE_LOOP ( 'NONE', ( #28671, #35318, #112579, #54851, #22154 ) ) ;
#25298 = CARTESIAN_POINT ( 'NONE',  ( 57.17148983090720549, -47.44491123044907965, -36.62621018406388629 ) ) ;
#25300 = ORIENTED_EDGE ( 'NONE', *, *, #12405, .T. ) ;
#25301 = DIRECTION ( 'NONE',  ( -0.3543493200069162685, -0.000000000000000000, -0.9351131265310288487 ) ) ;
#25302 = PLANE ( 'NONE',  #115423 ) ;
#25303 = ORIENTED_EDGE ( 'NONE', *, *, #48597, .F. ) ;
#25304 = DIRECTION ( 'NONE',  ( -0.000000000000000000, 0.000000000000000000, 1.000000000000000000 ) ) ;
#25305 = CIRCLE ( 'NONE', #87727, 2.500000000000000888 ) ;
#25306 = DIRECTION ( 'NONE',  ( -0.000000000000000000, -1.000000000000000000, -0.000000000000000000 ) ) ;
#25307 = CARTESIAN_POINT ( 'NONE',  ( 10.49999999999993605, -7.420205493532887608, -2.617629953481229510 ) ) ;
#25308 = ADVANCED_FACE ( 'NONE', ( #80885 ), #136665, .F. ) ;
#25309 = CARTESIAN_POINT ( 'NONE',  ( 25.82816939922334853, -11.24070752338417201, 4.000000000000000000 ) ) ;
#25310 = DIRECTION ( 'NONE',  ( 0.000000000000000000, 1.000000000000000000, 0.000000000000000000 ) ) ;
#25311 = ADVANCED_FACE ( 'NONE', ( #47574 ), #4669, .F. ) ;
#25312 = FACE_OUTER_BOUND ( 'NONE', #62899, .T. ) ;
#25313 = PLANE ( 'NONE',  #100088 ) ;
#25314 = LINE ( 'NONE', #112349, #118958 ) ;
#25315 = EDGE_CURVE ( 'NONE', #23280, #97308, #70738, .T. ) ;
#25316 = CARTESIAN_POINT ( 'NONE',  ( 23.20710678118638270, -20.24070752338408141, 5.000000000000000000 ) ) ;
#25317 = CARTESIAN_POINT ( 'NONE',  ( 22.14540314143522082, -2.126176841940958351, -7.934999999999989839 ) ) ;
#25319 = VECTOR ( 'NONE', #85763, 1000.000000000000000 ) ;
#25318 = CARTESIAN_POINT ( 'NONE',  ( -26.99999999999980815, 7.552185695429093570, 5.000000000000000000 ) ) ;
#25320 = CARTESIAN_POINT ( 'NONE',  ( 27.29974487139158512, -27.71228299555225405, 4.000000000000000000 ) ) ;
#25321 = AXIS2_PLACEMENT_3D ( 'NONE', #31539, #298, #10471 ) ;
#25322 = DIRECTION ( 'NONE',  ( 0.000000000000000000, -1.000000000000000000, 0.000000000000000000 ) ) ;
#25324 = EDGE_CURVE ( 'NONE', #124072, #139654, #17044, .T. ) ;
#25323 = FACE_OUTER_BOUND ( 'NONE', #133300, .T. ) ;
#25325 = ORIENTED_EDGE ( 'NONE', *, *, #41928, .F. ) ;
#25326 = ORIENTED_EDGE ( 'NONE', *, *, #19109, .T. ) ;
#25327 = CARTESIAN_POINT ( 'NONE',  ( 93.16666666666667140, 6.884901960086285300, 3.975000000000003642 ) ) ;
#25328 = ORIENTED_EDGE ( 'NONE', *, *, #100191, .F. ) ;
#25329 = VERTEX_POINT ( 'NONE', #70038 ) ;
#25330 = ORIENTED_EDGE ( 'NONE', *, *, #102791, .T. ) ;
#25331 = LINE ( 'NONE', #23172, #59563 ) ;
#25332 = CARTESIAN_POINT ( 'NONE',  ( 28.77149322861317771, 20.25929247661551003, 7.808871592221835911 ) ) ;
#25333 = CARTESIAN_POINT ( 'NONE',  ( 13.21584829534196182, 8.912386969599870312, 3.296154402857504273 ) ) ;
#25334 = ORIENTED_EDGE ( 'NONE', *, *, #12001, .T. ) ;
#25335 = VECTOR ( 'NONE', #86385, 1000.000000000000000 ) ;
#25336 = CARTESIAN_POINT ( 'NONE',  ( 14.66989781452726582, 17.25929247661554555, 19.83885114516067816 ) ) ;
#25337 = VECTOR ( 'NONE', #14646, 1000.000000000000000 ) ;
#25338 = DIRECTION ( 'NONE',  ( -1.000000000000000000, -0.000000000000000000, -0.000000000000000000 ) ) ;
#25339 = EDGE_CURVE ( 'NONE', #124629, #102653, #135961, .T. ) ;
#25340 = LINE ( 'NONE', #113790, #37112 ) ;
#25341 = CARTESIAN_POINT ( 'NONE',  ( 125.8175036712048609, 1.497365648122270798, -7.501076162823921756 ) ) ;
#25342 = EDGE_CURVE ( 'NONE', #137290, #25946, #138832, .T. ) ;
#25343 = CARTESIAN_POINT ( 'NONE',  ( 127.6620968585647802, -5.291415217122919401, 3.054999999999997939 ) ) ;
#25344 = FACE_OUTER_BOUND ( 'NONE', #10821, .T. ) ;
#25345 = DIRECTION ( 'NONE',  ( -0.000000000000000000, -0.3543493200069152693, 0.9351131265310292928 ) ) ;
#25346 = DIRECTION ( 'NONE',  ( 0.000000000000000000, 0.000000000000000000, -1.000000000000000000 ) ) ;
#25347 = VECTOR ( 'NONE', #119821, 1000.000000000000227 ) ;
#25348 = CARTESIAN_POINT ( 'NONE',  ( 26.99999999999999289, 5.724939966758856968, 3.387577145584128591 ) ) ;
#25349 = CARTESIAN_POINT ( 'NONE',  ( -45.48921356237309510, -27.52281430457087197, 5.000000000000000000 ) ) ;
#25350 = CARTESIAN_POINT ( 'NONE',  ( 34.49999999999975131, 9.054329344830847504, 4.994342998332164107 ) ) ;
#25351 = AXIS2_PLACEMENT_3D ( 'NONE', #142267, #8814, #130680 ) ;
#25352 = DIRECTION ( 'NONE',  ( 0.6830127018922181881, 0.6830127018922202975, -0.2588190451025214056 ) ) ;
#25353 = EDGE_CURVE ( 'NONE', #57316, #28471, #26491, .T. ) ;
#25354 = CARTESIAN_POINT ( 'NONE',  ( -11.51078643762690490, -27.52281430457047406, 5.000000000000000000 ) ) ;
#25355 = ORIENTED_EDGE ( 'NONE', *, *, #60001, .T. ) ;
#25356 = ORIENTED_EDGE ( 'NONE', *, *, #16602, .F. ) ;
#25357 = CARTESIAN_POINT ( 'NONE',  ( 106.7504301918981184, 3.055000000000002824, -5.291415217122919401 ) ) ;
#25358 = VERTEX_POINT ( 'NONE', #50392 ) ;
#25359 = CARTESIAN_POINT ( 'NONE',  ( -2.994519915287485734, 28.92564299267940342, 4.000000000000000000 ) ) ;
#25360 = EDGE_CURVE ( 'NONE', #48528, #107040, #125816, .T. ) ;
#25361 = AXIS2_PLACEMENT_3D ( 'NONE', #16958, #137320, #48884 ) ;
#25362 = PLANE ( 'NONE',  #111552 ) ;
#25363 = DIRECTION ( 'NONE',  ( -0.6830127018922180770, -0.6830127018922204085, -0.2588190451025213501 ) ) ;
#25364 = CARTESIAN_POINT ( 'NONE',  ( 108.8495968585647660, 6.109999999999996767, 1.637169565754163836 ) ) ;
#25365 = ORIENTED_EDGE ( 'NONE', *, *, #85247, .T. ) ;
#25366 = EDGE_LOOP ( 'NONE', ( #30790, #108634, #93827, #1980 ) ) ;
#25368 = EDGE_CURVE ( 'NONE', #51437, #12698, #48237, .T. ) ;
#25367 = LINE ( 'NONE', #80497, #128679 ) ;
#25369 = ORIENTED_EDGE ( 'NONE', *, *, #60359, .F. ) ;
#25370 = EDGE_LOOP ( 'NONE', ( #52717, #94324, #132502, #49727 ) ) ;
#25371 = ORIENTED_EDGE ( 'NONE', *, *, #138230, .T. ) ;
#25372 = FACE_OUTER_BOUND ( 'NONE', #104898, .T. ) ;
#25373 =( REPRESENTATION_RELATIONSHIP ('NONE','NONE', #69070, #428 ) REPRESENTATION_RELATIONSHIP_WITH_TRANSFORMATION ( #53211 )SHAPE_REPRESENTATION_RELATIONSHIP( ) );
#25374 = FACE_OUTER_BOUND ( 'NONE', #3713, .T. ) ;
#25375 = EDGE_CURVE ( 'NONE', #5308, #117459, #36637, .T. ) ;
#25376 = ORIENTED_EDGE ( 'NONE', *, *, #39059, .T. ) ;
#25377 = ORIENTED_EDGE ( 'NONE', *, *, #123106, .F. ) ;
#25378 = DIRECTION ( 'NONE',  ( -0.000000000000000000, 0.000000000000000000, 1.000000000000000000 ) ) ;
#25379 = ORIENTED_EDGE ( 'NONE', *, *, #13215, .F. ) ;
#25380 = EDGE_LOOP ( 'NONE', ( #122405, #83824, #128634, #45254 ) ) ;
#25381 = CARTESIAN_POINT ( 'NONE',  ( -15.79289321881334196, 15.75929247661555799, 5.000000000000000000 ) ) ;
#25382 = CARTESIAN_POINT ( 'NONE',  ( -48.18398860626899705, 28.73617430169820608, 5.000000000000000000 ) ) ;
#25383 = DIRECTION ( 'NONE',  ( 1.192622389734054877E-16, -1.000000000000000000, 0.000000000000000000 ) ) ;
#25384 = ORIENTED_EDGE ( 'NONE', *, *, #48230, .T. ) ;
#25385 = PLANE ( 'NONE',  #94626 ) ;
#25386 = ADVANCED_FACE ( 'NONE', ( #138107 ), #72902, .T. ) ;
#25387 = DIRECTION ( 'NONE',  ( -0.7071067811865486830, -0.7071067811865463515, 0.000000000000000000 ) ) ;
#25388 = VECTOR ( 'NONE', #119735, 1000.000000000000227 ) ;
#25389 = VECTOR ( 'NONE', #90850, 1000.000000000000000 ) ;
#25390 = SURFACE_STYLE_USAGE ( .BOTH. , #68945 ) ;
#25391 = AXIS2_PLACEMENT_3D ( 'NONE', #87309, #75030, #110452 ) ;
#25392 = FACE_BOUND ( 'NONE', #55209, .T. ) ;
#25393 = ORIENTED_EDGE ( 'NONE', *, *, #126470, .T. ) ;
#25394 = CARTESIAN_POINT ( 'NONE',  ( 63.37086038379622011, 6.884901960086289741, -3.974999999999993427 ) ) ;
#25395 = DIRECTION ( 'NONE',  ( 1.000000000000000000, 0.000000000000000000, 0.000000000000000000 ) ) ;
#25396 = DIRECTION ( 'NONE',  ( -0.7071067811865486830, -0.7071067811865464625, -0.000000000000000000 ) ) ;
#25397 = ORIENTED_EDGE ( 'NONE', *, *, #126154, .T. ) ;
#25398 = CARTESIAN_POINT ( 'NONE',  ( -34.45011844616455221, -16.48371918836235395, 5.000000000000000888 ) ) ;
#25399 = VERTEX_POINT ( 'NONE', #82313 ) ;
#25400 = ORIENTED_EDGE ( 'NONE', *, *, #99886, .T. ) ;
#25401 = AXIS2_PLACEMENT_3D ( 'NONE', #60858, #115868, #115148 ) ;
#25402 = VERTEX_POINT ( 'NONE', #15562 ) ;
#25403 = CARTESIAN_POINT ( 'NONE',  ( 41.18293019189811588, -1.637169565754158951, -6.109999999999998543 ) ) ;
#25404 = ORIENTED_EDGE ( 'NONE', *, *, #56033, .F. ) ;
#25405 = VECTOR ( 'NONE', #141181, 1000.000000000000000 ) ;
#25406 = CARTESIAN_POINT ( 'NONE',  ( -14.51078643762690490, -27.52281430457045275, 5.000000000000000000 ) ) ;
#25407 = FACE_OUTER_BOUND ( 'NONE', #11467, .T. ) ;
#25408 = DIRECTION ( 'NONE',  ( -0.7071067811865487940, 0.7071067811865463515, 0.000000000000000000 ) ) ;
#25409 = VERTEX_POINT ( 'NONE', #83017 ) ;
#25410 = VECTOR ( 'NONE', #127700, 1000.000000000000227 ) ;
#25411 = VECTOR ( 'NONE', #34164, 1000.000000000000000 ) ;
#25412 =( BOUNDED_CURVE ( )  B_SPLINE_CURVE ( 3, ( #22485, #66749, #86369, #65349 ),
 .UNSPECIFIED., .F., .F. ) 
 B_SPLINE_CURVE_WITH_KNOTS ( ( 4, 4 ),
 ( 5.106027341939277875, 6.645403452391244414 ),
 .UNSPECIFIED. ) 
 CURVE ( )  GEOMETRIC_REPRESENTATION_ITEM ( )  RATIONAL_B_SPLINE_CURVE ( ( 1.000000000000000000, 0.8120851936182275077, 0.8120851936182275077, 1.000000000000000000 ) ) 
 REPRESENTATION_ITEM ( '' )  );
#25413 = DIRECTION ( 'NONE',  ( 0.000000000000000000, -0.000000000000000000, -1.000000000000000000 ) ) ;
#25414 = VECTOR ( 'NONE', #39657, 1000.000000000000000 ) ;
#25415 = PLANE ( 'NONE',  #78346 ) ;
#25416 = CARTESIAN_POINT ( 'NONE',  ( 10.17183060077640100, -17.24070752338410628, 4.000000000000000000 ) ) ;
#25417 = EDGE_CURVE ( 'NONE', #37944, #24646, #92429, .T. ) ;
#25418 = DIRECTION ( 'NONE',  ( -0.7071067811865487940, 0.7071067811865463515, -0.000000000000000000 ) ) ;
#25419 = PLANE ( 'NONE',  #26229 ) ;
#25420 = ORIENTED_EDGE ( 'NONE', *, *, #106308, .T. ) ;
#25421 = ORIENTED_EDGE ( 'NONE', *, *, #18574, .F. ) ;
#25422 = VERTEX_POINT ( 'NONE', #49700 ) ;
#25423 = ORIENTED_EDGE ( 'NONE', *, *, #18574, .T. ) ;
#25424 = VECTOR ( 'NONE', #119309, 1000.000000000000000 ) ;
#25425 = DIRECTION ( 'NONE',  ( -0.000000000000000000, 0.000000000000000000, 1.000000000000000000 ) ) ;
#25426 = ORIENTED_EDGE ( 'NONE', *, *, #78762, .T. ) ;
#25427 = AXIS2_PLACEMENT_3D ( 'NONE', #121083, #85591, #54442 ) ;
#25428 = ORIENTED_EDGE ( 'NONE', *, *, #96776, .T. ) ;
#25429 = PLANE ( 'NONE',  #88373 ) ;
#25430 = EDGE_CURVE ( 'NONE', #49419, #7434, #115584, .T. ) ;
#25431 = VECTOR ( 'NONE', #57861, 1000.000000000000000 ) ;
#25432 = EDGE_CURVE ( 'NONE', #118358, #133102, #126494, .T. ) ;
#25433 = DIRECTION ( 'NONE',  ( 1.000000000000000000, 1.224606353822377258E-16, 0.000000000000000000 ) ) ;
#25434 = ORIENTED_EDGE ( 'NONE', *, *, #90990, .F. ) ;
#25435 = VECTOR ( 'NONE', #38034, 999.9999999999998863 ) ;
#25436 = PLANE ( 'NONE',  #16336 ) ;
#25437 = ORIENTED_EDGE ( 'NONE', *, *, #27628, .T. ) ;
#25438 = FACE_OUTER_BOUND ( 'NONE', #76679, .T. ) ;
#25439 = CARTESIAN_POINT ( 'NONE',  ( 33.17123647476855552, 0.000000000000000000, 7.934999999999990727 ) ) ;
#25440 = CARTESIAN_POINT ( 'NONE',  ( 2.983736474768552860, -5.808823158059035485, -5.808823158059033709 ) ) ;
#25441 = ORIENTED_EDGE ( 'NONE', *, *, #33969, .T. ) ;
#25443 = DIRECTION ( 'NONE',  ( -0.000000000000000000, 0.3543493200069153248, 0.9351131265310292928 ) ) ;
#25442 = CARTESIAN_POINT ( 'NONE',  ( 110.7454301918981088, -5.291415217122919401, -3.055000000000000604 ) ) ;
#25444 = FACE_OUTER_BOUND ( 'NONE', #77376, .T. ) ;
#25445 = DIRECTION ( 'NONE',  ( 0.3543493200069162685, -0.000000000000000000, -0.9351131265310288487 ) ) ;
#25446 = VERTEX_POINT ( 'NONE', #5419 ) ;
#25447 = DIRECTION ( 'NONE',  ( 0.000000000000000000, -1.000000000000000000, 0.000000000000000000 ) ) ;
#25448 = AXIS2_PLACEMENT_3D ( 'NONE', #70507, #16028, #104497 ) ;
#25449 = ORIENTED_EDGE ( 'NONE', *, *, #627, .T. ) ;
#25450 = CARTESIAN_POINT ( 'NONE',  ( 33.48921356237309510, -27.52281430457078670, 5.000000000000000000 ) ) ;
#25451 = CARTESIAN_POINT ( 'NONE',  ( -15.18398860626900237, 28.73617430169797871, 5.000000000000000000 ) ) ;
#25452 = CARTESIAN_POINT ( 'NONE',  ( -12.32816939922344623, -21.74070752338406365, 4.000000000000000000 ) ) ;
#25453 = CARTESIAN_POINT ( 'NONE',  ( -12.20000000000000284, -27.55040120718572894, 16.07347811296898854 ) ) ;
#25454 = CARTESIAN_POINT ( 'NONE',  ( 183.4386084925502303, -49.19295221410152408, -41.21232802153173225 ) ) ;
#25455 = EDGE_CURVE ( 'NONE', #18761, #47327, #27187, .T. ) ;
#25456 = ORIENTED_EDGE ( 'NONE', *, *, #120829, .F. ) ;
#25457 = CARTESIAN_POINT ( 'NONE',  ( -24.48921356237309510, -27.52281430457072631, 5.000000000000000000 ) ) ;
#25458 = CARTESIAN_POINT ( 'NONE',  ( 1.499999999999990896, 3.431123077392149501, 4.000000000000000000 ) ) ;
#25459 = DIRECTION ( 'NONE',  ( -1.000000000000000000, -1.224606353822377258E-16, -0.000000000000000000 ) ) ;
#25460 = EDGE_LOOP ( 'NONE', ( #118039, #101596, #31587, #91255 ) ) ;
#25461 = CARTESIAN_POINT ( 'NONE',  ( 16.49999999999988276, -19.91253812416055169, 4.000000000000000000 ) ) ;
#25462 = VECTOR ( 'NONE', #7417, 999.9999999999998863 ) ;
#25463 = DIRECTION ( 'NONE',  ( -0.6830127018922181881, 0.6830127018922202975, -0.2588190451025214056 ) ) ;
#25464 = ORIENTED_EDGE ( 'NONE', *, *, #69492, .F. ) ;
#25466 = ORIENTED_EDGE ( 'NONE', *, *, #53013, .F. ) ;
#25465 = DIRECTION ( 'NONE',  ( 0.7071067811865487940, 0.7071067811865463515, 0.000000000000000000 ) ) ;
#25467 = ORIENTED_EDGE ( 'NONE', *, *, #89622, .T. ) ;
#25468 = CARTESIAN_POINT ( 'NONE',  ( 2.075939324931954655, 13.65470463357565123, -24.43886132094158725 ) ) ;
#25469 = DIRECTION ( 'NONE',  ( 0.000000000000000000, -1.000000000000000000, 0.000000000000000000 ) ) ;
#25471 = ORIENTED_EDGE ( 'NONE', *, *, #142481, .F. ) ;
#25470 = AXIS2_PLACEMENT_3D ( 'NONE', #135364, #58550, #102718 ) ;
#25472 = VECTOR ( 'NONE', #13849, 1000.000000000000000 ) ;
#25473 = FACE_OUTER_BOUND ( 'NONE', #14063, .T. ) ;
#25474 = ADVANCED_FACE ( 'NONE', ( #6114 ), #28649, .T. ) ;
#25475 = CARTESIAN_POINT ( 'NONE',  ( 23.99999999999983302, -3.485240976185050243, -4.108735105802342247 ) ) ;
#25476 = ORIENTED_EDGE ( 'NONE', *, *, #82342, .F. ) ;
#25477 = LINE ( 'NONE', #1042, #117922 ) ;
#25478 = EDGE_CURVE ( 'NONE', #35412, #29685, #52514, .T. ) ;
#25479 = LINE ( 'NONE', #100214, #35102 ) ;
#25480 = CARTESIAN_POINT ( 'NONE',  ( 0.000000000000000000, 0.000000000000000000, 5.000000000000000000 ) ) ;
#25481 = LINE ( 'NONE', #124101, #58694 ) ;
#25482 = DIRECTION ( 'NONE',  ( -0.000000000000000000, -0.3543493200069152693, 0.9351131265310292928 ) ) ;
#25483 = CARTESIAN_POINT ( 'NONE',  ( 126.1492088369915194, -7.085075694611017383, 1.787438164688350817 ) ) ;
#25484 = CARTESIAN_POINT ( 'NONE',  ( 3.489213562373097322, -27.52281430457057709, 5.000000000000000000 ) ) ;
#25486 = EDGE_CURVE ( 'NONE', #34286, #95435, #74523, .T. ) ;
#25485 = DIRECTION ( 'NONE',  ( 0.7071067811865487940, -0.7071067811865463515, 0.000000000000000000 ) ) ;
#25488 = ADVANCED_FACE ( 'NONE', ( #42387 ), #106151, .F. ) ;
#25487 = ORIENTED_EDGE ( 'NONE', *, *, #99421, .F. ) ;
#25489 = ORIENTED_EDGE ( 'NONE', *, *, #122898, .F. ) ;
#25490 = ORIENTED_EDGE ( 'NONE', *, *, #54303, .T. ) ;
#25491 = CARTESIAN_POINT ( 'NONE',  ( 116.3541666666666856, -2.130196079827425315, -7.950000000000001066 ) ) ;
#25492 = VECTOR ( 'NONE', #41877, 1000.000000000000000 ) ;
#25493 = VERTEX_POINT ( 'NONE', #85143 ) ;
#25494 = VERTEX_POINT ( 'NONE', #109025 ) ;
#25495 = VERTEX_POINT ( 'NONE', #53981 ) ;
#25496 = PLANE ( 'NONE',  #80362 ) ;
#25497 = DIRECTION ( 'NONE',  ( 0.7071067811865487940, -0.7071067811865463515, 0.000000000000000000 ) ) ;
#25498 =( GEOMETRIC_REPRESENTATION_CONTEXT ( 3 ) GLOBAL_UNCERTAINTY_ASSIGNED_CONTEXT ( ( #118579 ) ) GLOBAL_UNIT_ASSIGNED_CONTEXT ( ( #90180, #66318, #57592 ) ) REPRESENTATION_CONTEXT ( 'NONE', 'WORKASPACE' ) );
#25499 = AXIS2_PLACEMENT_3D ( 'NONE', #44419, #111789, #134259 ) ;
#25500 = VECTOR ( 'NONE', #84845, 1000.000000000000000 ) ;
#25501 = ORIENTED_EDGE ( 'NONE', *, *, #97510, .T. ) ;
#25502 = LINE ( 'NONE', #23360, #18374 ) ;
#25503 = DIRECTION ( 'NONE',  ( -0.000000000000000000, 0.000000000000000000, 1.000000000000000000 ) ) ;
#25504 = EDGE_CURVE ( 'NONE', #101224, #26788, #19180, .T. ) ;
#25505 = DIRECTION ( 'NONE',  ( 1.000000000000000000, 0.000000000000000000, 0.000000000000000000 ) ) ;
#25506 = CARTESIAN_POINT ( 'NONE',  ( 113.3129301918981042, -1.637169565754159617, -6.110000000000001208 ) ) ;
#25507 = ORIENTED_EDGE ( 'NONE', *, *, #38003, .F. ) ;
#25508 = EDGE_CURVE ( 'NONE', #102312, #64028, #20589, .T. ) ;
#25509 = DIRECTION ( 'NONE',  ( 0.7071067811865487940, 0.7071067811865463515, 0.000000000000000000 ) ) ;
#25510 = LINE ( 'NONE', #135722, #141951 ) ;
#25511 = LINE ( 'NONE', #16034, #31219 ) ;
#25512 = AXIS2_PLACEMENT_3D ( 'NONE', #123623, #90237, #43901 ) ;
#25513 = CARTESIAN_POINT ( 'NONE',  ( 1.153023801772934176, 3.242423929075685329, 6.152118276231695937 ) ) ;
#25514 = DIRECTION ( 'NONE',  ( -0.6830127018922180770, -0.6830127018922204085, -0.2588190451025213501 ) ) ;
#25515 = CARTESIAN_POINT ( 'NONE',  ( -57.29974487139158157, -27.71228299555246011, 4.000000000000000000 ) ) ;
#25516 = CARTESIAN_POINT ( 'NONE',  ( 26.99999999999981171, -21.03360074219752462, 5.000000000000000000 ) ) ;
#25517 = CARTESIAN_POINT ( 'NONE',  ( 42.80836038379622011, 7.949999999999997513, 2.130196079827431088 ) ) ;
#25518 = DIRECTION ( 'NONE',  ( 0.7071067811865486830, -0.7071067811865464625, -0.000000000000000000 ) ) ;
#25519 = LINE ( 'NONE', #82788, #48409 ) ;
#25520 = ORIENTED_EDGE ( 'NONE', *, *, #48723, .T. ) ;
#25521 = VERTEX_POINT ( 'NONE', #84464 ) ;
#25522 = CARTESIAN_POINT ( 'NONE',  ( 35.85416666666666430, -2.130196079827425315, -7.950000000000001066 ) ) ;
#25523 = ADVANCED_FACE ( 'NONE', ( #64121 ), #140254, .F. ) ;
#25524 = VERTEX_POINT ( 'NONE', #74289 ) ;
#25525 = ORIENTED_EDGE ( 'NONE', *, *, #123549, .F. ) ;
#25526 = CARTESIAN_POINT ( 'NONE',  ( 18.17159235450331778, 2.500000000000001776, 0.000000000000000000 ) ) ;
#25527 = AXIS2_PLACEMENT_3D ( 'NONE', #74577, #86158, #9250 ) ;
#25528 = LINE ( 'NONE', #69803, #31602 ) ;
#25529 = ORIENTED_EDGE ( 'NONE', *, *, #111780, .T. ) ;
#25530 = EDGE_CURVE ( 'NONE', #84085, #139503, #86096, .T. ) ;
#25531 = CARTESIAN_POINT ( 'NONE',  ( -30.79289321881324071, 6.759292476615654799, 5.000000000000000000 ) ) ;
#25532 = CARTESIAN_POINT ( 'NONE',  ( 26.40000000000000568, -18.48000000000005372, -34.92499999999998295 ) ) ;
#25533 = DIRECTION ( 'NONE',  ( -1.000000000000000000, -1.224606353822377258E-16, -0.000000000000000000 ) ) ;
#25534 = AXIS2_PLACEMENT_3D ( 'NONE', #92382, #50341, #136613 ) ;
#25535 = AXIS2_PLACEMENT_3D ( 'NONE', #95847, #117569, #16112 ) ;
#25536 = CARTESIAN_POINT ( 'NONE',  ( 26.97959685856476497, 6.109999999999999432, 1.637169565754164280 ) ) ;
#25537 = ORIENTED_EDGE ( 'NONE', *, *, #108444, .F. ) ;
#25538 = VECTOR ( 'NONE', #51747, 1000.000000000000227 ) ;
#25539 = PLANE ( 'NONE',  #71105 ) ;
#25540 = ORIENTED_EDGE ( 'NONE', *, *, #112468, .T. ) ;
#25541 = EDGE_CURVE ( 'NONE', #39115, #60184, #142408, .T. ) ;
#25542 = CARTESIAN_POINT ( 'NONE',  ( 34.92499999999998295, 3.701285051063797571, 12.01932804697900004 ) ) ;
#25543 = AXIS2_PLACEMENT_3D ( 'NONE', #115492, #72082, #124987 ) ;
#25544 = CARTESIAN_POINT ( 'NONE',  ( -68.99451991528748351, 28.92564299267986172, 4.000000000000000000 ) ) ;
#25545 = PLANE ( 'NONE',  #97293 ) ;
#25546 = LINE ( 'NONE', #69083, #106647 ) ;
#25547 = VERTEX_POINT ( 'NONE', #86599 ) ;
#25548 = ORIENTED_EDGE ( 'NONE', *, *, #35789, .F. ) ;
#25549 = AXIS2_PLACEMENT_3D ( 'NONE', #5487, #133038, #32276 ) ;
#25550 = DIRECTION ( 'NONE',  ( -0.000000000000000000, -0.3543493200069152693, 0.9351131265310292928 ) ) ;
#25551 = CARTESIAN_POINT ( 'NONE',  ( -8.994519915287490619, 28.92564299267944250, 4.000000000000000000 ) ) ;
#25552 = LINE ( 'NONE', #61110, #68613 ) ;
#25553 = EDGE_CURVE ( 'NONE', #118674, #38224, #118481, .T. ) ;
#25554 = EDGE_CURVE ( 'NONE', #108223, #42984, #117741, .T. ) ;
#25555 = PLANE ( 'NONE',  #34733 ) ;
#25556 = DIRECTION ( 'NONE',  ( 0.7071067811865486830, -0.7071067811865464625, -0.000000000000000000 ) ) ;
#25557 = EDGE_CURVE ( 'NONE', #7223, #34604, #108287, .T. ) ;
#25558 = VECTOR ( 'NONE', #136656, 1000.000000000000000 ) ;
#25559 = CARTESIAN_POINT ( 'NONE',  ( 54.89126352523145158, -4.472830434245839371, -4.472830434245839371 ) ) ;
#25560 = FACE_OUTER_BOUND ( 'NONE', #12945, .T. ) ;
#25561 = PLANE ( 'NONE',  #89487 ) ;
#25562 = ORIENTED_EDGE ( 'NONE', *, *, #127489, .F. ) ;
#25563 = ORIENTED_EDGE ( 'NONE', *, *, #70203, .F. ) ;
#25564 = AXIS2_PLACEMENT_3D ( 'NONE', #43536, #42133, #89191 ) ;
#25565 = CARTESIAN_POINT ( 'NONE',  ( 32.99999999999977263, -13.97847968911257510, -0.1324546996126028109 ) ) ;
#25566 = ORIENTED_EDGE ( 'NONE', *, *, #127947, .F. ) ;
#25567 = PLANE ( 'NONE',  #137099 ) ;
#25568 = PRODUCT_DEFINITION_CONTEXT ( 'detailed design', #16032, 'design' ) ;
#25569 = EDGE_LOOP ( 'NONE', ( #46349, #47449, #33898, #103692, #24337, #45344, #109041, #129441 ) ) ;
#25570 = CARTESIAN_POINT ( 'NONE',  ( 72.18398860626899705, 28.73617430169837661, 5.000000000000000000 ) ) ;
#25571 = AXIS2_PLACEMENT_3D ( 'NONE', #34746, #68129, #22394 ) ;
#25572 = FACE_BOUND ( 'NONE', #42557, .T. ) ;
#25573 = CARTESIAN_POINT ( 'NONE',  ( 26.99999999999980105, -10.44781430457071458, 5.000000000000000000 ) ) ;
#25574 = PLANE ( 'NONE',  #113868 ) ;
#25575 = FACE_OUTER_BOUND ( 'NONE', #56046, .T. ) ;
#25576 = DIRECTION ( 'NONE',  ( -0.000000000000000000, 0.3543493200069153248, 0.9351131265310292928 ) ) ;
#25578 = EDGE_LOOP ( 'NONE', ( #78475, #136860, #39283, #80575 ) ) ;
#25577 = CARTESIAN_POINT ( 'NONE',  ( 25.39999999999999858, 0.000000000000000000, 0.000000000000000000 ) ) ;
#25579 = AXIS2_PLACEMENT_3D ( 'NONE', #50142, #49455, #48014 ) ;
#25580 = CARTESIAN_POINT ( 'NONE',  ( 1.226741607178325033, -11.24070752338417556, 18.24660765846982713 ) ) ;
#25581 = ORIENTED_EDGE ( 'NONE', *, *, #17914, .T. ) ;
#25582 = ORIENTED_EDGE ( 'NONE', *, *, #1729, .T. ) ;
#25583 = CARTESIAN_POINT ( 'NONE',  ( 61.89126352523144448, -4.472830434245838482, -4.472830434245838482 ) ) ;
#25584 = ORIENTED_EDGE ( 'NONE', *, *, #97169, .T. ) ;
#25585 =( BOUNDED_CURVE ( )  B_SPLINE_CURVE ( 3, ( #13275, #102478, #66275, #976 ),
 .UNSPECIFIED., .F., .T. ) 
 B_SPLINE_CURVE_WITH_KNOTS ( ( 4, 4 ),
 ( 1.864375635226918515, 1.933014472006551188 ),
 .UNSPECIFIED. ) 
 CURVE ( )  GEOMETRIC_REPRESENTATION_ITEM ( )  RATIONAL_B_SPLINE_CURVE ( ( 1.000000000000000000, 0.9996074310407762065, 0.9996074310407762065, 1.000000000000000000 ) ) 
 REPRESENTATION_ITEM ( '' )  );
#25586 = LINE ( 'NONE', #101733, #69862 ) ;
#25587 = ORIENTED_EDGE ( 'NONE', *, *, #127769, .T. ) ;
#25588 = PLANE ( 'NONE',  #93026 ) ;
#25589 = VECTOR ( 'NONE', #31571, 1000.000000000000227 ) ;
#25590 = CARTESIAN_POINT ( 'NONE',  ( 26.20710678118636494, -20.24070752338407075, 5.000000000000000000 ) ) ;
#25591 = AXIS2_PLACEMENT_3D ( 'NONE', #78213, #134015, #91246 ) ;
#25592 = LINE ( 'NONE', #24190, #91828 ) ;
#25593 = LINE ( 'NONE', #3129, #25064 ) ;
#25595 = DIRECTION ( 'NONE',  ( 0.7071067811865487940, 0.7071067811865463515, 0.000000000000000000 ) ) ;
#25594 = CARTESIAN_POINT ( 'NONE',  ( -25.01899999999999835, 3.174999999999998046, 4.000000000000000000 ) ) ;
#25596 = DIRECTION ( 'NONE',  ( -0.7071067811865486830, -0.7071067811865464625, 0.000000000000000000 ) ) ;
#25597 = DIRECTION ( 'NONE',  ( -0.7071067811865486830, -0.7071067811865464625, -0.000000000000000000 ) ) ;
#25598 = ORIENTED_EDGE ( 'NONE', *, *, #93574, .T. ) ;
#25599 = VECTOR ( 'NONE', #14602, 1000.000000000000000 ) ;
#25600 = VECTOR ( 'NONE', #101270, 1000.000000000000000 ) ;
#25601 = CIRCLE ( 'NONE', #11716, 0.5000000000000004441 ) ;
#25602 = VERTEX_POINT ( 'NONE', #75020 ) ;
#25603 = VECTOR ( 'NONE', #118238, 1000.000000000000000 ) ;
#25604 = LINE ( 'NONE', #94427, #72860 ) ;
#25605 = CARTESIAN_POINT ( 'NONE',  ( 7.940000000000001279, -33.26999999999999602, -10.00000000000000178 ) ) ;
#25606 = ORIENTED_EDGE ( 'NONE', *, *, #90156, .F. ) ;
#25607 = VECTOR ( 'NONE', #128687, 999.9999999999998863 ) ;
#25608 = ORIENTED_EDGE ( 'NONE', *, *, #67381, .F. ) ;
#25609 = VERTEX_POINT ( 'NONE', #96699 ) ;
#25610 = EDGE_CURVE ( 'NONE', #57920, #35696, #61999, .T. ) ;
#25611 = EDGE_CURVE ( 'NONE', #128927, #98397, #25865, .T. ) ;
#25612 = CARTESIAN_POINT ( 'NONE',  ( 0.7928932188134563130, -5.240707523384228850, 5.000000000000000000 ) ) ;
#25613 = ORIENTED_EDGE ( 'NONE', *, *, #122211, .T. ) ;
#25614 = AXIS2_PLACEMENT_3D ( 'NONE', #119464, #120917, #10698 ) ;
#25615 = DIRECTION ( 'NONE',  ( -0.3543493200069162685, -0.000000000000000000, -0.9351131265310288487 ) ) ;
#25616 = CARTESIAN_POINT ( 'NONE',  ( 35.99451991528749772, 28.92564299267963079, 4.000000000000000000 ) ) ;
#25617 = CARTESIAN_POINT ( 'NONE',  ( 30.67080628287044419, -3.047499999999997211, -5.278424836066143655 ) ) ;
#25618 = PLANE ( 'NONE',  #84297 ) ;
#25619 = ORIENTED_EDGE ( 'NONE', *, *, #36841, .T. ) ;
#25620 = EDGE_CURVE ( 'NONE', #93569, #10232, #119195, .T. ) ;
#25621 = DIRECTION ( 'NONE',  ( -0.000000000000000000, 0.000000000000000000, 1.000000000000000000 ) ) ;
#25622 = LINE ( 'NONE', #68465, #28100 ) ;
#25623 = VECTOR ( 'NONE', #2470, 1000.000000000000000 ) ;
#25624 = DIRECTION ( 'NONE',  ( 1.000000000000000000, 0.000000000000000000, 0.000000000000000000 ) ) ;
#25626 = EDGE_LOOP ( 'NONE', ( #143073, #90581, #141062, #127998 ) ) ;
#25625 = PLANE ( 'NONE',  #21696 ) ;
#25627 = ORIENTED_EDGE ( 'NONE', *, *, #112981, .T. ) ;
#25628 = FACE_OUTER_BOUND ( 'NONE', #129159, .T. ) ;
#25629 = CARTESIAN_POINT ( 'NONE',  ( -34.92500000000001137, 12.75929247661558996, 4.255531930566247567 ) ) ;
#25630 = CARTESIAN_POINT ( 'NONE',  ( -34.92500000000001137, -22.22500000000000142, 4.000000000000000000 ) ) ;
#25631 = ADVANCED_FACE ( 'NONE', ( #106889 ), #8958, .F. ) ;
#25632 = ORIENTED_EDGE ( 'NONE', *, *, #14998, .F. ) ;
#25633 = AXIS2_PLACEMENT_3D ( 'NONE', #120954, #110069, #31817 ) ;
#25634 = DIRECTION ( 'NONE',  ( 1.000000000000000000, 0.000000000000000000, 0.000000000000000000 ) ) ;
#25635 = CARTESIAN_POINT ( 'NONE',  ( 0.000000000000000000, 9.735942053221458872E-16, -7.950000000000000178 ) ) ;
#25636 = VECTOR ( 'NONE', #57673, 1000.000000000000227 ) ;
#25638 = CARTESIAN_POINT ( 'NONE',  ( 3.710381658649933190, 2.500000000000000888, 0.000000000000000000 ) ) ;
#25637 = CIRCLE ( 'NONE', #88168, 2.500000000000000888 ) ;
#25639 = CARTESIAN_POINT ( 'NONE',  ( 5.510786437626906675, -27.52281430457051314, 5.000000000000000000 ) ) ;
#25640 = DIRECTION ( 'NONE',  ( -0.000000000000000000, 0.000000000000000000, 1.000000000000000000 ) ) ;
#25641 = ORIENTED_EDGE ( 'NONE', *, *, #65820, .T. ) ;
#25642 = EDGE_CURVE ( 'NONE', #106829, #27961, #131519, .T. ) ;
#25643 = CARTESIAN_POINT ( 'NONE',  ( -34.45011844616454511, 0.002304141593953373465, 5.000000000000000888 ) ) ;
#25644 = VECTOR ( 'NONE', #69946, 1000.000000000000227 ) ;
#25645 = DIRECTION ( 'NONE',  ( -0.7071067811865486830, 0.7071067811865464625, 0.000000000000000000 ) ) ;
#25646 = CARTESIAN_POINT ( 'NONE',  ( 6.754139616203771901, 3.047499999999993214, -5.278424836066146320 ) ) ;
#25647 = CARTESIAN_POINT ( 'NONE',  ( 42.48921356237308800, -27.52281430457085065, 5.000000000000000000 ) ) ;
#25648 = DIRECTION ( 'NONE',  ( 0.7071067811865486830, -0.7071067811865464625, -0.000000000000000000 ) ) ;
#25649 = VERTEX_POINT ( 'NONE', #10427 ) ;
#25650 = VECTOR ( 'NONE', #1035, 1000.000000000000000 ) ;
#25651 = VERTEX_POINT ( 'NONE', #134382 ) ;
#25652 = EDGE_CURVE ( 'NONE', #94488, #41471, #65585, .T. ) ;
#25653 = PLANE ( 'NONE',  #54887 ) ;
#25654 = CARTESIAN_POINT ( 'NONE',  ( 54.18398860626899705, 28.73617430169825226, 5.000000000000000000 ) ) ;
#25655 = CARTESIAN_POINT ( 'NONE',  ( 8.291236474768552966, -9.717572351234235426E-16, -7.934999999999990727 ) ) ;
#25656 = CARTESIAN_POINT ( 'NONE',  ( 29.99999999999979750, 5.587461875839193404, 4.000000000000000000 ) ) ;
#25657 = VECTOR ( 'NONE', #7646, 1000.000000000000000 ) ;
#25658 = LINE ( 'NONE', #79387, #104023 ) ;
#25659 = LINE ( 'NONE', #78630, #89981 ) ;
#25660 = LINE ( 'NONE', #80780, #39810 ) ;
#25661 = ORIENTED_EDGE ( 'NONE', *, *, #101279, .T. ) ;
#25662 = EDGE_CURVE ( 'NONE', #100222, #117346, #132259, .T. ) ;
#25663 = STYLED_ITEM ( 'NONE', ( #79620 ), #23037 ) ;
#25664 = CARTESIAN_POINT ( 'NONE',  ( -40.26506670282026334, 12.75929247661558996, 18.34774599283965557 ) ) ;
#25665 = CARTESIAN_POINT ( 'NONE',  ( -7.940000000000007496, -60.26999999999998892, -7.752100000000004876 ) ) ;
#25666 = CARTESIAN_POINT ( 'NONE',  ( 56.93293019189810877, 1.637169565754156730, 6.110000000000001208 ) ) ;
#25667 = DIRECTION ( 'NONE',  ( -0.7071067811865486830, -0.7071067811865464625, 0.000000000000000000 ) ) ;
#25668 = EDGE_CURVE ( 'NONE', #38684, #114903, #143100, .T. ) ;
#25669 = ADVANCED_FACE ( 'NONE', ( #13273 ), #77851, .F. ) ;
#25670 = CARTESIAN_POINT ( 'NONE',  ( 10.17183060077640455, -8.240707523384196875, 4.000000000000000000 ) ) ;
#25671 = ORIENTED_EDGE ( 'NONE', *, *, #137252, .F. ) ;
#25672 = CARTESIAN_POINT ( 'NONE',  ( 77.99451991528749772, 28.92564299267992567, 4.000000000000000000 ) ) ;
#25673 = ORIENTED_EDGE ( 'NONE', *, *, #97328, .F. ) ;
#25674 = VECTOR ( 'NONE', #86812, 1000.000000000000000 ) ;
#25675 = LINE ( 'NONE', #124994, #38539 ) ;
#25676 = ADVANCED_FACE ( 'NONE', ( #90139 ), #57546, .F. ) ;
#25677 = LINE ( 'NONE', #71346, #136377 ) ;
#25678 = LINE ( 'NONE', #56227, #134605 ) ;
#25679 = FACE_OUTER_BOUND ( 'NONE', #81395, .T. ) ;
#25680 = ADVANCED_FACE ( 'NONE', ( #43794 ), #109755, .F. ) ;
#25681 = DIRECTION ( 'NONE',  ( -0.6830127018922181881, 0.6830127018922202975, -0.2588190451025214056 ) ) ;
#25682 = CARTESIAN_POINT ( 'NONE',  ( 11.37500000000000178, -6.094999999999989981, 3.732111120401553285E-16 ) ) ;
#25683 = ORIENTED_EDGE ( 'NONE', *, *, #3135, .T. ) ;
#25684 = ADVANCED_FACE ( 'NONE', ( #88008 ), #35083, .F. ) ;
#25685 = ORIENTED_EDGE ( 'NONE', *, *, #135187, .F. ) ;
#25686 = CARTESIAN_POINT ( 'NONE',  ( 28.00000000000002487, -49.14999999999999147, 34.92500000000003268 ) ) ;
#25687 = DIRECTION ( 'NONE',  ( 0.000000000000000000, -1.000000000000000000, 0.000000000000000000 ) ) ;
#25688 = UNCERTAINTY_MEASURE_WITH_UNIT (LENGTH_MEASURE( 1.000000000000000082E-05 ), #69170, 'distance_accuracy_value', 'NONE');
#25689 = VECTOR ( 'NONE', #138399, 1000.000000000000000 ) ;
#25690 = DIRECTION ( 'NONE',  ( -0.7071067811865486830, 0.7071067811865464625, 0.000000000000000000 ) ) ;
#25691 = DIRECTION ( 'NONE',  ( 0.7071067811865486830, -0.7071067811865464625, -0.000000000000000000 ) ) ;
#25692 = CARTESIAN_POINT ( 'NONE',  ( 75.47502705046287019, -5.819803920172572198, 5.819803920172572198 ) ) ;
#25693 = CARTESIAN_POINT ( 'NONE',  ( -29.18753812416032289, -22.22500000000000142, 4.000000000000000000 ) ) ;
#25694 = ORIENTED_EDGE ( 'NONE', *, *, #72112, .T. ) ;
#25695 = CARTESIAN_POINT ( 'NONE',  ( 62.39583333333332149, -2.130196079827427091, 7.949999999999999289 ) ) ;
#25696 = EDGE_CURVE ( 'NONE', #68874, #44719, #79324, .T. ) ;
#25697 = LINE ( 'NONE', #91674, #14594 ) ;
#25698 = DIRECTION ( 'NONE',  ( 1.000000000000000000, 0.000000000000000000, 0.000000000000000000 ) ) ;
#25699 = PLANE ( 'NONE',  #33546 ) ;
#25700 = ORIENTED_EDGE ( 'NONE', *, *, #86457, .F. ) ;
#25702 = EDGE_CURVE ( 'NONE', #56955, #63125, #22023, .T. ) ;
#25701 = VECTOR ( 'NONE', #96395, 1000.000000000000227 ) ;
#25703 = PLANE ( 'NONE',  #46784 ) ;
#25704 = AXIS2_PLACEMENT_3D ( 'NONE', #77358, #121517, #34528 ) ;
#25705 = VECTOR ( 'NONE', #76779, 1000.000000000000000 ) ;
#25706 = FACE_OUTER_BOUND ( 'NONE', #67787, .T. ) ;
#25707 = CARTESIAN_POINT ( 'NONE',  ( 64.89626352523144703, 4.472830434245840259, -4.472830434245839371 ) ) ;
#25708 = CARTESIAN_POINT ( 'NONE',  ( 0.000000000000000000, 0.000000000000000000, 0.000000000000000000 ) ) ;
#25709 = ORIENTED_EDGE ( 'NONE', *, *, #72740, .T. ) ;
#25711 = EDGE_LOOP ( 'NONE', ( #18441, #79046, #11225, #117144 ) ) ;
#25710 = VECTOR ( 'NONE', #70292, 1000.000000000000000 ) ;
#25712 = AXIS2_PLACEMENT_3D ( 'NONE', #108368, #133056, #130187 ) ;
#25713 = AXIS2_PLACEMENT_3D ( 'NONE', #29755, #53691, #118177 ) ;
#25714 = VECTOR ( 'NONE', #65166, 1000.000000000000227 ) ;
#25716 = LINE ( 'NONE', #67847, #70791 ) ;
#25715 =( GEOMETRIC_REPRESENTATION_CONTEXT ( 3 ) GLOBAL_UNCERTAINTY_ASSIGNED_CONTEXT ( ( #38863 ) ) GLOBAL_UNIT_ASSIGNED_CONTEXT ( ( #142435, #77195, #80058 ) ) REPRESENTATION_CONTEXT ( 'NONE', 'WORKASPACE' ) );
#25717 = CARTESIAN_POINT ( 'NONE',  ( -20.99451991528748707, 28.92564299267952777, 4.000000000000000000 ) ) ;
#25718 = CARTESIAN_POINT ( 'NONE',  ( 43.14583333333332860, 2.130196079827431976, -7.949999999999998401 ) ) ;
#25719 = DIRECTION ( 'NONE',  ( -1.000000000000000000, -1.224606353822377258E-16, -0.000000000000000000 ) ) ;
#25721 = ORIENTED_EDGE ( 'NONE', *, *, #42137, .T. ) ;
#25720 = LINE ( 'NONE', #69993, #135531 ) ;
#25722 = FACE_OUTER_BOUND ( 'NONE', #14171, .T. ) ;
#25723 = CARTESIAN_POINT ( 'NONE',  ( 0.000000000000000000, 0.000000000000000000, 5.000000000000000000 ) ) ;
#25724 = LINE ( 'NONE', #69997, #12330 ) ;
#25725 = AXIS2_PLACEMENT_3D ( 'NONE', #136077, #110724, #81007 ) ;
#25726 = ADVANCED_FACE ( 'NONE', ( #122039 ), #66272, .F. ) ;
#25727 = ORIENTED_EDGE ( 'NONE', *, *, #5153, .F. ) ;
#25728 = EDGE_CURVE ( 'NONE', #52039, #90340, #135118, .T. ) ;
#25729 = ORIENTED_EDGE ( 'NONE', *, *, #39468, .F. ) ;
#25730 = AXIS2_PLACEMENT_3D ( 'NONE', #6824, #140253, #94577 ) ;
#25731 = DIRECTION ( 'NONE',  ( -0.000000000000000000, 0.000000000000000000, 1.000000000000000000 ) ) ;
#25732 = EDGE_CURVE ( 'NONE', #40790, #81729, #22707, .T. ) ;
#25733 = CARTESIAN_POINT ( 'NONE',  ( 1.499999999999987566, -2.568876922607790103, 4.000000000000000000 ) ) ;
#25734 = MECHANICAL_DESIGN_GEOMETRIC_PRESENTATION_REPRESENTATION (  '', ( #58180 ), #7174 ) ;
#25735 = CARTESIAN_POINT ( 'NONE',  ( -25.17183060077629264, 0.7592924766157173044, 4.000000000000000000 ) ) ;
#25736 = DIRECTION ( 'NONE',  ( 0.7071067811865487940, 0.7071067811865463515, 0.000000000000000000 ) ) ;
#25737 = EDGE_LOOP ( 'NONE', ( #118478, #139867, #120670, #82514 ) ) ;
#25738 = EDGE_LOOP ( 'NONE', ( #120267, #92285, #10055, #109661 ) ) ;
#25739 = DIRECTION ( 'NONE',  ( -0.7071067811865487940, 0.7071067811865463515, 0.000000000000000000 ) ) ;
#25740 = EDGE_CURVE ( 'NONE', #26466, #45983, #111156, .T. ) ;
#25741 = VECTOR ( 'NONE', #98676, 1000.000000000000114 ) ;
#25742 = EDGE_LOOP ( 'NONE', ( #69325, #32223, #66386, #45708, #116129 ) ) ;
#25743 = VECTOR ( 'NONE', #84599, 1000.000000000000000 ) ;
#25744 = FILL_AREA_STYLE_COLOUR ( '', #111523 ) ;
#25745 = VERTEX_POINT ( 'NONE', #99569 ) ;
#25746 = VECTOR ( 'NONE', #80380, 1000.000000000000227 ) ;
#25747 = FACE_OUTER_BOUND ( 'NONE', #120181, .T. ) ;
#25748 = DIRECTION ( 'NONE',  ( -0.7071067811865486830, -0.7071067811865464625, -0.000000000000000000 ) ) ;
#25749 = VECTOR ( 'NONE', #132871, 1000.000000000000000 ) ;
#25750 = ORIENTED_EDGE ( 'NONE', *, *, #142025, .T. ) ;
#25751 = FACE_BOUND ( 'NONE', #135601, .T. ) ;
#25752 = VECTOR ( 'NONE', #50118, 1000.000000000000000 ) ;
#25753 = CYLINDRICAL_SURFACE ( 'NONE', #117262, 2.500000000000000000 ) ;
#25754 = CARTESIAN_POINT ( 'NONE',  ( 4.911592354503321545, -2.500000000000000444, 3.061616997868384620E-16 ) ) ;
#25755 = CARTESIAN_POINT ( 'NONE',  ( 36.68336038379622721, -2.130196079827426203, 7.949999999999996625 ) ) ;
#25756 = DIRECTION ( 'NONE',  ( 0.7071067811865486830, -0.7071067811865464625, -0.000000000000000000 ) ) ;
#25757 =( NAMED_UNIT ( * ) PLANE_ANGLE_UNIT ( ) SI_UNIT ( $, .RADIAN. ) );
#25758 = VERTEX_POINT ( 'NONE', #44546 ) ;
#25759 = VECTOR ( 'NONE', #128121, 999.9999999999998863 ) ;
#25760 = EDGE_LOOP ( 'NONE', ( #110190, #3416, #89841, #77109 ) ) ;
#25761 = CARTESIAN_POINT ( 'NONE',  ( 98.34959685856479439, 6.109999999999996767, 1.637169565754163836 ) ) ;
#25762 = ORIENTED_EDGE ( 'NONE', *, *, #6635, .T. ) ;
#25763 = CARTESIAN_POINT ( 'NONE',  ( 18.95833333333333570, -3.047499999999997211, -5.278424836066143655 ) ) ;
#25764 = VECTOR ( 'NONE', #2151, 1000.000000000000227 ) ;
#25765 = DIRECTION ( 'NONE',  ( 0.7071067811865487940, 0.7071067811865463515, -0.000000000000000000 ) ) ;
#25766 = VECTOR ( 'NONE', #42637, 1000.000000000000000 ) ;
#25767 = CARTESIAN_POINT ( 'NONE',  ( 12.35051985313232237, 4.584330080086930965E-16, 0.000000000000000000 ) ) ;
#25768 = DIRECTION ( 'NONE',  ( 0.000000000000000000, 1.000000000000000000, 0.000000000000000000 ) ) ;
#25769 = ORIENTED_EDGE ( 'NONE', *, *, #73282, .T. ) ;
#25770 = CARTESIAN_POINT ( 'NONE',  ( 18.17159235450331778, 9.902892378096218942E-16, 0.000000000000000000 ) ) ;
#25771 =( NAMED_UNIT ( * ) PLANE_ANGLE_UNIT ( ) SI_UNIT ( $, .RADIAN. ) );
#25772 = DIRECTION ( 'NONE',  ( -0.000000000000000000, 0.3543493200069153248, 0.9351131265310292928 ) ) ;
#25773 = CARTESIAN_POINT ( 'NONE',  ( 27.78752705046289151, 0.000000000000000000, -7.949999999999998401 ) ) ;
#25774 = VECTOR ( 'NONE', #40653, 1000.000000000000000 ) ;
#25775 = DIRECTION ( 'NONE',  ( 0.7071067811865486830, -0.7071067811865464625, -0.000000000000000000 ) ) ;
#25776 = EDGE_LOOP ( 'NONE', ( #20644, #13038, #97053, #52202 ) ) ;
#25777 = CARTESIAN_POINT ( 'NONE',  ( 12.18398860626900060, 28.73617430169795739, 5.000000000000000000 ) ) ;
#25778 = CARTESIAN_POINT ( 'NONE',  ( -12.70000000000000284, -34.64999999999999147, -39.50000000000000000 ) ) ;
#25779 = EDGE_CURVE ( 'NONE', #14666, #52856, #46829, .T. ) ;
#25780 = ORIENTED_EDGE ( 'NONE', *, *, #138182, .T. ) ;
#25781 = ORIENTED_EDGE ( 'NONE', *, *, #92911, .T. ) ;
#25782 = EDGE_CURVE ( 'NONE', #50596, #22720, #56135, .T. ) ;
#25783 = ADVANCED_FACE ( 'NONE', ( #89429 ), #34342, .T. ) ;
#25784 = VERTEX_POINT ( 'NONE', #16877 ) ;
#25785 = CARTESIAN_POINT ( 'NONE',  ( 43.60459685856476852, 1.637169565754164946, -6.109999999999999432 ) ) ;
#25786 = VECTOR ( 'NONE', #40674, 1000.000000000000227 ) ;
#25787 = VERTEX_POINT ( 'NONE', #115422 ) ;
#25788 = EDGE_CURVE ( 'NONE', #50127, #1245, #116182, .T. ) ;
#25789 = EDGE_CURVE ( 'NONE', #61139, #106547, #102475, .T. ) ;
#25790 = CARTESIAN_POINT ( 'NONE',  ( 9.524972949537108491, -4.461849672132299993, -4.461849672132299105 ) ) ;
#25791 = DIRECTION ( 'NONE',  ( 0.7071067811865487940, 0.7071067811865463515, 0.000000000000000000 ) ) ;
#25792 = ORIENTED_EDGE ( 'NONE', *, *, #119689, .T. ) ;
#25793 = ADVANCED_FACE ( 'NONE', ( #27025 ), #25588, .F. ) ;
#25794 = FACE_OUTER_BOUND ( 'NONE', #11194, .T. ) ;
#25795 = ORIENTED_EDGE ( 'NONE', *, *, #35700, .F. ) ;
#25796 = FACE_OUTER_BOUND ( 'NONE', #143286, .T. ) ;
#25797 = VECTOR ( 'NONE', #12086, 1000.000000000000227 ) ;
#25799 = ORIENTED_EDGE ( 'NONE', *, *, #57998, .T. ) ;
#25798 = DIRECTION ( 'NONE',  ( -0.000000000000000000, 0.3543493200069153248, 0.9351131265310292928 ) ) ;
#25800 = VERTEX_POINT ( 'NONE', #113309 ) ;
#25801 = CARTESIAN_POINT ( 'NONE',  ( -25.39999999999996305, 3.061616997868383141E-16, -2.500000000000000000 ) ) ;
#25802 = CARTESIAN_POINT ( 'NONE',  ( -42.18398860626899705, 28.73617430169816700, 5.000000000000000000 ) ) ;
#25804 = LINE ( 'NONE', #62559, #79924 ) ;
#25803 = AXIS2_PLACEMENT_3D ( 'NONE', #118318, #28492, #86440 ) ;
#25805 = EDGE_CURVE ( 'NONE', #92363, #27557, #58291, .T. ) ;
#25807 = VERTEX_POINT ( 'NONE', #71271 ) ;
#25806 = VECTOR ( 'NONE', #43955, 999.9999999999998863 ) ;
#25808 = CARTESIAN_POINT ( 'NONE',  ( -51.18398860626899705, 28.73617430169823095, 5.000000000000000000 ) ) ;
#25809 = VERTEX_POINT ( 'NONE', #24883 ) ;
#25810 = ORIENTED_EDGE ( 'NONE', *, *, #58757, .T. ) ;
#25811 = VERTEX_POINT ( 'NONE', #92267 ) ;
#25812 = VECTOR ( 'NONE', #36037, 999.9999999999998863 ) ;
#25813 = VECTOR ( 'NONE', #91842, 1000.000000000000000 ) ;
#25814 = AXIS2_PLACEMENT_3D ( 'NONE', #11374, #100583, #79590 ) ;
#25815 = CIRCLE ( 'NONE', #65279, 2.500000000000000888 ) ;
#25816 = ADVANCED_FACE ( 'NONE', ( #3799 ), #16116, .F. ) ;
#25817 = AXIS2_PLACEMENT_3D ( 'NONE', #10126, #86284, #107983 ) ;
#25818 = SURFACE_SIDE_STYLE ('',( #102686 ) ) ;
#25819 = DIRECTION ( 'NONE',  ( -0.7071067811865486830, 0.7071067811865464625, 0.000000000000000000 ) ) ;
#25820 = PLANE ( 'NONE',  #122772 ) ;
#25821 = CARTESIAN_POINT ( 'NONE',  ( 2.356812572482602786, -20.24070752338407786, 21.22881796311213520 ) ) ;
#25822 = VERTEX_POINT ( 'NONE', #81447 ) ;
#25823 = EDGE_CURVE ( 'NONE', #48102, #90432, #36484, .T. ) ;
#25824 = PLANE ( 'NONE',  #65652 ) ;
#25825 = CARTESIAN_POINT ( 'NONE',  ( 23.60373647476854941, 5.808823158059036373, 5.808823158059032821 ) ) ;
#25826 = DIRECTION ( 'NONE',  ( 0.000000000000000000, 0.000000000000000000, 1.000000000000000000 ) ) ;
#25827 = CARTESIAN_POINT ( 'NONE',  ( 68.99451991528748351, 28.92564299267986172, 4.000000000000000000 ) ) ;
#25828 = CIRCLE ( 'NONE', #58287, 2.500000000000000888 ) ;
#25829 = DIRECTION ( 'NONE',  ( 0.000000000000000000, 0.000000000000000000, -1.000000000000000000 ) ) ;
#25830 = ORIENTED_EDGE ( 'NONE', *, *, #105147, .T. ) ;
#25831 = ORIENTED_EDGE ( 'NONE', *, *, #26247, .T. ) ;
#25833 = ORIENTED_EDGE ( 'NONE', *, *, #89071, .F. ) ;
#25832 = EDGE_CURVE ( 'NONE', #33166, #42524, #103160, .T. ) ;
#25834 = DIRECTION ( 'NONE',  ( 0.000000000000000000, -1.000000000000000000, 0.000000000000000000 ) ) ;
#25835 = UNCERTAINTY_MEASURE_WITH_UNIT (LENGTH_MEASURE( 1.000000000000000082E-05 ), #68450, 'distance_accuracy_value', 'NONE');
#25836 = DIRECTION ( 'NONE',  ( 0.7071067811865487940, -0.7071067811865463515, 0.000000000000000000 ) ) ;
#25837 = FACE_OUTER_BOUND ( 'NONE', #49843, .T. ) ;
#25838 = FACE_OUTER_BOUND ( 'NONE', #106280, .T. ) ;
#25839 = CARTESIAN_POINT ( 'NONE',  ( 9.489213562373095101, -27.52281430457062328, 5.000000000000000000 ) ) ;
#25840 = COLOUR_RGB ( '', 0.08235294, 0.09019608, 0.10196078) ;
#25841 = CARTESIAN_POINT ( 'NONE',  ( 80.33333333333334281, -6.884901960086287964, 3.974999999999998312 ) ) ;
#25842 = EDGE_CURVE ( 'NONE', #28959, #11288, #127042, .T. ) ;
#25843 = CIRCLE ( 'NONE', #23458, 2.055000000000001048 ) ;
#25844 = CARTESIAN_POINT ( 'NONE',  ( -3.475126127850438618, 14.25929247661557397, 9.797011795316629801 ) ) ;
#25845 = CARTESIAN_POINT ( 'NONE',  ( 7.828169399223476432, 21.75929247661548871, 4.000000000000000000 ) ) ;
#25846 = DIRECTION ( 'NONE',  ( 0.7071067811865487940, -0.7071067811865463515, 0.000000000000000000 ) ) ;
#25847 = ADVANCED_FACE ( 'NONE', ( #5254 ), #69130, .F. ) ;
#25848 = AXIS2_PLACEMENT_3D ( 'NONE', #69700, #136344, #113883 ) ;
#25849 = PLANE ( 'NONE',  #51110 ) ;
#25850 = ORIENTED_EDGE ( 'NONE', *, *, #25136, .F. ) ;
#25851 = AXIS2_PLACEMENT_3D ( 'NONE', #22272, #65862, #110017 ) ;
#25852 = VERTEX_POINT ( 'NONE', #15401 ) ;
#25853 = ADVANCED_FACE ( 'NONE', ( #4494 ), #48799, .F. ) ;
#25854 = DIRECTION ( 'NONE',  ( 0.7071067811865487940, 0.7071067811865463515, -0.000000000000000000 ) ) ;
#25856 = ORIENTED_EDGE ( 'NONE', *, *, #117775, .F. ) ;
#25855 = CARTESIAN_POINT ( 'NONE',  ( -36.29974487139159578, -27.71228299555231445, 4.000000000000000000 ) ) ;
#25857 = FACE_OUTER_BOUND ( 'NONE', #90155, .T. ) ;
#25858 = DIRECTION ( 'NONE',  ( 0.7071067811865487940, -0.7071067811865463515, 0.000000000000000000 ) ) ;
#25859 = ORIENTED_EDGE ( 'NONE', *, *, #103131, .T. ) ;
#25860 = CARTESIAN_POINT ( 'NONE',  ( 31.49999999999977973, 11.52377502935406106, -1.522421517564156890 ) ) ;
#25861 = VERTEX_POINT ( 'NONE', #84980 ) ;
#25862 = LINE ( 'NONE', #125907, #134723 ) ;
#25863 = UNCERTAINTY_MEASURE_WITH_UNIT (LENGTH_MEASURE( 1.000000000000000082E-05 ), #97692, 'distance_accuracy_value', 'NONE');
#25864 = ORIENTED_EDGE ( 'NONE', *, *, #8711, .T. ) ;
#25865 = CIRCLE ( 'NONE', #137342, 2.500000000000000888 ) ;
#25866 = DIRECTION ( 'NONE',  ( 0.6830127018922180770, -0.6830127018922204085, -0.2588190451025213501 ) ) ;
#25867 = CARTESIAN_POINT ( 'NONE',  ( 102.8916937171295274, 2.130196079827421762, 7.950000000000001066 ) ) ;
#25868 = CARTESIAN_POINT ( 'NONE',  ( 14.99999999999990941, 4.384688058510586295, -7.090945410444652985 ) ) ;
#25869 = DIRECTION ( 'NONE',  ( 0.7071067811865487940, 0.7071067811865463515, -0.000000000000000000 ) ) ;
#25870 = ORIENTED_EDGE ( 'NONE', *, *, #64947, .T. ) ;
#25871 = EDGE_CURVE ( 'NONE', #41224, #118405, #64659, .T. ) ;
#25872 = CARTESIAN_POINT ( 'NONE',  ( 2.816011393730999401, 28.73617430169785436, 5.000000000000000000 ) ) ;
#25873 = LINE ( 'NONE', #48343, #84326 ) ;
#25874 = DIRECTION ( 'NONE',  ( 0.000000000000000000, -1.000000000000000000, 0.000000000000000000 ) ) ;
#25876 = AXIS2_PLACEMENT_3D ( 'NONE', #55890, #109528, #77640 ) ;
#25875 = CARTESIAN_POINT ( 'NONE',  ( 24.50000000000000000, 0.000000000000000000, 6.094999999999989981 ) ) ;
#25877 = CARTESIAN_POINT ( 'NONE',  ( 23.74956980810188867, 3.967499999999998916, 6.871911579029510442 ) ) ;
#25879 = VECTOR ( 'NONE', #1566, 1000.000000000000000 ) ;
#25878 = FACE_OUTER_BOUND ( 'NONE', #129067, .T. ) ;
#25880 = CARTESIAN_POINT ( 'NONE',  ( 40.22674160717809855, -11.24070752338416490, 18.24660765846991950 ) ) ;
#25881 = ORIENTED_EDGE ( 'NONE', *, *, #132212, .F. ) ;
#25882 = CARTESIAN_POINT ( 'NONE',  ( -33.18398860626899705, 28.73617430169810305, 5.000000000000000000 ) ) ;
#25883 = ORIENTED_EDGE ( 'NONE', *, *, #9743, .F. ) ;
#25884 = ADVANCED_FACE ( 'NONE', ( #8103 ), #140768, .F. ) ;
#25886 = AXIS2_PLACEMENT_3D ( 'NONE', #17911, #137607, #50585 ) ;
#25885 = CARTESIAN_POINT ( 'NONE',  ( 93.62543019189811844, 5.291415217122919401, 3.055000000000002824 ) ) ;
#25887 = CARTESIAN_POINT ( 'NONE',  ( 2.999999999999975131, -0.2811185226894337141, -5.995736974527521745 ) ) ;
#25888 = LINE ( 'NONE', #70159, #127044 ) ;
#25890 = AXIS2_PLACEMENT_3D ( 'NONE', #84347, #25640, #4536 ) ;
#25889 = LINE ( 'NONE', #126605, #12244 ) ;
#25891 = CARTESIAN_POINT ( 'NONE',  ( 127.5247579190697991, -47.99115898043766748, -37.22402166429520776 ) ) ;
#25892 = ORIENTED_EDGE ( 'NONE', *, *, #3980, .T. ) ;
#25893 = CARTESIAN_POINT ( 'NONE',  ( 0.2569208697893813342, -0.4000000000000003553, 2.015694669338588429 ) ) ;
#25894 =( BOUNDED_CURVE ( )  B_SPLINE_CURVE ( 3, ( #124123, #45176, #36406, #69050 ),
 .UNSPECIFIED., .F., .T. ) 
 B_SPLINE_CURVE_WITH_KNOTS ( ( 4, 4 ),
 ( 4.628641526727098388, 4.642507259593578794 ),
 .UNSPECIFIED. ) 
 CURVE ( )  GEOMETRIC_REPRESENTATION_ITEM ( )  RATIONAL_B_SPLINE_CURVE ( ( 1.000000000000000000, 0.9999839785185119512, 0.9999839785185119512, 1.000000000000000000 ) ) 
 REPRESENTATION_ITEM ( '' )  );
#25895 = FACE_OUTER_BOUND ( 'NONE', #1912, .T. ) ;
#25896 = EDGE_CURVE ( 'NONE', #83399, #22749, #116891, .T. ) ;
#25897 = ORIENTED_EDGE ( 'NONE', *, *, #132761, .T. ) ;
#25898 = DIRECTION ( 'NONE',  ( -0.7071067811865486830, -0.7071067811865464625, 0.000000000000000000 ) ) ;
#25899 = LINE ( 'NONE', #70853, #61122 ) ;
#25901 = ORIENTED_EDGE ( 'NONE', *, *, #14145, .F. ) ;
#25900 = DIRECTION ( 'NONE',  ( -0.7071067811865486830, -0.7071067811865464625, 0.000000000000000000 ) ) ;
#25902 = DIRECTION ( 'NONE',  ( -0.6830127018922181881, 0.6830127018922202975, -0.2588190451025214056 ) ) ;
#25903 = CARTESIAN_POINT ( 'NONE',  ( -34.49999999999976552, 13.46425560840034841, 4.994342998332165884 ) ) ;
#25904 = VECTOR ( 'NONE', #97139, 999.9999999999998863 ) ;
#25905 = CARTESIAN_POINT ( 'NONE',  ( 3.087196949643289834, 3.061616997868383141E-16, -2.500000000000000444 ) ) ;
#25906 = FACE_OUTER_BOUND ( 'NONE', #77892, .T. ) ;
#25907 = ORIENTED_EDGE ( 'NONE', *, *, #44575, .T. ) ;
#25908 = EDGE_CURVE ( 'NONE', #82619, #17176, #53803, .T. ) ;
#25909 = VERTEX_POINT ( 'NONE', #6654 ) ;
#25910 = ORIENTED_EDGE ( 'NONE', *, *, #86404, .T. ) ;
#25911 = CARTESIAN_POINT ( 'NONE',  ( 83.70876352523143282, -7.482591942790329030E-16, 6.110000000000001208 ) ) ;
#25912 = ORIENTED_EDGE ( 'NONE', *, *, #8372, .T. ) ;
#25913 = ADVANCED_FACE ( 'NONE', ( #29170 ), #95127, .F. ) ;
#25914 = CARTESIAN_POINT ( 'NONE',  ( -20.29289321881331887, -9.740707523384186217, 5.000000000000000000 ) ) ;
#25915 = CARTESIAN_POINT ( 'NONE',  ( -7.499999999999945821, 21.05218569542895324, 5.000000000000000000 ) ) ;
#25916 = CARTESIAN_POINT ( 'NONE',  ( 3.469446951953614189E-15, -6.033600742197680056, 5.000000000000000000 ) ) ;
#25917 = VERTEX_POINT ( 'NONE', #20412 ) ;
#25918 = VECTOR ( 'NONE', #124267, 1000.000000000000000 ) ;
#25919 = AXIS2_PLACEMENT_3D ( 'NONE', #129041, #38480, #52197 ) ;
#25920 = CARTESIAN_POINT ( 'NONE',  ( 102.6458333333333286, 2.130196079827470168, -7.949999999999977973 ) ) ;
#25922 = ADVANCED_FACE ( 'NONE', ( #119715 ), #17564, .F. ) ;
#25921 = LINE ( 'NONE', #34665, #69737 ) ;
#25923 = AXIS2_PLACEMENT_3D ( 'NONE', #46913, #122986, #99792 ) ;
#25924 = VECTOR ( 'NONE', #45076, 1000.000000000000227 ) ;
#25925 = CARTESIAN_POINT ( 'NONE',  ( 80.12043019189810877, 3.055000000000001936, -5.291415217122916737 ) ) ;
#25926 = EDGE_CURVE ( 'NONE', #60486, #103852, #141507, .T. ) ;
#25927 = EDGE_LOOP ( 'NONE', ( #126639, #84838, #50952, #12614 ) ) ;
#25928 = LINE ( 'NONE', #24490, #65196 ) ;
#25930 = LINE ( 'NONE', #131299, #124259 ) ;
#25929 = VECTOR ( 'NONE', #27132, 1000.000000000000000 ) ;
#25931 = LINE ( 'NONE', #15030, #612 ) ;
#25932 = VECTOR ( 'NONE', #129453, 1000.000000000000000 ) ;
#25933 = MECHANICAL_DESIGN_GEOMETRIC_PRESENTATION_REPRESENTATION (  '', ( #83915 ), #100031 ) ;
#25934 = VECTOR ( 'NONE', #46444, 1000.000000000000000 ) ;
#25935 = ORIENTED_EDGE ( 'NONE', *, *, #128341, .F. ) ;
#25936 = ORIENTED_EDGE ( 'NONE', *, *, #81730, .F. ) ;
#25937 = CARTESIAN_POINT ( 'NONE',  ( 64.58333333333332860, 6.884901960086290629, -3.974999999999994316 ) ) ;
#25938 = EDGE_CURVE ( 'NONE', #121113, #42588, #72739, .T. ) ;
#25939 = SURFACE_SIDE_STYLE ('',( #123841 ) ) ;
#25940 = CARTESIAN_POINT ( 'NONE',  ( -0.3281693992235254487, -18.74070752338409562, 4.000000000000000000 ) ) ;
#25941 = CARTESIAN_POINT ( 'NONE',  ( 16.75173015016484968, 2.055000000000001048, 0.000000000000000000 ) ) ;
#25942 =( NAMED_UNIT ( * ) PLANE_ANGLE_UNIT ( ) SI_UNIT ( $, .RADIAN. ) );
#25943 = DIRECTION ( 'NONE',  ( 0.6830127018922180770, -0.6830127018922204085, -0.2588190451025213501 ) ) ;
#25944 = CARTESIAN_POINT ( 'NONE',  ( 4.499999999999970690, 0.4311230773921797543, 4.000000000000000000 ) ) ;
#25945 = ORIENTED_EDGE ( 'NONE', *, *, #20117, .F. ) ;
#25946 = VERTEX_POINT ( 'NONE', #108840 ) ;
#25947 = CARTESIAN_POINT ( 'NONE',  ( 9.479166666666667851, 6.094999999999988205, -1.633150327867694651 ) ) ;
#25948 = ORIENTED_EDGE ( 'NONE', *, *, #15510, .T. ) ;
#25949 = AXIS2_PLACEMENT_3D ( 'NONE', #33826, #65030, #86775 ) ;
#25950 = AXIS2_PLACEMENT_3D ( 'NONE', #31640, #109185, #99010 ) ;
#25951 = CARTESIAN_POINT ( 'NONE',  ( 4.499999999999972466, 19.39370406404967540, 1.459788787078191374 ) ) ;
#25952 = EDGE_LOOP ( 'NONE', ( #910, #48842, #79667, #134857 ) ) ;
#25953 = DIRECTION ( 'NONE',  ( 0.6830127018922181881, 0.6830127018922202975, -0.2588190451025214056 ) ) ;
#25954 = DIRECTION ( 'NONE',  ( -0.7071067811865486830, 0.7071067811865464625, 0.000000000000000000 ) ) ;
#25955 = AXIS2_PLACEMENT_3D ( 'NONE', #15772, #36169, #68810 ) ;
#25956 = LINE ( 'NONE', #47060, #29952 ) ;
#25957 = VECTOR ( 'NONE', #135731, 999.9999999999998863 ) ;
#25958 = DIRECTION ( 'NONE',  ( 0.7071067811865487940, 0.7071067811865463515, 0.000000000000000000 ) ) ;
#25959 = ORIENTED_EDGE ( 'NONE', *, *, #22211, .T. ) ;
#25960 = ADVANCED_FACE ( 'NONE', ( #7394 ), #40778, .F. ) ;
#25961 = DIRECTION ( 'NONE',  ( 0.7071067811865487940, 0.7071067811865463515, 0.000000000000000000 ) ) ;
#25962 = FACE_OUTER_BOUND ( 'NONE', #73195, .T. ) ;
#25963 = VERTEX_POINT ( 'NONE', #74852 ) ;
#25964 = CARTESIAN_POINT ( 'NONE',  ( 55.78752705046288440, 0.000000000000000000, -7.949999999999998401 ) ) ;
#25965 = EDGE_LOOP ( 'NONE', ( #121718, #42606, #67254, #95329 ) ) ;
#25967 = ORIENTED_EDGE ( 'NONE', *, *, #39935, .T. ) ;
#25966 = EDGE_CURVE ( 'NONE', #49695, #49753, #9526, .T. ) ;
#25968 = CARTESIAN_POINT ( 'NONE',  ( -3.707106781186514599, 11.25929247661560240, 5.000000000000000000 ) ) ;
#25969 = VERTEX_POINT ( 'NONE', #119027 ) ;
#25970 = ORIENTED_EDGE ( 'NONE', *, *, #76244, .F. ) ;
#25971 = LINE ( 'NONE', #121861, #7028 ) ;
#25972 =( GEOMETRIC_REPRESENTATION_CONTEXT ( 3 ) GLOBAL_UNCERTAINTY_ASSIGNED_CONTEXT ( ( #5680 ) ) GLOBAL_UNIT_ASSIGNED_CONTEXT ( ( #58105, #27548, #2207 ) ) REPRESENTATION_CONTEXT ( 'NONE', 'WORKASPACE' ) );
#25973 = ORIENTED_EDGE ( 'NONE', *, *, #1558, .F. ) ;
#25974 = EDGE_CURVE ( 'NONE', #108223, #36313, #84303, .T. ) ;
#25975 = ADVANCED_FACE ( 'NONE', ( #52345 ), #29867, .F. ) ;
#25976 = CARTESIAN_POINT ( 'NONE',  ( 27.29974487139158512, -27.71228299555225405, 4.000000000000000000 ) ) ;
#25978 = EDGE_CURVE ( 'NONE', #101519, #86499, #142928, .T. ) ;
#25977 = LINE ( 'NONE', #36838, #37991 ) ;
#25979 = CARTESIAN_POINT ( 'NONE',  ( 114.3337635252314470, 6.110000000000001208, 1.122388791418549305E-15 ) ) ;
#25980 = FACE_OUTER_BOUND ( 'NONE', #33499, .T. ) ;
#25981 = EDGE_CURVE ( 'NONE', #18783, #129767, #45092, .T. ) ;
#25982 = PLANE ( 'NONE',  #20480 ) ;
#25983 = CONICAL_SURFACE ( 'NONE', #49083, 2.055000000000000604, 0.9599310885968764806 ) ;
#25984 = AXIS2_PLACEMENT_3D ( 'NONE', #34793, #121062, #46415 ) ;
#25985 = EDGE_CURVE ( 'NONE', #17335, #96047, #43610, .T. ) ;
#25986 = DIRECTION ( 'NONE',  ( -0.7071067811865486830, -0.7071067811865464625, 0.000000000000000000 ) ) ;
#25987 = DIRECTION ( 'NONE',  ( -0.6830127018922181881, 0.6830127018922202975, -0.2588190451025214056 ) ) ;
#25988 = DIRECTION ( 'NONE',  ( -0.7071067811865486830, -0.7071067811865464625, 0.000000000000000000 ) ) ;
#25989 = EDGE_CURVE ( 'NONE', #29835, #135832, #132321, .T. ) ;
#25990 = EDGE_LOOP ( 'NONE', ( #17409, #52601, #114989, #63644 ) ) ;
#25991 = CARTESIAN_POINT ( 'NONE',  ( 8.999999999999941380, 10.55218569542906160, 5.000000000000000000 ) ) ;
#25992 = CARTESIAN_POINT ( 'NONE',  ( -36.18398860626899705, 28.73617430169812437, 5.000000000000000000 ) ) ;
#25993 = VERTEX_POINT ( 'NONE', #98005 ) ;
#25994 = VERTEX_POINT ( 'NONE', #33488 ) ;
#25995 = AXIS2_PLACEMENT_3D ( 'NONE', #57256, #1381, #45668 ) ;
#25996 = LINE ( 'NONE', #126031, #100488 ) ;
#25997 = ORIENTED_EDGE ( 'NONE', *, *, #55411, .T. ) ;
#25998 = DIRECTION ( 'NONE',  ( -0.7071067811865486830, -0.7071067811865464625, 0.000000000000000000 ) ) ;
#25999 = LINE ( 'NONE', #138326, #98721 ) ;
#26001 = EDGE_CURVE ( 'NONE', #20396, #123770, #131342, .T. ) ;
#26000 = DIRECTION ( 'NONE',  ( 0.7071067811865487940, 0.7071067811865463515, 0.000000000000000000 ) ) ;
#26002 = CARTESIAN_POINT ( 'NONE',  ( 8.999999999999948486, 14.58746187583909837, 4.000000000000000000 ) ) ;
#26003 = DIRECTION ( 'NONE',  ( -0.7071067811865487940, 0.7071067811865463515, 0.000000000000000000 ) ) ;
#26004 = VERTEX_POINT ( 'NONE', #42927 ) ;
#26005 = SURFACE_SIDE_STYLE ('',( #93393 ) ) ;
#26006 = VECTOR ( 'NONE', #44999, 1000.000000000000000 ) ;
#26007 = EDGE_LOOP ( 'NONE', ( #42356, #80521, #47230, #93347 ) ) ;
#26008 = EDGE_CURVE ( 'NONE', #93151, #133915, #11662, .T. ) ;
#26009 = FACE_OUTER_BOUND ( 'NONE', #21733, .T. ) ;
#26010 = CARTESIAN_POINT ( 'NONE',  ( 31.85873647476855552, 5.808823158059031044, -5.808823158059038150 ) ) ;
#26011 = DIRECTION ( 'NONE',  ( 0.000000000000000000, -1.000000000000000000, 0.000000000000000000 ) ) ;
#26012 = DIRECTION ( 'NONE',  ( -0.7071067811865486830, 0.7071067811865464625, 0.000000000000000000 ) ) ;
#26013 = ORIENTED_EDGE ( 'NONE', *, *, #142999, .F. ) ;
#26014 = ORIENTED_EDGE ( 'NONE', *, *, #138417, .F. ) ;
#26015 = ORIENTED_EDGE ( 'NONE', *, *, #75777, .T. ) ;
#26016 = DIRECTION ( 'NONE',  ( -0.6830127018922181881, 0.6830127018922202975, -0.2588190451025214056 ) ) ;
#26017 = LINE ( 'NONE', #6342, #55746 ) ;
#26018 = AXIS2_PLACEMENT_3D ( 'NONE', #21921, #68333, #112504 ) ;
#26020 = DIRECTION ( 'NONE',  ( 0.7071067811865486830, -0.7071067811865464625, -0.000000000000000000 ) ) ;
#26019 = AXIS2_PLACEMENT_3D ( 'NONE', #15779, #64174, #140989 ) ;
#26021 = DIRECTION ( 'NONE',  ( -0.7071067811865486830, -0.7071067811865464625, -0.000000000000000000 ) ) ;
#26022 = ORIENTED_EDGE ( 'NONE', *, *, #125315, .F. ) ;
#26023 = CARTESIAN_POINT ( 'NONE',  ( 22.17665910159958997, 5.259292476615662792, 15.86257073897092518 ) ) ;
#26024 = AXIS2_PLACEMENT_3D ( 'NONE', #103347, #5454, #59193 ) ;
#26025 = CARTESIAN_POINT ( 'NONE',  ( 29.29387692260784704, 22.22500000000000497, 4.000000000000000000 ) ) ;
#26026 = VECTOR ( 'NONE', #85484, 1000.000000000000000 ) ;
#26027 = CARTESIAN_POINT ( 'NONE',  ( 8.207106781186489286, -5.240707523384232402, 5.000000000000000000 ) ) ;
#26028 = CARTESIAN_POINT ( 'NONE',  ( 34.92499999999998295, -9.281509562795639212, 4.759050581649326261 ) ) ;
#26029 = EDGE_CURVE ( 'NONE', #75514, #15522, #122588, .T. ) ;
#26030 = ORIENTED_EDGE ( 'NONE', *, *, #85244, .F. ) ;
#26031 = AXIS2_PLACEMENT_3D ( 'NONE', #28412, #51598, #38567 ) ;
#26032 = COLOUR_RGB ( '', 0.40784314, 0.44705882, 0.49803922) ;
#26033 = STYLED_ITEM ( 'NONE', ( #13607 ), #122638 ) ;
#26034 = CYLINDRICAL_SURFACE ( 'NONE', #21564, 0.5000000000000004441 ) ;
#26035 = VERTEX_POINT ( 'NONE', #100849 ) ;
#26036 = EDGE_CURVE ( 'NONE', #75052, #74837, #23263, .T. ) ;
#26038 = ORIENTED_EDGE ( 'NONE', *, *, #50281, .T. ) ;
#26037 = CARTESIAN_POINT ( 'NONE',  ( -60.18398860626900415, 28.73617430169829490, 5.000000000000000000 ) ) ;
#26039 = ORIENTED_EDGE ( 'NONE', *, *, #20414, .F. ) ;
#26040 = DIRECTION ( 'NONE',  ( -0.000000000000000000, -0.000000000000000000, 1.000000000000000000 ) ) ;
#26041 = DIRECTION ( 'NONE',  ( 0.6830127018922181881, 0.6830127018922202975, -0.2588190451025214056 ) ) ;
#26042 = ORIENTED_EDGE ( 'NONE', *, *, #125743, .T. ) ;
#26043 = CARTESIAN_POINT ( 'NONE',  ( 15.18398860626900237, 28.73617430169797871, 5.000000000000000000 ) ) ;
#26044 = UNCERTAINTY_MEASURE_WITH_UNIT (LENGTH_MEASURE( 1.000000000000000082E-05 ), #139461, 'distance_accuracy_value', 'NONE');
#26045 = ADVANCED_FACE ( 'NONE', ( #32026 ), #34903, .F. ) ;
#26046 = DIRECTION ( 'NONE',  ( -0.6830127018922180770, -0.6830127018922204085, -0.2588190451025213501 ) ) ;
#26047 = CARTESIAN_POINT ( 'NONE',  ( 0.000000000000000000, 0.000000000000000000, 5.000000000000000000 ) ) ;
#26048 = CARTESIAN_POINT ( 'NONE',  ( 31.84959685856478373, 6.109999999999997655, 1.637169565754163836 ) ) ;
#26049 = FACE_OUTER_BOUND ( 'NONE', #12058, .T. ) ;
#26050 = CARTESIAN_POINT ( 'NONE',  ( 48.49586038379622011, -3.974999999999998312, -6.884901960086286188 ) ) ;
#26051 = EDGE_CURVE ( 'NONE', #90068, #26803, #32762, .T. ) ;
#26052 = CARTESIAN_POINT ( 'NONE',  ( 153.6500000000000057, 0.000000000000000000, 4.749999999999997335 ) ) ;
#26053 = CARTESIAN_POINT ( 'NONE',  ( -2.816011393730999401, 28.73617430169785436, 5.000000000000000000 ) ) ;
#26054 = CARTESIAN_POINT ( 'NONE',  ( 23.22995720542188991, 21.73644205237998506, 5.000000000000000888 ) ) ;
#26055 = CARTESIAN_POINT ( 'NONE',  ( 26.52040314143521726, 7.934999999999989839, -2.126176841940961904 ) ) ;
#26056 = CARTESIAN_POINT ( 'NONE',  ( -1.499999999999984013, -14.94781430457067728, 5.000000000000000000 ) ) ;
#26057 = CARTESIAN_POINT ( 'NONE',  ( 45.48921356237309510, -27.52281430457087197, 5.000000000000000000 ) ) ;
#26058 = DIRECTION ( 'NONE',  ( 0.000000000000000000, -1.000000000000000000, 0.000000000000000000 ) ) ;
#26059 = CARTESIAN_POINT ( 'NONE',  ( 59.99451991528749772, 28.92564299267980132, 4.000000000000000000 ) ) ;
#26060 = VERTEX_POINT ( 'NONE', #10950 ) ;
#26061 = VECTOR ( 'NONE', #40264, 1000.000000000000000 ) ;
#26062 = ORIENTED_EDGE ( 'NONE', *, *, #78689, .T. ) ;
#26063 = CARTESIAN_POINT ( 'NONE',  ( 88.20833333333332860, -3.974999999999999201, -6.884901960086287964 ) ) ;
#26064 = ORIENTED_EDGE ( 'NONE', *, *, #98349, .T. ) ;
#26065 = VERTEX_POINT ( 'NONE', #121163 ) ;
#26066 = EDGE_CURVE ( 'NONE', #113921, #118671, #89956, .T. ) ;
#26067 = VECTOR ( 'NONE', #94786, 1000.000000000000000 ) ;
#26068 = DIRECTION ( 'NONE',  ( 0.7071067811865487940, 0.7071067811865463515, -0.000000000000000000 ) ) ;
#26069 = CARTESIAN_POINT ( 'NONE',  ( 1.998069433179001653, -22.22500000000000142, 4.500000000000000888 ) ) ;
#26070 =( GEOMETRIC_REPRESENTATION_CONTEXT ( 3 ) GLOBAL_UNCERTAINTY_ASSIGNED_CONTEXT ( ( #2461 ) ) GLOBAL_UNIT_ASSIGNED_CONTEXT ( ( #59794, #44099, #110729 ) ) REPRESENTATION_CONTEXT ( 'NONE', 'WORKASPACE' ) );
#26071 = VECTOR ( 'NONE', #134876, 1000.000000000000000 ) ;
#26072 = CARTESIAN_POINT ( 'NONE',  ( 12.27715408423077648, 8.651771236590469982, 3.925780828071965267 ) ) ;
#26073 = ORIENTED_EDGE ( 'NONE', *, *, #3588, .T. ) ;
#26074 = CARTESIAN_POINT ( 'NONE',  ( 28.49999999999980105, -10.04351517176476172, -1.623559851933757958 ) ) ;
#26075 = FACE_OUTER_BOUND ( 'NONE', #88484, .T. ) ;
#26076 = CARTESIAN_POINT ( 'NONE',  ( 11.81601139373100651, 28.73617430169779041, 5.000000000000000000 ) ) ;
#26077 = CARTESIAN_POINT ( 'NONE',  ( 125.9962588284267184, 4.199175705864780284, -6.163519753944560975 ) ) ;
#26078 = EDGE_CURVE ( 'NONE', #80179, #112545, #79429, .T. ) ;
#26079 = ADVANCED_FACE ( 'NONE', ( #109581 ), #21858, .T. ) ;
#26081 = ADVANCED_FACE ( 'NONE', ( #10258 ), #110981, .F. ) ;
#26080 = CARTESIAN_POINT ( 'NONE',  ( -48.48921356237309510, -27.52281430457089328, 5.000000000000000000 ) ) ;
#26082 = DIRECTION ( 'NONE',  ( 0.7071067811865486830, -0.7071067811865464625, -0.000000000000000000 ) ) ;
#26083 = DIRECTION ( 'NONE',  ( -0.000000000000000000, 0.3543493200069153248, 0.9351131265310292928 ) ) ;
#26084 = PLANE ( 'NONE',  #45246 ) ;
#26085 = DIRECTION ( 'NONE',  ( -0.7071067811865486830, -0.7071067811865464625, -0.000000000000000000 ) ) ;
#26086 = CARTESIAN_POINT ( 'NONE',  ( 12.18398860626900060, 28.73617430169795739, 5.000000000000000000 ) ) ;
#26087 = PLANE ( 'NONE',  #15178 ) ;
#26088 = CARTESIAN_POINT ( 'NONE',  ( 55.71344734891374628, -51.77943056867389515, 39.18578444878559708 ) ) ;
#26089 = EDGE_CURVE ( 'NONE', #4447, #55801, #114567, .T. ) ;
#26090 = ORIENTED_EDGE ( 'NONE', *, *, #10838, .F. ) ;
#26091 = VERTEX_POINT ( 'NONE', #81996 ) ;
#26092 = CARTESIAN_POINT ( 'NONE',  ( 108.7920968585647756, -5.291415217122921177, 3.054999999999999272 ) ) ;
#26093 = ORIENTED_EDGE ( 'NONE', *, *, #80863, .T. ) ;
#26094 = VECTOR ( 'NONE', #132413, 1000.000000000000000 ) ;
#26095 = CARTESIAN_POINT ( 'NONE',  ( -19.49999999999986500, 12.43112307739205669, 4.000000000000000000 ) ) ;
#26096 = DIRECTION ( 'NONE',  ( -0.7071067811865486830, -0.7071067811865464625, 0.000000000000000000 ) ) ;
#26097 = VERTEX_POINT ( 'NONE', #113863 ) ;
#26098 = PLANE ( 'NONE',  #67612 ) ;
#26100 = EDGE_CURVE ( 'NONE', #31004, #60184, #15236, .T. ) ;
#26099 = FACE_OUTER_BOUND ( 'NONE', #5474, .T. ) ;
#26101 = CARTESIAN_POINT ( 'NONE',  ( 105.3495968585647944, 6.109999999999996767, 1.637169565754163836 ) ) ;
#26102 = EDGE_CURVE ( 'NONE', #114079, #51588, #137050, .T. ) ;
#26103 = ORIENTED_EDGE ( 'NONE', *, *, #86740, .T. ) ;
#26104 = EDGE_LOOP ( 'NONE', ( #115477, #91178, #36005, #51860 ) ) ;
#26105 = CARTESIAN_POINT ( 'NONE',  ( 14.70692117890024697, -2.500000000000000000, 3.061616997868383634E-16 ) ) ;
#26106 = VECTOR ( 'NONE', #47029, 1000.000000000000000 ) ;
#26107 = DIRECTION ( 'NONE',  ( -0.000000000000000000, -0.000000000000000000, 1.000000000000000000 ) ) ;
#26108 = CARTESIAN_POINT ( 'NONE',  ( 39.18398860626899705, 28.73617430169814568, 5.000000000000000000 ) ) ;
#26109 = ORIENTED_EDGE ( 'NONE', *, *, #126522, .T. ) ;
#26110 = ORIENTED_EDGE ( 'NONE', *, *, #23606, .F. ) ;
#26111 = ORIENTED_EDGE ( 'NONE', *, *, #87183, .F. ) ;
#26112 = CARTESIAN_POINT ( 'NONE',  ( 9.781626882924877364, 21.74787736706807095, 4.999607392498048419 ) ) ;
#26113 = EDGE_CURVE ( 'NONE', #19552, #141993, #115982, .T. ) ;
#26114 = VECTOR ( 'NONE', #82780, 999.9999999999998863 ) ;
#26115 = DIRECTION ( 'NONE',  ( 0.000000000000000000, 0.000000000000000000, 1.000000000000000000 ) ) ;
#26116 = ORIENTED_EDGE ( 'NONE', *, *, #99351, .F. ) ;
#26117 = EDGE_LOOP ( 'NONE', ( #101439, #44321, #103175, #96317, #116610 ) ) ;
#26118 = ORIENTED_EDGE ( 'NONE', *, *, #19109, .F. ) ;
#26119 = ORIENTED_EDGE ( 'NONE', *, *, #48279, .F. ) ;
#26120 = VECTOR ( 'NONE', #103045, 1000.000000000000000 ) ;
#26121 = VECTOR ( 'NONE', #137986, 1000.000000000000000 ) ;
#26122 = DIRECTION ( 'NONE',  ( -0.7071067811865486830, 0.7071067811865464625, 0.000000000000000000 ) ) ;
#26123 = VECTOR ( 'NONE', #50234, 999.9999999999998863 ) ;
#26124 = DIRECTION ( 'NONE',  ( 0.000000000000000000, 0.000000000000000000, 1.000000000000000000 ) ) ;
#26125 = ORIENTED_EDGE ( 'NONE', *, *, #126518, .F. ) ;
#26126 = DIRECTION ( 'NONE',  ( -0.000000000000000000, 0.000000000000000000, 1.000000000000000000 ) ) ;
#26127 = EDGE_CURVE ( 'NONE', #54291, #29863, #136325, .T. ) ;
#26128 =( GEOMETRIC_REPRESENTATION_CONTEXT ( 3 ) GLOBAL_UNCERTAINTY_ASSIGNED_CONTEXT ( ( #34583 ) ) GLOBAL_UNIT_ASSIGNED_CONTEXT ( ( #71296, #14013, #48111 ) ) REPRESENTATION_CONTEXT ( 'NONE', 'WORKASPACE' ) );
#26129 = VECTOR ( 'NONE', #18542, 1000.000000000000000 ) ;
#26130 = MECHANICAL_DESIGN_GEOMETRIC_PRESENTATION_REPRESENTATION (  '', ( #7688 ), #9970 ) ;
#26131 = FACE_OUTER_BOUND ( 'NONE', #18069, .T. ) ;
#26132 = LINE ( 'NONE', #34883, #102243 ) ;
#26133 = LINE ( 'NONE', #114549, #92757 ) ;
#26134 = FACE_BOUND ( 'NONE', #53422, .T. ) ;
#26135 = EDGE_LOOP ( 'NONE', ( #135552, #18643, #37335, #5293 ) ) ;
#26136 = FACE_OUTER_BOUND ( 'NONE', #96626, .T. ) ;
#26137 = CARTESIAN_POINT ( 'NONE',  ( 3.489213562373097322, -27.52281430457057709, 5.000000000000000000 ) ) ;
#26138 = DIRECTION ( 'NONE',  ( -0.7071067811865486830, -0.7071067811865464625, 0.000000000000000000 ) ) ;
#26139 = VERTEX_POINT ( 'NONE', #92098 ) ;
#26140 = CARTESIAN_POINT ( 'NONE',  ( 2.816011393730999401, 28.73617430169785436, 5.000000000000000000 ) ) ;
#26141 = ORIENTED_EDGE ( 'NONE', *, *, #90866, .F. ) ;
#26142 = ORIENTED_EDGE ( 'NONE', *, *, #25620, .F. ) ;
#26143 = ORIENTED_EDGE ( 'NONE', *, *, #142163, .T. ) ;
#26144 = EDGE_CURVE ( 'NONE', #51152, #8757, #124039, .T. ) ;
#26145 = CARTESIAN_POINT ( 'NONE',  ( 36.22459685856478728, -1.637169565754160949, 6.109999999999997655 ) ) ;
#26146 = ORIENTED_EDGE ( 'NONE', *, *, #79394, .T. ) ;
#26147 = VECTOR ( 'NONE', #47481, 999.9999999999998863 ) ;
#26148 = PLANE ( 'NONE',  #76186 ) ;
#26149 = ADVANCED_FACE ( 'NONE', ( #13807 ), #47935, .F. ) ;
#26150 = EDGE_CURVE ( 'NONE', #6269, #127775, #69684, .T. ) ;
#26151 = DIRECTION ( 'NONE',  ( -1.000000000000000000, -0.000000000000000000, -0.000000000000000000 ) ) ;
#26152 = CARTESIAN_POINT ( 'NONE',  ( 2.994519915287485734, 28.92564299267940342, 4.000000000000000000 ) ) ;
#26153 = VERTEX_POINT ( 'NONE', #14557 ) ;
#26154 = EDGE_CURVE ( 'NONE', #106936, #29169, #93548, .T. ) ;
#26155 = DIRECTION ( 'NONE',  ( 0.7071067811865487940, -0.7071067811865463515, 0.000000000000000000 ) ) ;
#26156 = ADVANCED_FACE ( 'NONE', ( #124742 ), #58837, .T. ) ;
#26158 =( NAMED_UNIT ( * ) SI_UNIT ( $, .STERADIAN. ) SOLID_ANGLE_UNIT ( ) );
#26157 = AXIS2_PLACEMENT_3D ( 'NONE', #33162, #32415, #120083 ) ;
#26159 = SURFACE_STYLE_FILL_AREA ( #116726 ) ;
#26160 = CARTESIAN_POINT ( 'NONE',  ( -10.49999999999992539, 6.431123077392117082, 4.000000000000000000 ) ) ;
#26161 = AXIS2_PLACEMENT_3D ( 'NONE', #106763, #6704, #50986 ) ;
#26162 = DIRECTION ( 'NONE',  ( 0.6830127018922180770, -0.6830127018922204085, -0.2588190451025213501 ) ) ;
#26163 = EDGE_CURVE ( 'NONE', #73090, #3334, #46526, .T. ) ;
#26164 = ORIENTED_EDGE ( 'NONE', *, *, #71165, .F. ) ;
#26165 = ORIENTED_EDGE ( 'NONE', *, *, #68898, .T. ) ;
#26166 = EDGE_LOOP ( 'NONE', ( #94228, #33451, #39347, #94884 ) ) ;
#26167 = ORIENTED_EDGE ( 'NONE', *, *, #120535, .F. ) ;
#26168 = PLANE ( 'NONE',  #58830 ) ;
#26169 = ORIENTED_EDGE ( 'NONE', *, *, #16404, .T. ) ;
#26170 = EDGE_LOOP ( 'NONE', ( #121047, #93144, #126093, #34921 ) ) ;
#26171 = PLANE ( 'NONE',  #132377 ) ;
#26173 = ADVANCED_FACE ( 'NONE', ( #71103 ), #15932, .F. ) ;
#26172 = FACE_OUTER_BOUND ( 'NONE', #100355, .T. ) ;
#26174 = ADVANCED_FACE ( 'NONE', ( #52173 ), #62363, .F. ) ;
#26175 = LINE ( 'NONE', #38474, #64851 ) ;
#26176 = ORIENTED_EDGE ( 'NONE', *, *, #83036, .T. ) ;
#26177 = LINE ( 'NONE', #58127, #118165 ) ;
#26178 = VERTEX_POINT ( 'NONE', #29692 ) ;
#26179 = EDGE_CURVE ( 'NONE', #43903, #52144, #60969, .T. ) ;
#26181 = VECTOR ( 'NONE', #84188, 1000.000000000000000 ) ;
#26180 = CARTESIAN_POINT ( 'NONE',  ( -3.328169399223503966, 8.259292476615637923, 4.000000000000000000 ) ) ;
#26182 = LINE ( 'NONE', #70444, #77430 ) ;
#26183 = CARTESIAN_POINT ( 'NONE',  ( 1.817069808101886341, -2.126176841940956130, 7.934999999999991616 ) ) ;
#26184 = ORIENTED_EDGE ( 'NONE', *, *, #66179, .F. ) ;
#26186 = CARTESIAN_POINT ( 'NONE',  ( 0.000000000000000000, 0.000000000000000000, 5.000000000000000000 ) ) ;
#26185 = CARTESIAN_POINT ( 'NONE',  ( 104.9120968585647802, 5.291415217122922066, -3.054999999999995275 ) ) ;
#26187 = CARTESIAN_POINT ( 'NONE',  ( -25.39999999999996305, 0.000000000000000000, 2.500000000000000000 ) ) ;
#26188 = LINE ( 'NONE', #123379, #62777 ) ;
#26189 = EDGE_LOOP ( 'NONE', ( #120899, #79337, #135358 ) ) ;
#26190 = AXIS2_PLACEMENT_3D ( 'NONE', #132438, #135281, #13436 ) ;
#26191 = EDGE_LOOP ( 'NONE', ( #9931, #143466, #26763, #142696 ) ) ;
#26192 = ORIENTED_EDGE ( 'NONE', *, *, #104244, .F. ) ;
#26194 = VECTOR ( 'NONE', #128591, 1000.000000000000227 ) ;
#26193 = CARTESIAN_POINT ( 'NONE',  ( -7.499999999999944045, -17.94781430457063820, 5.000000000000000000 ) ) ;
#26195 = CARTESIAN_POINT ( 'NONE',  ( 18.32816939922340893, 17.25929247661554200, 4.000000000000000000 ) ) ;
#26196 = DIRECTION ( 'NONE',  ( 0.7071067811865486830, -0.7071067811865464625, -0.000000000000000000 ) ) ;
#26197 = CARTESIAN_POINT ( 'NONE',  ( 6.471592354503322042, 9.902892378096218942E-16, 0.000000000000000000 ) ) ;
#26198 = ORIENTED_EDGE ( 'NONE', *, *, #73012, .T. ) ;
#26199 = LINE ( 'NONE', #39958, #62162 ) ;
#26200 = DIRECTION ( 'NONE',  ( -0.000000000000000000, 0.3543493200069153248, 0.9351131265310292928 ) ) ;
#26201 = FACE_OUTER_BOUND ( 'NONE', #40766, .T. ) ;
#26202 = EDGE_CURVE ( 'NONE', #100179, #127004, #105129, .T. ) ;
#26203 = ORIENTED_EDGE ( 'NONE', *, *, #70832, .F. ) ;
#26204 = DIRECTION ( 'NONE',  ( 0.6830127018922180770, -0.6830127018922204085, -0.2588190451025213501 ) ) ;
#26205 = MECHANICAL_DESIGN_GEOMETRIC_PRESENTATION_REPRESENTATION (  '', ( #88724 ), #54072 ) ;
#26206 = LINE ( 'NONE', #90765, #93274 ) ;
#26207 = VERTEX_POINT ( 'NONE', #118857 ) ;
#26209 = ORIENTED_EDGE ( 'NONE', *, *, #31623, .T. ) ;
#26208 = DIRECTION ( 'NONE',  ( 0.7071067811865486830, -0.7071067811865464625, -0.000000000000000000 ) ) ;
#26210 = ORIENTED_EDGE ( 'NONE', *, *, #44231, .F. ) ;
#26211 = EDGE_CURVE ( 'NONE', #71184, #43157, #84129, .T. ) ;
#26212 = VECTOR ( 'NONE', #140527, 999.9999999999998863 ) ;
#26213 = PLANE ( 'NONE',  #2976 ) ;
#26214 = DIRECTION ( 'NONE',  ( -4.681814790819591790E-17, -0.3543493200069152693, 0.9351131265310292928 ) ) ;
#26215 = ORIENTED_EDGE ( 'NONE', *, *, #60740, .T. ) ;
#26216 = CARTESIAN_POINT ( 'NONE',  ( 33.18398860626899705, 28.73617430169810305, 5.000000000000000000 ) ) ;
#26217 = EDGE_CURVE ( 'NONE', #129157, #41854, #129728, .T. ) ;
#26218 = PLANE ( 'NONE',  #109959 ) ;
#26219 = ORIENTED_EDGE ( 'NONE', *, *, #53473, .F. ) ;
#26220 = DIRECTION ( 'NONE',  ( -0.7071067811865486830, -0.7071067811865464625, 0.000000000000000000 ) ) ;
#26221 = LINE ( 'NONE', #93619, #79099 ) ;
#26222 = ADVANCED_FACE ( 'NONE', ( #6476 ), #40605, .F. ) ;
#26223 = FILL_AREA_STYLE ('',( #13877 ) ) ;
#26224 = VECTOR ( 'NONE', #5669, 1000.000000000000000 ) ;
#26225 = DIRECTION ( 'NONE',  ( 0.7071067811865487940, 0.7071067811865463515, 0.000000000000000000 ) ) ;
#26226 = CARTESIAN_POINT ( 'NONE',  ( 27.99999999999999645, -57.14999999999999147, -49.92499999999968452 ) ) ;
#26227 = CARTESIAN_POINT ( 'NONE',  ( 10.49999999999992717, -13.91253812416061209, 4.000000000000000000 ) ) ;
#26228 = EDGE_LOOP ( 'NONE', ( #45202, #101419, #42025, #66753, #17994, #139240 ) ) ;
#26229 = AXIS2_PLACEMENT_3D ( 'NONE', #2216, #79149, #55221 ) ;
#26230 = ORIENTED_EDGE ( 'NONE', *, *, #137422, .F. ) ;
#26231 = ORIENTED_EDGE ( 'NONE', *, *, #7341, .F. ) ;
#26232 = CARTESIAN_POINT ( 'NONE',  ( 122.9166666666666714, -6.884901960086287076, -3.975000000000000977 ) ) ;
#26233 = ORIENTED_EDGE ( 'NONE', *, *, #137442, .T. ) ;
#26234 = ORIENTED_EDGE ( 'NONE', *, *, #94022, .F. ) ;
#26235 = EDGE_CURVE ( 'NONE', #75711, #39393, #50055, .T. ) ;
#26236 = EDGE_LOOP ( 'NONE', ( #99124, #60311, #83034, #37414 ) ) ;
#26237 = VECTOR ( 'NONE', #95808, 1000.000000000000000 ) ;
#26238 = CYLINDRICAL_SURFACE ( 'NONE', #119628, 28.00000000000003197 ) ;
#26239 = COLOUR_RGB ( '', 0.40784314, 0.44705882, 0.49803922) ;
#26240 = LINE ( 'NONE', #105212, #41677 ) ;
#26241 = VERTEX_POINT ( 'NONE', #74669 ) ;
#26242 = PRESENTATION_LAYER_ASSIGNMENT (  '', '', ( #14645 ) ) ;
#26243 = CARTESIAN_POINT ( 'NONE',  ( 19.10840764549667270, -3.851859888774471706E-31, 2.500000000000001332 ) ) ;
#26244 = CARTESIAN_POINT ( 'NONE',  ( -3.489213562373097322, -27.52281430457057709, 5.000000000000000000 ) ) ;
#26245 = FACE_OUTER_BOUND ( 'NONE', #117675, .T. ) ;
#26246 = CARTESIAN_POINT ( 'NONE',  ( 111.1254301918981042, 5.291415217122919401, 3.055000000000002824 ) ) ;
#26247 = EDGE_CURVE ( 'NONE', #75231, #13355, #39169, .T. ) ;
#26248 = ORIENTED_EDGE ( 'NONE', *, *, #27395, .F. ) ;
#26249 = CARTESIAN_POINT ( 'NONE',  ( 3.489213562373097322, -27.52281430457057709, 5.000000000000000000 ) ) ;
#26250 = DIRECTION ( 'NONE',  ( 0.6830127018922180770, -0.6830127018922204085, -0.2588190451025213501 ) ) ;
#26251 = CARTESIAN_POINT ( 'NONE',  ( -28.49999999999980460, -16.53360074219757081, 5.000000000000000000 ) ) ;
#26252 = CARTESIAN_POINT ( 'NONE',  ( 0.8414140276721195910, 6.733540184995763234, 2.728539860749207513 ) ) ;
#26253 = LINE ( 'NONE', #59613, #54420 ) ;
#26254 = CARTESIAN_POINT ( 'NONE',  ( 32.99999999999977263, -7.068876922607732816, 4.000000000000000000 ) ) ;
#26255 = CARTESIAN_POINT ( 'NONE',  ( -54.48921356237310221, -27.52281430457093236, 5.000000000000000000 ) ) ;
#26256 = CARTESIAN_POINT ( 'NONE',  ( 34.93336038379622011, 2.130196079827431532, -7.949999999999997513 ) ) ;
#26257 = CARTESIAN_POINT ( 'NONE',  ( 11.56505274454301357, 4.584330080086930965E-16, 0.000000000000000000 ) ) ;
#26259 = CARTESIAN_POINT ( 'NONE',  ( 16.49230000000001439, 3.130000000000008331, 0.000000000000000000 ) ) ;
#26258 = VECTOR ( 'NONE', #137853, 1000.000000000000000 ) ;
#26260 = EDGE_LOOP ( 'NONE', ( #27462, #140780, #85406, #29643 ) ) ;
#26261 = ORIENTED_EDGE ( 'NONE', *, *, #49349, .F. ) ;
#26262 = CARTESIAN_POINT ( 'NONE',  ( 36.43750000000000000, 5.819803920172573974, -5.819803920172572198 ) ) ;
#26263 = ORIENTED_EDGE ( 'NONE', *, *, #114155, .F. ) ;
#26264 = ORIENTED_EDGE ( 'NONE', *, *, #81670, .T. ) ;
#26265 = DIRECTION ( 'NONE',  ( 0.7071067811865486830, -0.7071067811865464625, -0.000000000000000000 ) ) ;
#26266 = LINE ( 'NONE', #43916, #8367 ) ;
#26267 = ORIENTED_EDGE ( 'NONE', *, *, #29839, .F. ) ;
#26268 = CARTESIAN_POINT ( 'NONE',  ( 69.18398860626899705, 28.73617430169835529, 5.000000000000000000 ) ) ;
#26269 = VECTOR ( 'NONE', #113513, 1000.000000000000000 ) ;
#26270 = CARTESIAN_POINT ( 'NONE',  ( 0.000000000000000000, 0.3999999999999995781, 2.015694669338588429 ) ) ;
#26271 = DIRECTION ( 'NONE',  ( 1.000000000000000000, 0.000000000000000000, 0.000000000000000000 ) ) ;
#26272 = CARTESIAN_POINT ( 'NONE',  ( 29.75043019189810423, 3.055000000000002824, -5.291415217122919401 ) ) ;
#26273 = EDGE_CURVE ( 'NONE', #91335, #44987, #42037, .T. ) ;
#26274 = AXIS2_PLACEMENT_3D ( 'NONE', #119229, #41683, #130864 ) ;
#26275 = ORIENTED_EDGE ( 'NONE', *, *, #131390, .T. ) ;
#26276 = FACE_OUTER_BOUND ( 'NONE', #135873, .T. ) ;
#26277 = ORIENTED_EDGE ( 'NONE', *, *, #95567, .F. ) ;
#26278 = LINE ( 'NONE', #15354, #31136 ) ;
#26279 = DIRECTION ( 'NONE',  ( -4.681814790819591790E-17, -0.3543493200069152693, 0.9351131265310292928 ) ) ;
#26280 = CARTESIAN_POINT ( 'NONE',  ( 19.04500000000000881, 3.130000000000007887, 0.000000000000000000 ) ) ;
#26281 = AXIS2_PLACEMENT_3D ( 'NONE', #29376, #49025, #139620 ) ;
#26282 = CARTESIAN_POINT ( 'NONE',  ( 62.68749999999999289, -5.819803920172573974, 5.819803920172573086 ) ) ;
#26284 = EDGE_CURVE ( 'NONE', #56703, #138242, #41289, .T. ) ;
#26283 = ORIENTED_EDGE ( 'NONE', *, *, #56019, .T. ) ;
#26285 = ORIENTED_EDGE ( 'NONE', *, *, #15370, .F. ) ;
#26286 = PLANE ( 'NONE',  #116468 ) ;
#26287 = ADVANCED_FACE ( 'NONE', ( #61658 ), #75372, .F. ) ;
#26288 = DIRECTION ( 'NONE',  ( -0.7071067811865486830, -0.7071067811865464625, 0.000000000000000000 ) ) ;
#26289 = DIRECTION ( 'NONE',  ( -0.000000000000000000, -0.3543493200069152693, 0.9351131265310292928 ) ) ;
#26290 = VECTOR ( 'NONE', #66447, 1000.000000000000000 ) ;
#26291 = AXIS2_PLACEMENT_3D ( 'NONE', #27973, #128709, #61363 ) ;
#26292 = VECTOR ( 'NONE', #85165, 1000.000000000000227 ) ;
#26293 = CARTESIAN_POINT ( 'NONE',  ( 48.03709685856477307, -3.054999999999998828, -5.291415217122919401 ) ) ;
#26294 = CARTESIAN_POINT ( 'NONE',  ( 123.9375000000000000, 5.819803920172574863, -5.819803920172573086 ) ) ;
#26295 = DIRECTION ( 'NONE',  ( 0.000000000000000000, 0.000000000000000000, 1.000000000000000000 ) ) ;
#26296 = ORIENTED_EDGE ( 'NONE', *, *, #39237, .F. ) ;
#26297 = ORIENTED_EDGE ( 'NONE', *, *, #107346, .F. ) ;
#26298 = AXIS2_PLACEMENT_3D ( 'NONE', #114329, #127343, #80308 ) ;
#26299 = LINE ( 'NONE', #71970, #118687 ) ;
#26300 = VERTEX_POINT ( 'NONE', #29005 ) ;
#26301 = EDGE_CURVE ( 'NONE', #116545, #40105, #8619, .T. ) ;
#26302 =( BOUNDED_CURVE ( )  B_SPLINE_CURVE ( 3, ( #94795, #82530, #73791, #106372 ),
 .UNSPECIFIED., .F., .F. ) 
 B_SPLINE_CURVE_WITH_KNOTS ( ( 4, 4 ),
 ( 5.920967161967926273, 7.341195215986580536 ),
 .UNSPECIFIED. ) 
 CURVE ( )  GEOMETRIC_REPRESENTATION_ITEM ( )  RATIONAL_B_SPLINE_CURVE ( ( 1.000000000000000000, 0.8388583629366737071, 0.8388583629366737071, 1.000000000000000000 ) ) 
 REPRESENTATION_ITEM ( '' )  );
#26303 = DIRECTION ( 'NONE',  ( 0.000000000000000000, -1.000000000000000000, 0.000000000000000000 ) ) ;
#26304 = ORIENTED_EDGE ( 'NONE', *, *, #11695, .T. ) ;
#26305 = FACE_OUTER_BOUND ( 'NONE', #139190, .T. ) ;
#26306 = CARTESIAN_POINT ( 'NONE',  ( 18.18398860626898994, 28.73617430169800002, 5.000000000000000000 ) ) ;
#26307 = AXIS2_PLACEMENT_3D ( 'NONE', #65634, #109801, #55432 ) ;
#26308 = CARTESIAN_POINT ( 'NONE',  ( -33.15612307739218778, -22.22500000000000142, 4.000000000000000000 ) ) ;
#26309 = FACE_BOUND ( 'NONE', #87626, .T. ) ;
#26310 = CARTESIAN_POINT ( 'NONE',  ( -34.92500000000001137, 22.22500000000000142, 4.000000000000000000 ) ) ;
#26311 = CARTESIAN_POINT ( 'NONE',  ( -21.79289321881330110, -8.240707523384198652, 5.000000000000000000 ) ) ;
#26312 = CARTESIAN_POINT ( 'NONE',  ( 2.999999999999984457, 19.55218569542897100, 5.000000000000000000 ) ) ;
#26313 = VECTOR ( 'NONE', #59121, 1000.000000000000000 ) ;
#26314 = DIRECTION ( 'NONE',  ( -0.000000000000000000, 0.000000000000000000, 1.000000000000000000 ) ) ;
#26316 = VERTEX_POINT ( 'NONE', #18821 ) ;
#26315 = LINE ( 'NONE', #4481, #124558 ) ;
#26317 = DIRECTION ( 'NONE',  ( -0.000000000000000000, -0.3543493200069152693, 0.9351131265310292928 ) ) ;
#26318 = VERTEX_POINT ( 'NONE', #51479 ) ;
#26319 = ADVANCED_FACE ( 'NONE', ( #95674 ), #105815, .F. ) ;
#26321 = ORIENTED_EDGE ( 'NONE', *, *, #14387, .F. ) ;
#26320 = ADVANCED_FACE ( 'NONE', ( #94946 ), #73237, .T. ) ;
#26322 = CARTESIAN_POINT ( 'NONE',  ( 63.78709685856477307, 3.054999999999997495, 5.291415217122919401 ) ) ;
#26323 = ORIENTED_EDGE ( 'NONE', *, *, #25250, .F. ) ;
#26324 = LINE ( 'NONE', #69863, #7282 ) ;
#26325 = ADVANCED_FACE ( 'NONE', ( #5785 ), #84808, .F. ) ;
#26326 = CARTESIAN_POINT ( 'NONE',  ( -19.05000000000000071, 3.174999999999997158, 5.000000000000000000 ) ) ;
#26327 = ORIENTED_EDGE ( 'NONE', *, *, #90415, .T. ) ;
#26328 = DIRECTION ( 'NONE',  ( -0.7071067811865486830, -0.7071067811865464625, 0.000000000000000000 ) ) ;
#26329 = ADVANCED_FACE ( 'NONE', ( #64483 ), #10093, .T. ) ;
#26330 = EDGE_CURVE ( 'NONE', #56258, #95511, #33330, .T. ) ;
#26331 = VECTOR ( 'NONE', #65958, 999.9999999999998863 ) ;
#26332 = CARTESIAN_POINT ( 'NONE',  ( 23.67183060077630685, -6.740707523384209310, 4.000000000000000000 ) ) ;
#26333 = LINE ( 'NONE', #138671, #4115 ) ;
#26334 = DIRECTION ( 'NONE',  ( 0.7071067811865487940, 0.7071067811865463515, 0.000000000000000000 ) ) ;
#26335 = CARTESIAN_POINT ( 'NONE',  ( 16.47916666666667140, 6.094999999999988205, -1.633150327867694651 ) ) ;
#26336 = LINE ( 'NONE', #90149, #97195 ) ;
#26337 = EDGE_LOOP ( 'NONE', ( #33210, #70369, #127038, #34689 ) ) ;
#26338 = ORIENTED_EDGE ( 'NONE', *, *, #78247, .F. ) ;
#26339 = ORIENTED_EDGE ( 'NONE', *, *, #134738, .T. ) ;
#26340 = LINE ( 'NONE', #91590, #26543 ) ;
#26341 = ORIENTED_EDGE ( 'NONE', *, *, #1747, .T. ) ;
#26342 = ORIENTED_EDGE ( 'NONE', *, *, #12462, .F. ) ;
#26343 = ORIENTED_EDGE ( 'NONE', *, *, #9227, .T. ) ;
#26344 = ADVANCED_FACE ( 'NONE', ( #99220 ), #23080, .F. ) ;
#26345 = EDGE_CURVE ( 'NONE', #44351, #123046, #44176, .T. ) ;
#26346 = DIRECTION ( 'NONE',  ( 0.7071067811865487940, 0.7071067811865463515, 0.000000000000000000 ) ) ;
#26347 = ORIENTED_EDGE ( 'NONE', *, *, #62331, .T. ) ;
#26348 = CARTESIAN_POINT ( 'NONE',  ( -8.287690060339658160, -21.73547319004781642, 4.999917730833664642 ) ) ;
#26349 = VECTOR ( 'NONE', #7007, 1000.000000000000227 ) ;
#26350 = EDGE_CURVE ( 'NONE', #16457, #398, #142760, .T. ) ;
#26351 = DIRECTION ( 'NONE',  ( 0.6830127018922180770, -0.6830127018922204085, -0.2588190451025213501 ) ) ;
#26352 = CIRCLE ( 'NONE', #63433, 2.247899999999998677 ) ;
#26353 = CARTESIAN_POINT ( 'NONE',  ( 9.108736474768550195, -5.808823158059033709, 5.808823158059035485 ) ) ;
#26354 = CARTESIAN_POINT ( 'NONE',  ( 34.49999999999976552, 0.05432934483094861711, 4.994342998332161443 ) ) ;
#26355 = ORIENTED_EDGE ( 'NONE', *, *, #14967, .F. ) ;
#26356 = LINE ( 'NONE', #70614, #78155 ) ;
#26357 = CARTESIAN_POINT ( 'NONE',  ( 20.99999999999986144, -13.44781430457069149, 5.000000000000000000 ) ) ;
#26358 = LINE ( 'NONE', #59718, #128313 ) ;
#26359 = EDGE_CURVE ( 'NONE', #43634, #11154, #98534, .T. ) ;
#26361 = ORIENTED_EDGE ( 'NONE', *, *, #92566, .T. ) ;
#26360 = DIRECTION ( 'NONE',  ( 0.3543493200069162685, -0.000000000000000000, -0.9351131265310288487 ) ) ;
#26362 = DIRECTION ( 'NONE',  ( -0.7071067811865486830, 0.7071067811865464625, 0.000000000000000000 ) ) ;
#26363 = ORIENTED_EDGE ( 'NONE', *, *, #26688, .T. ) ;
#26364 = LINE ( 'NONE', #72773, #137539 ) ;
#26365 = LINE ( 'NONE', #39391, #74792 ) ;
#26366 = VECTOR ( 'NONE', #27056, 1000.000000000000000 ) ;
#26367 = CARTESIAN_POINT ( 'NONE',  ( -42.48921356237308800, -27.52281430457085065, 5.000000000000000000 ) ) ;
#26368 = ORIENTED_EDGE ( 'NONE', *, *, #49153, .F. ) ;
#26369 = FACE_OUTER_BOUND ( 'NONE', #65871, .T. ) ;
#26370 = CARTESIAN_POINT ( 'NONE',  ( -42.18398860626899705, 28.73617430169816700, 5.000000000000000000 ) ) ;
#26371 = VECTOR ( 'NONE', #84849, 1000.000000000000000 ) ;
#26372 = VECTOR ( 'NONE', #31439, 1000.000000000000000 ) ;
#26373 = FACE_OUTER_BOUND ( 'NONE', #15651, .T. ) ;
#26374 = LINE ( 'NONE', #61871, #41870 ) ;
#26375 = CARTESIAN_POINT ( 'NONE',  ( -29.99999999999979039, 9.631307414974292769, -9.079085613539609412 ) ) ;
#26376 = EDGE_CURVE ( 'NONE', #93689, #140843, #45622, .T. ) ;
#26377 = EDGE_LOOP ( 'NONE', ( #96649, #61699, #41578, #44743 ) ) ;
#26378 = DIRECTION ( 'NONE',  ( -0.3543493200069162685, -0.000000000000000000, -0.9351131265310288487 ) ) ;
#26379 = DIRECTION ( 'NONE',  ( 0.6830127018922181881, 0.6830127018922202975, -0.2588190451025214056 ) ) ;
#26381 = VECTOR ( 'NONE', #50730, 1000.000000000000000 ) ;
#26380 = CARTESIAN_POINT ( 'NONE',  ( -5.999999999999970690, -22.22500000000000142, 4.412002311790005571 ) ) ;
#26382 = CARTESIAN_POINT ( 'NONE',  ( -22.41489890804854568, -1.755427004171023819, 4.190031470807584313 ) ) ;
#26383 = CARTESIAN_POINT ( 'NONE',  ( -23.99999999999982947, -19.22509904557638549, 1.855685503482122023 ) ) ;
#26384 = VECTOR ( 'NONE', #12435, 1000.000000000000227 ) ;
#26385 = EDGE_LOOP ( 'NONE', ( #86912, #119066, #20322, #96573 ) ) ;
#26386 = EDGE_CURVE ( 'NONE', #129048, #73712, #9339, .T. ) ;
#26387 = ORIENTED_EDGE ( 'NONE', *, *, #110151, .T. ) ;
#26388 = DIRECTION ( 'NONE',  ( 0.6830127018922181881, 0.6830127018922202975, -0.2588190451025214056 ) ) ;
#26389 = CARTESIAN_POINT ( 'NONE',  ( -20.99999999999984723, -21.41253812416053748, 4.000000000000000000 ) ) ;
#26390 = AXIS2_PLACEMENT_3D ( 'NONE', #124206, #24885, #100323 ) ;
#26391 = ADVANCED_FACE ( 'NONE', ( #97823 ), #32584, .F. ) ;
#26392 = CARTESIAN_POINT ( 'NONE',  ( 3.041236474768552966, 0.000000000000000000, 7.934999999999990727 ) ) ;
#26393 = PLANE ( 'NONE',  #115336 ) ;
#26394 = VECTOR ( 'NONE', #99986, 999.9999999999998863 ) ;
#26395 = FACE_OUTER_BOUND ( 'NONE', #10304, .T. ) ;
#26396 = DIRECTION ( 'NONE',  ( -1.000000000000000000, 0.000000000000000000, 0.000000000000000000 ) ) ;
#26397 = DIRECTION ( 'NONE',  ( 0.7071067811865486830, -0.7071067811865464625, -0.000000000000000000 ) ) ;
#26398 = ORIENTED_EDGE ( 'NONE', *, *, #123034, .F. ) ;
#26399 = FILL_AREA_STYLE_COLOUR ( '', #136796 ) ;
#26400 = CARTESIAN_POINT ( 'NONE',  ( 24.18398860626899705, 28.73617430169804265, 5.000000000000000000 ) ) ;
#26401 = CIRCLE ( 'NONE', #95820, 0.9999999999999997780 ) ;
#26402 = SURFACE_STYLE_FILL_AREA ( #70648 ) ;
#26403 = CARTESIAN_POINT ( 'NONE',  ( 47.16209685856477307, -5.291415217122919401, 3.054999999999998384 ) ) ;
#26404 = PLANE ( 'NONE',  #134432 ) ;
#26405 = COLOUR_RGB ( '', 0.09019608, 0.27058824, 0.51372549) ;
#26406 = ORIENTED_EDGE ( 'NONE', *, *, #33962, .T. ) ;
#26407 = ORIENTED_EDGE ( 'NONE', *, *, #49458, .T. ) ;
#26408 = DIRECTION ( 'NONE',  ( -0.6830127018922181881, 0.6830127018922202975, -0.2588190451025214056 ) ) ;
#26409 = ORIENTED_EDGE ( 'NONE', *, *, #95288, .T. ) ;
#26410 = VECTOR ( 'NONE', #63663, 1000.000000000000000 ) ;
#26411 = DIRECTION ( 'NONE',  ( 0.7071067811865486830, -0.7071067811865464625, -0.000000000000000000 ) ) ;
#26412 = LINE ( 'NONE', #69209, #43773 ) ;
#26413 = CARTESIAN_POINT ( 'NONE',  ( 5.816011393731002066, 28.73617430169783304, 5.000000000000000000 ) ) ;
#26414 = FACE_OUTER_BOUND ( 'NONE', #40103, .T. ) ;
#26415 = CARTESIAN_POINT ( 'NONE',  ( 6.423278458063501617, 11.25929247661559529, 17.85071094206583098 ) ) ;
#26416 = CARTESIAN_POINT ( 'NONE',  ( 128.8635666761377934, -49.19207878844991200, 41.22112633375493829 ) ) ;
#26417 = ORIENTED_EDGE ( 'NONE', *, *, #73373, .F. ) ;
#26418 = PLANE ( 'NONE',  #81136 ) ;
#26419 = CARTESIAN_POINT ( 'NONE',  ( 21.48921356237309155, -27.52281430457070499, 5.000000000000000000 ) ) ;
#26420 = CARTESIAN_POINT ( 'NONE',  ( -32.99999999999977263, 2.342191155542415970, -5.001666872980010226 ) ) ;
#26421 = FACE_OUTER_BOUND ( 'NONE', #72930, .T. ) ;
#26422 = CARTESIAN_POINT ( 'NONE',  ( 66.57919371712955581, 3.975000000000002753, -6.884901960086283523 ) ) ;
#26423 = VECTOR ( 'NONE', #45636, 1000.000000000000000 ) ;
#26424 = PLANE ( 'NONE',  #6763 ) ;
#26425 = ORIENTED_EDGE ( 'NONE', *, *, #111968, .T. ) ;
#26426 = ORIENTED_EDGE ( 'NONE', *, *, #41238, .T. ) ;
#26427 = CARTESIAN_POINT ( 'NONE',  ( 66.04166666666667140, -3.975000000000002753, 6.884901960086286188 ) ) ;
#26428 = LINE ( 'NONE', #93107, #70220 ) ;
#26429 = DIRECTION ( 'NONE',  ( -0.7071067811865486830, 0.7071067811865464625, 0.000000000000000000 ) ) ;
#26430 = CARTESIAN_POINT ( 'NONE',  ( 13.10362284818588741, 2.655808543615126638, 5.000000000000000000 ) ) ;
#26431 = ORIENTED_EDGE ( 'NONE', *, *, #107056, .T. ) ;
#26432 = VECTOR ( 'NONE', #73406, 999.9999999999998863 ) ;
#26433 = CARTESIAN_POINT ( 'NONE',  ( -30.29974487139158867, -27.71228299555227537, 4.000000000000000000 ) ) ;
#26434 = LINE ( 'NONE', #127905, #141606 ) ;
#26435 = CARTESIAN_POINT ( 'NONE',  ( 58.77126352523142572, 4.472830434245839371, 4.472830434245842035 ) ) ;
#26436 = PLANE ( 'NONE',  #87622 ) ;
#26437 = VERTEX_POINT ( 'NONE', #633 ) ;
#26438 = VERTEX_POINT ( 'NONE', #120992 ) ;
#26439 = LINE ( 'NONE', #88318, #21117 ) ;
#26440 = DIRECTION ( 'NONE',  ( 0.7071067811865487940, 0.7071067811865463515, 0.000000000000000000 ) ) ;
#26441 = LINE ( 'NONE', #25717, #125396 ) ;
#26442 = DIRECTION ( 'NONE',  ( 0.000000000000000000, -1.000000000000000000, 0.000000000000000000 ) ) ;
#26443 = ADVANCED_FACE ( 'NONE', ( #131890 ), #44928, .T. ) ;
#26444 = CARTESIAN_POINT ( 'NONE',  ( -5.671830600776424092, -21.74070752338406010, 4.000000000000000000 ) ) ;
#26446 = ORIENTED_EDGE ( 'NONE', *, *, #38896, .T. ) ;
#26445 = CARTESIAN_POINT ( 'NONE',  ( 85.87500000000000000, 7.950000000000000178, 1.460391307983218535E-15 ) ) ;
#26447 = EDGE_CURVE ( 'NONE', #27246, #126680, #65952, .T. ) ;
#26448 = DIRECTION ( 'NONE',  ( 0.7071067811865486830, -0.7071067811865464625, -0.000000000000000000 ) ) ;
#26449 = DIRECTION ( 'NONE',  ( 0.7071067811865487940, 0.7071067811865463515, 0.000000000000000000 ) ) ;
#26450 = FACE_OUTER_BOUND ( 'NONE', #83181, .T. ) ;
#26451 = VECTOR ( 'NONE', #109936, 1000.000000000000227 ) ;
#26452 = DIRECTION ( 'NONE',  ( -1.000000000000000000, -0.000000000000000000, -0.000000000000000000 ) ) ;
#26453 = ORIENTED_EDGE ( 'NONE', *, *, #133030, .T. ) ;
#26454 = ORIENTED_EDGE ( 'NONE', *, *, #19393, .F. ) ;
#26455 = EDGE_CURVE ( 'NONE', #21745, #6566, #67360, .T. ) ;
#26456 = CARTESIAN_POINT ( 'NONE',  ( 7.998069433178966570, -22.22500000000000142, 4.500000000000000888 ) ) ;
#26457 = VECTOR ( 'NONE', #19973, 999.9999999999998863 ) ;
#26458 = FACE_OUTER_BOUND ( 'NONE', #3102, .T. ) ;
#26459 = CARTESIAN_POINT ( 'NONE',  ( 111.6416937171295842, -2.130196079827424871, -7.949999999999998401 ) ) ;
#26460 = DIRECTION ( 'NONE',  ( -0.000000000000000000, 0.000000000000000000, 1.000000000000000000 ) ) ;
#26461 = ORIENTED_EDGE ( 'NONE', *, *, #83965, .T. ) ;
#26462 = ORIENTED_EDGE ( 'NONE', *, *, #26607, .F. ) ;
#26463 = CARTESIAN_POINT ( 'NONE',  ( -11.14994871458968539, -8.240707523384186217, 17.25253755692236268 ) ) ;
#26464 = LINE ( 'NONE', #70715, #62893 ) ;
#26465 = EDGE_CURVE ( 'NONE', #119913, #97364, #111551, .T. ) ;
#26466 = VERTEX_POINT ( 'NONE', #120244 ) ;
#26467 = AXIS2_PLACEMENT_3D ( 'NONE', #91302, #127459, #70286 ) ;
#26468 = CARTESIAN_POINT ( 'NONE',  ( 34.92499999999998295, 11.07784511950550410, 0.7759263132492005832 ) ) ;
#26469 = VERTEX_POINT ( 'NONE', #12228 ) ;
#26470 = CARTESIAN_POINT ( 'NONE',  ( 15.29177708983037931, -15.74070752338412049, 19.73771281079101314 ) ) ;
#26471 = LINE ( 'NONE', #127196, #98015 ) ;
#26472 = ADVANCED_FACE ( 'NONE', ( #20962 ), #56517, .F. ) ;
#26473 = CIRCLE ( 'NONE', #100577, 2.500000000000000888 ) ;
#26474 = FACE_BOUND ( 'NONE', #14127, .T. ) ;
#26475 = CARTESIAN_POINT ( 'NONE',  ( 48.29974487139158867, -27.71228299555239971, 4.000000000000000000 ) ) ;
#26476 = LINE ( 'NONE', #70727, #44365 ) ;
#26477 = CARTESIAN_POINT ( 'NONE',  ( -33.18398860626899705, 28.73617430169810305, 5.000000000000000000 ) ) ;
#26478 = FACE_OUTER_BOUND ( 'NONE', #101312, .T. ) ;
#26479 =( BOUNDED_CURVE ( )  B_SPLINE_CURVE ( 3, ( #28037, #114319, #103425, #136073 ),
 .UNSPECIFIED., .F., .T. ) 
 B_SPLINE_CURVE_WITH_KNOTS ( ( 4, 4 ),
 ( 4.350170835173023498, 4.500739107949268458 ),
 .UNSPECIFIED. ) 
 CURVE ( )  GEOMETRIC_REPRESENTATION_ITEM ( )  RATIONAL_B_SPLINE_CURVE ( ( 1.000000000000000000, 0.9981116584018941973, 0.9981116584018941973, 1.000000000000000000 ) ) 
 REPRESENTATION_ITEM ( '' )  );
#26480 = VECTOR ( 'NONE', #117934, 1000.000000000000000 ) ;
#26481 = CARTESIAN_POINT ( 'NONE',  ( 7.251592354503322291, -2.500000000000000000, 3.061616997868384127E-16 ) ) ;
#26482 = APPLICATION_PROTOCOL_DEFINITION ( 'draft international standard', 'automotive_design', 1998, #121683 ) ;
#26483 = VERTEX_POINT ( 'NONE', #54359 ) ;
#26484 = AXIS2_PLACEMENT_3D ( 'NONE', #93757, #4527, #48839 ) ;
#26486 = VERTEX_POINT ( 'NONE', #119543 ) ;
#26485 = VECTOR ( 'NONE', #106380, 999.9999999999998863 ) ;
#26487 = CARTESIAN_POINT ( 'NONE',  ( 96.59959685856476597, -6.109999999999997655, -1.637169565754160283 ) ) ;
#26488 = ORIENTED_EDGE ( 'NONE', *, *, #90691, .F. ) ;
#26489 = FACE_OUTER_BOUND ( 'NONE', #99717, .T. ) ;
#26490 = EDGE_CURVE ( 'NONE', #136986, #6450, #20240, .T. ) ;
#26491 = LINE ( 'NONE', #83758, #19145 ) ;
#26492 = EDGE_CURVE ( 'NONE', #106952, #81979, #66638, .T. ) ;
#26493 = ADVANCED_FACE ( 'NONE', ( #123885 ), #47767, .F. ) ;
#26494 = CONICAL_SURFACE ( 'NONE', #63479, 2.552699999999994418, 1.029744258676651869 ) ;
#26495 = CARTESIAN_POINT ( 'NONE',  ( 27.79289321881327268, -2.240707523384252386, 5.000000000000000000 ) ) ;
#26496 = ORIENTED_EDGE ( 'NONE', *, *, #27124, .F. ) ;
#26497 = LINE ( 'NONE', #28655, #140984 ) ;
#26498 = LINE ( 'NONE', #139575, #124226 ) ;
#26499 = CARTESIAN_POINT ( 'NONE',  ( -42.18398860626899705, 28.73617430169816700, 5.000000000000000000 ) ) ;
#26501 = FACE_OUTER_BOUND ( 'NONE', #81657, .T. ) ;
#26500 = DIRECTION ( 'NONE',  ( 0.7071067811865487940, 0.7071067811865463515, -0.000000000000000000 ) ) ;
#26502 = LINE ( 'NONE', #37382, #43847 ) ;
#26503 = LINE ( 'NONE', #16302, #125515 ) ;
#26504 = ORIENTED_EDGE ( 'NONE', *, *, #38426, .T. ) ;
#26505 = EDGE_CURVE ( 'NONE', #123992, #4634, #68104, .T. ) ;
#26506 = CARTESIAN_POINT ( 'NONE',  ( 34.42499999999998295, -1.458600742197942779, 5.000000000000000000 ) ) ;
#26507 = CARTESIAN_POINT ( 'NONE',  ( -57.18398860626899705, 28.73617430169827358, 5.000000000000000000 ) ) ;
#26508 = ORIENTED_EDGE ( 'NONE', *, *, #119460, .F. ) ;
#26509 = ORIENTED_EDGE ( 'NONE', *, *, #114974, .F. ) ;
#26510 = ADVANCED_FACE ( 'NONE', ( #15079 ), #137606, .F. ) ;
#26512 = ORIENTED_EDGE ( 'NONE', *, *, #143247, .T. ) ;
#26511 = EDGE_CURVE ( 'NONE', #103184, #104580, #115082, .T. ) ;
#26513 = CARTESIAN_POINT ( 'NONE',  ( 41.70876352523143993, -7.482591942790329030E-16, 6.110000000000001208 ) ) ;
#26514 = ORIENTED_EDGE ( 'NONE', *, *, #141793, .F. ) ;
#26515 = EDGE_CURVE ( 'NONE', #108363, #141564, #102838, .T. ) ;
#26516 = CARTESIAN_POINT ( 'NONE',  ( 12.87913961620377279, -5.278424836066145431, -3.047499999999993658 ) ) ;
#26517 = CARTESIAN_POINT ( 'NONE',  ( -14.95063623912963635, 4.191486776496043731, -32.28758159997615707 ) ) ;
#26518 = EDGE_CURVE ( 'NONE', #125176, #7159, #134772, .T. ) ;
#26519 = ORIENTED_EDGE ( 'NONE', *, *, #69908, .F. ) ;
#26520 = LINE ( 'NONE', #57747, #57266 ) ;
#26521 = ORIENTED_EDGE ( 'NONE', *, *, #20723, .F. ) ;
#26522 = CARTESIAN_POINT ( 'NONE',  ( 48.18398860626899705, 28.73617430169820608, 5.000000000000000000 ) ) ;
#26523 = DIRECTION ( 'NONE',  ( -0.000000000000000000, 1.000000000000000000, -0.000000000000000000 ) ) ;
#26524 = EDGE_CURVE ( 'NONE', #75364, #84656, #49178, .T. ) ;
#26526 = VERTEX_POINT ( 'NONE', #112287 ) ;
#26525 = LINE ( 'NONE', #80914, #135059 ) ;
#26527 = VERTEX_POINT ( 'NONE', #48440 ) ;
#26528 = VECTOR ( 'NONE', #114564, 999.9999999999998863 ) ;
#26529 = DIRECTION ( 'NONE',  ( -0.6830127018922181881, 0.6830127018922202975, -0.2588190451025214056 ) ) ;
#26530 = FACE_OUTER_BOUND ( 'NONE', #124595, .T. ) ;
#26531 = VERTEX_POINT ( 'NONE', #4883 ) ;
#26532 = DIRECTION ( 'NONE',  ( 0.7071067811865487940, -0.7071067811865463515, 0.000000000000000000 ) ) ;
#26533 = EDGE_LOOP ( 'NONE', ( #48639, #61342, #130404, #65510 ) ) ;
#26534 = ORIENTED_EDGE ( 'NONE', *, *, #65702, .T. ) ;
#26535 = ORIENTED_EDGE ( 'NONE', *, *, #15479, .T. ) ;
#26536 = ORIENTED_EDGE ( 'NONE', *, *, #82912, .F. ) ;
#26537 = CARTESIAN_POINT ( 'NONE',  ( 33.48921356237309510, -27.52281430457078670, 5.000000000000000000 ) ) ;
#26538 = LINE ( 'NONE', #68638, #60769 ) ;
#26539 = PLANE ( 'NONE',  #107498 ) ;
#26540 = LINE ( 'NONE', #117791, #32098 ) ;
#26541 = DIRECTION ( 'NONE',  ( -0.7071067811865486830, -0.7071067811865464625, -0.000000000000000000 ) ) ;
#26542 = ORIENTED_EDGE ( 'NONE', *, *, #106820, .T. ) ;
#26543 = VECTOR ( 'NONE', #4505, 1000.000000000000000 ) ;
#26544 = LINE ( 'NONE', #138167, #3094 ) ;
#26545 = EDGE_CURVE ( 'NONE', #130094, #79859, #81088, .T. ) ;
#26546 = EDGE_CURVE ( 'NONE', #13632, #94354, #69505, .T. ) ;
#26547 = CIRCLE ( 'NONE', #7997, 2.500000000000000888 ) ;
#26548 = CARTESIAN_POINT ( 'NONE',  ( 23.16623647476855652, 7.934999999999990727, -1.457635852685135314E-15 ) ) ;
#26549 = DIRECTION ( 'NONE',  ( 0.000000000000000000, -1.000000000000000000, 0.000000000000000000 ) ) ;
#26550 = DIRECTION ( 'NONE',  ( -0.7071067811865487940, 0.7071067811865463515, 0.000000000000000000 ) ) ;
#26551 = CARTESIAN_POINT ( 'NONE',  ( 31.17183060077625711, -11.24070752338416490, 4.000000000000000000 ) ) ;
#26552 = ORIENTED_EDGE ( 'NONE', *, *, #116552, .T. ) ;
#26553 = AXIS2_PLACEMENT_3D ( 'NONE', #32121, #87925, #45881 ) ;
#26554 = EDGE_LOOP ( 'NONE', ( #41139, #107211, #54506, #113254 ) ) ;
#26555 = ORIENTED_EDGE ( 'NONE', *, *, #82349, .F. ) ;
#26556 = DIRECTION ( 'NONE',  ( 0.7071067811865487940, 0.7071067811865463515, 0.000000000000000000 ) ) ;
#26557 = CARTESIAN_POINT ( 'NONE',  ( 45.18398860626900415, 28.73617430169818832, 5.000000000000000000 ) ) ;
#26558 = FACE_OUTER_BOUND ( 'NONE', #6866, .T. ) ;
#26559 = CARTESIAN_POINT ( 'NONE',  ( -25.39999999999996305, 0.000000000000000000, 0.000000000000000000 ) ) ;
#26560 = EDGE_CURVE ( 'NONE', #139534, #109138, #59906, .T. ) ;
#26561 = FILL_AREA_STYLE_COLOUR ( '', #133829 ) ;
#26562 = CARTESIAN_POINT ( 'NONE',  ( 71.22459685856478018, -1.637169565754161171, 6.109999999999998543 ) ) ;
#26563 = CARTESIAN_POINT ( 'NONE',  ( 74.45419371712955581, 6.884901960086283523, 3.975000000000002753 ) ) ;
#26564 = LINE ( 'NONE', #37454, #57671 ) ;
#26565 = VECTOR ( 'NONE', #84530, 1000.000000000000000 ) ;
#26566 = DIRECTION ( 'NONE',  ( -0.7071067811865486830, -0.7071067811865464625, 0.000000000000000000 ) ) ;
#26567 = DIRECTION ( 'NONE',  ( 0.6830127018922180770, -0.6830127018922204085, -0.2588190451025213501 ) ) ;
#26568 = CARTESIAN_POINT ( 'NONE',  ( 13.27644930412397350, 4.689949953678146599, 5.000000000000000000 ) ) ;
#26569 = ORIENTED_EDGE ( 'NONE', *, *, #105201, .F. ) ;
#26570 = PLANE ( 'NONE',  #80032 ) ;
#26571 = ORIENTED_EDGE ( 'NONE', *, *, #33444, .F. ) ;
#26572 = DIRECTION ( 'NONE',  ( 0.7071067811865486830, -0.7071067811865464625, -0.000000000000000000 ) ) ;
#26574 = VERTEX_POINT ( 'NONE', #136874 ) ;
#26573 = DIRECTION ( 'NONE',  ( 0.000000000000000000, 0.2631995976047524777, 0.9647414015272156584 ) ) ;
#26575 = CARTESIAN_POINT ( 'NONE',  ( -45.18398860626900415, 28.73617430169818832, 5.000000000000000000 ) ) ;
#26576 = CARTESIAN_POINT ( 'NONE',  ( 17.99451991528748351, 28.92564299267950645, 4.000000000000000000 ) ) ;
#26577 = ORIENTED_EDGE ( 'NONE', *, *, #129371, .T. ) ;
#26578 = DIRECTION ( 'NONE',  ( 0.000000000000000000, -1.000000000000000000, 0.000000000000000000 ) ) ;
#26579 = ORIENTED_EDGE ( 'NONE', *, *, #92951, .F. ) ;
#26580 = CARTESIAN_POINT ( 'NONE',  ( 121.5583603837962272, -7.949999999999996625, -2.130196079827426203 ) ) ;
#26581 = ORIENTED_EDGE ( 'NONE', *, *, #143517, .T. ) ;
#26582 = CARTESIAN_POINT ( 'NONE',  ( 19.49999999999986500, -7.420205493532880503, -2.617629953481207750 ) ) ;
#26583 = CONICAL_SURFACE ( 'NONE', #107598, 2.055000000000001048, 0.9599310885968758145 ) ;
#26584 = CARTESIAN_POINT ( 'NONE',  ( 100.7041937171295558, -6.884901960086285300, -3.975000000000000089 ) ) ;
#26586 = AXIS2_PLACEMENT_3D ( 'NONE', #114601, #15269, #59555 ) ;
#26585 = CARTESIAN_POINT ( 'NONE',  ( -21.48921356237309155, -27.52281430457070499, 5.000000000000000000 ) ) ;
#26587 = VECTOR ( 'NONE', #51315, 1000.000000000000227 ) ;
#26588 = CARTESIAN_POINT ( 'NONE',  ( 24.18398860626899705, 28.73617430169804265, 5.000000000000000000 ) ) ;
#26589 = EDGE_LOOP ( 'NONE', ( #67349, #27245, #134217, #75892 ) ) ;
#26590 = AXIS2_PLACEMENT_3D ( 'NONE', #102810, #46316, #112948 ) ;
#26591 = CARTESIAN_POINT ( 'NONE',  ( 21.48921356237309155, -27.52281430457070499, 5.000000000000000000 ) ) ;
#26592 = LINE ( 'NONE', #106072, #130579 ) ;
#26593 = EDGE_CURVE ( 'NONE', #95607, #70988, #113693, .T. ) ;
#26594 = CARTESIAN_POINT ( 'NONE',  ( 30.70710678118633297, 17.25929247661554200, 5.000000000000000000 ) ) ;
#26595 = CARTESIAN_POINT ( 'NONE',  ( 26.39583333333333925, 1.633150327867687324, -6.094999999999991758 ) ) ;
#26596 = FACE_OUTER_BOUND ( 'NONE', #36398, .T. ) ;
#26597 = DIRECTION ( 'NONE',  ( 0.7071067811865487940, 0.7071067811865463515, 0.000000000000000000 ) ) ;
#26598 = VERTEX_POINT ( 'NONE', #114406 ) ;
#26599 = DIRECTION ( 'NONE',  ( -0.3543493200069162685, -0.000000000000000000, -0.9351131265310288487 ) ) ;
#26600 = ORIENTED_EDGE ( 'NONE', *, *, #101106, .F. ) ;
#26601 = CARTESIAN_POINT ( 'NONE',  ( 86.47959685856477563, 6.109999999999999432, 1.637169565754164280 ) ) ;
#26602 = LINE ( 'NONE', #135392, #26924 ) ;
#26603 = CARTESIAN_POINT ( 'NONE',  ( 24.09999999999999787, 9.521314400968980422E-16, 0.000000000000000000 ) ) ;
#26604 = FACE_OUTER_BOUND ( 'NONE', #17881, .T. ) ;
#26605 = ORIENTED_EDGE ( 'NONE', *, *, #96670, .T. ) ;
#26606 = CARTESIAN_POINT ( 'NONE',  ( 57.48921356237308800, -27.52281430457095368, 5.000000000000000000 ) ) ;
#26607 = EDGE_CURVE ( 'NONE', #98525, #36255, #93372, .T. ) ;
#26608 = CARTESIAN_POINT ( 'NONE',  ( 8.306730066903963206, -3.740707523384244837, 12.88036043432865618 ) ) ;
#26609 = FACE_OUTER_BOUND ( 'NONE', #106654, .T. ) ;
#26610 = ADVANCED_FACE ( 'NONE', ( #14384 ), #55187, .T. ) ;
#26611 = LINE ( 'NONE', #124494, #68047 ) ;
#26613 = VERTEX_POINT ( 'NONE', #46342 ) ;
#26612 = DIRECTION ( 'NONE',  ( -0.7071067811865487940, 0.7071067811865463515, 0.000000000000000000 ) ) ;
#26614 = CARTESIAN_POINT ( 'NONE',  ( 29.99999999999980105, -19.06887692260762179, 4.000000000000000000 ) ) ;
#26615 = PLANE ( 'NONE',  #43056 ) ;
#26616 = SURFACE_SIDE_STYLE ('',( #70859 ) ) ;
#26617 = CARTESIAN_POINT ( 'NONE',  ( -23.20710678118638270, -17.24070752338409918, 5.000000000000000000 ) ) ;
#26618 = ADVANCED_FACE ( 'NONE', ( #3480 ), #25982, .F. ) ;
#26620 = ORIENTED_EDGE ( 'NONE', *, *, #132303, .T. ) ;
#26619 = EDGE_CURVE ( 'NONE', #93975, #84503, #81822, .T. ) ;
#26621 = ORIENTED_EDGE ( 'NONE', *, *, #70605, .T. ) ;
#26622 = ORIENTED_EDGE ( 'NONE', *, *, #98178, .T. ) ;
#26623 = CARTESIAN_POINT ( 'NONE',  ( 84.29209685856477563, -5.291415217122921177, 3.054999999999999272 ) ) ;
#26624 = EDGE_LOOP ( 'NONE', ( #9368, #2797, #124159, #131159 ) ) ;
#26625 = ADVANCED_FACE ( 'NONE', ( #90530 ), #35463, .F. ) ;
#26626 = CARTESIAN_POINT ( 'NONE',  ( 17.99999999999987566, 12.25461709320621928, -10.07315571508693175 ) ) ;
#26627 = LINE ( 'NONE', #38931, #80453 ) ;
#26628 = LINE ( 'NONE', #104896, #110476 ) ;
#26629 = DIRECTION ( 'NONE',  ( -0.6830127018922181881, 0.6830127018922202975, -0.2588190451025214056 ) ) ;
#26630 = ORIENTED_EDGE ( 'NONE', *, *, #81250, .F. ) ;
#26631 = CARTESIAN_POINT ( 'NONE',  ( 5.510786437626906675, -27.52281430457051314, 5.000000000000000000 ) ) ;
#26632 = CARTESIAN_POINT ( 'NONE',  ( 57.53752705046289151, -9.735942053221456900E-16, 7.949999999999998401 ) ) ;
#26633 = ADVANCED_FACE ( 'NONE', ( #71634 ), #29694, .T. ) ;
#26634 = CARTESIAN_POINT ( 'NONE',  ( 72.68293019189810877, -1.637169565754158951, -6.109999999999998543 ) ) ;
#26635 = VERTEX_POINT ( 'NONE', #10447 ) ;
#26636 = PLANE ( 'NONE',  #97554 ) ;
#26637 = CARTESIAN_POINT ( 'NONE',  ( -9.005480084712511157, 28.92564299267931816, 4.000000000000000000 ) ) ;
#26638 = DIRECTION ( 'NONE',  ( -0.7071067811865486830, -0.7071067811865464625, -0.000000000000000000 ) ) ;
#26639 = EDGE_CURVE ( 'NONE', #82012, #88219, #64144, .T. ) ;
#26640 = ORIENTED_EDGE ( 'NONE', *, *, #57950, .T. ) ;
#26641 = ORIENTED_EDGE ( 'NONE', *, *, #90268, .F. ) ;
#26642 = CARTESIAN_POINT ( 'NONE',  ( -54.48921356237310221, -27.52281430457093236, 5.000000000000000000 ) ) ;
#26643 = CARTESIAN_POINT ( 'NONE',  ( -57.48921356237308800, -27.52281430457095368, 5.000000000000000000 ) ) ;
#26644 = CARTESIAN_POINT ( 'NONE',  ( -9.299744871391588674, -27.71228299555212971, 4.000000000000000000 ) ) ;
#26645 = EDGE_CURVE ( 'NONE', #61603, #70779, #129249, .T. ) ;
#26646 = PRESENTATION_STYLE_ASSIGNMENT (( #135436 ) ) ;
#26647 = CARTESIAN_POINT ( 'NONE',  ( -34.45011844616454511, -14.99769585840588704, 5.000000000000000888 ) ) ;
#26648 = PLANE ( 'NONE',  #129877 ) ;
#26649 =( NAMED_UNIT ( * ) SI_UNIT ( $, .STERADIAN. ) SOLID_ANGLE_UNIT ( ) );
#26650 = VECTOR ( 'NONE', #125216, 1000.000000000000000 ) ;
#26651 = EDGE_LOOP ( 'NONE', ( #125863, #47279, #36656, #65357, #127384, #138879 ) ) ;
#26652 = ORIENTED_EDGE ( 'NONE', *, *, #119415, .F. ) ;
#26653 = PRESENTATION_LAYER_ASSIGNMENT (  '', '', ( #96072 ) ) ;
#26654 = CARTESIAN_POINT ( 'NONE',  ( -28.49999999999980105, 10.08746187583914988, 4.000000000000000000 ) ) ;
#26655 = EDGE_LOOP ( 'NONE', ( #101686, #43074, #100856, #75227 ) ) ;
#26656 = EDGE_CURVE ( 'NONE', #52412, #57071, #142428, .T. ) ;
#26657 = CARTESIAN_POINT ( 'NONE',  ( -0.2997448713915885632, -27.71228299555206220, 4.000000000000000000 ) ) ;
#26658 = EDGE_CURVE ( 'NONE', #70384, #71407, #109777, .T. ) ;
#26659 = CARTESIAN_POINT ( 'NONE',  ( -24.29974487139158867, -27.71228299555223273, 4.000000000000000000 ) ) ;
#26660 = VERTEX_POINT ( 'NONE', #141710 ) ;
#26661 = CIRCLE ( 'NONE', #40550, 1.898649999999994842 ) ;
#26662 = DIRECTION ( 'NONE',  ( 0.000000000000000000, 1.000000000000000000, -0.000000000000000000 ) ) ;
#26663 = PLANE ( 'NONE',  #139768 ) ;
#26664 = EDGE_CURVE ( 'NONE', #27623, #136020, #64866, .T. ) ;
#26665 = CARTESIAN_POINT ( 'NONE',  ( -34.92500000000001137, 17.81665438641024579, 4.500000000000000888 ) ) ;
#26666 = PLANE ( 'NONE',  #28235 ) ;
#26667 = ORIENTED_EDGE ( 'NONE', *, *, #54325, .T. ) ;
#26668 = EDGE_CURVE ( 'NONE', #34776, #26933, #9736, .T. ) ;
#26669 = CARTESIAN_POINT ( 'NONE',  ( 0.000000000000000000, 0.000000000000000000, 5.000000000000000000 ) ) ;
#26670 = PLANE ( 'NONE',  #134492 ) ;
#26671 = VERTEX_POINT ( 'NONE', #74315 ) ;
#26672 = LINE ( 'NONE', #51298, #13296 ) ;
#26673 = ORIENTED_EDGE ( 'NONE', *, *, #93291, .F. ) ;
#26674 = ORIENTED_EDGE ( 'NONE', *, *, #78642, .F. ) ;
#26675 = FACE_OUTER_BOUND ( 'NONE', #115994, .T. ) ;
#26676 = ORIENTED_EDGE ( 'NONE', *, *, #34925, .T. ) ;
#26677 = EDGE_LOOP ( 'NONE', ( #123293, #19191, #34772, #26765, #5871 ) ) ;
#26678 = CARTESIAN_POINT ( 'NONE',  ( 75.97959685856477563, 6.109999999999999432, 1.637169565754164280 ) ) ;
#26679 = ORIENTED_EDGE ( 'NONE', *, *, #119579, .T. ) ;
#26680 = MECHANICAL_DESIGN_GEOMETRIC_PRESENTATION_REPRESENTATION (  '', ( #10518 ), #33644 ) ;
#26681 = CYLINDRICAL_SURFACE ( 'NONE', #134536, 3.000000000000000000 ) ;
#26682 = VECTOR ( 'NONE', #104046, 1000.000000000000000 ) ;
#26683 = VECTOR ( 'NONE', #33165, 1000.000000000000000 ) ;
#26684 = CYLINDRICAL_SURFACE ( 'NONE', #72698, 2.500000000000000444 ) ;
#26685 = CARTESIAN_POINT ( 'NONE',  ( 107.9170968585647756, 3.054999999999998828, 5.291415217122922066 ) ) ;
#26686 = LINE ( 'NONE', #83957, #91116 ) ;
#26687 = AXIS2_PLACEMENT_3D ( 'NONE', #73527, #98129, #62649 ) ;
#26688 = EDGE_CURVE ( 'NONE', #138855, #115521, #18449, .T. ) ;
#26689 = DIRECTION ( 'NONE',  ( 1.000000000000000000, 1.224606353822377258E-16, 0.000000000000000000 ) ) ;
#26691 = CARTESIAN_POINT ( 'NONE',  ( 17.22560490425083657, 2.499999999999998224, 3.061616997868380183E-16 ) ) ;
#26690 = DIRECTION ( 'NONE',  ( 1.000000000000000000, 0.000000000000000000, 0.000000000000000000 ) ) ;
#26692 = PLANE ( 'NONE',  #88026 ) ;
#26693 = ADVANCED_FACE ( 'NONE', ( #21348 ), #51848, .F. ) ;
#26694 = PLANE ( 'NONE',  #90958 ) ;
#26695 = CARTESIAN_POINT ( 'NONE',  ( -2.000000000000000000, -2.375000000000000000, 1.069999999999998508 ) ) ;
#26696 = DIRECTION ( 'NONE',  ( -0.000000000000000000, -1.000000000000000000, -0.000000000000000000 ) ) ;
#26697 = VERTEX_POINT ( 'NONE', #119907 ) ;
#26698 = DIRECTION ( 'NONE',  ( 0.6830127018922181881, 0.6830127018922202975, -0.2588190451025214056 ) ) ;
#26699 = DIRECTION ( 'NONE',  ( -0.7071067811865486830, -0.7071067811865464625, 0.000000000000000000 ) ) ;
#26700 = ORIENTED_EDGE ( 'NONE', *, *, #79862, .F. ) ;
#26701 = EDGE_LOOP ( 'NONE', ( #100008, #16552, #128053, #87826 ) ) ;
#26702 = LINE ( 'NONE', #25263, #79641 ) ;
#26703 = ORIENTED_EDGE ( 'NONE', *, *, #96171, .T. ) ;
#26704 = CARTESIAN_POINT ( 'NONE',  ( -0.4892135623730947680, -27.52281430457055578, 5.000000000000000000 ) ) ;
#26705 = CARTESIAN_POINT ( 'NONE',  ( 113.0000000000000000, 0.000000000000000000, -7.950000000000000178 ) ) ;
#26706 = LINE ( 'NONE', #59369, #5 ) ;
#26707 = DIRECTION ( 'NONE',  ( 1.301042606982605074E-16, -1.000000000000000000, 0.000000000000000000 ) ) ;
#26708 = VERTEX_POINT ( 'NONE', #96036 ) ;
#26709 = CARTESIAN_POINT ( 'NONE',  ( 45.29974487139158867, -27.71228299555237840, 4.000000000000000000 ) ) ;
#26710 = EDGE_LOOP ( 'NONE', ( #136361, #88038, #67651, #139676 ) ) ;
#26711 = CARTESIAN_POINT ( 'NONE',  ( -11.24139925780195171, 21.72500000000000142, 5.000000000000000000 ) ) ;
#26712 = CARTESIAN_POINT ( 'NONE',  ( 24.85873647476855908, 5.808823158059031044, -5.808823158059038150 ) ) ;
#26713 = CARTESIAN_POINT ( 'NONE',  ( 12.18398860626900060, 28.73617430169795739, 5.000000000000000000 ) ) ;
#26714 = CARTESIAN_POINT ( 'NONE',  ( -27.29974487139158512, -27.71228299555225405, 4.000000000000000000 ) ) ;
#26715 = CARTESIAN_POINT ( 'NONE',  ( 13.22094965600862970, -8.914091344047001542, 3.291399616463569267 ) ) ;
#26716 = ORIENTED_EDGE ( 'NONE', *, *, #133281, .T. ) ;
#26717 = ORIENTED_EDGE ( 'NONE', *, *, #31581, .T. ) ;
#26718 = ORIENTED_EDGE ( 'NONE', *, *, #13230, .T. ) ;
#26719 = CARTESIAN_POINT ( 'NONE',  ( -34.92190055902135271, 21.78725130426367684, 4.173570450635298634 ) ) ;
#26720 = DIRECTION ( 'NONE',  ( 0.7071067811865486830, -0.7071067811865464625, -0.000000000000000000 ) ) ;
#26721 = CARTESIAN_POINT ( 'NONE',  ( 5.700255128608413102, -27.71228299555201957, 4.000000000000000000 ) ) ;
#26722 = PLANE ( 'NONE',  #51938 ) ;
#26724 = EDGE_CURVE ( 'NONE', #119189, #35816, #32226, .T. ) ;
#26723 = ORIENTED_EDGE ( 'NONE', *, *, #62050, .T. ) ;
#26725 = DIRECTION ( 'NONE',  ( 0.7071067811865487940, -0.7071067811865463515, 0.000000000000000000 ) ) ;
#26726 = LINE ( 'NONE', #128200, #61926 ) ;
#26727 = DIRECTION ( 'NONE',  ( 0.7071067811865486830, -0.7071067811865464625, -0.000000000000000000 ) ) ;
#26728 = CARTESIAN_POINT ( 'NONE',  ( 51.18398860626899705, 28.73617430169823095, 5.000000000000000000 ) ) ;
#26729 = CARTESIAN_POINT ( 'NONE',  ( 33.79289321881323360, -14.24070752338413648, 5.000000000000000000 ) ) ;
#26730 = VERTEX_POINT ( 'NONE', #75734 ) ;
#26731 = CARTESIAN_POINT ( 'NONE',  ( 73.47916666666665719, -7.950000000000000178, 2.130196079827424427 ) ) ;
#26732 = LINE ( 'NONE', #73123, #26224 ) ;
#26733 = VERTEX_POINT ( 'NONE', #75045 ) ;
#26734 =( BOUNDED_CURVE ( )  B_SPLINE_CURVE ( 3, ( #344, #77257, #133058, #78653 ),
 .UNSPECIFIED., .F., .F. ) 
 B_SPLINE_CURVE_WITH_KNOTS ( ( 4, 4 ),
 ( 1.208578181583235267, 1.359146454359428269 ),
 .UNSPECIFIED. ) 
 CURVE ( )  GEOMETRIC_REPRESENTATION_ITEM ( )  RATIONAL_B_SPLINE_CURVE ( ( 1.000000000000000000, 0.9981116584018955296, 0.9981116584018955296, 1.000000000000000000 ) ) 
 REPRESENTATION_ITEM ( '' )  );
#26735 = DIRECTION ( 'NONE',  ( -0.5735764363510503783, -0.8191520442889886899, 0.000000000000000000 ) ) ;
#26737 = ORIENTED_EDGE ( 'NONE', *, *, #70300, .F. ) ;
#26736 = CARTESIAN_POINT ( 'NONE',  ( 59.37656097284387613, -44.54322672568201114, -35.04755940938199643 ) ) ;
#26738 = EDGE_LOOP ( 'NONE', ( #63267, #95274, #106220, #77347 ) ) ;
#26739 = LINE ( 'NONE', #105698, #137172 ) ;
#26740 = CARTESIAN_POINT ( 'NONE',  ( 18.18398860626898994, 28.73617430169800002, 5.000000000000000000 ) ) ;
#26741 = LINE ( 'NONE', #16559, #34548 ) ;
#26742 = EDGE_LOOP ( 'NONE', ( #86435, #78249, #96890, #60013, #105443 ) ) ;
#26743 = FACE_OUTER_BOUND ( 'NONE', #20955, .T. ) ;
#26744 = EDGE_LOOP ( 'NONE', ( #107444, #28205, #50023, #68837, #44312, #41450 ) ) ;
#26745 = DIRECTION ( 'NONE',  ( -0.7071067811865486830, -0.7071067811865464625, 0.000000000000000000 ) ) ;
#26746 = CARTESIAN_POINT ( 'NONE',  ( -48.18398860626899705, 28.73617430169820608, 5.000000000000000000 ) ) ;
#26747 = AXIS2_PLACEMENT_3D ( 'NONE', #20716, #141818, #100441 ) ;
#26748 = CARTESIAN_POINT ( 'NONE',  ( 30.09959685856478018, -6.109999999999998543, -1.637169565754160727 ) ) ;
#26749 = FACE_OUTER_BOUND ( 'NONE', #71331, .T. ) ;
#26750 = FACE_OUTER_BOUND ( 'NONE', #51842, .T. ) ;
#26751 = VECTOR ( 'NONE', #109175, 1000.000000000000000 ) ;
#26752 = PLANE ( 'NONE',  #46844 ) ;
#26753 = LINE ( 'NONE', #49255, #68000 ) ;
#26754 = DIRECTION ( 'NONE',  ( -1.000000000000000000, -1.224606353822377258E-16, -0.000000000000000000 ) ) ;
#26755 = CARTESIAN_POINT ( 'NONE',  ( 26.95790314143522437, 6.871911579029515771, 3.967499999999989146 ) ) ;
#26756 = CARTESIAN_POINT ( 'NONE',  ( 10.77040314143521904, -7.934999999999988951, 2.126176841940957907 ) ) ;
#26757 = CARTESIAN_POINT ( 'NONE',  ( 15.35830628287044064, -1.633150327867690210, 6.094999999999989981 ) ) ;
#26758 = CARTESIAN_POINT ( 'NONE',  ( 28.82816939922332011, 3.759292476615674783, 4.000000000000000000 ) ) ;
#26759 = LINE ( 'NONE', #113041, #1410 ) ;
#26760 = ORIENTED_EDGE ( 'NONE', *, *, #24964, .T. ) ;
#26761 = ORIENTED_EDGE ( 'NONE', *, *, #65974, .T. ) ;
#26762 = CARTESIAN_POINT ( 'NONE',  ( 90.25000000000000000, -9.735942053221458872E-16, 7.950000000000000178 ) ) ;
#26763 = ORIENTED_EDGE ( 'NONE', *, *, #49739, .F. ) ;
#26764 = VECTOR ( 'NONE', #55657, 1000.000000000000000 ) ;
#26765 = ORIENTED_EDGE ( 'NONE', *, *, #43820, .T. ) ;
#26766 = EDGE_CURVE ( 'NONE', #139864, #132371, #109047, .T. ) ;
#26767 = DIRECTION ( 'NONE',  ( -0.000000000000000000, -0.3543493200069152693, 0.9351131265310292928 ) ) ;
#26768 = CARTESIAN_POINT ( 'NONE',  ( 60.29974487139158867, -27.71228299555248142, 4.000000000000000000 ) ) ;
#26769 = CARTESIAN_POINT ( 'NONE',  ( 33.18398860626899705, 28.73617430169810305, 5.000000000000000000 ) ) ;
#26770 = VERTEX_POINT ( 'NONE', #30819 ) ;
#26771 = CARTESIAN_POINT ( 'NONE',  ( 54.18398860626899705, 28.73617430169825226, 5.000000000000000000 ) ) ;
#26772 = FACE_OUTER_BOUND ( 'NONE', #42421, .T. ) ;
#26773 = CARTESIAN_POINT ( 'NONE',  ( -30.48921356237309510, -27.52281430457076894, 5.000000000000000000 ) ) ;
#26774 = CARTESIAN_POINT ( 'NONE',  ( 126.0262699974396838, 4.592503512758394635, -5.848864093691881649 ) ) ;
#26775 = ADVANCED_FACE ( 'NONE', ( #19204 ), #115792, .T. ) ;
#26776 = EDGE_CURVE ( 'NONE', #140063, #51562, #120332, .T. ) ;
#26777 = CARTESIAN_POINT ( 'NONE',  ( 0.000000000000000000, 0.000000000000000000, 5.000000000000000000 ) ) ;
#26778 = CARTESIAN_POINT ( 'NONE',  ( 2.924914550060625285, 4.584330080086930965E-16, 0.000000000000000000 ) ) ;
#26779 = SURFACE_STYLE_USAGE ( .BOTH. , #28220 ) ;
#26780 = DIRECTION ( 'NONE',  ( -1.000000000000000000, -0.000000000000000000, -0.000000000000000000 ) ) ;
#26781 = DIRECTION ( 'NONE',  ( -0.000000000000000000, 0.3543493200069153248, 0.9351131265310292928 ) ) ;
#26782 = LINE ( 'NONE', #71032, #6246 ) ;
#26783 = FACE_OUTER_BOUND ( 'NONE', #71848, .T. ) ;
#26784 = VECTOR ( 'NONE', #120009, 1000.000000000000000 ) ;
#26785 = CARTESIAN_POINT ( 'NONE',  ( 12.71159235450332048, 2.500000000000001776, 0.000000000000000000 ) ) ;
#26786 = EDGE_CURVE ( 'NONE', #55968, #66284, #128494, .T. ) ;
#26787 = EDGE_CURVE ( 'NONE', #23165, #50701, #124225, .T. ) ;
#26788 = VERTEX_POINT ( 'NONE', #99593 ) ;
#26789 = ORIENTED_EDGE ( 'NONE', *, *, #22690, .T. ) ;
#26790 = VECTOR ( 'NONE', #73172, 1000.000000000000000 ) ;
#26791 = CARTESIAN_POINT ( 'NONE',  ( 107.3337635252314470, 6.110000000000001208, 1.122388791418549305E-15 ) ) ;
#26792 = ORIENTED_EDGE ( 'NONE', *, *, #85085, .T. ) ;
#26793 = AXIS2_PLACEMENT_3D ( 'NONE', #100700, #36164, #1346 ) ;
#26794 = EDGE_CURVE ( 'NONE', #12163, #5176, #34368, .T. ) ;
#26796 = EDGE_CURVE ( 'NONE', #25077, #86768, #46729, .T. ) ;
#26795 = VECTOR ( 'NONE', #88268, 1000.000000000000000 ) ;
#26797 = LINE ( 'NONE', #135582, #131092 ) ;
#26798 = ORIENTED_EDGE ( 'NONE', *, *, #11382, .F. ) ;
#26799 = LINE ( 'NONE', #24652, #137020 ) ;
#26800 = CARTESIAN_POINT ( 'NONE',  ( -42.48921356237308800, -27.52281430457085065, 5.000000000000000000 ) ) ;
#26801 = EDGE_CURVE ( 'NONE', #32049, #2079, #24901, .T. ) ;
#26802 = CARTESIAN_POINT ( 'NONE',  ( 103.8912635252314516, -4.472830434245839371, -4.472830434245839371 ) ) ;
#26803 = VERTEX_POINT ( 'NONE', #88033 ) ;
#26804 = ORIENTED_EDGE ( 'NONE', *, *, #66937, .F. ) ;
#26805 = CARTESIAN_POINT ( 'NONE',  ( 57.18398860626899705, 28.73617430169827358, 5.000000000000000000 ) ) ;
#26806 = CARTESIAN_POINT ( 'NONE',  ( -24.66331758004193375, 1.142935889642021863, 4.329525704382053419 ) ) ;
#26807 = ADVANCED_FACE ( 'NONE', ( #13295 ), #101755, .F. ) ;
#26808 = VERTEX_POINT ( 'NONE', #56159 ) ;
#26809 = ORIENTED_EDGE ( 'NONE', *, *, #109435, .F. ) ;
#26810 = ORIENTED_EDGE ( 'NONE', *, *, #76425, .F. ) ;
#26811 = CARTESIAN_POINT ( 'NONE',  ( 9.983736474768551972, -5.808823158059035485, -5.808823158059033709 ) ) ;
#26812 = ADVANCED_FACE ( 'NONE', ( #113330 ), #14012, .F. ) ;
#26813 = PLANE ( 'NONE',  #64138 ) ;
#26814 = PRESENTATION_STYLE_ASSIGNMENT (( #66947 ) ) ;
#26815 = CARTESIAN_POINT ( 'NONE',  ( 22.53999999999999915, 9.521314400968980422E-16, 0.000000000000000000 ) ) ;
#26816 = ORIENTED_EDGE ( 'NONE', *, *, #135980, .F. ) ;
#26817 = VERTEX_POINT ( 'NONE', #143121 ) ;
#26818 = DIRECTION ( 'NONE',  ( -0.3543493200069162685, -0.000000000000000000, -0.9351131265310288487 ) ) ;
#26819 = ORIENTED_EDGE ( 'NONE', *, *, #44118, .T. ) ;
#26820 = ORIENTED_EDGE ( 'NONE', *, *, #31283, .F. ) ;
#26821 = EDGE_CURVE ( 'NONE', #41198, #33680, #43815, .T. ) ;
#26822 = DIRECTION ( 'NONE',  ( -0.000000000000000000, -0.000000000000000000, 1.000000000000000000 ) ) ;
#26823 = EDGE_CURVE ( 'NONE', #62376, #35148, #24208, .T. ) ;
#26824 = FACE_OUTER_BOUND ( 'NONE', #51193, .T. ) ;
#26825 = ORIENTED_EDGE ( 'NONE', *, *, #142710, .F. ) ;
#26826 = LINE ( 'NONE', #94921, #20525 ) ;
#26827 = EDGE_CURVE ( 'NONE', #99786, #68141, #143294, .T. ) ;
#26828 = DIRECTION ( 'NONE',  ( 0.6830127018922180770, -0.6830127018922204085, -0.2588190451025213501 ) ) ;
#26829 = LINE ( 'NONE', #124017, #103929 ) ;
#26830 = EDGE_CURVE ( 'NONE', #24642, #50272, #122798, .T. ) ;
#26831 = EDGE_CURVE ( 'NONE', #136190, #75148, #121357, .T. ) ;
#26832 = CARTESIAN_POINT ( 'NONE',  ( 24.18398860626899705, 28.73617430169804265, 5.000000000000000000 ) ) ;
#26833 = FACE_BOUND ( 'NONE', #90542, .T. ) ;
#26834 = VERTEX_POINT ( 'NONE', #77874 ) ;
#26835 = CARTESIAN_POINT ( 'NONE',  ( 63.51669371712956291, 7.950000000000000178, -2.130196079827421318 ) ) ;
#26836 = DIRECTION ( 'NONE',  ( -0.000000000000000000, -0.3543493200069152693, 0.9351131265310292928 ) ) ;
#26837 = DIRECTION ( 'NONE',  ( 0.7071067811865487940, 0.7071067811865463515, -0.000000000000000000 ) ) ;
#26838 = ORIENTED_EDGE ( 'NONE', *, *, #68388, .T. ) ;
#26839 = DIRECTION ( 'NONE',  ( 0.7071067811865487940, 0.7071067811865463515, -0.000000000000000000 ) ) ;
#26840 = EDGE_LOOP ( 'NONE', ( #66712, #21123, #82028, #46953, #133082, #126199 ) ) ;
#26841 = ORIENTED_EDGE ( 'NONE', *, *, #19138, .F. ) ;
#26842 = EDGE_LOOP ( 'NONE', ( #57581, #124651, #17644, #16651 ) ) ;
#26843 = CIRCLE ( 'NONE', #82439, 28.00000000000002487 ) ;
#26844 = CARTESIAN_POINT ( 'NONE',  ( 35.78709685856478018, 3.054999999999997495, 5.291415217122919401 ) ) ;
#26845 = VERTEX_POINT ( 'NONE', #11870 ) ;
#26846 = CARTESIAN_POINT ( 'NONE',  ( 7.408407645496676963, 2.500000000000002220, 3.061616997868384620E-16 ) ) ;
#26847 = VECTOR ( 'NONE', #63403, 1000.000000000000000 ) ;
#26848 = CARTESIAN_POINT ( 'NONE',  ( 42.29974487139158157, -27.71228299555235708, 4.000000000000000000 ) ) ;
#26849 = LINE ( 'NONE', #129015, #114472 ) ;
#26850 = EDGE_CURVE ( 'NONE', #29147, #19199, #994, .T. ) ;
#26851 = EDGE_LOOP ( 'NONE', ( #66549, #14049, #90546, #45496 ) ) ;
#26852 = SURFACE_STYLE_FILL_AREA ( #38456 ) ;
#26853 = CARTESIAN_POINT ( 'NONE',  ( 0.7307956238753654521, 3.821174125832445049E-16, 0.000000000000000000 ) ) ;
#26854 = LINE ( 'NONE', #103673, #118659 ) ;
#26855 = DIRECTION ( 'NONE',  ( -0.7071067811865486830, -0.7071067811865464625, 0.000000000000000000 ) ) ;
#26856 = CARTESIAN_POINT ( 'NONE',  ( 52.26932219902325727, -49.14999999999999147, 40.92499999999998295 ) ) ;
#26858 = EDGE_CURVE ( 'NONE', #38224, #65695, #23480, .T. ) ;
#26857 = LINE ( 'NONE', #71110, #115412 ) ;
#26859 = PLANE ( 'NONE',  #17017 ) ;
#26860 =( GEOMETRIC_REPRESENTATION_CONTEXT ( 3 ) GLOBAL_UNCERTAINTY_ASSIGNED_CONTEXT ( ( #36211 ) ) GLOBAL_UNIT_ASSIGNED_CONTEXT ( ( #137323, #136578, #14810 ) ) REPRESENTATION_CONTEXT ( 'NONE', 'WORKASPACE' ) );
#26861 = ORIENTED_EDGE ( 'NONE', *, *, #140373, .T. ) ;
#26862 = ORIENTED_EDGE ( 'NONE', *, *, #128865, .F. ) ;
#26863 = EDGE_LOOP ( 'NONE', ( #111763, #100415, #110102, #87794, #33703, #39684 ) ) ;
#26864 = ORIENTED_EDGE ( 'NONE', *, *, #69656, .F. ) ;
#26865 = FILL_AREA_STYLE ('',( #4327 ) ) ;
#26866 = ORIENTED_EDGE ( 'NONE', *, *, #121312, .F. ) ;
#26867 = ORIENTED_EDGE ( 'NONE', *, *, #130276, .F. ) ;
#26868 = CARTESIAN_POINT ( 'NONE',  ( -21.00548008471250938, 28.92564299267923644, 4.000000000000000000 ) ) ;
#26869 = CARTESIAN_POINT ( 'NONE',  ( -26.20710678118635428, -14.24070752338413470, 5.000000000000000000 ) ) ;
#26870 = ADVANCED_FACE ( 'NONE', ( #111938 ), #68457, .F. ) ;
#26871 = CARTESIAN_POINT ( 'NONE',  ( -42.18398860626899705, 28.73617430169816700, 5.000000000000000000 ) ) ;
#26872 = VERTEX_POINT ( 'NONE', #90160 ) ;
#26873 = DIRECTION ( 'NONE',  ( -1.000000000000000000, -0.000000000000000000, -0.000000000000000000 ) ) ;
#26874 = VERTEX_POINT ( 'NONE', #134407 ) ;
#26875 = AXIS2_PLACEMENT_3D ( 'NONE', #69252, #14123, #15524 ) ;
#26876 = CARTESIAN_POINT ( 'NONE',  ( 25.39999999999999858, 1.399999999999987699, -20.40202195861970580 ) ) ;
#26877 = ADVANCED_FACE ( 'NONE', ( #35105 ), #123545, .T. ) ;
#26878 = DIRECTION ( 'NONE',  ( -0.000000000000000000, 0.3543493200069153248, 0.9351131265310292928 ) ) ;
#26879 = VECTOR ( 'NONE', #103118, 999.9999999999998863 ) ;
#26880 = CARTESIAN_POINT ( 'NONE',  ( -0.6620968585647807325, -6.871911579029513106, -3.967499999999993587 ) ) ;
#26881 = EDGE_LOOP ( 'NONE', ( #74389, #124238, #35248, #68453 ) ) ;
#26883 = LINE ( 'NONE', #104433, #112476 ) ;
#26882 = CARTESIAN_POINT ( 'NONE',  ( 98.20376352523145158, 6.109999999999999432, 1.122388791418549108E-15 ) ) ;
#26884 = VECTOR ( 'NONE', #34114, 999.9999999999998863 ) ;
#26885 = CARTESIAN_POINT ( 'NONE',  ( 55.47138350052868105, -49.14501756083436135, -40.36361034346621324 ) ) ;
#26886 = LINE ( 'NONE', #138515, #99788 ) ;
#26887 = ORIENTED_EDGE ( 'NONE', *, *, #41052, .F. ) ;
#26888 = VERTEX_POINT ( 'NONE', #14747 ) ;
#26889 = CARTESIAN_POINT ( 'NONE',  ( 51.18398860626899705, 28.73617430169823095, 5.000000000000000000 ) ) ;
#26890 = ORIENTED_EDGE ( 'NONE', *, *, #77740, .T. ) ;
#26891 = CARTESIAN_POINT ( 'NONE',  ( 5.848407645496676466, 9.139736423841732040E-16, 0.000000000000000000 ) ) ;
#26892 = CARTESIAN_POINT ( 'NONE',  ( -2.292986735706930457, -21.74070752338405299, 4.999753212805217117 ) ) ;
#26893 = CIRCLE ( 'NONE', #124178, 1.000000000000000000 ) ;
#26894 = CARTESIAN_POINT ( 'NONE',  ( -32.99999999999976552, 17.58746187583906462, 4.000000000000000000 ) ) ;
#26895 = FACE_OUTER_BOUND ( 'NONE', #4936, .T. ) ;
#26896 = FACE_OUTER_BOUND ( 'NONE', #82955, .T. ) ;
#26897 = CARTESIAN_POINT ( 'NONE',  ( 183.6687791239651517, -49.11951764991120939, -40.13200514437819066 ) ) ;
#26899 = EDGE_CURVE ( 'NONE', #100056, #76924, #127071, .T. ) ;
#26898 = ORIENTED_EDGE ( 'NONE', *, *, #34872, .T. ) ;
#26900 = LINE ( 'NONE', #7254, #34416 ) ;
#26901 = EDGE_CURVE ( 'NONE', #122655, #119924, #111136, .T. ) ;
#26902 = LINE ( 'NONE', #60274, #134604 ) ;
#26903 = CARTESIAN_POINT ( 'NONE',  ( -15.29974487139158867, -27.71228299555216879, 4.000000000000000000 ) ) ;
#26904 = VERTEX_POINT ( 'NONE', #50249 ) ;
#26905 = CARTESIAN_POINT ( 'NONE',  ( 5.994519915287488843, 28.92564299267942118, 4.000000000000000000 ) ) ;
#26906 = DIRECTION ( 'NONE',  ( 0.7071067811865487940, 0.7071067811865463515, -0.000000000000000000 ) ) ;
#26907 = ORIENTED_EDGE ( 'NONE', *, *, #34068, .F. ) ;
#26909 = EDGE_LOOP ( 'NONE', ( #38254, #5721, #132158, #130865 ) ) ;
#26908 = DIRECTION ( 'NONE',  ( -0.6830127018922180770, -0.6830127018922202975, -0.2588190451025213501 ) ) ;
#26910 = EDGE_CURVE ( 'NONE', #91471, #99307, #127815, .T. ) ;
#26911 = ORIENTED_EDGE ( 'NONE', *, *, #83712, .T. ) ;
#26912 = CARTESIAN_POINT ( 'NONE',  ( 0.4878811198072842137, 13.74641354151631134, -24.36756908848417780 ) ) ;
#26913 = CARTESIAN_POINT ( 'NONE',  ( 0.000000000000000000, -4.870000000000014317, -10.00000000000000178 ) ) ;
#26914 = ORIENTED_EDGE ( 'NONE', *, *, #46115, .F. ) ;
#26915 = LINE ( 'NONE', #17456, #113667 ) ;
#26916 = DIRECTION ( 'NONE',  ( 0.000000000000000000, 5.559056632600921604E-15, -1.000000000000000000 ) ) ;
#26917 = FILL_AREA_STYLE ('',( #115309 ) ) ;
#26918 = ORIENTED_EDGE ( 'NONE', *, *, #27761, .F. ) ;
#26919 = LINE ( 'NONE', #98939, #50813 ) ;
#26920 = CARTESIAN_POINT ( 'NONE',  ( 22.22840764549667725, -3.851859888774471706E-31, 2.500000000000001332 ) ) ;
#26921 = DIRECTION ( 'NONE',  ( 0.7071067811865486830, -0.7071067811865464625, -0.000000000000000000 ) ) ;
#26922 = PRESENTATION_STYLE_ASSIGNMENT (( #82749 ) ) ;
#26924 = VECTOR ( 'NONE', #3393, 1000.000000000000000 ) ;
#26923 = DIRECTION ( 'NONE',  ( -0.000000000000000000, 0.3543493200069153248, 0.9351131265310292928 ) ) ;
#26925 = FACE_OUTER_BOUND ( 'NONE', #6271, .T. ) ;
#26926 = CARTESIAN_POINT ( 'NONE',  ( -34.92500000000001137, 4.701930566820959001, 4.500000000000000888 ) ) ;
#26927 =( NAMED_UNIT ( * ) SI_UNIT ( $, .STERADIAN. ) SOLID_ANGLE_UNIT ( ) );
#26928 = ORIENTED_EDGE ( 'NONE', *, *, #52021, .T. ) ;
#26929 = EDGE_LOOP ( 'NONE', ( #76494, #119941, #131558, #46333 ) ) ;
#26930 = EDGE_LOOP ( 'NONE', ( #134686, #138763, #19684, #13476, #34313, #25700 ) ) ;
#26931 = CARTESIAN_POINT ( 'NONE',  ( 124.5208333333333428, 7.949999999999999289, 2.130196079827431532 ) ) ;
#26932 = ORIENTED_EDGE ( 'NONE', *, *, #27303, .F. ) ;
#26933 = VERTEX_POINT ( 'NONE', #137257 ) ;
#26934 = ORIENTED_EDGE ( 'NONE', *, *, #39987, .T. ) ;
#26935 = CIRCLE ( 'NONE', #8469, 0.5000000000000004441 ) ;
#26936 = SURFACE_STYLE_FILL_AREA ( #105211 ) ;
#26937 = LINE ( 'NONE', #28384, #104150 ) ;
#26938 = ORIENTED_EDGE ( 'NONE', *, *, #131035, .F. ) ;
#26939 = CARTESIAN_POINT ( 'NONE',  ( 10.49999999999993427, 1.466399257802251999, 5.000000000000000000 ) ) ;
#26940 = DIRECTION ( 'NONE',  ( 0.000000000000000000, 1.000000000000000000, 0.000000000000000000 ) ) ;
#26941 = LINE ( 'NONE', #3041, #65151 ) ;
#26942 = CARTESIAN_POINT ( 'NONE',  ( 108.5004301918981184, -3.055000000000002380, 5.291415217122920289 ) ) ;
#26943 = ORIENTED_EDGE ( 'NONE', *, *, #45322, .F. ) ;
#26944 = EDGE_CURVE ( 'NONE', #84629, #115093, #62544, .T. ) ;
#26945 = CARTESIAN_POINT ( 'NONE',  ( -14.48042995505719510, 4.924559884198918880, -31.94719639125090538 ) ) ;
#26946 = CARTESIAN_POINT ( 'NONE',  ( 106.5375270504628844, -9.735942053221456900E-16, 7.949999999999998401 ) ) ;
#26947 = CARTESIAN_POINT ( 'NONE',  ( 14.99999999999989519, -8.731860332648830436, -2.120594902707502616 ) ) ;
#26948 = DIRECTION ( 'NONE',  ( 0.7071067811865486830, -0.7071067811865464625, -0.000000000000000000 ) ) ;
#26949 = FACE_OUTER_BOUND ( 'NONE', #134091, .T. ) ;
#26950 = CARTESIAN_POINT ( 'NONE',  ( 8.292893218813400580, 5.259292476615665457, 5.000000000000000000 ) ) ;
#26951 = CARTESIAN_POINT ( 'NONE',  ( 39.45419371712956291, 6.884901960086283523, 3.975000000000002753 ) ) ;
#26952 = CIRCLE ( 'NONE', #73231, 6.349999999999997868 ) ;
#26953 = DIRECTION ( 'NONE',  ( -0.6830127018922181881, 0.6830127018922202975, -0.2588190451025214056 ) ) ;
#26954 = ADVANCED_FACE ( 'NONE', ( #83603 ), #135820, .T. ) ;
#26955 = ORIENTED_EDGE ( 'NONE', *, *, #104183, .F. ) ;
#26956 = ORIENTED_EDGE ( 'NONE', *, *, #97633, .T. ) ;
#26957 = CARTESIAN_POINT ( 'NONE',  ( 39.79166666666665719, 3.975000000000003642, -6.884901960086285300 ) ) ;
#26958 = EDGE_CURVE ( 'NONE', #17934, #86656, #71293, .T. ) ;
#26959 = EDGE_LOOP ( 'NONE', ( #63870, #104094, #48901, #6639 ) ) ;
#26960 = ORIENTED_EDGE ( 'NONE', *, *, #5057, .F. ) ;
#26961 = CARTESIAN_POINT ( 'NONE',  ( -34.17183060077623225, 6.759292476615649470, 4.000000000000000000 ) ) ;
#26962 = ADVANCED_FACE ( 'NONE', ( #72026 ), #104609, .F. ) ;
#26963 = LINE ( 'NONE', #29809, #142728 ) ;
#26964 = VERTEX_POINT ( 'NONE', #17583 ) ;
#26965 = EDGE_CURVE ( 'NONE', #30975, #68687, #27047, .T. ) ;
#26966 = DIRECTION ( 'NONE',  ( 0.7071067811865487940, 0.7071067811865463515, -0.000000000000000000 ) ) ;
#26967 = SURFACE_STYLE_USAGE ( .BOTH. , #116111 ) ;
#26968 = CARTESIAN_POINT ( 'NONE',  ( -13.99806943317891772, -22.22500000000000142, 4.500000000000000888 ) ) ;
#26969 = CARTESIAN_POINT ( 'NONE',  ( 30.47959685856476852, 6.109999999999999432, 1.637169565754164280 ) ) ;
#26972 = EDGE_CURVE ( 'NONE', #79253, #14518, #5273, .T. ) ;
#26971 = ORIENTED_EDGE ( 'NONE', *, *, #73533, .F. ) ;
#26970 = AXIS2_PLACEMENT_3D ( 'NONE', #51991, #104926, #17883 ) ;
#26973 = CARTESIAN_POINT ( 'NONE',  ( -12.48921356237309155, -27.52281430457064104, 5.000000000000000000 ) ) ;
#26974 = ORIENTED_EDGE ( 'NONE', *, *, #94830, .F. ) ;
#26975 = DIRECTION ( 'NONE',  ( 0.3543493200069162685, -0.000000000000000000, -0.9351131265310288487 ) ) ;
#26976 = CARTESIAN_POINT ( 'NONE',  ( -25.49999999999981881, 0.05218569542917578241, 5.000000000000000000 ) ) ;
#26977 = LINE ( 'NONE', #5202, #46798 ) ;
#26978 = EDGE_CURVE ( 'NONE', #118900, #133790, #126358, .T. ) ;
#26979 = CARTESIAN_POINT ( 'NONE',  ( 48.48921356237309510, -27.52281430457089328, 5.000000000000000000 ) ) ;
#26980 = ORIENTED_EDGE ( 'NONE', *, *, #83909, .T. ) ;
#26981 = VECTOR ( 'NONE', #66412, 1000.000000000000000 ) ;
#26982 = EDGE_CURVE ( 'NONE', #63812, #111783, #3820, .T. ) ;
#26983 = ORIENTED_EDGE ( 'NONE', *, *, #39718, .T. ) ;
#26984 = FACE_OUTER_BOUND ( 'NONE', #96100, .T. ) ;
#26985 = CARTESIAN_POINT ( 'NONE',  ( 5.821832416544749478, 22.22500000000000142, -10.44049799921112687 ) ) ;
#26986 = CARTESIAN_POINT ( 'NONE',  ( 12.48921356237309155, -27.52281430457064104, 5.000000000000000000 ) ) ;
#26987 = LINE ( 'NONE', #35041, #99578 ) ;
#26988 = EDGE_CURVE ( 'NONE', #138243, #13156, #48107, .T. ) ;
#26989 = CIRCLE ( 'NONE', #80315, 2.500000000000000888 ) ;
#26990 = CIRCLE ( 'NONE', #103333, 1.249999999999969802 ) ;
#26991 = VECTOR ( 'NONE', #87785, 1000.000000000000000 ) ;
#26992 = CARTESIAN_POINT ( 'NONE',  ( 48.32876352523145158, 0.000000000000000000, -6.109999999999998543 ) ) ;
#26993 = VERTEX_POINT ( 'NONE', #92290 ) ;
#26994 = LINE ( 'NONE', #124883, #85936 ) ;
#26995 = DIRECTION ( 'NONE',  ( 1.000000000000000000, -0.000000000000000000, 0.000000000000000000 ) ) ;
#26996 = VERTEX_POINT ( 'NONE', #136514 ) ;
#26997 = ORIENTED_EDGE ( 'NONE', *, *, #46857, .T. ) ;
#26998 = VECTOR ( 'NONE', #50654, 1000.000000000000000 ) ;
#26999 = CARTESIAN_POINT ( 'NONE',  ( 12.48921356237309155, -27.52281430457064104, 5.000000000000000000 ) ) ;
#27000 = VERTEX_POINT ( 'NONE', #61168 ) ;
#27001 = DIRECTION ( 'NONE',  ( -0.7071067811865486830, -0.7071067811865464625, -0.000000000000000000 ) ) ;
#27002 = VERTEX_POINT ( 'NONE', #59705 ) ;
#27003 = CARTESIAN_POINT ( 'NONE',  ( 28.49999999999979750, 15.43112307739202649, 4.000000000000000000 ) ) ;
#27004 = EDGE_CURVE ( 'NONE', #94256, #109940, #137971, .T. ) ;
#27005 = CARTESIAN_POINT ( 'NONE',  ( -30.48921356237309510, -27.52281430457076894, 5.000000000000000000 ) ) ;
#27006 = FILL_AREA_STYLE_COLOUR ( '', #109026 ) ;
#27007 = FACE_BOUND ( 'NONE', #66167, .T. ) ;
#27008 = DIRECTION ( 'NONE',  ( -0.000000000000000000, 0.3543493200069153248, 0.9351131265310292928 ) ) ;
#27009 = FACE_OUTER_BOUND ( 'NONE', #120235, .T. ) ;
#27010 = DIRECTION ( 'NONE',  ( 0.7071067811865487940, 0.7071067811865463515, 0.000000000000000000 ) ) ;
#27011 = ORIENTED_EDGE ( 'NONE', *, *, #64744, .T. ) ;
#27012 = CARTESIAN_POINT ( 'NONE',  ( 13.49999999999991829, 16.08746187583907883, 4.000000000000000000 ) ) ;
#27014 = ORIENTED_EDGE ( 'NONE', *, *, #58594, .F. ) ;
#27013 = DIRECTION ( 'NONE',  ( 0.000000000000000000, -3.469446951953615372E-15, 1.000000000000000000 ) ) ;
#27015 = CARTESIAN_POINT ( 'NONE',  ( -39.18398860626899705, 28.73617430169814568, 5.000000000000000000 ) ) ;
#27016 = EDGE_CURVE ( 'NONE', #120012, #14271, #74738, .T. ) ;
#27017 = VERTEX_POINT ( 'NONE', #38650 ) ;
#27018 = ORIENTED_EDGE ( 'NONE', *, *, #86896, .F. ) ;
#27019 = CARTESIAN_POINT ( 'NONE',  ( 62.47459685856478018, 1.637169565754164280, -6.109999999999996767 ) ) ;
#27020 = EDGE_LOOP ( 'NONE', ( #32429, #16460, #67252, #94353, #13800, #10745 ) ) ;
#27021 = DIRECTION ( 'NONE',  ( 4.681814790819592407E-17, 0.3543493200069153248, 0.9351131265310292928 ) ) ;
#27022 = CARTESIAN_POINT ( 'NONE',  ( 0.000000000000000000, 9.735942053221458872E-16, -7.950000000000000178 ) ) ;
#27023 = EDGE_CURVE ( 'NONE', #15277, #53474, #59093, .T. ) ;
#27024 = ORIENTED_EDGE ( 'NONE', *, *, #128606, .F. ) ;
#27025 = FACE_OUTER_BOUND ( 'NONE', #136346, .T. ) ;
#27026 = AXIS2_PLACEMENT_3D ( 'NONE', #103617, #126802, #136989 ) ;
#27027 = DIRECTION ( 'NONE',  ( -0.7071067811865486830, -0.7071067811865464625, 0.000000000000000000 ) ) ;
#27028 = EDGE_CURVE ( 'NONE', #142647, #67143, #93025, .T. ) ;
#27029 = DIRECTION ( 'NONE',  ( 1.000000000000000000, 0.000000000000000000, 0.000000000000000000 ) ) ;
#27030 = CARTESIAN_POINT ( 'NONE',  ( 11.99999999999991296, -22.22500000000000853, 4.412002311790018894 ) ) ;
#27031 = CARTESIAN_POINT ( 'NONE',  ( 6.489213562373093325, -27.52281430457059841, 5.000000000000000000 ) ) ;
#27032 = CARTESIAN_POINT ( 'NONE',  ( -78.29974487139158157, -27.71228299555260577, 4.000000000000000000 ) ) ;
#27033 = ORIENTED_EDGE ( 'NONE', *, *, #12222, .T. ) ;
#27034 = VECTOR ( 'NONE', #65485, 1000.000000000000227 ) ;
#27035 = ORIENTED_EDGE ( 'NONE', *, *, #55103, .T. ) ;
#27036 = FACE_OUTER_BOUND ( 'NONE', #126254, .T. ) ;
#27037 = FACE_OUTER_BOUND ( 'NONE', #2917, .T. ) ;
#27038 = VERTEX_POINT ( 'NONE', #86449 ) ;
#27039 = ORIENTED_EDGE ( 'NONE', *, *, #12647, .T. ) ;
#27040 = ORIENTED_EDGE ( 'NONE', *, *, #24484, .F. ) ;
#27041 = DIRECTION ( 'NONE',  ( 1.000000000000000000, 0.000000000000000000, 0.000000000000000000 ) ) ;
#27042 = CARTESIAN_POINT ( 'NONE',  ( 54.76669371712954870, -7.949999999999998401, 2.130196079827423983 ) ) ;
#27043 = AXIS2_PLACEMENT_3D ( 'NONE', #41264, #17379, #85475 ) ;
#27044 = ADVANCED_FACE ( 'NONE', ( #118327 ), #62554, .F. ) ;
#27045 = CARTESIAN_POINT ( 'NONE',  ( 28.99999999999999645, 0.000000000000000000, -7.950000000000000178 ) ) ;
#27046 = ORIENTED_EDGE ( 'NONE', *, *, #74309, .T. ) ;
#27047 = LINE ( 'NONE', #114748, #118055 ) ;
#27048 = AXIS2_PLACEMENT_3D ( 'NONE', #131345, #118305, #140770 ) ;
#27049 = CARTESIAN_POINT ( 'NONE',  ( 42.51669371712955581, 7.950000000000000178, -2.130196079827421318 ) ) ;
#27050 = CARTESIAN_POINT ( 'NONE',  ( 6.046236474768552860, -7.934999999999990727, 4.858786175617117713E-16 ) ) ;
#27051 = DIRECTION ( 'NONE',  ( 0.7071067811865486830, -0.7071067811865464625, -0.000000000000000000 ) ) ;
#27052 = ORIENTED_EDGE ( 'NONE', *, *, #35015, .T. ) ;
#27053 = CIRCLE ( 'NONE', #119650, 0.5000000000000004441 ) ;
#27054 = LINE ( 'NONE', #50257, #118320 ) ;
#27055 = CARTESIAN_POINT ( 'NONE',  ( 24.93750000000000000, -4.461849672132299105, 4.461849672132299993 ) ) ;
#27057 = ORIENTED_EDGE ( 'NONE', *, *, #20748, .T. ) ;
#27056 = DIRECTION ( 'NONE',  ( -0.7071067811865486830, -0.7071067811865464625, 0.000000000000000000 ) ) ;
#27058 = CARTESIAN_POINT ( 'NONE',  ( 10.25413961620377457, 3.047499999999993214, -5.278424836066146320 ) ) ;
#27059 = VERTEX_POINT ( 'NONE', #107458 ) ;
#27060 = CARTESIAN_POINT ( 'NONE',  ( 35.99451991528749772, 28.92564299267963079, 4.000000000000000000 ) ) ;
#27061 = CARTESIAN_POINT ( 'NONE',  ( -6.489213562373093325, -27.52281430457059841, 5.000000000000000000 ) ) ;
#27062 = PLANE ( 'NONE',  #72567 ) ;
#27063 = ORIENTED_EDGE ( 'NONE', *, *, #98081, .F. ) ;
#27064 = LINE ( 'NONE', #117435, #13480 ) ;
#27065 = ADVANCED_FACE ( 'NONE', ( #139421 ), #142262, .T. ) ;
#27066 = CARTESIAN_POINT ( 'NONE',  ( 27.22000000000000242, 9.521314400968980422E-16, 0.000000000000000000 ) ) ;
#27067 = CARTESIAN_POINT ( 'NONE',  ( 125.3739199777178754, -1.810106405121186368, 7.950000000000005507 ) ) ;
#27068 = DIRECTION ( 'NONE',  ( 0.7071067811865487940, 0.7071067811865463515, 0.000000000000000000 ) ) ;
#27069 = ORIENTED_EDGE ( 'NONE', *, *, #84374, .T. ) ;
#27070 = CARTESIAN_POINT ( 'NONE',  ( 0.000000000000000000, 0.000000000000000000, 5.000000000000000000 ) ) ;
#27071 = LINE ( 'NONE', #71316, #141982 ) ;
#27072 = CARTESIAN_POINT ( 'NONE',  ( 20.75413961620377279, 3.047499999999993214, -5.278424836066146320 ) ) ;
#27073 = FACE_OUTER_BOUND ( 'NONE', #44443, .T. ) ;
#27074 = VECTOR ( 'NONE', #46301, 1000.000000000000000 ) ;
#27075 = SURFACE_STYLE_USAGE ( .BOTH. , #93772 ) ;
#27076 = ORIENTED_EDGE ( 'NONE', *, *, #37001, .T. ) ;
#27077 = EDGE_CURVE ( 'NONE', #42201, #7059, #119737, .T. ) ;
#27078 = VERTEX_POINT ( 'NONE', #29890 ) ;
#27079 = LINE ( 'NONE', #136548, #54142 ) ;
#27080 = LINE ( 'NONE', #106044, #6549 ) ;
#27081 = VECTOR ( 'NONE', #122930, 999.9999999999998863 ) ;
#27082 = VECTOR ( 'NONE', #140568, 1000.000000000000227 ) ;
#27083 = CARTESIAN_POINT ( 'NONE',  ( 0.7079031414352194851, -6.871911579029513106, -3.967499999999993587 ) ) ;
#27084 = CARTESIAN_POINT ( 'NONE',  ( 34.92499999999998295, -0.1586646689214626926, -3.482007288379075582 ) ) ;
#27085 = AXIS2_PLACEMENT_3D ( 'NONE', #31431, #71551, #49095 ) ;
#27086 = DIRECTION ( 'NONE',  ( -0.3543493200069162685, -0.000000000000000000, -0.9351131265310288487 ) ) ;
#27087 = LINE ( 'NONE', #27805, #80712 ) ;
#27088 = PLANE ( 'NONE',  #21357 ) ;
#27089 = ORIENTED_EDGE ( 'NONE', *, *, #54485, .F. ) ;
#27090 = LINE ( 'NONE', #93072, #18693 ) ;
#27091 = VECTOR ( 'NONE', #40534, 1000.000000000000000 ) ;
#27092 = CARTESIAN_POINT ( 'NONE',  ( -3.183988606268992161, 28.73617430169789699, 5.000000000000000000 ) ) ;
#27093 = AXIS2_PLACEMENT_3D ( 'NONE', #117679, #51769, #140877 ) ;
#27094 = CARTESIAN_POINT ( 'NONE',  ( -72.18398860626899705, 28.73617430169837661, 5.000000000000000000 ) ) ;
#27095 = CARTESIAN_POINT ( 'NONE',  ( 49.93293019189810167, 1.637169565754156730, 6.110000000000001208 ) ) ;
#27096 = ADVANCED_FACE ( 'NONE', ( #74134 ), #40110, .F. ) ;
#27097 = CARTESIAN_POINT ( 'NONE',  ( -6.489213562373093325, -27.52281430457059841, 5.000000000000000000 ) ) ;
#27098 = EDGE_LOOP ( 'NONE', ( #78878, #19768, #78182, #32617 ) ) ;
#27099 = FILL_AREA_STYLE ('',( #14071 ) ) ;
#27100 = VERTEX_POINT ( 'NONE', #40796 ) ;
#27101 = ORIENTED_EDGE ( 'NONE', *, *, #130577, .T. ) ;
#27102 = LINE ( 'NONE', #138740, #140357 ) ;
#27103 = CARTESIAN_POINT ( 'NONE',  ( 27.18398860626900060, 28.73617430169806042, 5.000000000000000000 ) ) ;
#27104 = CARTESIAN_POINT ( 'NONE',  ( -17.99999999999986855, -16.02097659208072145, -11.96015758381204286 ) ) ;
#27105 = DIRECTION ( 'NONE',  ( 0.7071067811865487940, 0.7071067811865463515, 0.000000000000000000 ) ) ;
#27106 = CARTESIAN_POINT ( 'NONE',  ( 0.1161069444170889225, -0.4000000000000003553, 2.220360628129160130 ) ) ;
#27107 = CARTESIAN_POINT ( 'NONE',  ( 128.6956467655707854, -52.10358567239623540, 40.45860062937848767 ) ) ;
#27108 = ORIENTED_EDGE ( 'NONE', *, *, #140260, .F. ) ;
#27109 = CARTESIAN_POINT ( 'NONE',  ( -27.70898713287128956, 22.22500000000000142, 7.734417024081176706 ) ) ;
#27110 = DIRECTION ( 'NONE',  ( 0.7071067811865486830, -0.7071067811865464625, -0.000000000000000000 ) ) ;
#27111 = UNCERTAINTY_MEASURE_WITH_UNIT (LENGTH_MEASURE( 1.000000000000000082E-05 ), #49107, 'distance_accuracy_value', 'NONE');
#27112 = VECTOR ( 'NONE', #3310, 1000.000000000000000 ) ;
#27113 = CARTESIAN_POINT ( 'NONE',  ( -34.49999999999976552, -14.94567065516890558, 4.994342998332162331 ) ) ;
#27114 = DIRECTION ( 'NONE',  ( 0.3543493200069162685, -0.000000000000000000, -0.9351131265310288487 ) ) ;
#27115 = CARTESIAN_POINT ( 'NONE',  ( 7.637717201596474048, 3.061616997868383634E-16, -2.500000000000000444 ) ) ;
#27116 = CARTESIAN_POINT ( 'NONE',  ( 63.37086038379622011, 6.884901960086289741, -3.974999999999993427 ) ) ;
#27117 = EDGE_CURVE ( 'NONE', #75508, #104180, #29188, .T. ) ;
#27118 = VECTOR ( 'NONE', #48208, 1000.000000000000000 ) ;
#27119 = FACE_OUTER_BOUND ( 'NONE', #127849, .T. ) ;
#27120 = VERTEX_POINT ( 'NONE', #85696 ) ;
#27121 = VERTEX_POINT ( 'NONE', #73429 ) ;
#27122 = CARTESIAN_POINT ( 'NONE',  ( 63.12500000000000000, -7.950000000000000178, -4.867971026610729436E-16 ) ) ;
#27123 = FACE_OUTER_BOUND ( 'NONE', #117085, .T. ) ;
#27124 = EDGE_CURVE ( 'NONE', #63599, #22463, #32050, .T. ) ;
#27125 = FACE_OUTER_BOUND ( 'NONE', #78405, .T. ) ;
#27126 = DIRECTION ( 'NONE',  ( -0.7071067811865486830, -0.7071067811865464625, -0.000000000000000000 ) ) ;
#27127 = EDGE_CURVE ( 'NONE', #32567, #36781, #108860, .T. ) ;
#27128 = VECTOR ( 'NONE', #77912, 1000.000000000000000 ) ;
#27129 = EDGE_LOOP ( 'NONE', ( #31397, #79534, #21667, #69449 ) ) ;
#27130 = EDGE_CURVE ( 'NONE', #98666, #40296, #106731, .T. ) ;
#27131 =( BOUNDED_SURFACE ( )  B_SPLINE_SURFACE ( 3, 2, ( 
 ( #135519, #123226, #68159 ),
 ( #2835, #112332, #47129 ),
 ( #47817, #59403, #26736 ),
 ( #115134, #12984, #57261 ),
 ( #134823, #35519, #79751 ),
 ( #91313, #36202, #80431 ),
 ( #124623, #25298, #69564 ),
 ( #82552, #129609, #63679 ),
 ( #96242, #117988, #62967 ),
 ( #83268, #7820, #118735 ),
 ( #93427, #60847, #41175 ),
 ( #85385, #39788, #28173 ),
 ( #84014, #94119, #19428 ),
 ( #72435, #61547, #18691 ),
 ( #140484, #138360, #107839 ),
 ( #38336, #8504, #107144 ) ),
 .UNSPECIFIED., .F., .F., .F. ) 
 B_SPLINE_SURFACE_WITH_KNOTS ( ( 4, 2, 2, 2, 2, 2, 2, 4 ),
 ( 3, 3 ),
 ( 4.712388980384689674, 5.060738160973319744, 5.234912751267634334, 5.409087341561949813, 5.583261931856265292, 5.757436522150579883, 5.931611112444894474, 6.105785702739209952 ),
 ( 0.000000000000000000, 1.000000000000000000 ),
 .UNSPECIFIED. ) 
 GEOMETRIC_REPRESENTATION_ITEM ( )  RATIONAL_B_SPLINE_SURFACE ( (
 ( 1.000000000000000000, 1.000000000000000000, 1.000000000000000000),
 ( 1.000000000000000000, 1.000097732991066080, 1.000000000000000000),
 ( 1.000000000000000000, 0.9896287210066593287, 1.000000000000000000),
 ( 1.000000000000000000, 0.9608359430471657969, 1.000000000000000000),
 ( 1.000000000000000000, 0.9490805577171574914, 1.000000000000000000),
 ( 1.000000000000000000, 0.9222453908327415961, 1.000000000000000000),
 ( 1.000000000000000000, 0.9071649184813681543, 1.000000000000000000),
 ( 1.000000000000000000, 0.8751006588766465644, 1.000000000000000000),
 ( 1.000000000000000000, 0.8581174656085591712, 1.000000000000000000),
 ( 1.000000000000000000, 0.8241077986061765559, 1.000000000000000000),
 ( 1.000000000000000000, 0.8070860741947217809, 1.000000000000000000),
 ( 1.000000000000000000, 0.7752313834060545750, 1.000000000000000000),
 ( 1.000000000000000000, 0.7604116155351108297, 1.000000000000000000),
 ( 1.000000000000000000, 0.7353122387368615787, 1.000000000000000000),
 ( 1.000000000000000000, 0.7250426641248349791, 1.000000000000000000),
 ( 1.000000000000000000, 0.7180326832784534874, 1.000000000000000000) ) ) 
 REPRESENTATION_ITEM ( '' )  SURFACE ( )  );
#27132 = DIRECTION ( 'NONE',  ( 0.7071067811865487940, 0.7071067811865463515, -0.000000000000000000 ) ) ;
#27133 = DIRECTION ( 'NONE',  ( -0.5735764363510501562, 0.8191520442889890230, 1.003171929053521419E-16 ) ) ;
#27134 = CARTESIAN_POINT ( 'NONE',  ( 54.97959685856476852, 6.109999999999999432, 1.637169565754164280 ) ) ;
#27135 = VECTOR ( 'NONE', #7850, 1000.000000000000000 ) ;
#27136 = CARTESIAN_POINT ( 'NONE',  ( -26.99451991528749417, 28.92564299267956685, 4.000000000000000000 ) ) ;
#27137 = VERTEX_POINT ( 'NONE', #131367 ) ;
#27138 = VERTEX_POINT ( 'NONE', #76284 ) ;
#27139 = DIRECTION ( 'NONE',  ( -0.6830127018922181881, 0.6830127018922202975, -0.2588190451025214056 ) ) ;
#27140 = DIRECTION ( 'NONE',  ( 0.6830127018922180770, -0.6830127018922204085, -0.2588190451025213501 ) ) ;
#27141 = FACE_OUTER_BOUND ( 'NONE', #104491, .T. ) ;
#27142 = EDGE_CURVE ( 'NONE', #20400, #47125, #19735, .T. ) ;
#27143 = DIRECTION ( 'NONE',  ( -0.6830127018922180770, -0.6830127018922204085, -0.2588190451025213501 ) ) ;
#27144 = EDGE_CURVE ( 'NONE', #35648, #63600, #95869, .T. ) ;
#27145 = DIRECTION ( 'NONE',  ( 0.7071067811865487940, -0.7071067811865463515, 0.000000000000000000 ) ) ;
#27147 = ORIENTED_EDGE ( 'NONE', *, *, #137345, .F. ) ;
#27146 = CARTESIAN_POINT ( 'NONE',  ( -16.78948154309660268, -0.07126238382044708386, -34.10854881514017478 ) ) ;
#27148 = LINE ( 'NONE', #106108, #110896 ) ;
#27149 = FACE_OUTER_BOUND ( 'NONE', #36811, .T. ) ;
#27150 = DIRECTION ( 'NONE',  ( -0.7071067811865486830, -0.7071067811865464625, 0.000000000000000000 ) ) ;
#27151 = CARTESIAN_POINT ( 'NONE',  ( 44.99451991528749772, 28.92564299267969474, 4.000000000000000000 ) ) ;
#27152 = EDGE_CURVE ( 'NONE', #39448, #72881, #120438, .T. ) ;
#27153 = VERTEX_POINT ( 'NONE', #129204 ) ;
#27154 = ORIENTED_EDGE ( 'NONE', *, *, #17351, .F. ) ;
#27155 = PRESENTATION_LAYER_ASSIGNMENT (  '', '', ( #3930 ) ) ;
#27156 = DIRECTION ( 'NONE',  ( 1.000000000000000000, 0.000000000000000000, 0.000000000000000000 ) ) ;
#27157 = PLANE ( 'NONE',  #126521 ) ;
#27158 = FILL_AREA_STYLE ('',( #82288 ) ) ;
#27159 = EDGE_LOOP ( 'NONE', ( #57738, #126429, #112627, #95023 ) ) ;
#27161 = EDGE_CURVE ( 'NONE', #25602, #49545, #96551, .T. ) ;
#27160 = ORIENTED_EDGE ( 'NONE', *, *, #114345, .F. ) ;
#27162 = CARTESIAN_POINT ( 'NONE',  ( 123.5000000000000000, 0.000000000000000000, -7.950000000000000178 ) ) ;
#27163 = CARTESIAN_POINT ( 'NONE',  ( -1.228506771386643770, 20.25929247661551003, 7.808871592221766633 ) ) ;
#27164 = VERTEX_POINT ( 'NONE', #9554 ) ;
#27165 = ORIENTED_EDGE ( 'NONE', *, *, #129738, .F. ) ;
#27166 = CARTESIAN_POINT ( 'NONE',  ( -17.20710678118642178, -8.240707523384195099, 5.000000000000000000 ) ) ;
#27167 = ORIENTED_EDGE ( 'NONE', *, *, #47160, .T. ) ;
#27168 = CARTESIAN_POINT ( 'NONE',  ( 0.000000000000000000, 0.000000000000000000, 5.000000000000000000 ) ) ;
#27169 = EDGE_CURVE ( 'NONE', #126557, #15065, #95155, .T. ) ;
#27170 = FACE_OUTER_BOUND ( 'NONE', #4690, .T. ) ;
#27171 = MECHANICAL_DESIGN_GEOMETRIC_PRESENTATION_REPRESENTATION (  '', ( #89683 ), #124455 ) ;
#27172 = FACE_BOUND ( 'NONE', #61531, .T. ) ;
#27173 = CARTESIAN_POINT ( 'NONE',  ( 63.48921356237309510, -27.52281430457099631, 5.000000000000000000 ) ) ;
#27174 = CARTESIAN_POINT ( 'NONE',  ( -21.18398860626899349, 28.73617430169802134, 5.000000000000000000 ) ) ;
#27175 = LINE ( 'NONE', #71420, #73740 ) ;
#27176 = LINE ( 'NONE', #84452, #103727 ) ;
#27177 = AXIS2_PLACEMENT_3D ( 'NONE', #143443, #118841, #85483 ) ;
#27178 = CIRCLE ( 'NONE', #135948, 2.999999999999999112 ) ;
#27179 = EDGE_CURVE ( 'NONE', #31209, #15110, #8807, .T. ) ;
#27180 = EDGE_LOOP ( 'NONE', ( #15051, #4526, #47385, #61463, #107086 ) ) ;
#27181 = AXIS2_PLACEMENT_3D ( 'NONE', #8048, #95790, #63208 ) ;
#27182 = ORIENTED_EDGE ( 'NONE', *, *, #122526, .T. ) ;
#27183 = CARTESIAN_POINT ( 'NONE',  ( 94.99543019189812298, 5.291415217122916737, 3.055000000000001936 ) ) ;
#27184 = ORIENTED_EDGE ( 'NONE', *, *, #63475, .T. ) ;
#27185 = DIRECTION ( 'NONE',  ( 0.7071067811865487940, -0.7071067811865463515, 0.000000000000000000 ) ) ;
#27186 = VECTOR ( 'NONE', #110743, 1000.000000000000000 ) ;
#27187 = LINE ( 'NONE', #72181, #81469 ) ;
#27188 = CARTESIAN_POINT ( 'NONE',  ( -4.499999999999967137, 16.77039438581778796, 0.4657186855307844375 ) ) ;
#27189 = CARTESIAN_POINT ( 'NONE',  ( 25.34840764549667469, -3.851859888774471706E-31, 2.500000000000001332 ) ) ;
#27190 = ORIENTED_EDGE ( 'NONE', *, *, #24251, .T. ) ;
#27191 = LINE ( 'NONE', #83763, #15945 ) ;
#27192 = DIRECTION ( 'NONE',  ( 0.000000000000000000, 0.000000000000000000, 1.000000000000000000 ) ) ;
#27193 = EDGE_CURVE ( 'NONE', #103105, #129709, #97263, .T. ) ;
#27194 = CARTESIAN_POINT ( 'NONE',  ( -2.816011393730999401, 28.73617430169785436, 5.000000000000000000 ) ) ;
#27196 = DIRECTION ( 'NONE',  ( -0.000000000000000000, 0.3543493200069153248, 0.9351131265310292928 ) ) ;
#27195 = LINE ( 'NONE', #108842, #62115 ) ;
#27197 = DIRECTION ( 'NONE',  ( -0.7071067811865486830, 0.7071067811865464625, 0.000000000000000000 ) ) ;
#27198 = CARTESIAN_POINT ( 'NONE',  ( 181.0878408821075141, -48.47815212813053165, -38.14157743968407033 ) ) ;
#27199 = CARTESIAN_POINT ( 'NONE',  ( 20.99999999999983658, -22.22500000000000142, 4.412002311789984255 ) ) ;
#27200 = ORIENTED_EDGE ( 'NONE', *, *, #140070, .F. ) ;
#27201 = LINE ( 'NONE', #93891, #56616 ) ;
#27202 = CARTESIAN_POINT ( 'NONE',  ( -4.171830600776442743, -14.24070752338413648, 4.000000000000000000 ) ) ;
#27203 = ORIENTED_EDGE ( 'NONE', *, *, #136295, .T. ) ;
#27204 = ORIENTED_EDGE ( 'NONE', *, *, #48479, .T. ) ;
#27205 = EDGE_CURVE ( 'NONE', #90987, #66739, #111009, .T. ) ;
#27206 = VERTEX_POINT ( 'NONE', #123368 ) ;
#27207 = CARTESIAN_POINT ( 'NONE',  ( 46.81293019189811133, -1.637169565754159617, -6.110000000000001208 ) ) ;
#27208 = AXIS2_PLACEMENT_3D ( 'NONE', #81475, #103185, #37223 ) ;
#27209 = ORIENTED_EDGE ( 'NONE', *, *, #2416, .T. ) ;
#27210 = VECTOR ( 'NONE', #22419, 1000.000000000000000 ) ;
#27211 = CARTESIAN_POINT ( 'NONE',  ( 16.81663961620377634, -1.633150327867691987, -6.094999999999989093 ) ) ;
#27212 = CARTESIAN_POINT ( 'NONE',  ( -13.03876099366718400, 6.774379884391048101, -28.62998901354190195 ) ) ;
#27213 = VERTEX_POINT ( 'NONE', #111758 ) ;
#27214 = CARTESIAN_POINT ( 'NONE',  ( -51.29974487139158867, -27.71228299555242103, 4.000000000000000000 ) ) ;
#27215 = VERTEX_POINT ( 'NONE', #12425 ) ;
#27216 = FACE_OUTER_BOUND ( 'NONE', #124598, .T. ) ;
#27217 = CARTESIAN_POINT ( 'NONE',  ( -10.49999999999992184, -7.533600742197662292, 5.000000000000000000 ) ) ;
#27219 = ORIENTED_EDGE ( 'NONE', *, *, #124288, .F. ) ;
#27218 = CARTESIAN_POINT ( 'NONE',  ( -34.92500000000001137, -22.22500000000000142, 5.000000000000000000 ) ) ;
#27220 = ORIENTED_EDGE ( 'NONE', *, *, #86410, .T. ) ;
#27221 = CARTESIAN_POINT ( 'NONE',  ( -34.49999999999975842, -11.94567065516892690, 4.994342998332167660 ) ) ;
#27222 = DIRECTION ( 'NONE',  ( 0.000000000000000000, 0.000000000000000000, -1.000000000000000000 ) ) ;
#27223 = VERTEX_POINT ( 'NONE', #56705 ) ;
#27224 = PLANE ( 'NONE',  #82871 ) ;
#27225 = ORIENTED_EDGE ( 'NONE', *, *, #103716, .F. ) ;
#27227 = ORIENTED_EDGE ( 'NONE', *, *, #83239, .T. ) ;
#27226 = EDGE_CURVE ( 'NONE', #19025, #9588, #24033, .T. ) ;
#27228 = ORIENTED_EDGE ( 'NONE', *, *, #101625, .F. ) ;
#27229 = ORIENTED_EDGE ( 'NONE', *, *, #83980, .T. ) ;
#27230 = DIRECTION ( 'NONE',  ( 0.000000000000000000, -1.000000000000000000, 0.000000000000000000 ) ) ;
#27231 = CARTESIAN_POINT ( 'NONE',  ( -17.57672154193636160, 11.25929247661559529, 17.85071094206588427 ) ) ;
#27233 = ADVANCED_FACE ( 'NONE', ( #101570 ), #68292, .F. ) ;
#27232 = DIRECTION ( 'NONE',  ( -0.7071067811865486830, -0.7071067811865464625, 0.000000000000000000 ) ) ;
#27234 = LINE ( 'NONE', #127266, #122417 ) ;
#27235 = ADVANCED_FACE ( 'NONE', ( #21878 ), #21170, .F. ) ;
#27236 = LINE ( 'NONE', #71481, #97589 ) ;
#27237 = ORIENTED_EDGE ( 'NONE', *, *, #102774, .T. ) ;
#27238 = CARTESIAN_POINT ( 'NONE',  ( 27.18398860626900060, 28.73617430169806042, 5.000000000000000000 ) ) ;
#27239 = CARTESIAN_POINT ( 'NONE',  ( 18.93706980810188867, 2.126176841940952134, -7.934999999999993392 ) ) ;
#27240 = PLANE ( 'NONE',  #71680 ) ;
#27241 = CARTESIAN_POINT ( 'NONE',  ( -15.18398860626900237, 28.73617430169797871, 5.000000000000000000 ) ) ;
#27242 =( GEOMETRIC_REPRESENTATION_CONTEXT ( 3 ) GLOBAL_UNCERTAINTY_ASSIGNED_CONTEXT ( ( #60498 ) ) GLOBAL_UNIT_ASSIGNED_CONTEXT ( ( #69301, #112096, #3966 ) ) REPRESENTATION_CONTEXT ( 'NONE', 'WORKASPACE' ) );
#27243 = EDGE_CURVE ( 'NONE', #27246, #104944, #43635, .T. ) ;
#27244 = FACE_OUTER_BOUND ( 'NONE', #129947, .T. ) ;
#27245 = ORIENTED_EDGE ( 'NONE', *, *, #65035, .T. ) ;
#27246 = VERTEX_POINT ( 'NONE', #134964 ) ;
#27247 = ORIENTED_EDGE ( 'NONE', *, *, #66929, .T. ) ;
#27248 = CARTESIAN_POINT ( 'NONE',  ( 5.816011393731002066, 28.73617430169783304, 5.000000000000000000 ) ) ;
#27249 = DIRECTION ( 'NONE',  ( 0.6830127018922181881, 0.6830127018922202975, -0.2588190451025214056 ) ) ;
#27250 = UNCERTAINTY_MEASURE_WITH_UNIT (LENGTH_MEASURE( 1.000000000000000082E-05 ), #109529, 'distance_accuracy_value', 'NONE');
#27251 = CARTESIAN_POINT ( 'NONE',  ( -11.99451991528749417, 28.92564299267946382, 4.000000000000000000 ) ) ;
#27252 = CARTESIAN_POINT ( 'NONE',  ( 34.49999999999976552, 1.087461875839230707, 4.000000000000000000 ) ) ;
#27253 = CARTESIAN_POINT ( 'NONE',  ( 24.60486233187506855, 21.75929247661550647, 21.32995629748181088 ) ) ;
#27254 = CARTESIAN_POINT ( 'NONE',  ( 77.20376352523145158, 6.109999999999999432, 1.122388791418549108E-15 ) ) ;
#27255 = EDGE_CURVE ( 'NONE', #16368, #122297, #133512, .T. ) ;
#27256 = CARTESIAN_POINT ( 'NONE',  ( 80.62500000000000000, -7.950000000000000178, -4.867971026610729436E-16 ) ) ;
#27258 = VECTOR ( 'NONE', #19805, 1000.000000000000000 ) ;
#27257 = DIRECTION ( 'NONE',  ( -0.7071067811865486830, -0.7071067811865464625, 0.000000000000000000 ) ) ;
#27259 = CARTESIAN_POINT ( 'NONE',  ( -12.20000000000000284, -28.33999999999998565, 13.17925390838734323 ) ) ;
#27260 = DIRECTION ( 'NONE',  ( -0.000000000000000000, -0.3543493200069152693, 0.9351131265310292928 ) ) ;
#27261 = DIRECTION ( 'NONE',  ( 0.6830127018922180770, -0.6830127018922204085, -0.2588190451025213501 ) ) ;
#27262 = ORIENTED_EDGE ( 'NONE', *, *, #17321, .F. ) ;
#27263 = CARTESIAN_POINT ( 'NONE',  ( 19.93618820135884917, -3.269999999999996909, -36.39086428169088094 ) ) ;
#27264 = ORIENTED_EDGE ( 'NONE', *, *, #86785, .T. ) ;
#27265 = VECTOR ( 'NONE', #93206, 1000.000000000000000 ) ;
#27266 = CARTESIAN_POINT ( 'NONE',  ( -30.48921356237309510, -27.52281430457076894, 5.000000000000000000 ) ) ;
#27268 = VERTEX_POINT ( 'NONE', #121886 ) ;
#27267 = CARTESIAN_POINT ( 'NONE',  ( 7.940000000000001279, -35.14999999999999858, -11.89864999999999640 ) ) ;
#27269 = VECTOR ( 'NONE', #3112, 1000.000000000000000 ) ;
#27270 = CARTESIAN_POINT ( 'NONE',  ( -42.48921356237308800, -27.52281430457085065, 5.000000000000000000 ) ) ;
#27271 = LINE ( 'NONE', #93257, #109692 ) ;
#27272 = ORIENTED_EDGE ( 'NONE', *, *, #39785, .F. ) ;
#27273 = CARTESIAN_POINT ( 'NONE',  ( -28.49999999999979750, -13.91253812416061386, 4.000000000000000000 ) ) ;
#27274 = ORIENTED_EDGE ( 'NONE', *, *, #80634, .F. ) ;
#27275 = CARTESIAN_POINT ( 'NONE',  ( -8.700255128608413102, -27.71228299555199825, 4.000000000000000000 ) ) ;
#27276 = ORIENTED_EDGE ( 'NONE', *, *, #14799, .F. ) ;
#27277 = CARTESIAN_POINT ( 'NONE',  ( 69.18398860626899705, 28.73617430169835529, 5.000000000000000000 ) ) ;
#27278 = CARTESIAN_POINT ( 'NONE',  ( 90.93336038379621300, 2.130196079827431532, -7.949999999999997513 ) ) ;
#27279 = CARTESIAN_POINT ( 'NONE',  ( 72.60416666666665719, 2.130196079827422206, 7.950000000000001954 ) ) ;
#27280 = ADVANCED_FACE ( 'NONE', ( #44389 ), #22560, .F. ) ;
#27281 =( NAMED_UNIT ( * ) PLANE_ANGLE_UNIT ( ) SI_UNIT ( $, .RADIAN. ) );
#27282 = ORIENTED_EDGE ( 'NONE', *, *, #88553, .F. ) ;
#27283 = CARTESIAN_POINT ( 'NONE',  ( 26.75159235450331963, 9.902892378096218942E-16, 0.000000000000000000 ) ) ;
#27284 = EDGE_CURVE ( 'NONE', #90422, #47233, #66128, .T. ) ;
#27285 = CARTESIAN_POINT ( 'NONE',  ( 42.48921356237308800, -27.52281430457085065, 5.000000000000000000 ) ) ;
#27286 = CARTESIAN_POINT ( 'NONE',  ( 23.18750000000000355, 4.461849672132297329, -4.461849672132302658 ) ) ;
#27287 = CARTESIAN_POINT ( 'NONE',  ( -7.499999999999940492, 10.46639925780215208, 5.000000000000000000 ) ) ;
#27288 = CARTESIAN_POINT ( 'NONE',  ( 5.999999999999960032, -19.06887692260762179, 4.000000000000000000 ) ) ;
#27289 = VERTEX_POINT ( 'NONE', #2235 ) ;
#27290 = EDGE_CURVE ( 'NONE', #37516, #141779, #11685, .T. ) ;
#27291 = EDGE_CURVE ( 'NONE', #40629, #34286, #115673, .T. ) ;
#27292 = CARTESIAN_POINT ( 'NONE',  ( 45.57919371712955581, 3.975000000000002753, -6.884901960086283523 ) ) ;
#27293 = ORIENTED_EDGE ( 'NONE', *, *, #47177, .F. ) ;
#27294 = CARTESIAN_POINT ( 'NONE',  ( 85.75043019189810423, 3.055000000000002824, -5.291415217122919401 ) ) ;
#27295 = CARTESIAN_POINT ( 'NONE',  ( 32.99451991528749062, 28.92564299267960948, 4.000000000000000000 ) ) ;
#27296 = LINE ( 'NONE', #28760, #97840 ) ;
#27297 = DIRECTION ( 'NONE',  ( 0.6830127018922180770, -0.6830127018922204085, -0.2588190451025213501 ) ) ;
#27298 = VERTEX_POINT ( 'NONE', #88594 ) ;
#27299 = LINE ( 'NONE', #96126, #139216 ) ;
#27300 = LINE ( 'NONE', #26608, #136756 ) ;
#27301 = EDGE_CURVE ( 'NONE', #22851, #107195, #10279, .T. ) ;
#27302 = CARTESIAN_POINT ( 'NONE',  ( 117.0375270504628986, -9.735942053221456900E-16, 7.949999999999998401 ) ) ;
#27303 = EDGE_CURVE ( 'NONE', #105156, #113756, #34922, .T. ) ;
#27304 = DIRECTION ( 'NONE',  ( 0.000000000000000000, -1.000000000000000000, 0.000000000000000000 ) ) ;
#27306 = ORIENTED_EDGE ( 'NONE', *, *, #139933, .T. ) ;
#27305 = DIRECTION ( 'NONE',  ( -0.000000000000000000, 0.000000000000000000, 1.000000000000000000 ) ) ;
#27308 = VECTOR ( 'NONE', #98006, 999.9999999999998863 ) ;
#27307 = CARTESIAN_POINT ( 'NONE',  ( 12.25000000000000000, -7.464222240803106570E-16, -6.094999999999989981 ) ) ;
#27309 = CARTESIAN_POINT ( 'NONE',  ( -19.88982677111775388, -22.22500000000000142, 4.785647885939353863 ) ) ;
#27310 = CARTESIAN_POINT ( 'NONE',  ( 0.000000000000000000, -21.76999999999999247, 0.000000000000000000 ) ) ;
#27311 =( BOUNDED_CURVE ( )  B_SPLINE_CURVE ( 2, ( #24272, #2481, #66365, #55490, #12663 ),
 .UNSPECIFIED., .F., .T. ) 
 B_SPLINE_CURVE_WITH_KNOTS ( ( 3, 2, 3 ),
 ( 0.9703747093734275131, 0.9722222222222222099, 0.9749999999999999778 ),
 .UNSPECIFIED. ) 
 CURVE ( )  GEOMETRIC_REPRESENTATION_ITEM ( )  RATIONAL_B_SPLINE_CURVE ( ( 0.9848206055686921090, 0.9773371094525169500, 1.000000000000000000, 0.9659258262890684232, 1.000000000000000000 ) ) 
 REPRESENTATION_ITEM ( '' )  );
#27312 = ORIENTED_EDGE ( 'NONE', *, *, #16847, .F. ) ;
#27313 = VERTEX_POINT ( 'NONE', #33509 ) ;
#27314 = VERTEX_POINT ( 'NONE', #66827 ) ;
#27315 = CARTESIAN_POINT ( 'NONE',  ( 78.45876352523144703, 0.000000000000000000, -6.110000000000001208 ) ) ;
#27316 = ORIENTED_EDGE ( 'NONE', *, *, #8960, .F. ) ;
#27317 = ADVANCED_FACE ( 'NONE', ( #100175 ), #822, .F. ) ;
#27318 = PLANE ( 'NONE',  #5725 ) ;
#27319 = CARTESIAN_POINT ( 'NONE',  ( 12.19999999999999574, -39.93000000000000682, -39.50000000000000000 ) ) ;
#27320 = DIRECTION ( 'NONE',  ( -1.000000000000000000, -1.224606353822377258E-16, -0.000000000000000000 ) ) ;
#27321 = CARTESIAN_POINT ( 'NONE',  ( 7.720000000000001528, 9.521314400968980422E-16, 0.000000000000000000 ) ) ;
#27322 = ORIENTED_EDGE ( 'NONE', *, *, #65445, .T. ) ;
#27323 = ADVANCED_FACE ( 'NONE', ( #35658 ), #67566, .F. ) ;
#27324 = DIRECTION ( 'NONE',  ( 0.7071067811865486830, -0.7071067811865464625, -0.000000000000000000 ) ) ;
#27325 = DIRECTION ( 'NONE',  ( -0.000000000000000000, 0.3543493200069153248, 0.9351131265310291818 ) ) ;
#27326 = VECTOR ( 'NONE', #69943, 1000.000000000000227 ) ;
#27327 = ORIENTED_EDGE ( 'NONE', *, *, #35134, .T. ) ;
#27328 = CARTESIAN_POINT ( 'NONE',  ( 1.320799999999991092, -0.1737498520445722172, 3.775643966265890938 ) ) ;
#27329 = FACE_OUTER_BOUND ( 'NONE', #87629, .T. ) ;
#27330 = EDGE_CURVE ( 'NONE', #111999, #135296, #101953, .T. ) ;
#27331 = CARTESIAN_POINT ( 'NONE',  ( 12.35051985313232237, -2.500000000000000444, 3.061616997868384127E-16 ) ) ;
#27332 = EDGE_LOOP ( 'NONE', ( #19956, #77522, #135414, #20382 ) ) ;
#27333 = EDGE_LOOP ( 'NONE', ( #50597, #7173, #93192, #104103 ) ) ;
#27334 = CARTESIAN_POINT ( 'NONE',  ( 24.27626632409106477, -22.22500000000000142, 27.43357286974619669 ) ) ;
#27335 = FACE_OUTER_BOUND ( 'NONE', #107760, .T. ) ;
#27336 = DIRECTION ( 'NONE',  ( -1.000000000000000000, -0.000000000000000000, -0.000000000000000000 ) ) ;
#27337 = LINE ( 'NONE', #73716, #72004 ) ;
#27338 = CARTESIAN_POINT ( 'NONE',  ( 11.99999999999991296, -13.97847968911259109, -0.1324546996126522713 ) ) ;
#27339 = EDGE_CURVE ( 'NONE', #71183, #116824, #26177, .T. ) ;
#27340 = CARTESIAN_POINT ( 'NONE',  ( 149.2199999999997999, -3.180000000000061444, -34.92499999999998295 ) ) ;
#27341 = LINE ( 'NONE', #73044, #60470 ) ;
#27342 = ADVANCED_FACE ( 'NONE', ( #125491 ), #37776, .F. ) ;
#27343 = ORIENTED_EDGE ( 'NONE', *, *, #119876, .F. ) ;
#27344 = ORIENTED_EDGE ( 'NONE', *, *, #96496, .T. ) ;
#27345 = VECTOR ( 'NONE', #10433, 1000.000000000000000 ) ;
#27346 = ORIENTED_EDGE ( 'NONE', *, *, #27144, .T. ) ;
#27347 = ORIENTED_EDGE ( 'NONE', *, *, #5485, .F. ) ;
#27348 = FACE_OUTER_BOUND ( 'NONE', #104031, .T. ) ;
#27349 = ORIENTED_EDGE ( 'NONE', *, *, #94836, .T. ) ;
#27350 = CARTESIAN_POINT ( 'NONE',  ( -20.99999999999986500, 14.87792677143806941, -11.06722581663444771 ) ) ;
#27351 = DIRECTION ( 'NONE',  ( -0.7071067811865486830, -0.7071067811865464625, 0.000000000000000000 ) ) ;
#27352 = CARTESIAN_POINT ( 'NONE',  ( -50.99451991528749062, 28.92564299267973738, 4.000000000000000000 ) ) ;
#27353 = DIRECTION ( 'NONE',  ( 0.7071067811865487940, -0.7071067811865463515, 0.000000000000000000 ) ) ;
#27354 = VECTOR ( 'NONE', #105673, 1000.000000000000000 ) ;
#27355 = DIRECTION ( 'NONE',  ( 0.7071067811865487940, 0.7071067811865463515, -0.000000000000000000 ) ) ;
#27356 = ORIENTED_EDGE ( 'NONE', *, *, #91186, .F. ) ;
#27357 = DIRECTION ( 'NONE',  ( 0.000000000000000000, -1.000000000000000000, 0.000000000000000000 ) ) ;
#27358 = DIRECTION ( 'NONE',  ( -0.6830127018922180770, -0.6830127018922204085, -0.2588190451025213501 ) ) ;
#27359 = ORIENTED_EDGE ( 'NONE', *, *, #102990, .F. ) ;
#27360 = CARTESIAN_POINT ( 'NONE',  ( -28.17183060077627843, -2.240707523384257716, 4.000000000000000000 ) ) ;
#27361 = ORIENTED_EDGE ( 'NONE', *, *, #14169, .F. ) ;
#27362 = VERTEX_POINT ( 'NONE', #92119 ) ;
#27363 = PLANE ( 'NONE',  #1878 ) ;
#27364 = ORIENTED_EDGE ( 'NONE', *, *, #127528, .T. ) ;
#27365 = ORIENTED_EDGE ( 'NONE', *, *, #131799, .T. ) ;
#27366 = CARTESIAN_POINT ( 'NONE',  ( 75.54209685856477563, 5.291415217122923842, -3.054999999999996163 ) ) ;
#27367 = VECTOR ( 'NONE', #100327, 1000.000000000000000 ) ;
#27368 = ORIENTED_EDGE ( 'NONE', *, *, #33855, .F. ) ;
#27369 = VECTOR ( 'NONE', #29682, 1000.000000000000000 ) ;
#27370 = SURFACE_SIDE_STYLE ('',( #126687 ) ) ;
#27371 = DIRECTION ( 'NONE',  ( -0.3543493200069162685, -0.000000000000000000, -0.9351131265310288487 ) ) ;
#27372 = CARTESIAN_POINT ( 'NONE',  ( 109.8129301918981184, -1.637169565754159617, -6.110000000000001208 ) ) ;
#27373 = CARTESIAN_POINT ( 'NONE',  ( 27.99999999999999645, -49.14999999999999147, -45.92499999999969873 ) ) ;
#27374 = EDGE_CURVE ( 'NONE', #42523, #15565, #37172, .T. ) ;
#27376 = ADVANCED_FACE ( 'NONE', ( #126198 ), #113525, .T. ) ;
#27375 = CARTESIAN_POINT ( 'NONE',  ( 30.18398860626900060, 28.73617430169808173, 5.000000000000000000 ) ) ;
#27377 = DIRECTION ( 'NONE',  ( -0.6830127018922181881, 0.6830127018922202975, -0.2588190451025214056 ) ) ;
#27378 = FACE_OUTER_BOUND ( 'NONE', #11783, .T. ) ;
#27379 = VECTOR ( 'NONE', #77746, 1000.000000000000000 ) ;
#27380 = DIRECTION ( 'NONE',  ( -0.000000000000000000, 0.000000000000000000, 1.000000000000000000 ) ) ;
#27381 = CARTESIAN_POINT ( 'NONE',  ( -11.99451991528749417, 28.92564299267946382, 4.000000000000000000 ) ) ;
#27382 = CARTESIAN_POINT ( 'NONE',  ( -1.499999999999990896, 21.43112307739196609, 4.000000000000000000 ) ) ;
#27383 = ORIENTED_EDGE ( 'NONE', *, *, #31327, .T. ) ;
#27384 = AXIS2_PLACEMENT_3D ( 'NONE', #57104, #112185, #78128 ) ;
#27385 = CARTESIAN_POINT ( 'NONE',  ( -48.18398860626899705, 28.73617430169820608, 5.000000000000000000 ) ) ;
#27386 = ORIENTED_EDGE ( 'NONE', *, *, #123231, .F. ) ;
#27387 = ORIENTED_EDGE ( 'NONE', *, *, #66984, .F. ) ;
#27388 = VECTOR ( 'NONE', #67076, 999.9999999999998863 ) ;
#27389 = LINE ( 'NONE', #15768, #135176 ) ;
#27390 = ORIENTED_EDGE ( 'NONE', *, *, #28430, .T. ) ;
#27391 = VECTOR ( 'NONE', #93066, 1000.000000000000000 ) ;
#27392 = DIRECTION ( 'NONE',  ( -0.7071067811865486830, 0.7071067811865464625, 0.000000000000000000 ) ) ;
#27393 = CARTESIAN_POINT ( 'NONE',  ( 114.6041666666666856, 2.130196079827402666, 7.950000000000014388 ) ) ;
#27394 = VECTOR ( 'NONE', #62365, 999.9999999999998863 ) ;
#27395 = EDGE_CURVE ( 'NONE', #45081, #40200, #74227, .T. ) ;
#27396 = PLANE ( 'NONE',  #69511 ) ;
#27397 = DIRECTION ( 'NONE',  ( 0.6830127018922181881, 0.6830127018922202975, -0.2588190451025214056 ) ) ;
#27398 = ORIENTED_EDGE ( 'NONE', *, *, #34695, .F. ) ;
#27399 = ADVANCED_FACE ( 'NONE', ( #80569 ), #39193, .F. ) ;
#27400 =( NAMED_UNIT ( * ) SI_UNIT ( $, .STERADIAN. ) SOLID_ANGLE_UNIT ( ) );
#27401 = ORIENTED_EDGE ( 'NONE', *, *, #131043, .F. ) ;
#27402 = EDGE_CURVE ( 'NONE', #70361, #98020, #47268, .T. ) ;
#27403 = CARTESIAN_POINT ( 'NONE',  ( 24.12956980810188767, -3.967499999999998028, -6.871911579029511330 ) ) ;
#27404 = DIRECTION ( 'NONE',  ( 0.000000000000000000, -1.000000000000000000, 0.000000000000000000 ) ) ;
#27405 = CARTESIAN_POINT ( 'NONE',  ( 18.17159235450331778, 9.902892378096218942E-16, 0.000000000000000000 ) ) ;
#27406 = EDGE_CURVE ( 'NONE', #75064, #90194, #91437, .T. ) ;
#27407 = DIRECTION ( 'NONE',  ( 0.7071067811865487940, 0.7071067811865463515, 0.000000000000000000 ) ) ;
#27408 = ORIENTED_EDGE ( 'NONE', *, *, #69462, .T. ) ;
#27409 = B_SPLINE_CURVE_WITH_KNOTS ( 'NONE', 3,
 ( #76781, #9295, #142719, #87623, #45583, #78188, #53579, #12192, #97782, #55727, #99930, #42718, #21660, #122371, #592, #44891, #131132, #131853, #109370, #120208 ),
 .UNSPECIFIED., .F., .F.,
 ( 4, 2, 2, 2, 2, 2, 2, 2, 2, 4 ),
 ( 0.000000000000000000, 0.002083055955866117918, 0.003124583933799176226, 0.004166111911732234101, 0.005207639889665291975, 0.006249167867598350717, 0.006769931856564878787, 0.007290695845531407725, 0.007811459834497935795, 0.008332223823464464732 ),
 .UNSPECIFIED. ) ;
#27410 = ORIENTED_EDGE ( 'NONE', *, *, #96857, .F. ) ;
#27411 = EDGE_LOOP ( 'NONE', ( #17700, #115430, #7606, #88964 ) ) ;
#27412 = LINE ( 'NONE', #126054, #919 ) ;
#27413 = CARTESIAN_POINT ( 'NONE',  ( 33.70710678118631165, 20.25929247661551003, 5.000000000000000000 ) ) ;
#27415 = VECTOR ( 'NONE', #63087, 1000.000000000000000 ) ;
#27414 = FACE_OUTER_BOUND ( 'NONE', #70257, .T. ) ;
#27416 = CARTESIAN_POINT ( 'NONE',  ( -19.82816939922339827, -14.24070752338414181, 4.000000000000000000 ) ) ;
#27417 = CARTESIAN_POINT ( 'NONE',  ( 21.29974487139158512, -27.71228299555221142, 4.000000000000000000 ) ) ;
#27418 = CARTESIAN_POINT ( 'NONE',  ( -30.48921356237309510, -27.52281430457076894, 5.000000000000000000 ) ) ;
#27419 = ADVANCED_FACE ( 'NONE', ( #103018 ), #25436, .F. ) ;
#27420 = CARTESIAN_POINT ( 'NONE',  ( 45.48921356237309510, -27.52281430457087197, 5.000000000000000000 ) ) ;
#27421 = CARTESIAN_POINT ( 'NONE',  ( -24.29974487139158867, -27.71228299555223273, 4.000000000000000000 ) ) ;
#27422 = DIRECTION ( 'NONE',  ( 0.6830127018922180770, -0.6830127018922204085, -0.2588190451025213501 ) ) ;
#27423 = ORIENTED_EDGE ( 'NONE', *, *, #48068, .T. ) ;
#27424 = CARTESIAN_POINT ( 'NONE',  ( 15.52000000000000135, 2.055000000000001492, 2.516649172247811554E-16 ) ) ;
#27425 = EDGE_CURVE ( 'NONE', #39039, #6977, #124057, .T. ) ;
#27426 = CARTESIAN_POINT ( 'NONE',  ( 32.99451991528749062, 28.92564299267960948, 4.000000000000000000 ) ) ;
#27427 = ORIENTED_EDGE ( 'NONE', *, *, #72986, .F. ) ;
#27428 = DIRECTION ( 'NONE',  ( 0.7071067811865487940, 0.7071067811865463515, 0.000000000000000000 ) ) ;
#27430 = ORIENTED_EDGE ( 'NONE', *, *, #80883, .T. ) ;
#27429 = FACE_OUTER_BOUND ( 'NONE', #52218, .T. ) ;
#27431 = ORIENTED_EDGE ( 'NONE', *, *, #102563, .F. ) ;
#27432 = FACE_OUTER_BOUND ( 'NONE', #46552, .T. ) ;
#27433 = FACE_OUTER_BOUND ( 'NONE', #45050, .T. ) ;
#27434 = CARTESIAN_POINT ( 'NONE',  ( 11.99999999999991473, -19.22509904557635707, 1.855685503482207510 ) ) ;
#27435 = EDGE_CURVE ( 'NONE', #55364, #132228, #47954, .T. ) ;
#27436 = ORIENTED_EDGE ( 'NONE', *, *, #74856, .T. ) ;
#27437 = VERTEX_POINT ( 'NONE', #69703 ) ;
#27438 = LINE ( 'NONE', #105011, #82262 ) ;
#27439 = DIRECTION ( 'NONE',  ( -0.000000000000000000, 0.000000000000000000, 1.000000000000000000 ) ) ;
#27440 = CARTESIAN_POINT ( 'NONE',  ( 125.2041937171295700, -6.884901960086285300, -3.975000000000000089 ) ) ;
#27441 = FACE_OUTER_BOUND ( 'NONE', #109799, .T. ) ;
#27442 = CARTESIAN_POINT ( 'NONE',  ( 34.92499999999998295, 17.71849043720409256, 4.759050581649320932 ) ) ;
#27443 = LINE ( 'NONE', #115871, #37585 ) ;
#27445 = EDGE_CURVE ( 'NONE', #139988, #128738, #126881, .T. ) ;
#27444 = FACE_OUTER_BOUND ( 'NONE', #97075, .T. ) ;
#27446 = DIRECTION ( 'NONE',  ( -1.000000000000000000, -1.224606353822377258E-16, -0.000000000000000000 ) ) ;
#27447 = CARTESIAN_POINT ( 'NONE',  ( 34.10373647476854586, 5.808823158059036373, 5.808823158059032821 ) ) ;
#27448 = CARTESIAN_POINT ( 'NONE',  ( 10.91623647476855297, -7.934999999999990727, 4.858786175617117713E-16 ) ) ;
#27449 = LINE ( 'NONE', #5693, #39007 ) ;
#27450 = PLANE ( 'NONE',  #139310 ) ;
#27451 = LINE ( 'NONE', #84036, #26998 ) ;
#27452 = ORIENTED_EDGE ( 'NONE', *, *, #49428, .T. ) ;
#27454 = ORIENTED_EDGE ( 'NONE', *, *, #121698, .T. ) ;
#27453 = EDGE_CURVE ( 'NONE', #68687, #74997, #90357, .T. ) ;
#27455 = ADVANCED_FACE ( 'NONE', ( #137077 ), #70440, .T. ) ;
#27456 = CARTESIAN_POINT ( 'NONE',  ( 80.04166666666665719, -3.975000000000002753, 6.884901960086286188 ) ) ;
#27458 = ORIENTED_EDGE ( 'NONE', *, *, #108285, .T. ) ;
#27457 = CARTESIAN_POINT ( 'NONE',  ( 122.6835989386367345, -43.14999999999999147, 34.92499999999998295 ) ) ;
#27459 = ORIENTED_EDGE ( 'NONE', *, *, #24251, .F. ) ;
#27460 = FACE_OUTER_BOUND ( 'NONE', #28180, .T. ) ;
#27461 = CARTESIAN_POINT ( 'NONE',  ( -1.956830458227830416, -22.22500000000000142, 17.49287185427191460 ) ) ;
#27462 = ORIENTED_EDGE ( 'NONE', *, *, #107627, .F. ) ;
#27463 = VECTOR ( 'NONE', #7740, 1000.000000000000000 ) ;
#27464 = VECTOR ( 'NONE', #53468, 1000.000000000000000 ) ;
#27466 = DIRECTION ( 'NONE',  ( -0.6830127018922181881, 0.6830127018922202975, -0.2588190451025214056 ) ) ;
#27465 = VECTOR ( 'NONE', #47223, 1000.000000000000000 ) ;
#27467 = EDGE_CURVE ( 'NONE', #132789, #113538, #27575, .T. ) ;
#27468 = FACE_OUTER_BOUND ( 'NONE', #126771, .T. ) ;
#27469 = VECTOR ( 'NONE', #104378, 1000.000000000000000 ) ;
#27470 = CARTESIAN_POINT ( 'NONE',  ( 29.47599861414531475, 22.03583458319438293, 4.979811245910086726 ) ) ;
#27471 = CARTESIAN_POINT ( 'NONE',  ( 126.4635698499963752, 6.971130382529067582, 0.5264722768656378005 ) ) ;
#27472 = EDGE_CURVE ( 'NONE', #99005, #110390, #94268, .T. ) ;
#27473 = CARTESIAN_POINT ( 'NONE',  ( 32.99999999999977263, -16.06887692260765377, 4.000000000000000000 ) ) ;
#27474 = FACE_OUTER_BOUND ( 'NONE', #96547, .T. ) ;
#27475 = PRESENTATION_STYLE_ASSIGNMENT (( #26779 ) ) ;
#27477 = PLANE ( 'NONE',  #75336 ) ;
#27476 = VECTOR ( 'NONE', #98011, 1000.000000000000227 ) ;
#27478 = PLANE ( 'NONE',  #30780 ) ;
#27479 = CARTESIAN_POINT ( 'NONE',  ( 34.82816939922328459, -8.240707523384196875, 4.000000000000000000 ) ) ;
#27480 = AXIS2_PLACEMENT_3D ( 'NONE', #23519, #47473, #15463 ) ;
#27481 = CARTESIAN_POINT ( 'NONE',  ( -39.48921356237310221, -27.52281430457082934, 5.000000000000000000 ) ) ;
#27482 = ORIENTED_EDGE ( 'NONE', *, *, #594, .T. ) ;
#27483 = ORIENTED_EDGE ( 'NONE', *, *, #10619, .F. ) ;
#27484 = CARTESIAN_POINT ( 'NONE',  ( 109.3754301918981042, -5.291415217122920289, -3.055000000000001492 ) ) ;
#27485 = ORIENTED_EDGE ( 'NONE', *, *, #139619, .T. ) ;
#27486 = ADVANCED_FACE ( 'NONE', ( #116008 ), #24732, .T. ) ;
#27487 = FACE_OUTER_BOUND ( 'NONE', #121615, .T. ) ;
#27488 = ORIENTED_EDGE ( 'NONE', *, *, #36918, .T. ) ;
#27489 = EDGE_CURVE ( 'NONE', #78997, #26888, #42061, .T. ) ;
#27490 = LINE ( 'NONE', #28946, #42152 ) ;
#27491 = LINE ( 'NONE', #107207, #139270 ) ;
#27492 = VECTOR ( 'NONE', #106991, 1000.000000000000000 ) ;
#27493 = CARTESIAN_POINT ( 'NONE',  ( 106.8079301918981230, -6.109999999999998543, 1.637169565754158063 ) ) ;
#27494 = ORIENTED_EDGE ( 'NONE', *, *, #22708, .F. ) ;
#27495 = CARTESIAN_POINT ( 'NONE',  ( -2.241399257802041856, 21.72499999999999432, 5.000000000000000000 ) ) ;
#27496 = ORIENTED_EDGE ( 'NONE', *, *, #92334, .F. ) ;
#27497 = PLANE ( 'NONE',  #77785 ) ;
#27498 = VECTOR ( 'NONE', #63166, 999.9999999999998863 ) ;
#27499 = CARTESIAN_POINT ( 'NONE',  ( 34.92499999999998295, 13.51246187583934955, 4.000000000000000000 ) ) ;
#27500 = CARTESIAN_POINT ( 'NONE',  ( 32.58838509405146056, 22.22500000000000497, 4.777194822843813249 ) ) ;
#27501 = VECTOR ( 'NONE', #128439, 999.9999999999998863 ) ;
#27502 = VECTOR ( 'NONE', #3361, 1000.000000000000000 ) ;
#27503 = CONICAL_SURFACE ( 'NONE', #55377, 2.055000000000001048, 0.9599310885968758145 ) ;
#27504 = VERTEX_POINT ( 'NONE', #72583 ) ;
#27505 = ORIENTED_EDGE ( 'NONE', *, *, #54200, .F. ) ;
#27506 = ORIENTED_EDGE ( 'NONE', *, *, #12062, .T. ) ;
#27507 = CARTESIAN_POINT ( 'NONE',  ( 1.953608656376216022E-15, -6.270000000000002238, -40.00000000000000000 ) ) ;
#27508 = LINE ( 'NONE', #10049, #89368 ) ;
#27509 = CARTESIAN_POINT ( 'NONE',  ( 8.379569808101887674, 3.967499999999998916, 6.871911579029510442 ) ) ;
#27510 = AXIS2_PLACEMENT_3D ( 'NONE', #123243, #47841, #36909 ) ;
#27511 = VECTOR ( 'NONE', #21691, 1000.000000000000000 ) ;
#27512 = LINE ( 'NONE', #13243, #24797 ) ;
#27513 = EDGE_CURVE ( 'NONE', #13138, #42047, #116741, .T. ) ;
#27514 = EDGE_CURVE ( 'NONE', #102792, #33609, #99661, .T. ) ;
#27515 = DIRECTION ( 'NONE',  ( -1.000000000000000000, -1.224606353822377258E-16, -0.000000000000000000 ) ) ;
#27516 = ORIENTED_EDGE ( 'NONE', *, *, #35678, .F. ) ;
#27517 = ORIENTED_EDGE ( 'NONE', *, *, #14709, .T. ) ;
#27518 = DIRECTION ( 'NONE',  ( -0.3543493200069163240, 4.681814790819596721E-17, -0.9351131265310288487 ) ) ;
#27519 = ORIENTED_EDGE ( 'NONE', *, *, #64484, .T. ) ;
#27520 = EDGE_LOOP ( 'NONE', ( #103009, #8488, #74126, #6497 ) ) ;
#27521 = VECTOR ( 'NONE', #72061, 1000.000000000000227 ) ;
#27522 = CARTESIAN_POINT ( 'NONE',  ( 112.2037635252314516, 6.109999999999998543, 1.122388791418548911E-15 ) ) ;
#27523 = LINE ( 'NONE', #3611, #97545 ) ;
#27524 = CARTESIAN_POINT ( 'NONE',  ( -3.851816449618530758, 17.25929247661554911, 8.802941693769193776 ) ) ;
#27525 = ORIENTED_EDGE ( 'NONE', *, *, #103521, .F. ) ;
#27526 = DIRECTION ( 'NONE',  ( -0.6830127018922181881, 0.6830127018922202975, -0.2588190451025214056 ) ) ;
#27527 = DIRECTION ( 'NONE',  ( 0.6830127018922180770, -0.6830127018922204085, -0.2588190451025213501 ) ) ;
#27528 = PLANE ( 'NONE',  #127021 ) ;
#27529 = FILL_AREA_STYLE_COLOUR ( '', #25840 ) ;
#27530 = ORIENTED_EDGE ( 'NONE', *, *, #66589, .T. ) ;
#27531 = CARTESIAN_POINT ( 'NONE',  ( -19.61351471301484750, 9.118430946277902294, 4.525620927308363406 ) ) ;
#27532 = FACE_BOUND ( 'NONE', #55297, .T. ) ;
#27533 = ORIENTED_EDGE ( 'NONE', *, *, #130847, .T. ) ;
#27534 = CARTESIAN_POINT ( 'NONE',  ( 27.53159235450332076, 9.902892378096218942E-16, 0.000000000000000000 ) ) ;
#27535 = LINE ( 'NONE', #61642, #15654 ) ;
#27536 = FACE_OUTER_BOUND ( 'NONE', #32334, .T. ) ;
#27537 = EDGE_LOOP ( 'NONE', ( #733, #22451, #10611, #40769 ) ) ;
#27538 = FACE_OUTER_BOUND ( 'NONE', #79746, .T. ) ;
#27539 = ORIENTED_EDGE ( 'NONE', *, *, #23256, .F. ) ;
#27540 = ORIENTED_EDGE ( 'NONE', *, *, #63621, .T. ) ;
#27541 = ORIENTED_EDGE ( 'NONE', *, *, #13327, .F. ) ;
#27542 = CARTESIAN_POINT ( 'NONE',  ( 41.62043019189810877, 3.055000000000001936, -5.291415217122916737 ) ) ;
#27543 = ORIENTED_EDGE ( 'NONE', *, *, #24429, .T. ) ;
#27544 = CARTESIAN_POINT ( 'NONE',  ( 19.05000000000000071, 3.174999999999997158, 4.000000000000000000 ) ) ;
#27545 = SURFACE_STYLE_USAGE ( .BOTH. , #81262 ) ;
#27546 = DIRECTION ( 'NONE',  ( 1.000000000000000000, 1.224606353822377258E-16, 0.000000000000000000 ) ) ;
#27547 = ADVANCED_FACE ( 'NONE', ( #6498 ), #94968, .F. ) ;
#27548 =( NAMED_UNIT ( * ) PLANE_ANGLE_UNIT ( ) SI_UNIT ( $, .RADIAN. ) );
#27549 = DIRECTION ( 'NONE',  ( 0.7071067811865487940, -0.7071067811865463515, 0.000000000000000000 ) ) ;
#27550 = CARTESIAN_POINT ( 'NONE',  ( -18.33010218547253345, 17.25929247661553845, 19.83885114516075632 ) ) ;
#27551 = PLANE ( 'NONE',  #50603 ) ;
#27552 = CONICAL_SURFACE ( 'NONE', #129395, 2.055000000000001048, 0.9599310885968758145 ) ;
#27553 = CARTESIAN_POINT ( 'NONE',  ( 18.48921356237309510, -27.52281430457068367, 5.000000000000000000 ) ) ;
#27554 = DIRECTION ( 'NONE',  ( -0.7071067811865486830, -0.7071067811865464625, 0.000000000000000000 ) ) ;
#27555 = PLANE ( 'NONE',  #109530 ) ;
#27556 = EDGE_CURVE ( 'NONE', #61244, #124821, #130497, .T. ) ;
#27557 = VERTEX_POINT ( 'NONE', #74696 ) ;
#27558 = ORIENTED_EDGE ( 'NONE', *, *, #58243, .T. ) ;
#27559 = VERTEX_POINT ( 'NONE', #73959 ) ;
#27560 = ORIENTED_EDGE ( 'NONE', *, *, #43514, .F. ) ;
#27561 = LINE ( 'NONE', #71831, #54157 ) ;
#27562 = VECTOR ( 'NONE', #92094, 1000.000000000000227 ) ;
#27563 = CIRCLE ( 'NONE', #6732, 2.500000000000000888 ) ;
#27564 = EDGE_LOOP ( 'NONE', ( #106558, #124021, #5866, #16526 ) ) ;
#27565 = VECTOR ( 'NONE', #14846, 1000.000000000000000 ) ;
#27566 =( BOUNDED_CURVE ( )  B_SPLINE_CURVE ( 3, ( #115039, #15034, #70887, #82462 ),
 .UNSPECIFIED., .F., .T. ) 
 B_SPLINE_CURVE_WITH_KNOTS ( ( 4, 4 ),
 ( 1.901594255663603183, 1.933014472006554740 ),
 .UNSPECIFIED. ) 
 CURVE ( )  GEOMETRIC_REPRESENTATION_ITEM ( )  RATIONAL_B_SPLINE_CURVE ( ( 1.000000000000000000, 0.9999177325257868620, 0.9999177325257868620, 1.000000000000000000 ) ) 
 REPRESENTATION_ITEM ( '' )  );
#27568 = EDGE_LOOP ( 'NONE', ( #76928, #116368, #4757, #67538 ) ) ;
#27567 = EDGE_CURVE ( 'NONE', #28113, #133506, #20264, .T. ) ;
#27569 = FACE_OUTER_BOUND ( 'NONE', #119856, .T. ) ;
#27570 = DIRECTION ( 'NONE',  ( -0.7071067811865486830, 0.7071067811865464625, 0.000000000000000000 ) ) ;
#27571 = EDGE_CURVE ( 'NONE', #110890, #139365, #128353, .T. ) ;
#27572 = EDGE_CURVE ( 'NONE', #47491, #141426, #18843, .T. ) ;
#27573 = CARTESIAN_POINT ( 'NONE',  ( 6.183988606268994381, 28.73617430169791476, 5.000000000000000000 ) ) ;
#27574 = ORIENTED_EDGE ( 'NONE', *, *, #113028, .T. ) ;
#27575 = LINE ( 'NONE', #103693, #73 ) ;
#27577 = VERTEX_POINT ( 'NONE', #31179 ) ;
#27576 = PRESENTATION_LAYER_ASSIGNMENT (  '', '', ( #25208 ) ) ;
#27579 = EDGE_CURVE ( 'NONE', #83894, #92198, #32373, .T. ) ;
#27578 = CARTESIAN_POINT ( 'NONE',  ( -24.32816939922335919, 8.259292476615634371, 4.000000000000000000 ) ) ;
#27580 = ADVANCED_FACE ( 'NONE', ( #29024 ), #39934, .F. ) ;
#27581 = CARTESIAN_POINT ( 'NONE',  ( 10.77958563595370833, 0.000000000000000000, 2.500000000000000444 ) ) ;
#27582 = CARTESIAN_POINT ( 'NONE',  ( -0.2245968585647807325, -2.126176841940958351, -7.934999999999989839 ) ) ;
#27583 = VERTEX_POINT ( 'NONE', #52195 ) ;
#27585 = CARTESIAN_POINT ( 'NONE',  ( -38.57672154193621594, 11.25929247661560240, 17.85071094206593401 ) ) ;
#27584 = CARTESIAN_POINT ( 'NONE',  ( 99.37043019189812298, -3.055000000000001936, 5.291415217122918513 ) ) ;
#27586 = ADVANCED_FACE ( 'NONE', ( #51506 ), #118877, .F. ) ;
#27587 = CARTESIAN_POINT ( 'NONE',  ( 16.00193056682086379, -22.22500000000000142, 4.500000000000000888 ) ) ;
#27588 = ORIENTED_EDGE ( 'NONE', *, *, #1887, .F. ) ;
#27589 = ORIENTED_EDGE ( 'NONE', *, *, #131094, .F. ) ;
#27590 = FACE_OUTER_BOUND ( 'NONE', #57545, .T. ) ;
#27591 = ORIENTED_EDGE ( 'NONE', *, *, #32114, .F. ) ;
#27592 = CARTESIAN_POINT ( 'NONE',  ( 7.140000000000044089, -1.036479131253094653E-14, -40.00000000000000000 ) ) ;
#27594 = LINE ( 'NONE', #15267, #101961 ) ;
#27593 = CIRCLE ( 'NONE', #85537, 5.999999999999998224 ) ;
#27595 = FACE_OUTER_BOUND ( 'NONE', #32719, .T. ) ;
#27596 = CARTESIAN_POINT ( 'NONE',  ( -36.18398860626899705, 28.73617430169812437, 5.000000000000000000 ) ) ;
#27597 = CARTESIAN_POINT ( 'NONE',  ( 34.92499999999998295, -14.33753812416083129, 4.000000000000000000 ) ) ;
#27598 = PRESENTATION_STYLE_ASSIGNMENT (( #58878 ) ) ;
#27599 = VERTEX_POINT ( 'NONE', #7957 ) ;
#27600 = DIRECTION ( 'NONE',  ( 0.7071067811865487940, -0.7071067811865463515, 0.000000000000000000 ) ) ;
#27601 = EDGE_CURVE ( 'NONE', #118949, #5220, #108680, .T. ) ;
#27602 = AXIS2_PLACEMENT_3D ( 'NONE', #51032, #5351, #14820 ) ;
#27603 = CARTESIAN_POINT ( 'NONE',  ( -4.912274722134691121E-20, 1.320799999999990870, 4.000000000000000000 ) ) ;
#27604 = PLANE ( 'NONE',  #104737 ) ;
#27605 = VERTEX_POINT ( 'NONE', #95697 ) ;
#27606 = CARTESIAN_POINT ( 'NONE',  ( 15.48921356237309510, -27.52281430457066236, 5.000000000000000000 ) ) ;
#27607 = AXIS2_PLACEMENT_3D ( 'NONE', #108409, #96825, #143226 ) ;
#27609 = VECTOR ( 'NONE', #42479, 1000.000000000000000 ) ;
#27608 = CARTESIAN_POINT ( 'NONE',  ( -2.999999999999977351, -15.03360074219758502, 5.000000000000000000 ) ) ;
#27610 = ORIENTED_EDGE ( 'NONE', *, *, #3651, .F. ) ;
#27611 = AXIS2_PLACEMENT_3D ( 'NONE', #31924, #110173, #110872 ) ;
#27613 = ORIENTED_EDGE ( 'NONE', *, *, #65135, .F. ) ;
#27612 = FACE_OUTER_BOUND ( 'NONE', #57709, .T. ) ;
#27614 = ORIENTED_EDGE ( 'NONE', *, *, #85117, .F. ) ;
#27615 = CARTESIAN_POINT ( 'NONE',  ( -15.56688804974254126, 7.140284830960222706, -28.42913291040909840 ) ) ;
#27616 = AXIS2_PLACEMENT_3D ( 'NONE', #129463, #22122, #74401 ) ;
#27617 = CARTESIAN_POINT ( 'NONE',  ( -34.49999999999975131, -19.53574439159930876, 4.994342998332169437 ) ) ;
#27618 = EDGE_CURVE ( 'NONE', #75984, #94048, #96382, .T. ) ;
#27619 = VERTEX_POINT ( 'NONE', #140623 ) ;
#27620 = DIRECTION ( 'NONE',  ( 0.6830127018922180770, -0.6830127018922204085, -0.2588190451025213501 ) ) ;
#27621 = MECHANICAL_DESIGN_GEOMETRIC_PRESENTATION_REPRESENTATION (  '', ( #134140 ), #48434 ) ;
#27622 = CARTESIAN_POINT ( 'NONE',  ( -10.49999999999992539, -20.53675388469231322, 2.352720554255868013 ) ) ;
#27623 = VERTEX_POINT ( 'NONE', #41310 ) ;
#27624 = CARTESIAN_POINT ( 'NONE',  ( 18.32266436734346726, 4.202752102959690472E-16, 0.000000000000000000 ) ) ;
#27625 = PLANE ( 'NONE',  #32720 ) ;
#27626 = CARTESIAN_POINT ( 'NONE',  ( 18.32266436734346726, 4.202752102959690472E-16, 0.000000000000000000 ) ) ;
#27627 = CARTESIAN_POINT ( 'NONE',  ( -66.29974487139159578, -27.71228299555252406, 4.000000000000000000 ) ) ;
#27628 = EDGE_CURVE ( 'NONE', #7053, #81238, #129755, .T. ) ;
#27629 = LINE ( 'NONE', #105197, #16560 ) ;
#27630 = CARTESIAN_POINT ( 'NONE',  ( 26.33642480454907187, 4.648522628062373485, -4.648522628062370821 ) ) ;
#27631 = CARTESIAN_POINT ( 'NONE',  ( 29.39169371712955936, 2.130196079827421762, 7.950000000000000178 ) ) ;
#27632 = CARTESIAN_POINT ( 'NONE',  ( 21.18398860626899349, 28.73617430169802134, 5.000000000000000000 ) ) ;
#27633 = EDGE_LOOP ( 'NONE', ( #63830, #7601, #79392, #68573 ) ) ;
#27634 = ORIENTED_EDGE ( 'NONE', *, *, #53003, .T. ) ;
#27635 = ORIENTED_EDGE ( 'NONE', *, *, #113058, .T. ) ;
#27636 = EDGE_CURVE ( 'NONE', #23479, #24882, #53641, .T. ) ;
#27637 = CARTESIAN_POINT ( 'NONE',  ( 119.4166666666666714, -6.884901960086287076, -3.975000000000000977 ) ) ;
#27638 = ORIENTED_EDGE ( 'NONE', *, *, #9938, .T. ) ;
#27639 = ORIENTED_EDGE ( 'NONE', *, *, #45037, .F. ) ;
#27640 = ADVANCED_FACE ( 'NONE', ( #127630 ), #20986, .F. ) ;
#27641 = ORIENTED_EDGE ( 'NONE', *, *, #131462, .F. ) ;
#27642 =( NAMED_UNIT ( * ) SI_UNIT ( $, .STERADIAN. ) SOLID_ANGLE_UNIT ( ) );
#27643 = CARTESIAN_POINT ( 'NONE',  ( -30.70679250724055009, 20.25929247661551358, 20.83292124670821721 ) ) ;
#27644 = ORIENTED_EDGE ( 'NONE', *, *, #44593, .F. ) ;
#27645 = CARTESIAN_POINT ( 'NONE',  ( 2.343289998337851898, 3.759292476615681888, 13.27625715073266122 ) ) ;
#27646 = EDGE_CURVE ( 'NONE', #14833, #16596, #112308, .T. ) ;
#27647 = CARTESIAN_POINT ( 'NONE',  ( 0.3281693992235254487, 5.259292476615662792, 4.000000000000000000 ) ) ;
#27648 = DIRECTION ( 'NONE',  ( -0.7071067811865487940, 0.7071067811865463515, 0.000000000000000000 ) ) ;
#27649 = CARTESIAN_POINT ( 'NONE',  ( 0.000000000000000000, 0.000000000000000000, 5.000000000000000000 ) ) ;
#27650 = CARTESIAN_POINT ( 'NONE',  ( 113.8962635252314328, 4.472830434245840259, -4.472830434245839371 ) ) ;
#27651 = ORIENTED_EDGE ( 'NONE', *, *, #74258, .T. ) ;
#27652 = CARTESIAN_POINT ( 'NONE',  ( 4.499999999999968914, 8.319652575858395238, -8.582050562765816792 ) ) ;
#27653 = CARTESIAN_POINT ( 'NONE',  ( -5.292893218813418343, 20.25929247661551358, 5.000000000000000000 ) ) ;
#27654 = DIRECTION ( 'NONE',  ( -0.5735764363510503783, -0.8191520442889886899, 0.000000000000000000 ) ) ;
#27655 = CARTESIAN_POINT ( 'NONE',  ( -15.48921356237309510, -27.52281430457066236, 5.000000000000000000 ) ) ;
#27656 = FILL_AREA_STYLE ('',( #93651 ) ) ;
#27657 = ADVANCED_FACE ( 'NONE', ( #100715 ), #12957, .F. ) ;
#27658 = CARTESIAN_POINT ( 'NONE',  ( 18.32266436734346726, 4.202752102959690472E-16, 0.000000000000000000 ) ) ;
#27659 = DIRECTION ( 'NONE',  ( -0.6830127018922180770, -0.6830127018922204085, -0.2588190451025213501 ) ) ;
#27660 = CARTESIAN_POINT ( 'NONE',  ( 33.62086038379622011, -6.884901960086286188, 3.974999999999997424 ) ) ;
#27661 = DIRECTION ( 'NONE',  ( -0.7071067811865486830, -0.7071067811865464625, 0.000000000000000000 ) ) ;
#27662 = FILL_AREA_STYLE ('',( #5887 ) ) ;
#27663 = VERTEX_POINT ( 'NONE', #32612 ) ;
#27664 = ORIENTED_EDGE ( 'NONE', *, *, #84258, .T. ) ;
#27665 = CARTESIAN_POINT ( 'NONE',  ( 33.95833333333332860, 3.974999999999997424, 6.884901960086288852 ) ) ;
#27666 = ORIENTED_EDGE ( 'NONE', *, *, #115171, .T. ) ;
#27667 = EDGE_CURVE ( 'NONE', #132444, #10395, #110826, .T. ) ;
#27668 = CARTESIAN_POINT ( 'NONE',  ( -27.18398860626900060, 28.73617430169806042, 5.000000000000000000 ) ) ;
#27669 = CARTESIAN_POINT ( 'NONE',  ( 150.3000000000000114, 0.000000000000000000, 0.000000000000000000 ) ) ;
#27670 = ORIENTED_EDGE ( 'NONE', *, *, #112372, .T. ) ;
#27671 = LINE ( 'NONE', #8729, #54947 ) ;
#27672 = LINE ( 'NONE', #138602, #12145 ) ;
#27673 = CARTESIAN_POINT ( 'NONE',  ( -33.48921356237309510, -27.52281430457078670, 5.000000000000000000 ) ) ;
#27674 = LINE ( 'NONE', #62471, #14114 ) ;
#27675 = CARTESIAN_POINT ( 'NONE',  ( 31.06293019189809712, 1.637169565754157174, 6.110000000000002984 ) ) ;
#27676 = EDGE_LOOP ( 'NONE', ( #29143, #128343, #38816, #118288, #106743 ) ) ;
#27677 = CARTESIAN_POINT ( 'NONE',  ( 9.707106781186478628, -18.74070752338408496, 5.000000000000000000 ) ) ;
#27678 = ORIENTED_EDGE ( 'NONE', *, *, #141668, .F. ) ;
#27679 = CARTESIAN_POINT ( 'NONE',  ( -12.20000000000000284, -34.64999999999999147, -39.50000000000000000 ) ) ;
#27680 = AXIS2_PLACEMENT_3D ( 'NONE', #55766, #131164, #130471 ) ;
#27681 = VECTOR ( 'NONE', #132852, 1000.000000000000000 ) ;
#27682 = VECTOR ( 'NONE', #47283, 1000.000000000000000 ) ;
#27683 = CARTESIAN_POINT ( 'NONE',  ( -16.88982677111777875, -22.22500000000000142, 4.785647885939354751 ) ) ;
#27684 = DIRECTION ( 'NONE',  ( -0.000000000000000000, -0.3543493200069152693, 0.9351131265310292928 ) ) ;
#27685 = VECTOR ( 'NONE', #11296, 1000.000000000000000 ) ;
#27686 = CARTESIAN_POINT ( 'NONE',  ( 0.000000000000000000, 0.000000000000000000, 5.000000000000000000 ) ) ;
#27687 = ORIENTED_EDGE ( 'NONE', *, *, #120542, .T. ) ;
#27688 = EDGE_CURVE ( 'NONE', #10245, #52878, #111574, .T. ) ;
#27689 = CARTESIAN_POINT ( 'NONE',  ( 59.35459685856476142, -1.637169565754161615, 6.110000000000000320 ) ) ;
#27690 = VERTEX_POINT ( 'NONE', #132661 ) ;
#27691 = CARTESIAN_POINT ( 'NONE',  ( -26.51078643762690845, -27.52281430457036748, 5.000000000000000000 ) ) ;
#27692 = CARTESIAN_POINT ( 'NONE',  ( 34.92382263987068569, 21.75929247661549937, 4.252424926123345550 ) ) ;
#27693 = EDGE_CURVE ( 'NONE', #42437, #26598, #10806, .T. ) ;
#27694 = LINE ( 'NONE', #5913, #87115 ) ;
#27695 = CARTESIAN_POINT ( 'NONE',  ( -33.48921356237309510, -27.52281430457078670, 5.000000000000000000 ) ) ;
#27696 = AXIS2_PLACEMENT_3D ( 'NONE', #102899, #57274, #68860 ) ;
#27697 = ADVANCED_FACE ( 'NONE', ( #121719 ), #1359, .F. ) ;
#27698 = VECTOR ( 'NONE', #113, 999.9999999999998863 ) ;
#27699 =( BOUNDED_CURVE ( )  B_SPLINE_CURVE ( 3, ( #83104, #93965, #138923, #125903 ),
 .UNSPECIFIED., .F., .T. ) 
 B_SPLINE_CURVE_WITH_KNOTS ( ( 4, 4 ),
 ( 5.143245962375972091, 6.645403452391247079 ),
 .UNSPECIFIED. ) 
 CURVE ( )  GEOMETRIC_REPRESENTATION_ITEM ( )  RATIONAL_B_SPLINE_CURVE ( ( 1.000000000000000000, 0.8206354192515254997, 0.8206354192515254997, 1.000000000000000000 ) ) 
 REPRESENTATION_ITEM ( '' )  );
#27700 = CARTESIAN_POINT ( 'NONE',  ( 49.93293019189810167, 1.637169565754156508, 6.110000000000000320 ) ) ;
#27701 = EDGE_LOOP ( 'NONE', ( #140740, #57063, #30762, #92783, #107120 ) ) ;
#27702 = CARTESIAN_POINT ( 'NONE',  ( 20.20710678118640402, -20.24070752338407431, 5.000000000000000000 ) ) ;
#27703 = LINE ( 'NONE', #125617, #94033 ) ;
#27704 = EDGE_LOOP ( 'NONE', ( #22659, #18274, #87342 ) ) ;
#27705 = EDGE_LOOP ( 'NONE', ( #87469, #463, #19680, #5954 ) ) ;
#27706 = VECTOR ( 'NONE', #110353, 999.9999999999998863 ) ;
#27707 = CARTESIAN_POINT ( 'NONE',  ( -14.67183060077637080, 8.259292476615636147, 4.000000000000000000 ) ) ;
#27708 = EDGE_LOOP ( 'NONE', ( #2167, #110550, #19514, #73047 ) ) ;
#27709 = EDGE_CURVE ( 'NONE', #107864, #43625, #76100, .T. ) ;
#27710 = AXIS2_PLACEMENT_3D ( 'NONE', #15335, #71206, #59622 ) ;
#27711 = EDGE_CURVE ( 'NONE', #43404, #116730, #88421, .T. ) ;
#27712 = DIRECTION ( 'NONE',  ( -0.7071067811865486830, 0.7071067811865464625, 0.000000000000000000 ) ) ;
#27713 = ORIENTED_EDGE ( 'NONE', *, *, #53457, .F. ) ;
#27714 = CARTESIAN_POINT ( 'NONE',  ( 2.999999999999999112, -43.14999999999999147, -40.92499999999998295 ) ) ;
#27715 = VECTOR ( 'NONE', #31448, 1000.000000000000227 ) ;
#27716 = VECTOR ( 'NONE', #75627, 1000.000000000000000 ) ;
#27718 = VECTOR ( 'NONE', #111443, 1000.000000000000000 ) ;
#27717 = CARTESIAN_POINT ( 'NONE',  ( -25.49999999999981881, -20.94781430457061333, 5.000000000000000000 ) ) ;
#27719 = FACE_BOUND ( 'NONE', #25279, .T. ) ;
#27720 = EDGE_CURVE ( 'NONE', #122403, #99882, #57231, .T. ) ;
#27721 = CARTESIAN_POINT ( 'NONE',  ( 3.706123077391933140, 22.22500000000000142, 4.000000000000000000 ) ) ;
#27722 = VECTOR ( 'NONE', #116591, 1000.000000000000000 ) ;
#27723 = DIRECTION ( 'NONE',  ( -0.7071067811865486830, -0.7071067811865464625, 0.000000000000000000 ) ) ;
#27725 = AXIS2_PLACEMENT_3D ( 'NONE', #75490, #97954, #31279 ) ;
#27724 = CARTESIAN_POINT ( 'NONE',  ( -81.29974487139159578, -27.71228299555262709, 4.000000000000000000 ) ) ;
#27726 = VERTEX_POINT ( 'NONE', #98552 ) ;
#27727 = DIRECTION ( 'NONE',  ( 0.7071067811865487940, 0.7071067811865463515, 0.000000000000000000 ) ) ;
#27729 = ORIENTED_EDGE ( 'NONE', *, *, #58261, .T. ) ;
#27728 = CYLINDRICAL_SURFACE ( 'NONE', #96880, 0.5000000000000004441 ) ;
#27730 = VECTOR ( 'NONE', #130018, 1000.000000000000000 ) ;
#27731 = ORIENTED_EDGE ( 'NONE', *, *, #69478, .T. ) ;
#27732 = CARTESIAN_POINT ( 'NONE',  ( -6.997731156109542106, -34.88439582560590679, 17.99210858042622974 ) ) ;
#27733 = ORIENTED_EDGE ( 'NONE', *, *, #115798, .F. ) ;
#27734 = VERTEX_POINT ( 'NONE', #33351 ) ;
#27735 = CARTESIAN_POINT ( 'NONE',  ( 65.97459685856478018, 1.637169565754164280, -6.109999999999996767 ) ) ;
#27736 = ORIENTED_EDGE ( 'NONE', *, *, #19575, .T. ) ;
#27737 = DIRECTION ( 'NONE',  ( 0.000000000000000000, -1.000000000000000000, 0.000000000000000000 ) ) ;
#27738 = DIRECTION ( 'NONE',  ( -0.6830127018922180770, -0.6830127018922204085, -0.2588190451025213501 ) ) ;
#27739 = VERTEX_POINT ( 'NONE', #142778 ) ;
#27740 = CARTESIAN_POINT ( 'NONE',  ( -66.18398860626901126, 28.73617430169833753, 5.000000000000000000 ) ) ;
#27741 = CARTESIAN_POINT ( 'NONE',  ( 34.54166666666666430, -3.975000000000002753, 6.884901960086286188 ) ) ;
#27742 = CARTESIAN_POINT ( 'NONE',  ( -12.52400138585440281, 22.03583458319438293, 4.979811245910087614 ) ) ;
#27743 = DIRECTION ( 'NONE',  ( -0.000000000000000000, 0.000000000000000000, 1.000000000000000000 ) ) ;
#27744 = DIRECTION ( 'NONE',  ( -0.7071067811865486830, -0.7071067811865464625, -0.000000000000000000 ) ) ;
#27745 = DIRECTION ( 'NONE',  ( 0.7071067811865487940, -0.7071067811865463515, 0.000000000000000000 ) ) ;
#27746 = VERTEX_POINT ( 'NONE', #11513 ) ;
#27747 = EDGE_CURVE ( 'NONE', #26469, #32802, #661, .T. ) ;
#27748 = AXIS2_PLACEMENT_3D ( 'NONE', #86623, #41666, #82504 ) ;
#27749 = ORIENTED_EDGE ( 'NONE', *, *, #117963, .F. ) ;
#27750 = CARTESIAN_POINT ( 'NONE',  ( 11.56505274454301357, 4.584330080086930965E-16, 0.000000000000000000 ) ) ;
#27751 = FACE_OUTER_BOUND ( 'NONE', #92387, .T. ) ;
#27752 = ORIENTED_EDGE ( 'NONE', *, *, #105978, .T. ) ;
#27753 = ORIENTED_EDGE ( 'NONE', *, *, #11276, .T. ) ;
#27754 = ORIENTED_EDGE ( 'NONE', *, *, #21616, .F. ) ;
#27755 = DIRECTION ( 'NONE',  ( -0.6830127018922180770, -0.6830127018922204085, -0.2588190451025213501 ) ) ;
#27756 = ADVANCED_FACE ( 'NONE', ( #123190 ), #87683, .F. ) ;
#27757 = PLANE ( 'NONE',  #20742 ) ;
#27758 = VERTEX_POINT ( 'NONE', #101407 ) ;
#27759 = DIRECTION ( 'NONE',  ( 0.000000000000000000, -1.000000000000000000, 0.000000000000000000 ) ) ;
#27761 = EDGE_CURVE ( 'NONE', #7238, #46933, #143483, .T. ) ;
#27760 =( BOUNDED_CURVE ( )  B_SPLINE_CURVE ( 3, ( #89527, #64940, #109134, #54089 ),
 .UNSPECIFIED., .F., .T. ) 
 B_SPLINE_CURVE_WITH_KNOTS ( ( 4, 4 ),
 ( 5.043186909253412509, 5.074607125596344304 ),
 .UNSPECIFIED. ) 
 CURVE ( )  GEOMETRIC_REPRESENTATION_ITEM ( )  RATIONAL_B_SPLINE_CURVE ( ( 1.000000000000000000, 0.9999177325257868620, 0.9999177325257868620, 1.000000000000000000 ) ) 
 REPRESENTATION_ITEM ( '' )  );
#27763 = EDGE_CURVE ( 'NONE', #117341, #25152, #99998, .T. ) ;
#27762 = DIRECTION ( 'NONE',  ( -0.6830127018922180770, -0.6830127018922204085, -0.2588190451025213501 ) ) ;
#27764 = ADVANCED_FACE ( 'NONE', ( #131916 ), #76844, .F. ) ;
#27765 = CARTESIAN_POINT ( 'NONE',  ( 11.87956980810188767, 3.967499999999998916, 6.871911579029510442 ) ) ;
#27766 = FACE_OUTER_BOUND ( 'NONE', #51200, .T. ) ;
#27767 = EDGE_CURVE ( 'NONE', #50410, #89049, #88095, .T. ) ;
#27768 = ORIENTED_EDGE ( 'NONE', *, *, #71170, .T. ) ;
#27769 = EDGE_CURVE ( 'NONE', #133213, #64361, #90555, .T. ) ;
#27770 = LINE ( 'NONE', #84332, #132237 ) ;
#27771 = PLANE ( 'NONE',  #17364 ) ;
#27773 = VERTEX_POINT ( 'NONE', #115102 ) ;
#27772 = LINE ( 'NONE', #5982, #65736 ) ;
#27774 = LINE ( 'NONE', #93037, #67979 ) ;
#27775 = EDGE_LOOP ( 'NONE', ( #97098, #109204, #83985, #52209 ) ) ;
#27776 = EDGE_CURVE ( 'NONE', #22900, #6599, #58690, .T. ) ;
#27777 = CARTESIAN_POINT ( 'NONE',  ( -65.99451991528749772, 28.92564299267984396, 4.000000000000000000 ) ) ;
#27778 = CARTESIAN_POINT ( 'NONE',  ( 28.00000000000002487, -57.14999999999999147, -34.92499999999976978 ) ) ;
#27779 = CARTESIAN_POINT ( 'NONE',  ( -34.92500000000001137, -13.48753812416036446, 4.000000000000000000 ) ) ;
#27780 = EDGE_LOOP ( 'NONE', ( #32467, #122244, #113887, #74320 ) ) ;
#27781 = EDGE_CURVE ( 'NONE', #61225, #73668, #80403, .T. ) ;
#27782 = AXIS2_PLACEMENT_3D ( 'NONE', #2055, #36859, #48457 ) ;
#27783 = CARTESIAN_POINT ( 'NONE',  ( 63.18398860626900415, 28.73617430169831621, 5.000000000000000000 ) ) ;
#27784 = CARTESIAN_POINT ( 'NONE',  ( 0.000000000000000000, 0.000000000000000000, 0.000000000000000000 ) ) ;
#27785 = CARTESIAN_POINT ( 'NONE',  ( -4.499999999999966249, -8.947814304570732347, 5.000000000000000000 ) ) ;
#27786 = ORIENTED_EDGE ( 'NONE', *, *, #72386, .F. ) ;
#27787 = AXIS2_PLACEMENT_3D ( 'NONE', #116739, #97083, #29022 ) ;
#27788 = VECTOR ( 'NONE', #98582, 999.9999999999998863 ) ;
#27789 = COLOUR_RGB ( '', 0.40784314, 0.44705882, 0.49803922) ;
#27790 = PLANE ( 'NONE',  #18451 ) ;
#27791 = CARTESIAN_POINT ( 'NONE',  ( -28.49999999999980105, 19.39370406404964697, 1.459788787078267092 ) ) ;
#27792 = LINE ( 'NONE', #128545, #123420 ) ;
#27793 =( GEOMETRIC_REPRESENTATION_CONTEXT ( 3 ) GLOBAL_UNCERTAINTY_ASSIGNED_CONTEXT ( ( #101253 ) ) GLOBAL_UNIT_ASSIGNED_CONTEXT ( ( #49543, #40785, #137240 ) ) REPRESENTATION_CONTEXT ( 'NONE', 'WORKASPACE' ) );
#27794 = ADVANCED_FACE ( 'NONE', ( #81114 ), #135493, .F. ) ;
#27795 = CARTESIAN_POINT ( 'NONE',  ( -21.16809626817622103, 8.755558144015518351, 4.000000000000000000 ) ) ;
#27796 = ORIENTED_EDGE ( 'NONE', *, *, #36482, .T. ) ;
#27797 = EDGE_LOOP ( 'NONE', ( #72271, #53401, #40955, #82930, #18978 ) ) ;
#27798 = DIRECTION ( 'NONE',  ( 0.000000000000000000, -1.000000000000000000, -6.938893903907222067E-15 ) ) ;
#27799 = VECTOR ( 'NONE', #21429, 1000.000000000000227 ) ;
#27800 = CARTESIAN_POINT ( 'NONE',  ( -25.39999999999996305, 0.000000000000000000, 2.500000000000000000 ) ) ;
#27801 = EDGE_CURVE ( 'NONE', #19828, #3251, #124597, .T. ) ;
#27802 = CARTESIAN_POINT ( 'NONE',  ( 3.332903141435219929, -3.967499999999994476, 6.871911579029513106 ) ) ;
#27803 = CARTESIAN_POINT ( 'NONE',  ( 8.901564193917579360, 11.25929247661560595, 10.79108189686409069 ) ) ;
#27804 = DIRECTION ( 'NONE',  ( -0.7071067811865486830, -0.7071067811865464625, 0.000000000000000000 ) ) ;
#27805 = CARTESIAN_POINT ( 'NONE',  ( -34.42500000000001137, -22.22500000000000142, 5.000000000000000000 ) ) ;
#27806 = FACE_OUTER_BOUND ( 'NONE', #122802, .T. ) ;
#27807 = EDGE_LOOP ( 'NONE', ( #87421, #137769, #84567, #81035 ) ) ;
#27808 = DIRECTION ( 'NONE',  ( 0.7071067811865487940, 0.7071067811865463515, 0.000000000000000000 ) ) ;
#27809 = DIRECTION ( 'NONE',  ( -0.7071067811865486830, -0.7071067811865464625, 0.000000000000000000 ) ) ;
#27810 = PLANE ( 'NONE',  #90948 ) ;
#27811 = VECTOR ( 'NONE', #141949, 1000.000000000000227 ) ;
#27812 = VECTOR ( 'NONE', #33242, 1000.000000000000000 ) ;
#27813 = DIRECTION ( 'NONE',  ( 0.000000000000000000, 1.000000000000000000, -4.625929269271485322E-15 ) ) ;
#27814 = CARTESIAN_POINT ( 'NONE',  ( 46.14126352523144448, 4.472830434245837594, 4.472830434245841147 ) ) ;
#27815 = LINE ( 'NONE', #15475, #25644 ) ;
#27816 = VECTOR ( 'NONE', #24991, 1000.000000000000000 ) ;
#27817 = ORIENTED_EDGE ( 'NONE', *, *, #5014, .T. ) ;
#27818 = ORIENTED_EDGE ( 'NONE', *, *, #25557, .T. ) ;
#27819 = ADVANCED_FACE ( 'NONE', ( #24563 ), #102859, .F. ) ;
#27820 = PRESENTATION_LAYER_ASSIGNMENT (  '', '', ( #53263 ) ) ;
#27821 = EDGE_LOOP ( 'NONE', ( #122648, #53613, #64189, #4001 ) ) ;
#27822 = DIRECTION ( 'NONE',  ( 0.000000000000000000, -0.000000000000000000, -1.000000000000000000 ) ) ;
#27823 = VECTOR ( 'NONE', #52957, 1000.000000000000000 ) ;
#27824 = EDGE_CURVE ( 'NONE', #133731, #8580, #57954, .T. ) ;
#27825 = CARTESIAN_POINT ( 'NONE',  ( 45.18398860626900415, 28.73617430169818832, 5.000000000000000000 ) ) ;
#27826 = DIRECTION ( 'NONE',  ( -0.000000000000000000, 0.000000000000000000, 1.000000000000000000 ) ) ;
#27827 = DIRECTION ( 'NONE',  ( 0.6830127018922181881, 0.6830127018922202975, -0.2588190451025214056 ) ) ;
#27828 = CARTESIAN_POINT ( 'NONE',  ( 18.32816939922339827, 14.25929247661557397, 4.000000000000000000 ) ) ;
#27829 = CARTESIAN_POINT ( 'NONE',  ( 12.10416666666666785, -1.633150327867681995, -6.094999999999993534 ) ) ;
#27830 = VECTOR ( 'NONE', #79562, 999.9999999999998863 ) ;
#27831 = ORIENTED_EDGE ( 'NONE', *, *, #35124, .F. ) ;
#27832 = DIRECTION ( 'NONE',  ( -0.000000000000000000, -0.3543493200069152693, 0.9351131265310292928 ) ) ;
#27833 = CARTESIAN_POINT ( 'NONE',  ( 27.53159235450332076, 9.902892378096218942E-16, 0.000000000000000000 ) ) ;
#27834 = CARTESIAN_POINT ( 'NONE',  ( 19.82816939922339117, 12.75929247661558641, 4.000000000000000000 ) ) ;
#27835 = LINE ( 'NONE', #3213, #116783 ) ;
#27836 = EDGE_CURVE ( 'NONE', #90351, #118870, #102148, .T. ) ;
#27837 = FACE_OUTER_BOUND ( 'NONE', #8447, .T. ) ;
#27838 = CARTESIAN_POINT ( 'NONE',  ( 68.62086038379622721, -6.884901960086286188, 3.974999999999997424 ) ) ;
#27839 = DIRECTION ( 'NONE',  ( 0.6830127018922181881, 0.6830127018922202975, -0.2588190451025214056 ) ) ;
#27840 = STYLED_ITEM ( 'NONE', ( #52503 ), #41862 ) ;
#27841 = ORIENTED_EDGE ( 'NONE', *, *, #75179, .T. ) ;
#27842 = VERTEX_POINT ( 'NONE', #113719 ) ;
#27843 = CARTESIAN_POINT ( 'NONE',  ( 68.66666666666665719, 6.884901960086285300, 3.975000000000003642 ) ) ;
#27844 = DIRECTION ( 'NONE',  ( 0.3543493200069163240, 0.000000000000000000, -0.9351131265310288487 ) ) ;
#27845 = ADVANCED_FACE ( 'NONE', ( #48461 ), #70949, .F. ) ;
#27846 = CARTESIAN_POINT ( 'NONE',  ( 12.70710678118645198, 17.25929247661553489, 5.000000000000000000 ) ) ;
#27847 = VECTOR ( 'NONE', #139490, 1000.000000000000000 ) ;
#27848 = ORIENTED_EDGE ( 'NONE', *, *, #131131, .T. ) ;
#27849 = LINE ( 'NONE', #6058, #102315 ) ;
#27850 = CARTESIAN_POINT ( 'NONE',  ( 1.001930566820972812, -22.22500000000000142, 4.500000000000000888 ) ) ;
#27851 = CARTESIAN_POINT ( 'NONE',  ( 55.56293019189809712, 1.637169565754157174, 6.110000000000002984 ) ) ;
#27852 = DIRECTION ( 'NONE',  ( -0.7071067811865487940, 0.7071067811865463515, -0.000000000000000000 ) ) ;
#27853 = ORIENTED_EDGE ( 'NONE', *, *, #73623, .F. ) ;
#27854 = ORIENTED_EDGE ( 'NONE', *, *, #47148, .F. ) ;
#27855 = AXIS2_PLACEMENT_3D ( 'NONE', #121019, #44952, #89131 ) ;
#27856 = DIRECTION ( 'NONE',  ( -0.000000000000000000, 0.000000000000000000, 1.000000000000000000 ) ) ;
#27857 = DIRECTION ( 'NONE',  ( 0.3543493200069162685, -0.000000000000000000, -0.9351131265310288487 ) ) ;
#27858 = CARTESIAN_POINT ( 'NONE',  ( 24.18398860626899705, 28.73617430169804265, 5.000000000000000000 ) ) ;
#27859 = DIRECTION ( 'NONE',  ( -1.000000000000000000, -1.224606353822377258E-16, -0.000000000000000000 ) ) ;
#27860 = EDGE_CURVE ( 'NONE', #35758, #100009, #91960, .T. ) ;
#27861 = LINE ( 'NONE', #103969, #127573 ) ;
#27864 = EDGE_CURVE ( 'NONE', #25222, #32191, #103529, .T. ) ;
#27863 = ORIENTED_EDGE ( 'NONE', *, *, #9944, .T. ) ;
#27862 = CARTESIAN_POINT ( 'NONE',  ( 100.7041937171295558, -6.884901960086285300, -3.975000000000000089 ) ) ;
#27865 = LINE ( 'NONE', #6780, #85447 ) ;
#27866 = CARTESIAN_POINT ( 'NONE',  ( -2.510786437626908008, -27.52281430457053446, 5.000000000000000000 ) ) ;
#27867 = DIRECTION ( 'NONE',  ( 0.7071067811865487940, 0.7071067811865463515, 0.000000000000000000 ) ) ;
#27868 = VECTOR ( 'NONE', #22104, 1000.000000000000000 ) ;
#27869 = CARTESIAN_POINT ( 'NONE',  ( 33.48921356237309510, -27.52281430457078670, 5.000000000000000000 ) ) ;
#27870 = ORIENTED_EDGE ( 'NONE', *, *, #109684, .F. ) ;
#27871 = ORIENTED_EDGE ( 'NONE', *, *, #427, .F. ) ;
#27872 = CARTESIAN_POINT ( 'NONE',  ( -81.18398860626899705, 28.73617430169844056, 5.000000000000000000 ) ) ;
#27873 = DIRECTION ( 'NONE',  ( 0.7071067811865486830, -0.7071067811865464625, -0.000000000000000000 ) ) ;
#27874 = DIRECTION ( 'NONE',  ( 0.7071067811865487940, 0.7071067811865463515, -0.000000000000000000 ) ) ;
#27875 = CARTESIAN_POINT ( 'NONE',  ( 111.2041937171295558, -6.884901960086285300, -3.975000000000000089 ) ) ;
#27876 = DIRECTION ( 'NONE',  ( -0.6830127018922180770, -0.6830127018922204085, -0.2588190451025213501 ) ) ;
#27877 = ORIENTED_EDGE ( 'NONE', *, *, #141182, .F. ) ;
#27878 = ORIENTED_EDGE ( 'NONE', *, *, #44194, .F. ) ;
#27879 = FACE_OUTER_BOUND ( 'NONE', #66074, .T. ) ;
#27881 = AXIS2_PLACEMENT_3D ( 'NONE', #35160, #79402, #68505 ) ;
#27880 =( NAMED_UNIT ( * ) PLANE_ANGLE_UNIT ( ) SI_UNIT ( $, .RADIAN. ) );
#27882 = VERTEX_POINT ( 'NONE', #81847 ) ;
#27883 = EDGE_CURVE ( 'NONE', #94410, #83442, #126040, .T. ) ;
#27884 = VECTOR ( 'NONE', #23821, 1000.000000000000000 ) ;
#27886 = EDGE_LOOP ( 'NONE', ( #66439, #26342, #139504, #39256 ) ) ;
#27885 = VECTOR ( 'NONE', #11087, 999.9999999999998863 ) ;
#27887 = EDGE_CURVE ( 'NONE', #43549, #59763, #72087, .T. ) ;
#27888 = FACE_OUTER_BOUND ( 'NONE', #98271, .T. ) ;
#27889 = ORIENTED_EDGE ( 'NONE', *, *, #37604, .F. ) ;
#27890 = CARTESIAN_POINT ( 'NONE',  ( 61.32919371712955581, -3.975000000000001865, 6.884901960086284411 ) ) ;
#27891 = CARTESIAN_POINT ( 'NONE',  ( 8.994519915287490619, 28.92564299267944250, 4.000000000000000000 ) ) ;
#27892 = VECTOR ( 'NONE', #46217, 1000.000000000000000 ) ;
#27893 = AXIS2_PLACEMENT_3D ( 'NONE', #92501, #69365, #25834 ) ;
#27894 = CONICAL_SURFACE ( 'NONE', #11950, 2.055000000000000604, 0.9599310885968764806 ) ;
#27895 = AXIS2_PLACEMENT_3D ( 'NONE', #33160, #22213, #77371 ) ;
#27896 = FACE_BOUND ( 'NONE', #52513, .T. ) ;
#27897 = EDGE_CURVE ( 'NONE', #42914, #5341, #94092, .T. ) ;
#27898 = DIRECTION ( 'NONE',  ( 0.000000000000000000, 0.000000000000000000, 1.000000000000000000 ) ) ;
#27899 = FACE_OUTER_BOUND ( 'NONE', #48277, .T. ) ;
#27900 = VECTOR ( 'NONE', #15849, 1000.000000000000000 ) ;
#27902 = VERTEX_POINT ( 'NONE', #86094 ) ;
#27901 = DIRECTION ( 'NONE',  ( -0.7071067811865486830, -0.7071067811865464625, -0.000000000000000000 ) ) ;
#27903 = LINE ( 'NONE', #16276, #6991 ) ;
#27904 = APPLICATION_PROTOCOL_DEFINITION ( 'draft international standard', 'automotive_design', 1998, #60569 ) ;
#27905 = ORIENTED_EDGE ( 'NONE', *, *, #114605, .F. ) ;
#27906 = VERTEX_POINT ( 'NONE', #117958 ) ;
#27907 = CARTESIAN_POINT ( 'NONE',  ( 96.74543019189810877, -5.291415217122918513, -3.055000000000000160 ) ) ;
#27908 = ORIENTED_EDGE ( 'NONE', *, *, #105476, .F. ) ;
#27909 = CARTESIAN_POINT ( 'NONE',  ( -24.18398860626899705, 28.73617430169804265, 5.000000000000000000 ) ) ;
#27910 = VECTOR ( 'NONE', #40490, 999.9999999999998863 ) ;
#27911 = CARTESIAN_POINT ( 'NONE',  ( -25.39999999999996305, 0.000000000000000000, 0.000000000000000000 ) ) ;
#27912 = DIRECTION ( 'NONE',  ( -0.000000000000000000, -0.3543493200069152693, 0.9351131265310292928 ) ) ;
#27913 = AXIS2_PLACEMENT_3D ( 'NONE', #42166, #117532, #97196 ) ;
#27914 = DIRECTION ( 'NONE',  ( 0.000000000000000000, 0.000000000000000000, -1.000000000000000000 ) ) ;
#27915 = EDGE_LOOP ( 'NONE', ( #40340, #77604, #27359, #128660, #31298 ) ) ;
#27916 = LINE ( 'NONE', #48976, #73849 ) ;
#27917 = CONICAL_SURFACE ( 'NONE', #90426, 2.500000000000000888, 0.9599310885968822538 ) ;
#27918 = DIRECTION ( 'NONE',  ( -0.000000000000000000, 0.3543493200069153248, 0.9351131265310292928 ) ) ;
#27919 = CARTESIAN_POINT ( 'NONE',  ( 21.71230993966012690, -21.73547319004781997, 4.999917730833664642 ) ) ;
#27921 = CARTESIAN_POINT ( 'NONE',  ( -27.48921356237309155, -27.52281430457074762, 5.000000000000000000 ) ) ;
#27920 = CARTESIAN_POINT ( 'NONE',  ( -19.05000000000000071, 3.174999999999997158, 4.000000000000000000 ) ) ;
#27922 = VECTOR ( 'NONE', #64040, 1000.000000000000000 ) ;
#27923 = DIRECTION ( 'NONE',  ( 0.7071067811865486830, -0.7071067811865464625, -0.000000000000000000 ) ) ;
#27924 = DIRECTION ( 'NONE',  ( -0.6830127018922180770, -0.6830127018922204085, -0.2588190451025213501 ) ) ;
#27925 = ADVANCED_FACE ( 'NONE', ( #51332 ), #1819, .T. ) ;
#27926 = LINE ( 'NONE', #117752, #134850 ) ;
#27927 = VERTEX_POINT ( 'NONE', #85353 ) ;
#27928 = AXIS2_PLACEMENT_3D ( 'NONE', #99653, #111238, #132333 ) ;
#27929 = CARTESIAN_POINT ( 'NONE',  ( 2.999999999999985345, -16.06887692260765377, 4.000000000000000000 ) ) ;
#27930 = DIRECTION ( 'NONE',  ( -0.7071067811865486830, -0.7071067811865464625, 0.000000000000000000 ) ) ;
#27931 = ORIENTED_EDGE ( 'NONE', *, *, #14153, .F. ) ;
#27932 = ORIENTED_EDGE ( 'NONE', *, *, #63023, .F. ) ;
#27933 = VECTOR ( 'NONE', #49603, 1000.000000000000227 ) ;
#27934 = EDGE_LOOP ( 'NONE', ( #59810, #46466, #132654, #122599 ) ) ;
#27935 = CARTESIAN_POINT ( 'NONE',  ( 44.18793019189811133, 6.110000000000002984, -1.637169565754156730 ) ) ;
#27936 = VERTEX_POINT ( 'NONE', #120842 ) ;
#27937 = ADVANCED_FACE ( 'NONE', ( #32430 ), #33864, .T. ) ;
#27938 = CARTESIAN_POINT ( 'NONE',  ( 11.27497294953710671, 4.461849672132300881, 4.461849672132299105 ) ) ;
#27939 = CARTESIAN_POINT ( 'NONE',  ( -13.40214831053034850, 6.329416083240667845, -31.22042670906152040 ) ) ;
#27940 = EDGE_CURVE ( 'NONE', #18168, #137344, #43308, .T. ) ;
#27941 = ORIENTED_EDGE ( 'NONE', *, *, #113793, .F. ) ;
#27942 = ADVANCED_FACE ( 'NONE', ( #65074 ), #78082, .F. ) ;
#27943 = CARTESIAN_POINT ( 'NONE',  ( -8.816011393731004731, 28.73617430169781173, 5.000000000000000000 ) ) ;
#27945 = ORIENTED_EDGE ( 'NONE', *, *, #113814, .T. ) ;
#27944 = EDGE_CURVE ( 'NONE', #55527, #20152, #126759, .T. ) ;
#27946 = CARTESIAN_POINT ( 'NONE',  ( 18.75860074219783868, 21.72500000000000853, 5.000000000000000000 ) ) ;
#27947 = CIRCLE ( 'NONE', #6996, 2.500000000000000444 ) ;
#27948 = CARTESIAN_POINT ( 'NONE',  ( -34.92500000000001137, -22.22500000000000142, 4.000000000000000000 ) ) ;
#27950 = ORIENTED_EDGE ( 'NONE', *, *, #86033, .F. ) ;
#27949 = CARTESIAN_POINT ( 'NONE',  ( 28.49999999999981171, -4.912538124160708897, 4.000000000000000000 ) ) ;
#27951 = ORIENTED_EDGE ( 'NONE', *, *, #64635, .F. ) ;
#27952 = EDGE_CURVE ( 'NONE', #23925, #133903, #55614, .T. ) ;
#27953 = DIRECTION ( 'NONE',  ( 0.6830127018922181881, 0.6830127018922202975, -0.2588190451025214056 ) ) ;
#27954 = FACE_OUTER_BOUND ( 'NONE', #25742, .T. ) ;
#27955 = ORIENTED_EDGE ( 'NONE', *, *, #125969, .T. ) ;
#27956 = LINE ( 'NONE', #6870, #129192 ) ;
#27957 = ORIENTED_EDGE ( 'NONE', *, *, #89336, .F. ) ;
#27958 = VERTEX_POINT ( 'NONE', #481 ) ;
#27959 = ORIENTED_EDGE ( 'NONE', *, *, #5979, .T. ) ;
#27960 = EDGE_CURVE ( 'NONE', #81752, #112523, #1189, .T. ) ;
#27961 = VERTEX_POINT ( 'NONE', #34569 ) ;
#27962 = PLANE ( 'NONE',  #30873 ) ;
#27963 = AXIS2_PLACEMENT_3D ( 'NONE', #62759, #138892, #128707 ) ;
#27964 = DIRECTION ( 'NONE',  ( 0.000000000000000000, -1.000000000000000000, 0.000000000000000000 ) ) ;
#27965 = EDGE_CURVE ( 'NONE', #46724, #104812, #44020, .T. ) ;
#27966 = FACE_OUTER_BOUND ( 'NONE', #139332, .T. ) ;
#27967 = CARTESIAN_POINT ( 'NONE',  ( -7.140000000000001457, -39.92999999999999261, 18.97874025153853239 ) ) ;
#27968 = ADVANCED_FACE ( 'NONE', ( #88239 ), #10638, .F. ) ;
#27969 = ORIENTED_EDGE ( 'NONE', *, *, #96630, .T. ) ;
#27970 = CARTESIAN_POINT ( 'NONE',  ( 66.18749999999998579, -5.819803920172573974, 5.819803920172573086 ) ) ;
#27971 = ORIENTED_EDGE ( 'NONE', *, *, #35581, .F. ) ;
#27972 = VECTOR ( 'NONE', #7487, 1000.000000000000000 ) ;
#27973 = CARTESIAN_POINT ( 'NONE',  ( -36.48921356237310221, -27.52281430457080802, 5.000000000000000000 ) ) ;
#27974 = EDGE_CURVE ( 'NONE', #358, #90591, #122257, .T. ) ;
#27975 = CARTESIAN_POINT ( 'NONE',  ( 28.99956980810188867, -3.967499999999998028, -6.871911579029511330 ) ) ;
#27976 = PLANE ( 'NONE',  #122672 ) ;
#27977 = DIRECTION ( 'NONE',  ( 0.7071067811865487940, -0.7071067811865463515, 0.000000000000000000 ) ) ;
#27978 = DIRECTION ( 'NONE',  ( 0.000000000000000000, -1.000000000000000000, 0.000000000000000000 ) ) ;
#27979 = ORIENTED_EDGE ( 'NONE', *, *, #65956, .T. ) ;
#27980 = ORIENTED_EDGE ( 'NONE', *, *, #47335, .T. ) ;
#27981 = ORIENTED_EDGE ( 'NONE', *, *, #12367, .F. ) ;
#27982 = CARTESIAN_POINT ( 'NONE',  ( -26.99451991528749417, 28.92564299267956685, 4.000000000000000000 ) ) ;
#27983 = CARTESIAN_POINT ( 'NONE',  ( 34.49999999999975842, 18.43112307739199451, 4.000000000000000000 ) ) ;
#27984 = DIRECTION ( 'NONE',  ( -0.7071067811865486830, 0.7071067811865464625, 0.000000000000000000 ) ) ;
#27985 = CARTESIAN_POINT ( 'NONE',  ( -7.140000000000001457, -35.14999999999999147, -39.50000000000000000 ) ) ;
#27986 = VECTOR ( 'NONE', #111241, 1000.000000000000000 ) ;
#27987 = CARTESIAN_POINT ( 'NONE',  ( 0.01167931549069694576, -50.55966373067267483, -35.89041033429499095 ) ) ;
#27988 = CARTESIAN_POINT ( 'NONE',  ( 75.59959685856478018, -6.109999999999998543, -1.637169565754160727 ) ) ;
#27989 =( BOUNDED_CURVE ( )  B_SPLINE_CURVE ( 3, ( #136800, #126617, #27309, #71561 ),
 .UNSPECIFIED., .F., .F. ) 
 B_SPLINE_CURVE_WITH_KNOTS ( ( 4, 4 ),
 ( 1.964434688349492752, 3.503810798801450854 ),
 .UNSPECIFIED. ) 
 CURVE ( )  GEOMETRIC_REPRESENTATION_ITEM ( )  RATIONAL_B_SPLINE_CURVE ( ( 1.000000000000000000, 0.8120851936182292841, 0.8120851936182292841, 1.000000000000000000 ) ) 
 REPRESENTATION_ITEM ( '' )  );
#27990 = DIRECTION ( 'NONE',  ( -0.7071067811865487940, 0.7071067811865463515, 0.000000000000000000 ) ) ;
#27991 = VECTOR ( 'NONE', #9147, 1000.000000000000000 ) ;
#27992 = VECTOR ( 'NONE', #49139, 1000.000000000000000 ) ;
#27993 = LINE ( 'NONE', #17117, #85450 ) ;
#27994 = PLANE ( 'NONE',  #95812 ) ;
#27995 = DIRECTION ( 'NONE',  ( 0.000000000000000000, -1.000000000000000000, 0.000000000000000000 ) ) ;
#27996 = CARTESIAN_POINT ( 'NONE',  ( -34.42500000000001137, -21.72500000000000142, 0.5000000000000000000 ) ) ;
#27997 = ADVANCED_FACE ( 'NONE', ( #123006 ), #66492, .T. ) ;
#27998 = VERTEX_POINT ( 'NONE', #120102 ) ;
#27999 = VECTOR ( 'NONE', #78442, 1000.000000000000227 ) ;
#28000 = AXIS2_PLACEMENT_3D ( 'NONE', #47494, #36558, #124999 ) ;
#28001 = AXIS2_PLACEMENT_3D ( 'NONE', #4378, #48680, #39974 ) ;
#28002 = CARTESIAN_POINT ( 'NONE',  ( 7.171830600776418763, -2.240707523384260824, 4.000000000000000000 ) ) ;
#28003 = ORIENTED_EDGE ( 'NONE', *, *, #70732, .T. ) ;
#28004 = COLOUR_RGB ( '', 0.72549020, 0.75294118, 0.79215686) ;
#28005 = CARTESIAN_POINT ( 'NONE',  ( 13.49999999999990052, -9.462702396501002866, -9.474982329943548720 ) ) ;
#28007 = ORIENTED_EDGE ( 'NONE', *, *, #63553, .T. ) ;
#28006 = LINE ( 'NONE', #83101, #64966 ) ;
#28008 = FACE_OUTER_BOUND ( 'NONE', #93814, .T. ) ;
#28009 = LINE ( 'NONE', #59245, #40284 ) ;
#28010 = ORIENTED_EDGE ( 'NONE', *, *, #19829, .F. ) ;
#28011 = ORIENTED_EDGE ( 'NONE', *, *, #35662, .F. ) ;
#28012 = PLANE ( 'NONE',  #30419 ) ;
#28013 = VECTOR ( 'NONE', #55687, 1000.000000000000000 ) ;
#28014 = ORIENTED_EDGE ( 'NONE', *, *, #19785, .F. ) ;
#28015 = DIRECTION ( 'NONE',  ( -0.7071067811865486830, -0.7071067811865464625, 0.000000000000000000 ) ) ;
#28016 = EDGE_CURVE ( 'NONE', #93928, #68985, #138626, .T. ) ;
#28017 = CARTESIAN_POINT ( 'NONE',  ( 89.32919371712955581, -3.975000000000001865, 6.884901960086284411 ) ) ;
#28018 = DIRECTION ( 'NONE',  ( 0.6830127018922181881, 0.6830127018922202975, -0.2588190451025214056 ) ) ;
#28019 = DIRECTION ( 'NONE',  ( 0.000000000000000000, 1.000000000000000000, 0.000000000000000000 ) ) ;
#28020 = ORIENTED_EDGE ( 'NONE', *, *, #138465, .F. ) ;
#28021 = VECTOR ( 'NONE', #13250, 1000.000000000000000 ) ;
#28022 = PLANE ( 'NONE',  #14494 ) ;
#28023 = EDGE_CURVE ( 'NONE', #57534, #113103, #131745, .T. ) ;
#28024 = CARTESIAN_POINT ( 'NONE',  ( 21.46453280170069888, 4.202752102959690472E-16, 0.000000000000000000 ) ) ;
#28025 = CARTESIAN_POINT ( 'NONE',  ( 24.35416666666666785, 1.633150327867695095, 6.094999999999988205 ) ) ;
#28026 = DIRECTION ( 'NONE',  ( -0.7071067811865486830, -0.7071067811865464625, 0.000000000000000000 ) ) ;
#28027 = DIRECTION ( 'NONE',  ( -0.7071067811865487940, 0.7071067811865463515, -0.000000000000000000 ) ) ;
#28028 = ORIENTED_EDGE ( 'NONE', *, *, #139767, .F. ) ;
#28029 = VECTOR ( 'NONE', #3782, 999.9999999999998863 ) ;
#28030 = CARTESIAN_POINT ( 'NONE',  ( 45.72502705046288440, 5.819803920172573974, -5.819803920172573086 ) ) ;
#28031 = EDGE_LOOP ( 'NONE', ( #137315, #16031 ) ) ;
#28032 = CIRCLE ( 'NONE', #85862, 2.500000000000000444 ) ;
#28033 = EDGE_CURVE ( 'NONE', #13955, #4136, #141925, .T. ) ;
#28034 = CARTESIAN_POINT ( 'NONE',  ( 82.83376352523144703, 6.110000000000001208, 1.122388791418549305E-15 ) ) ;
#28035 = COLOUR_RGB ( '', 0.09019608, 0.27058824, 0.51372549) ;
#28036 = DIRECTION ( 'NONE',  ( -0.000000000000000000, -0.3543493200069152693, 0.9351131265310292928 ) ) ;
#28037 = CARTESIAN_POINT ( 'NONE',  ( 34.42499999999998295, 19.54139925780185294, 5.000000000000000000 ) ) ;
#28038 = DIRECTION ( 'NONE',  ( 0.000000000000000000, 0.000000000000000000, 1.000000000000000000 ) ) ;
#28039 = VERTEX_POINT ( 'NONE', #109260 ) ;
#28040 = VECTOR ( 'NONE', #29077, 1000.000000000000000 ) ;
#28041 = PLANE ( 'NONE',  #53516 ) ;
#28042 = CARTESIAN_POINT ( 'NONE',  ( 26.75159235450331963, -2.500000000000000000, 3.061616997868384127E-16 ) ) ;
#28043 = CARTESIAN_POINT ( 'NONE',  ( 118.6416937171303516, -2.130196079817768595, -7.950000000005574385 ) ) ;
#28044 = EDGE_CURVE ( 'NONE', #8196, #39664, #54905, .T. ) ;
#28045 = VECTOR ( 'NONE', #60296, 1000.000000000000000 ) ;
#28047 = VERTEX_POINT ( 'NONE', #76669 ) ;
#28046 = DIRECTION ( 'NONE',  ( -0.6830127018922181881, 0.6830127018922202975, -0.2588190451025214056 ) ) ;
#28048 = CARTESIAN_POINT ( 'NONE',  ( -12.20000000000000284, -34.64999999999999147, 17.49210858042622263 ) ) ;
#28049 = CARTESIAN_POINT ( 'NONE',  ( -34.92500000000001137, 2.816654386410402555, 4.500000000000000888 ) ) ;
#28050 = PLANE ( 'NONE',  #70238 ) ;
#28051 = CARTESIAN_POINT ( 'NONE',  ( 59.62500000000000000, -7.950000000000000178, -4.867971026610729436E-16 ) ) ;
#28052 = ORIENTED_EDGE ( 'NONE', *, *, #135880, .F. ) ;
#28053 = EDGE_LOOP ( 'NONE', ( #96545, #12561, #36367, #53262 ) ) ;
#28054 = CARTESIAN_POINT ( 'NONE',  ( 72.62543019189810423, 5.291415217122919401, 3.055000000000002824 ) ) ;
#28055 = AXIS2_PLACEMENT_3D ( 'NONE', #117898, #96159, #120781 ) ;
#28056 = ORIENTED_EDGE ( 'NONE', *, *, #89094, .T. ) ;
#28057 = CARTESIAN_POINT ( 'NONE',  ( 2.000000000000000000, 2.375000000000000000, 1.069999999999998508 ) ) ;
#28058 = AXIS2_PLACEMENT_3D ( 'NONE', #52785, #133252, #132557 ) ;
#28059 = LINE ( 'NONE', #125230, #66539 ) ;
#28060 = CARTESIAN_POINT ( 'NONE',  ( 26.99999999999981526, -1.068876922607795654, 4.000000000000000000 ) ) ;
#28061 = VERTEX_POINT ( 'NONE', #98398 ) ;
#28062 = CARTESIAN_POINT ( 'NONE',  ( 51.29974487139158867, -27.71228299555242103, 4.000000000000000000 ) ) ;
#28063 = DIRECTION ( 'NONE',  ( 0.000000000000000000, 1.000000000000000000, 0.000000000000000000 ) ) ;
#28064 = VERTEX_POINT ( 'NONE', #142618 ) ;
#28065 = EDGE_CURVE ( 'NONE', #83610, #88267, #121554, .T. ) ;
#28066 = CARTESIAN_POINT ( 'NONE',  ( 1.285559789426349520, -0.3484322621842600443, 3.788421920936591025 ) ) ;
#28067 = LINE ( 'NONE', #26637, #47922 ) ;
#28068 = CARTESIAN_POINT ( 'NONE',  ( 36.18398860626899705, 28.73617430169812437, 5.000000000000000000 ) ) ;
#28069 = VECTOR ( 'NONE', #23892, 1000.000000000000000 ) ;
#28070 = EDGE_LOOP ( 'NONE', ( #12400, #80896, #141579, #127451 ) ) ;
#28071 = ORIENTED_EDGE ( 'NONE', *, *, #121803, .F. ) ;
#28072 = EDGE_CURVE ( 'NONE', #47652, #143140, #2624, .T. ) ;
#28073 = EDGE_CURVE ( 'NONE', #42777, #82100, #70097, .T. ) ;
#28074 = FACE_OUTER_BOUND ( 'NONE', #19293, .T. ) ;
#28075 = LINE ( 'NONE', #72342, #64734 ) ;
#28076 = CARTESIAN_POINT ( 'NONE',  ( 20.66840764549667497, 9.139736423841732040E-16, 0.000000000000000000 ) ) ;
#28077 = CARTESIAN_POINT ( 'NONE',  ( -9.328169399223467551, 14.25929247661557397, 4.000000000000000000 ) ) ;
#28078 = AXIS2_PLACEMENT_3D ( 'NONE', #122508, #132729, #78317 ) ;
#28079 = DIRECTION ( 'NONE',  ( 0.3543493200069162685, -0.000000000000000000, -0.9351131265310288487 ) ) ;
#28080 = SHAPE_REPRESENTATION_RELATIONSHIP ( 'NONE' , 'NONE' ,  #39429, #96673 ) ;
#28081 = VERTEX_POINT ( 'NONE', #23682 ) ;
#28082 = ORIENTED_EDGE ( 'NONE', *, *, #57353, .T. ) ;
#28083 = ORIENTED_EDGE ( 'NONE', *, *, #73695, .F. ) ;
#28084 = ORIENTED_EDGE ( 'NONE', *, *, #102283, .T. ) ;
#28085 = CIRCLE ( 'NONE', #116027, 3.000000000000000444 ) ;
#28086 = EDGE_CURVE ( 'NONE', #62473, #72185, #136716, .T. ) ;
#28087 = LINE ( 'NONE', #139003, #61770 ) ;
#28088 = VECTOR ( 'NONE', #122054, 999.9999999999998863 ) ;
#28089 = VECTOR ( 'NONE', #104742, 1000.000000000000114 ) ;
#28090 = ORIENTED_EDGE ( 'NONE', *, *, #64767, .F. ) ;
#28091 = FACE_OUTER_BOUND ( 'NONE', #74963, .T. ) ;
#28092 = CARTESIAN_POINT ( 'NONE',  ( -5.999999999999954703, -9.033600742197647193, 5.000000000000000000 ) ) ;
#28093 = FACE_OUTER_BOUND ( 'NONE', #106651, .T. ) ;
#28094 = CARTESIAN_POINT ( 'NONE',  ( -39.29974487139159578, -27.71228299555233576, 4.000000000000000000 ) ) ;
#28095 = VECTOR ( 'NONE', #130378, 1000.000000000000000 ) ;
#28096 = AXIS2_PLACEMENT_3D ( 'NONE', #142650, #65112, #86850 ) ;
#28097 = AXIS2_PLACEMENT_3D ( 'NONE', #143408, #576, #54298 ) ;
#28098 = CARTESIAN_POINT ( 'NONE',  ( 0.000000000000000000, 0.000000000000000000, 5.000000000000000000 ) ) ;
#28099 = ORIENTED_EDGE ( 'NONE', *, *, #39600, .F. ) ;
#28100 = VECTOR ( 'NONE', #91608, 999.9999999999998863 ) ;
#28101 = CARTESIAN_POINT ( 'NONE',  ( -34.92500000000001137, -10.48753812416038933, 4.000000000000000000 ) ) ;
#28102 = LINE ( 'NONE', #6287, #85935 ) ;
#28103 = ORIENTED_EDGE ( 'NONE', *, *, #749, .F. ) ;
#28104 = PLANE ( 'NONE',  #66629 ) ;
#28105 = VERTEX_POINT ( 'NONE', #59210 ) ;
#28106 = ORIENTED_EDGE ( 'NONE', *, *, #56488, .T. ) ;
#28107 = LINE ( 'NONE', #85319, #108479 ) ;
#28108 = VERTEX_POINT ( 'NONE', #13488 ) ;
#28109 = ORIENTED_EDGE ( 'NONE', *, *, #111355, .T. ) ;
#28110 = EDGE_CURVE ( 'NONE', #23291, #27437, #125872, .T. ) ;
#28111 = PRESENTATION_LAYER_ASSIGNMENT (  '', '', ( #72138 ) ) ;
#28112 = CARTESIAN_POINT ( 'NONE',  ( 77.72959685856477563, -6.110000000000000320, -1.637169565754161393 ) ) ;
#28113 = VERTEX_POINT ( 'NONE', #37427 ) ;
#28114 = LINE ( 'NONE', #61493, #67491 ) ;
#28115 = EDGE_CURVE ( 'NONE', #97839, #54633, #93221, .T. ) ;
#28116 = DIRECTION ( 'NONE',  ( -1.000000000000000000, -0.000000000000000000, -0.000000000000000000 ) ) ;
#28117 = CARTESIAN_POINT ( 'NONE',  ( 111.8545968585647756, -1.637169565754161615, 6.110000000000000320 ) ) ;
#28118 = CARTESIAN_POINT ( 'NONE',  ( 21.29974487139158512, -27.71228299555221142, 4.000000000000000000 ) ) ;
#28119 = VECTOR ( 'NONE', #97428, 1000.000000000000000 ) ;
#28120 = ADVANCED_FACE ( 'NONE', ( #124423 ), #113529, .F. ) ;
#28121 = FACE_OUTER_BOUND ( 'NONE', #55710, .T. ) ;
#28122 = CARTESIAN_POINT ( 'NONE',  ( -25.63753812416080180, 22.22500000000000142, 4.000000000000000000 ) ) ;
#28123 = CARTESIAN_POINT ( 'NONE',  ( 13.49999999999991118, -2.568876922607790103, 4.000000000000000000 ) ) ;
#28124 = EDGE_CURVE ( 'NONE', #21745, #123150, #24393, .T. ) ;
#28125 = ADVANCED_FACE ( 'NONE', ( #79549 ), #70785, .F. ) ;
#28126 = CARTESIAN_POINT ( 'NONE',  ( 35.07919371712955581, 3.975000000000002753, -6.884901960086283523 ) ) ;
#28127 = AXIS2_PLACEMENT_3D ( 'NONE', #5041, #2184, #57355 ) ;
#28128 = DIRECTION ( 'NONE',  ( 0.000000000000000000, 1.000000000000000000, 0.000000000000000000 ) ) ;
#28129 = EDGE_LOOP ( 'NONE', ( #47210, #5079, #17635, #23284 ) ) ;
#28130 = VECTOR ( 'NONE', #68058, 1000.000000000000000 ) ;
#28131 = ORIENTED_EDGE ( 'NONE', *, *, #45682, .T. ) ;
#28132 =( GEOMETRIC_REPRESENTATION_CONTEXT ( 3 ) GLOBAL_UNCERTAINTY_ASSIGNED_CONTEXT ( ( #134475 ) ) GLOBAL_UNIT_ASSIGNED_CONTEXT ( ( #45802, #99411, #89282 ) ) REPRESENTATION_CONTEXT ( 'NONE', 'WORKASPACE' ) );
#28133 = VERTEX_POINT ( 'NONE', #14231 ) ;
#28134 = CARTESIAN_POINT ( 'NONE',  ( 14.99999999999989875, 17.58746187583906462, 4.000000000000000000 ) ) ;
#28135 = ORIENTED_EDGE ( 'NONE', *, *, #135299, .T. ) ;
#28136 = VECTOR ( 'NONE', #91333, 1000.000000000000227 ) ;
#28137 = DIRECTION ( 'NONE',  ( 0.3543493200069162685, -0.000000000000000000, -0.9351131265310288487 ) ) ;
#28138 = CARTESIAN_POINT ( 'NONE',  ( 113.7291666666666572, 7.950000000000001954, -2.130196079827421762 ) ) ;
#28139 = EDGE_CURVE ( 'NONE', #88966, #5504, #9502, .T. ) ;
#28140 = VECTOR ( 'NONE', #142498, 1000.000000000000227 ) ;
#28141 = DIRECTION ( 'NONE',  ( -1.000000000000000000, 0.000000000000000000, -0.000000000000000000 ) ) ;
#28142 = ADVANCED_FACE ( 'NONE', ( #92489 ), #46926, .F. ) ;
#28143 = LINE ( 'NONE', #122823, #106497 ) ;
#28144 =( REPRESENTATION_RELATIONSHIP ('NONE','NONE', #69070, #9754 ) REPRESENTATION_RELATIONSHIP_WITH_TRANSFORMATION ( #42377 )SHAPE_REPRESENTATION_RELATIONSHIP( ) );
#28145 = EDGE_LOOP ( 'NONE', ( #100535, #27517, #75599, #56640 ) ) ;
#28146 = ORIENTED_EDGE ( 'NONE', *, *, #123833, .F. ) ;
#28147 = ADVANCED_FACE ( 'NONE', ( #4010 ), #48289, .F. ) ;
#28148 = CARTESIAN_POINT ( 'NONE',  ( 4.353736474768552966, -5.808823158059035485, -5.808823158059033709 ) ) ;
#28149 = DIRECTION ( 'NONE',  ( 0.7071067811865486830, -0.7071067811865464625, -0.000000000000000000 ) ) ;
#28150 = DIRECTION ( 'NONE',  ( -0.7071067811865487940, 0.7071067811865463515, -0.000000000000000000 ) ) ;
#28151 = DIRECTION ( 'NONE',  ( 0.6830127018922181881, 0.6830127018922202975, -0.2588190451025214056 ) ) ;
#28152 = ORIENTED_EDGE ( 'NONE', *, *, #123929, .F. ) ;
#28153 = EDGE_LOOP ( 'NONE', ( #62439, #19044, #25780, #142894 ) ) ;
#28154 = VECTOR ( 'NONE', #53745, 1000.000000000000000 ) ;
#28155 = ORIENTED_EDGE ( 'NONE', *, *, #64017, .T. ) ;
#28156 = LINE ( 'NONE', #127455, #107418 ) ;
#28157 = FACE_OUTER_BOUND ( 'NONE', #96031, .T. ) ;
#28158 = ADVANCED_FACE ( 'NONE', ( #114932 ), #90361, .T. ) ;
#28159 = CARTESIAN_POINT ( 'NONE',  ( 26.99451991528749417, 28.92564299267956685, 4.000000000000000000 ) ) ;
#28160 = AXIS2_PLACEMENT_3D ( 'NONE', #76149, #120314, #139997 ) ;
#28161 = PLANE ( 'NONE',  #106407 ) ;
#28162 = DIRECTION ( 'NONE',  ( 0.6830127018922181881, 0.6830127018922202975, -0.2588190451025214056 ) ) ;
#28163 = LINE ( 'NONE', #72424, #27722 ) ;
#28164 = CARTESIAN_POINT ( 'NONE',  ( 11.99999999999991651, 19.55218569542897100, 5.000000000000000000 ) ) ;
#28165 = CARTESIAN_POINT ( 'NONE',  ( 3.000000000000000000, -47.62213595499959951, 36.92500000000000426 ) ) ;
#28166 = ORIENTED_EDGE ( 'NONE', *, *, #60540, .T. ) ;
#28167 = DIRECTION ( 'NONE',  ( 0.000000000000000000, 0.6666666666666631880, -0.7453559924999331177 ) ) ;
#28168 = EDGE_CURVE ( 'NONE', #75175, #59824, #15610, .T. ) ;
#28169 = AXIS2_PLACEMENT_3D ( 'NONE', #73987, #8669, #7984 ) ;
#28170 = CARTESIAN_POINT ( 'NONE',  ( -9.812461875839401770, -22.22500000000000142, 4.000000000000000000 ) ) ;
#28171 = ORIENTED_EDGE ( 'NONE', *, *, #10881, .F. ) ;
#28172 = DIRECTION ( 'NONE',  ( -0.7071067811865487940, 0.7071067811865463515, 0.000000000000000000 ) ) ;
#28174 = ORIENTED_EDGE ( 'NONE', *, *, #143347, .T. ) ;
#28173 = CARTESIAN_POINT ( 'NONE',  ( 53.41963127661841781, -48.51451318982912397, -38.21513923099966092 ) ) ;
#28175 = DIRECTION ( 'NONE',  ( 0.000000000000000000, -1.000000000000000000, 0.000000000000000000 ) ) ;
#28176 = EDGE_CURVE ( 'NONE', #49695, #68309, #91786, .T. ) ;
#28178 = EDGE_CURVE ( 'NONE', #139670, #70176, #59897, .T. ) ;
#28177 = CARTESIAN_POINT ( 'NONE',  ( 105.8541666666666714, -2.130196079827445299, -7.949999999999990408 ) ) ;
#28180 = EDGE_LOOP ( 'NONE', ( #66642, #76843, #57562, #129584 ) ) ;
#28179 = VECTOR ( 'NONE', #94518, 1000.000000000000000 ) ;
#28181 = FACE_OUTER_BOUND ( 'NONE', #75709, .T. ) ;
#28182 = ORIENTED_EDGE ( 'NONE', *, *, #13763, .T. ) ;
#28183 =( BOUNDED_CURVE ( )  B_SPLINE_CURVE ( 3, ( #12861, #76004, #142689, #86889 ),
 .UNSPECIFIED., .F., .T. ) 
 B_SPLINE_CURVE_WITH_KNOTS ( ( 4, 4 ),
 ( 4.350170835173036821, 4.500739107949268458 ),
 .UNSPECIFIED. ) 
 CURVE ( )  GEOMETRIC_REPRESENTATION_ITEM ( )  RATIONAL_B_SPLINE_CURVE ( ( 1.000000000000000000, 0.9981116584018945304, 0.9981116584018945304, 1.000000000000000000 ) ) 
 REPRESENTATION_ITEM ( '' )  );
#28184 = DIRECTION ( 'NONE',  ( -0.6830127018922180770, -0.6830127018922204085, -0.2588190451025213501 ) ) ;
#28185 = EDGE_CURVE ( 'NONE', #25281, #50352, #112137, .T. ) ;
#28186 = CARTESIAN_POINT ( 'NONE',  ( 117.3291937171295558, -3.975000000000001865, 6.884901960086284411 ) ) ;
#28187 = DIRECTION ( 'NONE',  ( 0.6830127018922180770, -0.6830127018922204085, -0.2588190451025213501 ) ) ;
#28188 = FACE_OUTER_BOUND ( 'NONE', #61012, .T. ) ;
#28189 = CARTESIAN_POINT ( 'NONE',  ( -15.48921356237309510, -27.52281430457066236, 5.000000000000000000 ) ) ;
#28190 = CARTESIAN_POINT ( 'NONE',  ( 39.48921356237310221, -27.52281430457082934, 5.000000000000000000 ) ) ;
#28191 = PLANE ( 'NONE',  #43675 ) ;
#28192 = CARTESIAN_POINT ( 'NONE',  ( 29.87456980810189222, 6.871911579029510442, -3.967499999999998916 ) ) ;
#28193 = CARTESIAN_POINT ( 'NONE',  ( 10.33290314143522082, -3.967499999999994476, 6.871911579029513106 ) ) ;
#28194 = LINE ( 'NONE', #141792, #129228 ) ;
#28195 = AXIS2_PLACEMENT_3D ( 'NONE', #120673, #131583, #107667 ) ;
#28196 = AXIS2_PLACEMENT_3D ( 'NONE', #109603, #98031, #131368 ) ;
#28197 = CARTESIAN_POINT ( 'NONE',  ( 7.226741607178295723, -11.24070752338416135, 18.24660765846983779 ) ) ;
#28198 = DIRECTION ( 'NONE',  ( 0.7071067811865487940, 0.7071067811865463515, 0.000000000000000000 ) ) ;
#28199 = ORIENTED_EDGE ( 'NONE', *, *, #49349, .T. ) ;
#28200 = EDGE_LOOP ( 'NONE', ( #11947, #62410, #114500 ) ) ;
#28201 = VECTOR ( 'NONE', #60057, 999.9999999999998863 ) ;
#28202 = CARTESIAN_POINT ( 'NONE',  ( 78.58333333333334281, 6.884901960086290629, -3.974999999999994316 ) ) ;
#28203 = VECTOR ( 'NONE', #116164, 999.9999999999998863 ) ;
#28204 = CARTESIAN_POINT ( 'NONE',  ( 11.15159235450332176, 2.500000000000001776, 0.000000000000000000 ) ) ;
#28205 = ORIENTED_EDGE ( 'NONE', *, *, #36474, .T. ) ;
#28206 = CARTESIAN_POINT ( 'NONE',  ( 22.94163961620376924, -6.094999999999989093, 1.633150327867691542 ) ) ;
#28207 = VECTOR ( 'NONE', #102742, 999.9999999999998863 ) ;
#28208 = CIRCLE ( 'NONE', #86160, 2.999999999999999112 ) ;
#28209 = COLOUR_RGB ( '', 0.08235294, 0.09019608, 0.10196078) ;
#28210 = DIRECTION ( 'NONE',  ( 0.7071067811865487940, -0.7071067811865463515, 0.000000000000000000 ) ) ;
#28211 = EDGE_LOOP ( 'NONE', ( #110566, #41433, #55263, #101001 ) ) ;
#28212 = VECTOR ( 'NONE', #99322, 1000.000000000000000 ) ;
#28213 = CARTESIAN_POINT ( 'NONE',  ( -36.29974487139159578, -27.71228299555231445, 4.000000000000000000 ) ) ;
#28214 = CARTESIAN_POINT ( 'NONE',  ( 48.29974487139158867, -27.71228299555239971, 4.000000000000000000 ) ) ;
#28215 = DIRECTION ( 'NONE',  ( 0.7071067811865487940, 0.7071067811865463515, 0.000000000000000000 ) ) ;
#28216 = CARTESIAN_POINT ( 'NONE',  ( 55.32809448528696095, -52.14999999999999147, -41.05261164187028555 ) ) ;
#28217 = DIRECTION ( 'NONE',  ( -0.7071067811865486830, -0.7071067811865464625, 0.000000000000000000 ) ) ;
#28218 = LINE ( 'NONE', #83316, #112343 ) ;
#28219 = STYLED_ITEM ( 'NONE', ( #108786 ), #142006 ) ;
#28220 = SURFACE_SIDE_STYLE ('',( #17327 ) ) ;
#28221 = CARTESIAN_POINT ( 'NONE',  ( -24.48921356237309510, -27.52281430457072631, 5.000000000000000000 ) ) ;
#28222 = LINE ( 'NONE', #5716, #95633 ) ;
#28223 = DIRECTION ( 'NONE',  ( -0.7071067811865486830, -0.7071067811865463515, 0.000000000000000000 ) ) ;
#28224 = DIRECTION ( 'NONE',  ( 0.7071067811865487940, 0.7071067811865463515, 0.000000000000000000 ) ) ;
#28225 = CARTESIAN_POINT ( 'NONE',  ( 55.86145213702157264, -48.75494892434544880, 38.51155878621108286 ) ) ;
#28226 = ORIENTED_EDGE ( 'NONE', *, *, #87652, .T. ) ;
#28227 = ORIENTED_EDGE ( 'NONE', *, *, #94146, .T. ) ;
#28228 = CARTESIAN_POINT ( 'NONE',  ( 102.5212635252314328, -4.472830434245839371, -4.472830434245840259 ) ) ;
#28229 = EDGE_LOOP ( 'NONE', ( #100723, #102779, #53041, #20585 ) ) ;
#28230 = CARTESIAN_POINT ( 'NONE',  ( 122.6835989386367345, -43.14999999999999147, 34.92499999999998295 ) ) ;
#28231 = CARTESIAN_POINT ( 'NONE',  ( -13.49999999999988987, 19.08746187583904330, 4.000000000000000000 ) ) ;
#28232 = ORIENTED_EDGE ( 'NONE', *, *, #123395, .F. ) ;
#28233 = CARTESIAN_POINT ( 'NONE',  ( -34.82816939922328459, -8.240707523384189770, 4.000000000000000000 ) ) ;
#28234 = PLANE ( 'NONE',  #92870 ) ;
#28235 = AXIS2_PLACEMENT_3D ( 'NONE', #113668, #15056, #25958 ) ;
#28236 = AXIS2_PLACEMENT_3D ( 'NONE', #141663, #1645, #101706 ) ;
#28237 = CARTESIAN_POINT ( 'NONE',  ( 106.0787635252314516, -7.482591942790325086E-16, 6.109999999999998543 ) ) ;
#28238 = VERTEX_POINT ( 'NONE', #35309 ) ;
#28239 = CONICAL_SURFACE ( 'NONE', #139406, 2.055000000000001048, 0.9599310885968758145 ) ;
#28240 = CARTESIAN_POINT ( 'NONE',  ( 5.700255128608413102, -27.71228299555201957, 4.000000000000000000 ) ) ;
#28241 = ORIENTED_EDGE ( 'NONE', *, *, #23223, .T. ) ;
#28242 = DIRECTION ( 'NONE',  ( 1.000000000000000000, 1.224606353822377258E-16, 0.000000000000000000 ) ) ;
#28243 = LINE ( 'NONE', #95625, #127943 ) ;
#28244 = VECTOR ( 'NONE', #93657, 1000.000000000000000 ) ;
#28245 = DIRECTION ( 'NONE',  ( -0.7071067811865486830, -0.7071067811865464625, 0.000000000000000000 ) ) ;
#28246 = CARTESIAN_POINT ( 'NONE',  ( 16.36246187583891754, 22.22499999999999432, 4.000000000000000000 ) ) ;
#28247 = ORIENTED_EDGE ( 'NONE', *, *, #67840, .F. ) ;
#28248 = ORIENTED_EDGE ( 'NONE', *, *, #49978, .F. ) ;
#28249 = EDGE_CURVE ( 'NONE', #94548, #64904, #40991, .T. ) ;
#28250 = ORIENTED_EDGE ( 'NONE', *, *, #49810, .F. ) ;
#28251 = DIRECTION ( 'NONE',  ( -1.000000000000000000, 0.000000000000000000, 0.000000000000000000 ) ) ;
#28252 = EDGE_CURVE ( 'NONE', #94631, #103858, #28704, .T. ) ;
#28253 = FACE_OUTER_BOUND ( 'NONE', #90726, .T. ) ;
#28254 = CARTESIAN_POINT ( 'NONE',  ( 12.31706980810188590, -2.126176841940956130, 7.934999999999990727 ) ) ;
#28255 =( GEOMETRIC_REPRESENTATION_CONTEXT ( 3 ) GLOBAL_UNCERTAINTY_ASSIGNED_CONTEXT ( ( #133388 ) ) GLOBAL_UNIT_ASSIGNED_CONTEXT ( ( #5955, #94417, #82860 ) ) REPRESENTATION_CONTEXT ( 'NONE', 'WORKASPACE' ) );
#28256 = LINE ( 'NONE', #85460, #20124 ) ;
#28257 = DIRECTION ( 'NONE',  ( -0.3543493200069162685, -0.000000000000000000, -0.9351131265310288487 ) ) ;
#28258 = VERTEX_POINT ( 'NONE', #116408 ) ;
#28260 = ORIENTED_EDGE ( 'NONE', *, *, #137131, .T. ) ;
#28259 = EDGE_CURVE ( 'NONE', #117324, #53860, #96750, .T. ) ;
#28261 = CARTESIAN_POINT ( 'NONE',  ( 20.99999999999985789, -19.44781430457063465, 5.000000000000000000 ) ) ;
#28262 = ORIENTED_EDGE ( 'NONE', *, *, #106005, .F. ) ;
#28263 = VERTEX_POINT ( 'NONE', #63491 ) ;
#28264 = VECTOR ( 'NONE', #68737, 1000.000000000000114 ) ;
#28265 = AXIS2_PLACEMENT_3D ( 'NONE', #97717, #141969, #17978 ) ;
#28266 = CARTESIAN_POINT ( 'NONE',  ( 110.4537635252314516, -6.109999999999998543, -3.741295971395162543E-16 ) ) ;
#28267 = EDGE_CURVE ( 'NONE', #28405, #81467, #72948, .T. ) ;
#28268 = FACE_OUTER_BOUND ( 'NONE', #50792, .T. ) ;
#28269 = CARTESIAN_POINT ( 'NONE',  ( -21.18398860626899349, 28.73617430169802134, 5.000000000000000000 ) ) ;
#28270 = EDGE_LOOP ( 'NONE', ( #47949, #72683, #14178, #39552 ) ) ;
#28271 = CARTESIAN_POINT ( 'NONE',  ( 21.42327845806341102, 11.25929247661560240, 17.85071094206579545 ) ) ;
#28272 = CARTESIAN_POINT ( 'NONE',  ( -20.70025512860841133, -27.71228299555191654, 4.000000000000000000 ) ) ;
#28273 = DIRECTION ( 'NONE',  ( -0.7071067811865486830, 0.7071067811865464625, 0.000000000000000000 ) ) ;
#28274 = EDGE_CURVE ( 'NONE', #44583, #68847, #7619, .T. ) ;
#28275 = ADVANCED_FACE ( 'NONE', ( #128022 ), #94632, .F. ) ;
#28276 = DIRECTION ( 'NONE',  ( 0.6830127018922181881, 0.6830127018922202975, -0.2588190451025214056 ) ) ;
#28277 = VERTEX_POINT ( 'NONE', #40304 ) ;
#28278 = LINE ( 'NONE', #49344, #118197 ) ;
#28279 = CARTESIAN_POINT ( 'NONE',  ( 37.02083333333332149, 7.949999999999998401, 2.130196079827431532 ) ) ;
#28280 = EDGE_LOOP ( 'NONE', ( #104922, #111019, #132005, #45244 ) ) ;
#28281 = DIRECTION ( 'NONE',  ( -0.5735764363510499342, -0.8191520442889891340, 0.000000000000000000 ) ) ;
#28282 = CARTESIAN_POINT ( 'NONE',  ( -5.510786437626906675, -27.52281430457051314, 5.000000000000000000 ) ) ;
#28283 = DIRECTION ( 'NONE',  ( 0.7071067811865486830, -0.7071067811865464625, -0.000000000000000000 ) ) ;
#28284 = VERTEX_POINT ( 'NONE', #107659 ) ;
#28285 = CARTESIAN_POINT ( 'NONE',  ( -8.671830600776409881, 17.25929247661554911, 4.000000000000000000 ) ) ;
#28286 = VERTEX_POINT ( 'NONE', #5472 ) ;
#28287 = ORIENTED_EDGE ( 'NONE', *, *, #98516, .F. ) ;
#28288 = AXIS2_PLACEMENT_3D ( 'NONE', #93980, #138215, #38900 ) ;
#28289 = ORIENTED_EDGE ( 'NONE', *, *, #111727, .F. ) ;
#28290 = CARTESIAN_POINT ( 'NONE',  ( 33.30793019189810877, -6.109999999999998543, 1.637169565754158507 ) ) ;
#28291 = ORIENTED_EDGE ( 'NONE', *, *, #89180, .T. ) ;
#28292 = CARTESIAN_POINT ( 'NONE',  ( -31.49999999999977973, 6.052185695429109558, 5.000000000000000000 ) ) ;
#28293 = DIRECTION ( 'NONE',  ( -0.3543493200069162685, -0.000000000000000000, -0.9351131265310288487 ) ) ;
#28294 = LINE ( 'NONE', #105813, #84496 ) ;
#28295 = ADVANCED_FACE ( 'NONE', ( #17097 ), #50447, .F. ) ;
#28296 = CARTESIAN_POINT ( 'NONE',  ( -33.69326993309579166, -3.740707523384244837, 12.88036043432875388 ) ) ;
#28297 = VECTOR ( 'NONE', #112676, 1000.000000000000000 ) ;
#28298 = VECTOR ( 'NONE', #98229, 999.9999999999998863 ) ;
#28299 = VECTOR ( 'NONE', #128976, 999.9999999999998863 ) ;
#28300 = LINE ( 'NONE', #52867, #16846 ) ;
#28301 = ADVANCED_FACE ( 'NONE', ( #106207 ), #8317, .F. ) ;
#28303 = EDGE_CURVE ( 'NONE', #113567, #72906, #37009, .T. ) ;
#28302 = VECTOR ( 'NONE', #124408, 1000.000000000000000 ) ;
#28304 = AXIS2_PLACEMENT_3D ( 'NONE', #92804, #81978, #3620 ) ;
#28305 = PLANE ( 'NONE',  #129338 ) ;
#28306 = CARTESIAN_POINT ( 'NONE',  ( -34.47516574401892342, -11.97193265888405200, 4.998110765256834398 ) ) ;
#28307 = CARTESIAN_POINT ( 'NONE',  ( -30.00000000000000355, -2.375000000000000000, 4.319999999999998508 ) ) ;
#28308 = VERTEX_POINT ( 'NONE', #117794 ) ;
#28309 = ORIENTED_EDGE ( 'NONE', *, *, #103114, .T. ) ;
#28310 = VECTOR ( 'NONE', #30154, 1000.000000000000000 ) ;
#28311 = EDGE_LOOP ( 'NONE', ( #130483, #74611, #131634, #54374 ) ) ;
#28312 = VECTOR ( 'NONE', #32860, 1000.000000000000000 ) ;
#28313 = VERTEX_POINT ( 'NONE', #39580 ) ;
#28314 = VECTOR ( 'NONE', #140230, 1000.000000000000000 ) ;
#28315 = CARTESIAN_POINT ( 'NONE',  ( -0.8730705227619277586, 0.9948348601054731732, 3.904059355167917911 ) ) ;
#28316 = VERTEX_POINT ( 'NONE', #83816 ) ;
#28317 = EDGE_CURVE ( 'NONE', #98487, #27213, #18482, .T. ) ;
#28318 = VERTEX_POINT ( 'NONE', #17774 ) ;
#28319 = CARTESIAN_POINT ( 'NONE',  ( -55.65468426143998215, -27.55040120718572894, 16.07347811296898854 ) ) ;
#28320 = DIRECTION ( 'NONE',  ( -1.000000000000000000, -0.000000000000000000, -0.000000000000000000 ) ) ;
#28321 = EDGE_CURVE ( 'NONE', #48577, #35756, #62051, .T. ) ;
#28322 = EDGE_CURVE ( 'NONE', #43125, #26437, #118537, .T. ) ;
#28323 = DIRECTION ( 'NONE',  ( 0.000000000000000000, -1.000000000000000000, 0.000000000000000000 ) ) ;
#28324 = ORIENTED_EDGE ( 'NONE', *, *, #73067, .T. ) ;
#28325 = DIRECTION ( 'NONE',  ( -0.000000000000000000, -0.3543493200069152693, 0.9351131265310292928 ) ) ;
#28326 = ORIENTED_EDGE ( 'NONE', *, *, #116500, .F. ) ;
#28327 = CARTESIAN_POINT ( 'NONE',  ( 34.75611968250419181, 20.81293425470717651, 4.955485411084878500 ) ) ;
#28328 = CARTESIAN_POINT ( 'NONE',  ( 20.67906569311139009, 2.055000000000001048, 2.516649172247811554E-16 ) ) ;
#28329 = CARTESIAN_POINT ( 'NONE',  ( 5.462903141435219823, -3.967499999999994476, 6.871911579029513106 ) ) ;
#28330 = ORIENTED_EDGE ( 'NONE', *, *, #63803, .T. ) ;
#28332 = DIRECTION ( 'NONE',  ( -1.000000000000000000, -1.224606353822377258E-16, -0.000000000000000000 ) ) ;
#28331 = CARTESIAN_POINT ( 'NONE',  ( 103.0162635252314374, -4.472830434245839371, 4.472830434245839371 ) ) ;
#28333 = EDGE_CURVE ( 'NONE', #24066, #59015, #27236, .T. ) ;
#28334 = PLANE ( 'NONE',  #113656 ) ;
#28335 = ORIENTED_EDGE ( 'NONE', *, *, #100798, .F. ) ;
#28336 = EDGE_LOOP ( 'NONE', ( #16042, #86527, #66773 ) ) ;
#28337 = SURFACE_STYLE_FILL_AREA ( #113900 ) ;
#28338 = ORIENTED_EDGE ( 'NONE', *, *, #131964, .F. ) ;
#28339 = LINE ( 'NONE', #30473, #129794 ) ;
#28340 = EDGE_CURVE ( 'NONE', #132946, #488, #67033, .T. ) ;
#28341 = CYLINDRICAL_SURFACE ( 'NONE', #70525, 0.5000000000000004441 ) ;
#28342 = ORIENTED_EDGE ( 'NONE', *, *, #93125, .T. ) ;
#28343 = VECTOR ( 'NONE', #125829, 1000.000000000000000 ) ;
#28344 = DIRECTION ( 'NONE',  ( 0.000000000000000000, 1.000000000000000000, -0.000000000000000000 ) ) ;
#28345 = AXIS2_PLACEMENT_3D ( 'NONE', #78788, #11332, #12074 ) ;
#28346 = CARTESIAN_POINT ( 'NONE',  ( -34.42500000000001137, 14.97718569542927014, 5.000000000000000000 ) ) ;
#28347 = DIRECTION ( 'NONE',  ( 0.7071067811865486830, -0.7071067811865464625, -0.000000000000000000 ) ) ;
#28348 = VERTEX_POINT ( 'NONE', #55445 ) ;
#28349 = CARTESIAN_POINT ( 'NONE',  ( -2.999999999999981792, 7.588810512006209485, -3.013526669885219889 ) ) ;
#28350 = MECHANICAL_DESIGN_GEOMETRIC_PRESENTATION_REPRESENTATION (  '', ( #65415 ), #127912 ) ;
#28351 = DIRECTION ( 'NONE',  ( 0.7071067811865487940, 0.7071067811865463515, 0.000000000000000000 ) ) ;
#28352 = ORIENTED_EDGE ( 'NONE', *, *, #139445, .T. ) ;
#28354 = ORIENTED_EDGE ( 'NONE', *, *, #71521, .T. ) ;
#28353 = PLANE ( 'NONE',  #57944 ) ;
#28355 = ORIENTED_EDGE ( 'NONE', *, *, #57916, .F. ) ;
#28356 = CARTESIAN_POINT ( 'NONE',  ( -11.99999999999992006, 14.58746187583910192, 4.000000000000000000 ) ) ;
#28357 = CARTESIAN_POINT ( 'NONE',  ( 21.76000000000000156, 2.055000000000001492, 2.516649172247811554E-16 ) ) ;
#28358 = EDGE_LOOP ( 'NONE', ( #97553, #84936, #78559, #94393 ) ) ;
#28359 = CARTESIAN_POINT ( 'NONE',  ( 16.27785539607886633, 4.584330080086930965E-16, 0.000000000000000000 ) ) ;
#28360 = ADVANCED_FACE ( 'NONE', ( #20645 ), #111217, .F. ) ;
#28361 = FACE_OUTER_BOUND ( 'NONE', #58845, .T. ) ;
#28362 = ADVANCED_FACE ( 'NONE', ( #108339 ), #88797, .F. ) ;
#28363 = CARTESIAN_POINT ( 'NONE',  ( -34.45011844616454511, 18.00230414159377190, 5.000000000000000888 ) ) ;
#28364 = ORIENTED_EDGE ( 'NONE', *, *, #37969, .F. ) ;
#28365 = CARTESIAN_POINT ( 'NONE',  ( 1.353980332882009252, 4.584330080086930965E-16, 0.000000000000000000 ) ) ;
#28366 = DIRECTION ( 'NONE',  ( 0.000000000000000000, 0.2631995976047524777, 0.9647414015272156584 ) ) ;
#28367 = CARTESIAN_POINT ( 'NONE',  ( 68.99451991528748351, 28.92564299267986172, 4.000000000000000000 ) ) ;
#28368 = CARTESIAN_POINT ( 'NONE',  ( 24.29974487139158867, -27.71228299555223273, 4.000000000000000000 ) ) ;
#28369 = AXIS2_PLACEMENT_3D ( 'NONE', #30013, #85824, #74254 ) ;
#28370 = CARTESIAN_POINT ( 'NONE',  ( 26.99999999999981526, -0.03360074219773204196, 5.000000000000000000 ) ) ;
#28371 = CARTESIAN_POINT ( 'NONE',  ( -57.48921356237308800, -27.52281430457095368, 5.000000000000000000 ) ) ;
#28372 = VECTOR ( 'NONE', #31598, 1000.000000000000000 ) ;
#28373 = FACE_OUTER_BOUND ( 'NONE', #35882, .T. ) ;
#28374 = EDGE_CURVE ( 'NONE', #10908, #129366, #51853, .T. ) ;
#28375 = FACE_OUTER_BOUND ( 'NONE', #101865, .T. ) ;
#28376 = PLANE ( 'NONE',  #59327 ) ;
#28377 = ORIENTED_EDGE ( 'NONE', *, *, #11876, .F. ) ;
#28378 = ORIENTED_EDGE ( 'NONE', *, *, #64111, .T. ) ;
#28379 = ORIENTED_EDGE ( 'NONE', *, *, #39957, .F. ) ;
#28380 = CARTESIAN_POINT ( 'NONE',  ( 112.5624999999999858, -5.819803920172572198, -5.819803920172573086 ) ) ;
#28381 = ORIENTED_EDGE ( 'NONE', *, *, #10425, .T. ) ;
#28382 = EDGE_LOOP ( 'NONE', ( #117678, #141279 ) ) ;
#28383 = VERTEX_POINT ( 'NONE', #130155 ) ;
#28384 = CARTESIAN_POINT ( 'NONE',  ( -48.48921356237309510, -27.52281430457089328, 5.000000000000000000 ) ) ;
#28385 = CIRCLE ( 'NONE', #60805, 2.500000000000000888 ) ;
#28386 = ORIENTED_EDGE ( 'NONE', *, *, #72395, .F. ) ;
#28387 = DIRECTION ( 'NONE',  ( -1.000000000000000000, -1.224606353822377258E-16, -0.000000000000000000 ) ) ;
#28388 = SURFACE_SIDE_STYLE ('',( #127704 ) ) ;
#28389 = DIRECTION ( 'NONE',  ( -0.6830127018922180770, -0.6830127018922204085, -0.2588190451025213501 ) ) ;
#28390 = CARTESIAN_POINT ( 'NONE',  ( 31.49999999999977263, 16.18958161055405043, -11.56426086740804138 ) ) ;
#28391 = CARTESIAN_POINT ( 'NONE',  ( 110.5420968585647756, 5.291415217122923842, -3.054999999999996163 ) ) ;
#28392 = ORIENTED_EDGE ( 'NONE', *, *, #131571, .T. ) ;
#28393 = CARTESIAN_POINT ( 'NONE',  ( -10.95743729084448859, 8.751477814956837520, -29.75791556614341360 ) ) ;
#28394 = LINE ( 'NONE', #17495, #5299 ) ;
#28396 = VECTOR ( 'NONE', #13033, 999.9999999999998863 ) ;
#28395 = CARTESIAN_POINT ( 'NONE',  ( 24.39999999999999858, -7.600000000000061817, 34.92499999999998295 ) ) ;
#28397 = SURFACE_STYLE_USAGE ( .BOTH. , #127714 ) ;
#28398 = DIRECTION ( 'NONE',  ( -1.000000000000000000, -1.224606353822377258E-16, -0.000000000000000000 ) ) ;
#28399 = CARTESIAN_POINT ( 'NONE',  ( 40.76669371712956291, -7.949999999999999289, 2.130196079827424427 ) ) ;
#28400 = CARTESIAN_POINT ( 'NONE',  ( -27.09843580608220392, 11.25929247661560950, 10.79108189686400721 ) ) ;
#28401 = DIRECTION ( 'NONE',  ( -0.3543493200069162685, -0.000000000000000000, -0.9351131265310288487 ) ) ;
#28402 = ORIENTED_EDGE ( 'NONE', *, *, #69563, .F. ) ;
#28403 = VERTEX_POINT ( 'NONE', #44606 ) ;
#28404 = CARTESIAN_POINT ( 'NONE',  ( 25.20833333333333215, -3.974999999999999201, -6.884901960086287964 ) ) ;
#28405 = VERTEX_POINT ( 'NONE', #98918 ) ;
#28406 = CARTESIAN_POINT ( 'NONE',  ( -54.18398860626899705, 28.73617430169825226, 5.000000000000000000 ) ) ;
#28407 = EDGE_CURVE ( 'NONE', #118585, #131755, #32262, .T. ) ;
#28408 = PLANE ( 'NONE',  #15402 ) ;
#28409 = VECTOR ( 'NONE', #127094, 999.9999999999998863 ) ;
#28410 = VECTOR ( 'NONE', #125970, 999.9999999999998863 ) ;
#28411 = DIRECTION ( 'NONE',  ( 0.7071067811865487940, -0.7071067811865463515, 0.000000000000000000 ) ) ;
#28412 = CARTESIAN_POINT ( 'NONE',  ( -31.92499999999997584, -22.26999999999999247, -37.00000000000000000 ) ) ;
#28413 = AXIS2_PLACEMENT_3D ( 'NONE', #137440, #27953, #38131 ) ;
#28414 = FILL_AREA_STYLE_COLOUR ( '', #62848 ) ;
#28416 = VECTOR ( 'NONE', #60412, 1000.000000000000000 ) ;
#28415 = DIRECTION ( 'NONE',  ( -0.7071067811865487940, 0.7071067811865463515, 0.000000000000000000 ) ) ;
#28417 = CARTESIAN_POINT ( 'NONE',  ( 25.22959685856476142, -6.110000000000000320, -1.637169565754161393 ) ) ;
#28418 = VERTEX_POINT ( 'NONE', #33704 ) ;
#28419 = CARTESIAN_POINT ( 'NONE',  ( 6.299744871391586898, -27.71228299555210484, 4.000000000000000000 ) ) ;
#28420 = VERTEX_POINT ( 'NONE', #64900 ) ;
#28421 = VECTOR ( 'NONE', #82801, 1000.000000000000000 ) ;
#28422 = CARTESIAN_POINT ( 'NONE',  ( -6.838293875473762107, -6.740707523384212863, 16.75550250614865888 ) ) ;
#28423 = CARTESIAN_POINT ( 'NONE',  ( 30.48921356237309510, -27.52281430457076894, 5.000000000000000000 ) ) ;
#28424 = LINE ( 'NONE', #84931, #109231 ) ;
#28425 = ADVANCED_FACE ( 'NONE', ( #121390 ), #102355, .F. ) ;
#28426 = FACE_OUTER_BOUND ( 'NONE', #141867, .T. ) ;
#28427 = ORIENTED_EDGE ( 'NONE', *, *, #61087, .F. ) ;
#28428 = CARTESIAN_POINT ( 'NONE',  ( 57.45876352523143993, 0.000000000000000000, -6.110000000000001208 ) ) ;
#28429 = EDGE_CURVE ( 'NONE', #43110, #22506, #142458, .T. ) ;
#28430 = EDGE_CURVE ( 'NONE', #29863, #33461, #131573, .T. ) ;
#28431 = ORIENTED_EDGE ( 'NONE', *, *, #9655, .F. ) ;
#28432 = DIRECTION ( 'NONE',  ( 1.000000000000000000, 0.000000000000000000, 0.000000000000000000 ) ) ;
#28433 = FACE_OUTER_BOUND ( 'NONE', #105766, .T. ) ;
#28434 = DIRECTION ( 'NONE',  ( 0.000000000000000000, -1.000000000000000000, 0.000000000000000000 ) ) ;
#28435 = DIRECTION ( 'NONE',  ( -1.000000000000000000, -1.224606353822377258E-16, -0.000000000000000000 ) ) ;
#28436 = EDGE_CURVE ( 'NONE', #61275, #10245, #72195, .T. ) ;
#28437 = ADVANCED_FACE ( 'NONE', ( #9014 ), #42448, .F. ) ;
#28438 = VECTOR ( 'NONE', #69194, 1000.000000000000000 ) ;
#28439 = CARTESIAN_POINT ( 'NONE',  ( 46.14126352523144448, 4.472830434245836706, 4.472830434245840259 ) ) ;
#28440 = VERTEX_POINT ( 'NONE', #43146 ) ;
#28441 = DIRECTION ( 'NONE',  ( 1.000000000000000000, 0.000000000000000000, 0.000000000000000000 ) ) ;
#28442 = EDGE_CURVE ( 'NONE', #117951, #54976, #21384, .T. ) ;
#28443 = LINE ( 'NONE', #63239, #31653 ) ;
#28444 = ORIENTED_EDGE ( 'NONE', *, *, #125315, .T. ) ;
#28445 = VERTEX_POINT ( 'NONE', #10477 ) ;
#28446 = LINE ( 'NONE', #59659, #33158 ) ;
#28447 = EDGE_LOOP ( 'NONE', ( #63912, #69037, #141231, #43824 ) ) ;
#28448 = VECTOR ( 'NONE', #108658, 1000.000000000000000 ) ;
#28449 = EDGE_CURVE ( 'NONE', #100336, #66493, #143150, .T. ) ;
#28450 = PRODUCT_DEFINITION_SHAPE ( 'NONE', 'NONE',  #143575 ) ;
#28451 = FACE_OUTER_BOUND ( 'NONE', #59411, .T. ) ;
#28452 = EDGE_LOOP ( 'NONE', ( #1640, #15920, #89965, #43301 ) ) ;
#28453 = VECTOR ( 'NONE', #67025, 1000.000000000000000 ) ;
#28454 = CARTESIAN_POINT ( 'NONE',  ( 34.58990935480147755, 9.759292476615625489, 11.28811694763786733 ) ) ;
#28455 = VECTOR ( 'NONE', #6064, 1000.000000000000000 ) ;
#28456 = VECTOR ( 'NONE', #96135, 1000.000000000000000 ) ;
#28457 = EDGE_CURVE ( 'NONE', #13719, #110313, #94295, .T. ) ;
#28458 = DIRECTION ( 'NONE',  ( -0.7071067811865486830, -0.7071067811865464625, 0.000000000000000000 ) ) ;
#28459 = FACE_BOUND ( 'NONE', #97100, .T. ) ;
#28460 = CARTESIAN_POINT ( 'NONE',  ( 34.92499999999998295, 22.22500000000000142, 4.500000000000000888 ) ) ;
#28461 = PLANE ( 'NONE',  #34079 ) ;
#28462 = ORIENTED_EDGE ( 'NONE', *, *, #24503, .T. ) ;
#28463 = DIRECTION ( 'NONE',  ( 0.6830127018922180770, -0.6830127018922204085, -0.2588190451025213501 ) ) ;
#28465 = EDGE_LOOP ( 'NONE', ( #55166, #1548, #59594, #62242 ) ) ;
#28464 = DIRECTION ( 'NONE',  ( 0.7071067811865486830, -0.7071067811865464625, -0.000000000000000000 ) ) ;
#28467 = VERTEX_POINT ( 'NONE', #71870 ) ;
#28466 = EDGE_CURVE ( 'NONE', #100977, #32778, #113916, .T. ) ;
#28468 = CARTESIAN_POINT ( 'NONE',  ( -20.56494995367816614, -2.598550695876024275, 5.000000000000000000 ) ) ;
#28469 = ORIENTED_EDGE ( 'NONE', *, *, #71350, .F. ) ;
#28470 = VECTOR ( 'NONE', #97122, 1000.000000000000000 ) ;
#28471 = VERTEX_POINT ( 'NONE', #103044 ) ;
#28472 = CARTESIAN_POINT ( 'NONE',  ( 65.24543019189810877, -5.291415217122918513, -3.055000000000000160 ) ) ;
#28473 = ORIENTED_EDGE ( 'NONE', *, *, #128991, .F. ) ;
#28474 = FACE_OUTER_BOUND ( 'NONE', #92525, .T. ) ;
#28475 = PLANE ( 'NONE',  #47389 ) ;
#28476 = VECTOR ( 'NONE', #4463, 1000.000000000000114 ) ;
#28477 = ADVANCED_FACE ( 'NONE', ( #116765 ), #4366, .F. ) ;
#28478 = ORIENTED_EDGE ( 'NONE', *, *, #49256, .F. ) ;
#28479 = CARTESIAN_POINT ( 'NONE',  ( -24.48921356237309510, -27.52281430457072631, 5.000000000000000000 ) ) ;
#28480 = AXIS2_PLACEMENT_3D ( 'NONE', #47513, #3222, #114821 ) ;
#28481 = ADVANCED_FACE ( 'NONE', ( #137830 ), #70468, .F. ) ;
#28482 = PLANE ( 'NONE',  #114973 ) ;
#28483 = PLANE ( 'NONE',  #43605 ) ;
#28484 = DIRECTION ( 'NONE',  ( -1.000000000000000000, -0.000000000000000000, -0.000000000000000000 ) ) ;
#28485 = ADVANCED_FACE ( 'NONE', ( #116039 ), #48669, .T. ) ;
#28486 = LINE ( 'NONE', #27031, #79473 ) ;
#28487 = DIRECTION ( 'NONE',  ( -0.000000000000000000, 0.000000000000000000, 1.000000000000000000 ) ) ;
#28488 = ORIENTED_EDGE ( 'NONE', *, *, #41132, .F. ) ;
#28489 = VECTOR ( 'NONE', #62136, 1000.000000000000000 ) ;
#28490 = ORIENTED_EDGE ( 'NONE', *, *, #24228, .T. ) ;
#28491 = DIRECTION ( 'NONE',  ( 1.000000000000000000, 0.000000000000000000, 0.000000000000000000 ) ) ;
#28492 = DIRECTION ( 'NONE',  ( -0.6830127018922180770, -0.6830127018922204085, -0.2588190451025213501 ) ) ;
#28493 = ORIENTED_EDGE ( 'NONE', *, *, #95539, .F. ) ;
#28494 = ADVANCED_FACE ( 'NONE', ( #115294 ), #3685, .T. ) ;
#28495 = VERTEX_POINT ( 'NONE', #124790 ) ;
#28496 = VERTEX_POINT ( 'NONE', #25461 ) ;
#28497 = CARTESIAN_POINT ( 'NONE',  ( 36.29974487139159578, -27.71228299555231445, 4.000000000000000000 ) ) ;
#28498 = AXIS2_PLACEMENT_3D ( 'NONE', #7127, #51409, #139858 ) ;
#28499 = EDGE_LOOP ( 'NONE', ( #109879, #62542, #103760, #12047 ) ) ;
#28500 = DIRECTION ( 'NONE',  ( -0.000000000000000000, -0.000000000000000000, 1.000000000000000000 ) ) ;
#28501 = CARTESIAN_POINT ( 'NONE',  ( 12.19999999999999574, -60.26999999999998892, 25.00000000000000000 ) ) ;
#28502 = CARTESIAN_POINT ( 'NONE',  ( 12.60873647476855197, -5.808823158059033709, 5.808823158059035485 ) ) ;
#28503 = CARTESIAN_POINT ( 'NONE',  ( 1.666965064704732269, -1.287028696899377367E-11, -6.428034935295263708 ) ) ;
#28504 = ORIENTED_EDGE ( 'NONE', *, *, #73493, .T. ) ;
#28505 = CARTESIAN_POINT ( 'NONE',  ( 23.32000000000000028, 2.055000000000001492, 2.516649172247811554E-16 ) ) ;
#28506 = EDGE_CURVE ( 'NONE', #46033, #66739, #61018, .T. ) ;
#28507 = CARTESIAN_POINT ( 'NONE',  ( -13.00193056682089043, -22.22500000000000142, 4.500000000000000888 ) ) ;
#28508 = DIRECTION ( 'NONE',  ( 0.7071067811865486830, -0.7071067811865464625, -0.000000000000000000 ) ) ;
#28509 = VECTOR ( 'NONE', #77578, 999.9999999999998863 ) ;
#28511 = ORIENTED_EDGE ( 'NONE', *, *, #2100, .F. ) ;
#28510 = CARTESIAN_POINT ( 'NONE',  ( -13.49999999999990763, 11.52377502935402198, -1.522421517564052751 ) ) ;
#28512 = DIRECTION ( 'NONE',  ( 0.7071067811865487940, 0.7071067811865463515, 0.000000000000000000 ) ) ;
#28513 = ORIENTED_EDGE ( 'NONE', *, *, #1401, .F. ) ;
#28514 = DIRECTION ( 'NONE',  ( 0.7071067811865487940, 0.7071067811865463515, 0.000000000000000000 ) ) ;
#28515 = EDGE_CURVE ( 'NONE', #66659, #73980, #38505, .T. ) ;
#28516 = CARTESIAN_POINT ( 'NONE',  ( -18.48921356237309510, -27.52281430457068367, 5.000000000000000000 ) ) ;
#28517 = AXIS2_PLACEMENT_3D ( 'NONE', #1539, #122632, #23303 ) ;
#28518 = LINE ( 'NONE', #5291, #44836 ) ;
#28520 = ORIENTED_EDGE ( 'NONE', *, *, #68849, .F. ) ;
#28519 = VECTOR ( 'NONE', #118308, 1000.000000000000000 ) ;
#28521 = DIRECTION ( 'NONE',  ( 0.6830127018922181881, 0.6830127018922202975, -0.2588190451025214056 ) ) ;
#28522 = CARTESIAN_POINT ( 'NONE',  ( -14.51078643762690490, -27.52281430457045275, 5.000000000000000000 ) ) ;
#28523 = DIRECTION ( 'NONE',  ( -0.6830127018922181881, 0.6830127018922202975, -0.2588190451025214056 ) ) ;
#28524 = AXIS2_PLACEMENT_3D ( 'NONE', #132763, #20369, #107397 ) ;
#28525 = ORIENTED_EDGE ( 'NONE', *, *, #130833, .T. ) ;
#28526 = CARTESIAN_POINT ( 'NONE',  ( 6.060110710440158144, -9.740707523384187994, 10.89222023123379302 ) ) ;
#28527 = CARTESIAN_POINT ( 'NONE',  ( 27.18398860626900060, 28.73617430169806042, 5.000000000000000000 ) ) ;
#28528 = CARTESIAN_POINT ( 'NONE',  ( 19.10813147593277250, 4.202752102959690472E-16, 0.000000000000000000 ) ) ;
#28529 = DIRECTION ( 'NONE',  ( -0.6830127018922181881, 0.6830127018922202975, -0.2588190451025214056 ) ) ;
#28530 = CARTESIAN_POINT ( 'NONE',  ( 10.82816939922345867, 9.759292476615614831, 4.000000000000000000 ) ) ;
#28531 = VERTEX_POINT ( 'NONE', #82044 ) ;
#28532 = EDGE_CURVE ( 'NONE', #49419, #1370, #69734, .T. ) ;
#28533 = ORIENTED_EDGE ( 'NONE', *, *, #67653, .F. ) ;
#28534 = LINE ( 'NONE', #83644, #68025 ) ;
#28535 = DIRECTION ( 'NONE',  ( -0.6830127018922181881, 0.6830127018922202975, -0.2588190451025214056 ) ) ;
#28536 = CARTESIAN_POINT ( 'NONE',  ( 7.707903141435220817, -6.871911579029513106, -3.967499999999993587 ) ) ;
#28537 = LINE ( 'NONE', #39414, #138464 ) ;
#28538 = AXIS2_PLACEMENT_3D ( 'NONE', #29936, #106053, #130723 ) ;
#28539 = DIRECTION ( 'NONE',  ( -0.000000000000000000, 0.000000000000000000, 1.000000000000000000 ) ) ;
#28540 = CARTESIAN_POINT ( 'NONE',  ( -32.48334561358932149, 22.22500000000000142, 4.500000000000000888 ) ) ;
#28541 = CARTESIAN_POINT ( 'NONE',  ( 16.49999999999988276, 14.14708470758592540, -0.5283514160166939977 ) ) ;
#28542 = ORIENTED_EDGE ( 'NONE', *, *, #120572, .F. ) ;
#28543 = DIRECTION ( 'NONE',  ( 0.6830127018922181881, 0.6830127018922202975, -0.2588190451025214056 ) ) ;
#28544 = CARTESIAN_POINT ( 'NONE',  ( 3.459838389497381872, 18.75929247661552779, 8.305906642995493527 ) ) ;
#28545 = CARTESIAN_POINT ( 'NONE',  ( 5.295806282870439752, -5.278424836066144543, 3.047499999999995879 ) ) ;
#28546 = CARTESIAN_POINT ( 'NONE',  ( -0.7071067811865398012, -3.740707523384244837, 5.000000000000000000 ) ) ;
#28547 = CARTESIAN_POINT ( 'NONE',  ( 47.74543019189811588, -5.291415217122919401, -3.055000000000000604 ) ) ;
#28548 = EDGE_CURVE ( 'NONE', #142104, #20334, #37808, .T. ) ;
#28549 = VECTOR ( 'NONE', #85169, 1000.000000000000227 ) ;
#28550 = CARTESIAN_POINT ( 'NONE',  ( 24.56840764549667355, 3.061616997868385113E-16, -2.500000000000001332 ) ) ;
#28551 = EDGE_CURVE ( 'NONE', #50573, #26834, #116119, .T. ) ;
#28552 = ORIENTED_EDGE ( 'NONE', *, *, #29628, .T. ) ;
#28553 = CARTESIAN_POINT ( 'NONE',  ( 12.45512140948705415, 22.22500000000000142, 22.95409916400075900 ) ) ;
#28554 = ORIENTED_EDGE ( 'NONE', *, *, #49754, .T. ) ;
#28555 = VERTEX_POINT ( 'NONE', #15988 ) ;
#28556 = CARTESIAN_POINT ( 'NONE',  ( 11.51078643762690490, -27.52281430457047406, 5.000000000000000000 ) ) ;
#28557 = PLANE ( 'NONE',  #106238 ) ;
#28559 = VECTOR ( 'NONE', #51156, 1000.000000000000000 ) ;
#28558 = DIRECTION ( 'NONE',  ( -0.7071067811865487940, 0.7071067811865463515, -0.000000000000000000 ) ) ;
#28560 = CARTESIAN_POINT ( 'NONE',  ( -2.293876922608026003, 22.22500000000000142, 4.000000000000000000 ) ) ;
#28561 = EDGE_CURVE ( 'NONE', #13220, #141911, #60277, .T. ) ;
#28562 = LINE ( 'NONE', #26415, #44131 ) ;
#28563 = CARTESIAN_POINT ( 'NONE',  ( 131.5423521607622490, -49.05583548141700589, 39.86617647058822911 ) ) ;
#28564 = EDGE_LOOP ( 'NONE', ( #114187, #105495, #87074, #58858 ) ) ;
#28565 = LINE ( 'NONE', #63360, #127708 ) ;
#28566 = CARTESIAN_POINT ( 'NONE',  ( -24.18398860626899705, 28.73617430169804265, 5.000000000000000000 ) ) ;
#28567 = UNCERTAINTY_MEASURE_WITH_UNIT (LENGTH_MEASURE( 1.000000000000000082E-05 ), #62873, 'distance_accuracy_value', 'NONE');
#28568 = FACE_OUTER_BOUND ( 'NONE', #8144, .T. ) ;
#28569 = FACE_OUTER_BOUND ( 'NONE', #20487, .T. ) ;
#28570 = DIRECTION ( 'NONE',  ( -0.3543493200069163240, -0.000000000000000000, 0.9351131265310288487 ) ) ;
#28571 = AXIS2_PLACEMENT_3D ( 'NONE', #41821, #143266, #54167 ) ;
#28572 = CARTESIAN_POINT ( 'NONE',  ( 66.14169371712955581, -2.130196079827424871, -7.949999999999999289 ) ) ;
#28573 = VECTOR ( 'NONE', #62053, 1000.000000000000000 ) ;
#28574 = DIRECTION ( 'NONE',  ( -0.7071067811865486830, 0.7071067811865464625, 0.000000000000000000 ) ) ;
#28575 = ORIENTED_EDGE ( 'NONE', *, *, #63637, .F. ) ;
#28576 = VERTEX_POINT ( 'NONE', #5113 ) ;
#28577 =( BOUNDED_CURVE ( )  B_SPLINE_CURVE ( 3, ( #113984, #126289, #14675, #26968 ),
 .UNSPECIFIED., .F., .T. ) 
 B_SPLINE_CURVE_WITH_KNOTS ( ( 4, 4 ),
 ( 1.964434688349484315, 3.503810798801450854 ),
 .UNSPECIFIED. ) 
 CURVE ( )  GEOMETRIC_REPRESENTATION_ITEM ( )  RATIONAL_B_SPLINE_CURVE ( ( 1.000000000000000000, 0.8120851936182275077, 0.8120851936182275077, 1.000000000000000000 ) ) 
 REPRESENTATION_ITEM ( '' )  );
#28578 = CARTESIAN_POINT ( 'NONE',  ( 60.20833333333333570, -3.974999999999999201, -6.884901960086287964 ) ) ;
#28579 = PLANE ( 'NONE',  #63273 ) ;
#28580 = DIRECTION ( 'NONE',  ( -1.000000000000000000, 0.000000000000000000, 0.000000000000000000 ) ) ;
#28581 = AXIS2_PLACEMENT_3D ( 'NONE', #49101, #60713, #81743 ) ;
#28582 = DIRECTION ( 'NONE',  ( 0.000000000000000000, -1.000000000000000000, 0.000000000000000000 ) ) ;
#28583 = ORIENTED_EDGE ( 'NONE', *, *, #80030, .T. ) ;
#28584 = DIRECTION ( 'NONE',  ( 2.781805975412905274E-17, -0.3543493200069152138, 0.9351131265310292928 ) ) ;
#28585 = CARTESIAN_POINT ( 'NONE',  ( 1.110173228882102237, -22.22499999999999787, 4.785647885939354751 ) ) ;
#28586 = CARTESIAN_POINT ( 'NONE',  ( 61.10459685856476852, 1.637169565754164946, -6.109999999999999432 ) ) ;
#28587 = ORIENTED_EDGE ( 'NONE', *, *, #99810, .T. ) ;
#28588 = ADVANCED_FACE ( 'NONE', ( #49413 ), #82729, .F. ) ;
#28589 = FACE_OUTER_BOUND ( 'NONE', #22383, .T. ) ;
#28590 = VERTEX_POINT ( 'NONE', #5833 ) ;
#28591 = VERTEX_POINT ( 'NONE', #83443 ) ;
#28592 = VECTOR ( 'NONE', #79217, 1000.000000000000000 ) ;
#28593 = CARTESIAN_POINT ( 'NONE',  ( 12.70710678118645198, 20.25929247661551003, 5.000000000000000000 ) ) ;
#28594 = DIRECTION ( 'NONE',  ( 0.000000000000000000, -0.000000000000000000, 1.000000000000000000 ) ) ;
#28595 = LINE ( 'NONE', #81565, #39725 ) ;
#28596 = PLANE ( 'NONE',  #90311 ) ;
#28597 = FACE_OUTER_BOUND ( 'NONE', #76200, .T. ) ;
#28598 = EDGE_CURVE ( 'NONE', #39505, #129536, #61704, .T. ) ;
#28599 = ADVANCED_FACE ( 'NONE', ( #36368 ), #80596, .F. ) ;
#28601 = ORIENTED_EDGE ( 'NONE', *, *, #67581, .T. ) ;
#28600 = CARTESIAN_POINT ( 'NONE',  ( 100.4125270504628986, -7.949999999999998401, -4.867971026610728450E-16 ) ) ;
#28602 = LINE ( 'NONE', #72857, #92377 ) ;
#28603 = LINE ( 'NONE', #42344, #89394 ) ;
#28604 = VECTOR ( 'NONE', #117014, 1000.000000000000000 ) ;
#28605 = PLANE ( 'NONE',  #19274 ) ;
#28606 = CARTESIAN_POINT ( 'NONE',  ( -7.940000000000001279, -33.26999999999999602, -11.89864999999999462 ) ) ;
#28607 = CARTESIAN_POINT ( 'NONE',  ( -29.99999999999978328, 17.96639925780208102, 5.000000000000000000 ) ) ;
#28609 = EDGE_LOOP ( 'NONE', ( #1499, #97149, #126990, #85272 ) ) ;
#28608 = EDGE_CURVE ( 'NONE', #73287, #86117, #107313, .T. ) ;
#28610 = EDGE_CURVE ( 'NONE', #71524, #89805, #129065, .T. ) ;
#28611 = VERTEX_POINT ( 'NONE', #29738 ) ;
#28612 = VECTOR ( 'NONE', #81820, 999.9999999999998863 ) ;
#28613 = ADVANCED_FACE ( 'NONE', ( #84181 ), #51534, .T. ) ;
#28614 = DIRECTION ( 'NONE',  ( -0.7071067811865486830, 0.7071067811865464625, 0.000000000000000000 ) ) ;
#28615 = DIRECTION ( 'NONE',  ( -0.3543493200069162685, -0.000000000000000000, -0.9351131265310288487 ) ) ;
#28617 = EDGE_CURVE ( 'NONE', #20377, #45045, #95728, .T. ) ;
#28616 = CARTESIAN_POINT ( 'NONE',  ( -34.92500000000001137, -22.22500000000000142, 4.500000000000000888 ) ) ;
#28618 = CARTESIAN_POINT ( 'NONE',  ( -21.32816939922337696, 14.25929247661557753, 4.000000000000000000 ) ) ;
#28619 = CARTESIAN_POINT ( 'NONE',  ( 72.12086038379622721, -6.884901960086286188, 3.974999999999997424 ) ) ;
#28620 = ORIENTED_EDGE ( 'NONE', *, *, #86927, .F. ) ;
#28621 = ORIENTED_EDGE ( 'NONE', *, *, #110411, .F. ) ;
#28622 = EDGE_CURVE ( 'NONE', #14566, #3084, #41334, .T. ) ;
#28623 = FACE_OUTER_BOUND ( 'NONE', #38888, .T. ) ;
#28624 = DIRECTION ( 'NONE',  ( 0.7071067811865486830, -0.7071067811865464625, -0.000000000000000000 ) ) ;
#28625 = EDGE_LOOP ( 'NONE', ( #35645, #70866, #93255, #60037 ) ) ;
#28626 = CIRCLE ( 'NONE', #21568, 2.500000000000000444 ) ;
#28627 = ADVANCED_FACE ( 'NONE', ( #108001 ), #84856, .T. ) ;
#28628 = ORIENTED_EDGE ( 'NONE', *, *, #136515, .T. ) ;
#28629 = CARTESIAN_POINT ( 'NONE',  ( -21.48921356237309155, -27.52281430457070499, 5.000000000000000000 ) ) ;
#28630 = VERTEX_POINT ( 'NONE', #108709 ) ;
#28631 = CARTESIAN_POINT ( 'NONE',  ( 0.000000000000000000, 0.000000000000000000, 0.000000000000000000 ) ) ;
#28632 = CARTESIAN_POINT ( 'NONE',  ( 34.92499999999998295, 4.701930566820937685, 4.500000000000000888 ) ) ;
#28633 =( GEOMETRIC_REPRESENTATION_CONTEXT ( 3 ) GLOBAL_UNCERTAINTY_ASSIGNED_CONTEXT ( ( #76225 ) ) GLOBAL_UNIT_ASSIGNED_CONTEXT ( ( #3279, #25757, #61990 ) ) REPRESENTATION_CONTEXT ( 'NONE', 'WORKASPACE' ) );
#28634 = ADVANCED_FACE ( 'NONE', ( #7261 ), #96410, .F. ) ;
#28635 = FACE_BOUND ( 'NONE', #92468, .T. ) ;
#28636 = DIRECTION ( 'NONE',  ( -0.7071067811865486830, -0.7071067811865464625, 0.000000000000000000 ) ) ;
#28637 = DIRECTION ( 'NONE',  ( 0.3543493200069162685, -0.000000000000000000, -0.9351131265310288487 ) ) ;
#28639 = ORIENTED_EDGE ( 'NONE', *, *, #138710, .T. ) ;
#28638 = DIRECTION ( 'NONE',  ( 0.7071067811865487940, 0.7071067811865463515, -0.000000000000000000 ) ) ;
#28641 = EDGE_CURVE ( 'NONE', #47477, #28496, #118164, .T. ) ;
#28640 = AXIS2_PLACEMENT_3D ( 'NONE', #49871, #72365, #27357 ) ;
#28642 = SURFACE_STYLE_USAGE ( .BOTH. , #107597 ) ;
#28643 = APPLICATION_PROTOCOL_DEFINITION ( 'draft international standard', 'automotive_design', 1998, #92057 ) ;
#28644 = ORIENTED_EDGE ( 'NONE', *, *, #100005, .T. ) ;
#28645 = EDGE_LOOP ( 'NONE', ( #55699, #54321, #24173, #100740 ) ) ;
#28646 = CARTESIAN_POINT ( 'NONE',  ( 89.74543019189812298, -5.291415217122918513, -3.055000000000000160 ) ) ;
#28647 = ORIENTED_EDGE ( 'NONE', *, *, #72371, .T. ) ;
#28648 = DIRECTION ( 'NONE',  ( -1.000000000000000000, -1.224606353822377258E-16, -0.000000000000000000 ) ) ;
#28649 = PLANE ( 'NONE',  #386 ) ;
#28650 = VECTOR ( 'NONE', #56719, 1000.000000000000000 ) ;
#28651 = LINE ( 'NONE', #72903, #10898 ) ;
#28652 = CARTESIAN_POINT ( 'NONE',  ( -20.99999999999984013, 11.58746187583912324, 4.000000000000000000 ) ) ;
#28654 = ORIENTED_EDGE ( 'NONE', *, *, #33903, .F. ) ;
#28653 = EDGE_CURVE ( 'NONE', #19482, #85621, #11898, .T. ) ;
#28655 = CARTESIAN_POINT ( 'NONE',  ( -34.92500000000001137, 22.22500000000000142, 4.000000000000000000 ) ) ;
#28656 = FACE_OUTER_BOUND ( 'NONE', #117804, .T. ) ;
#28657 = CIRCLE ( 'NONE', #65738, 2.500000000000000888 ) ;
#28658 = PLANE ( 'NONE',  #78194 ) ;
#28659 = FACE_OUTER_BOUND ( 'NONE', #4251, .T. ) ;
#28660 = EDGE_CURVE ( 'NONE', #13520, #70281, #85549, .T. ) ;
#28661 = DIRECTION ( 'NONE',  ( 0.6830127018922181881, 0.6830127018922202975, -0.2588190451025214056 ) ) ;
#28662 = CARTESIAN_POINT ( 'NONE',  ( 181.1499999999998067, -47.87246431468548735, -37.20487561447684044 ) ) ;
#28663 = DIRECTION ( 'NONE',  ( -0.7071067811865486830, 0.7071067811865464625, 0.000000000000000000 ) ) ;
#28664 = EDGE_LOOP ( 'NONE', ( #8712, #92068, #68677, #61736, #69215, #71369 ) ) ;
#28665 = CARTESIAN_POINT ( 'NONE',  ( 0.000000000000000000, 10.21212019023809425, -2.019456568337797187 ) ) ;
#28666 = ADVANCED_FACE ( 'NONE', ( #30486 ), #74725, .F. ) ;
#28667 = DIRECTION ( 'NONE',  ( -1.000000000000000000, -1.224606353822377258E-16, -0.000000000000000000 ) ) ;
#28668 = VECTOR ( 'NONE', #103904, 1000.000000000000000 ) ;
#28669 = ORIENTED_EDGE ( 'NONE', *, *, #91681, .F. ) ;
#28670 = EDGE_LOOP ( 'NONE', ( #79254, #115144, #48341, #68111 ) ) ;
#28671 = ORIENTED_EDGE ( 'NONE', *, *, #109229, .F. ) ;
#28672 = CARTESIAN_POINT ( 'NONE',  ( 46.08376352523143993, -6.110000000000001208, -3.741295971395164515E-16 ) ) ;
#28673 = ORIENTED_EDGE ( 'NONE', *, *, #3987, .T. ) ;
#28674 = AXIS2_PLACEMENT_3D ( 'NONE', #53619, #31159, #42757 ) ;
#28675 = VECTOR ( 'NONE', #68118, 999.9999999999998863 ) ;
#28676 = CARTESIAN_POINT ( 'NONE',  ( 11.71247294953710671, 0.000000000000000000, 6.094999999999989981 ) ) ;
#28677 = CARTESIAN_POINT ( 'NONE',  ( -12.12207849854756248, 7.746936202595393617, -28.17582321246111832 ) ) ;
#28678 = ORIENTED_EDGE ( 'NONE', *, *, #20774, .F. ) ;
#28679 = EDGE_CURVE ( 'NONE', #43879, #111424, #118901, .T. ) ;
#28680 = DIRECTION ( 'NONE',  ( 0.7071067811865486830, -0.7071067811865464625, -0.000000000000000000 ) ) ;
#28681 = VERTEX_POINT ( 'NONE', #18128 ) ;
#28682 = SPHERICAL_SURFACE ( 'NONE', #113564, 0.5000000000000000000 ) ;
#28683 = AXIS2_PLACEMENT_3D ( 'NONE', #133221, #136045, #112174 ) ;
#28684 = DIRECTION ( 'NONE',  ( -1.000000000000000000, -0.000000000000000000, -0.000000000000000000 ) ) ;
#28686 = ORIENTED_EDGE ( 'NONE', *, *, #87190, .F. ) ;
#28685 = DIRECTION ( 'NONE',  ( -1.000000000000000000, -1.224606353822377258E-16, -0.000000000000000000 ) ) ;
#28687 = VERTEX_POINT ( 'NONE', #128376 ) ;
#28688 = CARTESIAN_POINT ( 'NONE',  ( -45.48921356237309510, -27.52281430457087197, 5.000000000000000000 ) ) ;
#28689 = DIRECTION ( 'NONE',  ( 0.000000000000000000, 0.000000000000000000, 1.000000000000000000 ) ) ;
#28690 = ORIENTED_EDGE ( 'NONE', *, *, #66417, .F. ) ;
#28691 = CARTESIAN_POINT ( 'NONE',  ( -35.99451991528749772, 28.92564299267963079, 4.000000000000000000 ) ) ;
#28692 = ORIENTED_EDGE ( 'NONE', *, *, #71997, .F. ) ;
#28693 = ORIENTED_EDGE ( 'NONE', *, *, #131884, .T. ) ;
#28694 = EDGE_CURVE ( 'NONE', #84890, #109323, #109188, .T. ) ;
#28695 = ORIENTED_EDGE ( 'NONE', *, *, #53166, .T. ) ;
#28696 = ORIENTED_EDGE ( 'NONE', *, *, #31879, .F. ) ;
#28697 = CARTESIAN_POINT ( 'NONE',  ( 0.000000000000000000, -7.068876922607745250, 4.000000000000000000 ) ) ;
#28698 = VECTOR ( 'NONE', #61188, 1000.000000000000227 ) ;
#28699 = CARTESIAN_POINT ( 'NONE',  ( 14.27159235450332098, 2.500000000000001776, 0.000000000000000000 ) ) ;
#28700 = DIRECTION ( 'NONE',  ( 0.7071067811865487940, 0.7071067811865463515, 0.000000000000000000 ) ) ;
#28701 = ADVANCED_FACE ( 'NONE', ( #42090 ), #95212, .T. ) ;
#28702 = CARTESIAN_POINT ( 'NONE',  ( -29.67183060077626422, -21.74070752338406010, 4.000000000000000000 ) ) ;
#28703 = ORIENTED_EDGE ( 'NONE', *, *, #63637, .T. ) ;
#28704 = LINE ( 'NONE', #96061, #79012 ) ;
#28705 = VERTEX_POINT ( 'NONE', #62411 ) ;
#28706 = CARTESIAN_POINT ( 'NONE',  ( 57.48921356237308800, -27.52281430457095368, 5.000000000000000000 ) ) ;
#28707 = CARTESIAN_POINT ( 'NONE',  ( 34.24956980810188156, 3.967499999999998916, 6.871911579029510442 ) ) ;
#28708 = EDGE_CURVE ( 'NONE', #12409, #47805, #31204, .T. ) ;
#28709 = CARTESIAN_POINT ( 'NONE',  ( 0.000000000000000000, 0.000000000000000000, 5.000000000000000000 ) ) ;
#28710 = VECTOR ( 'NONE', #140123, 999.9999999999998863 ) ;
#28711 = CARTESIAN_POINT ( 'NONE',  ( 2.187538124160505415, -22.22500000000000142, 4.000000000000000000 ) ) ;
#28712 = CARTESIAN_POINT ( 'NONE',  ( -33.98013387480477832, 22.27000000000000313, -13.08571143629930944 ) ) ;
#28713 = ORIENTED_EDGE ( 'NONE', *, *, #38592, .T. ) ;
#28714 = EDGE_LOOP ( 'NONE', ( #13135, #73655, #120558, #85999 ) ) ;
#28715 = EDGE_LOOP ( 'NONE', ( #129696, #42268, #61373, #39847 ) ) ;
#28716 = CARTESIAN_POINT ( 'NONE',  ( 0.000000000000000000, 0.000000000000000000, 5.000000000000000000 ) ) ;
#28717 = CARTESIAN_POINT ( 'NONE',  ( -18.48921356237309510, -27.52281430457068367, 5.000000000000000000 ) ) ;
#28718 = FACE_OUTER_BOUND ( 'NONE', #76137, .T. ) ;
#28719 = CARTESIAN_POINT ( 'NONE',  ( -34.49999999999974420, -17.94567065516885762, 4.994342998332165884 ) ) ;
#28720 = CARTESIAN_POINT ( 'NONE',  ( 2.999999999999999112, -47.62213595499957108, -36.92499999999996874 ) ) ;
#28721 = CARTESIAN_POINT ( 'NONE',  ( 73.55793019189812298, 6.110000000000001208, -1.637169565754156286 ) ) ;
#28723 = EDGE_CURVE ( 'NONE', #47408, #117065, #75421, .T. ) ;
#28722 = VECTOR ( 'NONE', #27351, 1000.000000000000000 ) ;
#28724 = CARTESIAN_POINT ( 'NONE',  ( 22.85159235450332105, 9.902892378096218942E-16, 0.000000000000000000 ) ) ;
#28725 = DIRECTION ( 'NONE',  ( -0.7071067811865486830, -0.7071067811865464625, -0.000000000000000000 ) ) ;
#28726 = EDGE_CURVE ( 'NONE', #38372, #15838, #41670, .T. ) ;
#28727 = DIRECTION ( 'NONE',  ( -0.7071067811865486830, -0.7071067811865464625, -0.000000000000000000 ) ) ;
#28728 = CYLINDRICAL_SURFACE ( 'NONE', #34940, 7.950000000000000178 ) ;
#28729 = CARTESIAN_POINT ( 'NONE',  ( 5.510786437626906675, -27.52281430457051314, 5.000000000000000000 ) ) ;
#28730 = ORIENTED_EDGE ( 'NONE', *, *, #111668, .F. ) ;
#28731 = CARTESIAN_POINT ( 'NONE',  ( -6.640000000000001457, -40.29840020119761590, 19.55137198191482995 ) ) ;
#28732 = VERTEX_POINT ( 'NONE', #21746 ) ;
#28733 = CARTESIAN_POINT ( 'NONE',  ( 45.48921356237309510, -27.52281430457087197, 5.000000000000000000 ) ) ;
#28735 = EDGE_LOOP ( 'NONE', ( #124249, #103039, #6293, #18726 ) ) ;
#28734 = CARTESIAN_POINT ( 'NONE',  ( 34.45011844616452379, -16.48371918836233618, 5.000000000000000888 ) ) ;
#28736 = ADVANCED_FACE ( 'NONE', ( #10832 ), #89839, .F. ) ;
#28737 = CARTESIAN_POINT ( 'NONE',  ( 18.32840764549667512, 9.139736423841732040E-16, 0.000000000000000000 ) ) ;
#28738 = LINE ( 'NONE', #59937, #19449 ) ;
#28739 = ORIENTED_EDGE ( 'NONE', *, *, #35984, .T. ) ;
#28740 = ORIENTED_EDGE ( 'NONE', *, *, #90259, .T. ) ;
#28741 = FACE_OUTER_BOUND ( 'NONE', #62863, .T. ) ;
#28742 = FACE_OUTER_BOUND ( 'NONE', #108997, .T. ) ;
#28743 = VECTOR ( 'NONE', #30055, 1000.000000000000000 ) ;
#28744 = DIRECTION ( 'NONE',  ( -0.7071067811865487940, 0.7071067811865463515, -0.000000000000000000 ) ) ;
#28745 = CARTESIAN_POINT ( 'NONE',  ( 93.12086038379622721, -6.884901960086286188, 3.974999999999997424 ) ) ;
#28746 = FACE_OUTER_BOUND ( 'NONE', #87234, .T. ) ;
#28747 = VECTOR ( 'NONE', #59258, 1000.000000000000227 ) ;
#28748 = SURFACE_STYLE_USAGE ( .BOTH. , #6214 ) ;
#28749 = ORIENTED_EDGE ( 'NONE', *, *, #84087, .F. ) ;
#28750 = CARTESIAN_POINT ( 'NONE',  ( 0.000000000000000000, 1.399999999999986366, 20.40202195861970580 ) ) ;
#28751 = CARTESIAN_POINT ( 'NONE',  ( 12.19999999999999574, -34.65000000000001279, -40.00000000000000000 ) ) ;
#28752 = CARTESIAN_POINT ( 'NONE',  ( 32.81250000000000000, -4.461849672132299993, -4.461849672132299105 ) ) ;
#28753 = CARTESIAN_POINT ( 'NONE',  ( -20.51078643762690490, -27.52281430457041012, 5.000000000000000000 ) ) ;
#28754 = ORIENTED_EDGE ( 'NONE', *, *, #83233, .T. ) ;
#28755 = CARTESIAN_POINT ( 'NONE',  ( -18.18398860626898994, 28.73617430169800002, 5.000000000000000000 ) ) ;
#28756 = ORIENTED_EDGE ( 'NONE', *, *, #48574, .T. ) ;
#28757 = CARTESIAN_POINT ( 'NONE',  ( 81.95876352523143282, 0.000000000000000000, -6.110000000000001208 ) ) ;
#28758 = DIRECTION ( 'NONE',  ( 0.7071067811865486830, -0.7071067811865464625, -0.000000000000000000 ) ) ;
#28759 = EDGE_CURVE ( 'NONE', #65937, #25994, #46649, .T. ) ;
#28760 = CARTESIAN_POINT ( 'NONE',  ( 32.99451991528749062, 28.92564299267960948, 4.000000000000000000 ) ) ;
#28761 = DIRECTION ( 'NONE',  ( 0.000000000000000000, 0.000000000000000000, 1.000000000000000000 ) ) ;
#28762 = EDGE_LOOP ( 'NONE', ( #81984, #16445, #80653, #37772 ) ) ;
#28763 = CARTESIAN_POINT ( 'NONE',  ( -24.70710678118636494, -6.740707523384212863, 5.000000000000000000 ) ) ;
#28764 = VECTOR ( 'NONE', #98061, 1000.000000000000227 ) ;
#28765 = LINE ( 'NONE', #62110, #37216 ) ;
#28766 = AXIS2_PLACEMENT_3D ( 'NONE', #105163, #137817, #5099 ) ;
#28767 = FACE_OUTER_BOUND ( 'NONE', #8254, .T. ) ;
#28768 = EDGE_CURVE ( 'NONE', #125118, #135031, #45670, .T. ) ;
#28770 = ORIENTED_EDGE ( 'NONE', *, *, #120357, .T. ) ;
#28769 = CARTESIAN_POINT ( 'NONE',  ( 69.48921356237309510, -27.52281430457103895, 5.000000000000000000 ) ) ;
#28771 = PLANE ( 'NONE',  #57667 ) ;
#28772 = CARTESIAN_POINT ( 'NONE',  ( -31.49999999999977973, 3.653845994658361906, -4.504631822206299319 ) ) ;
#28773 = CARTESIAN_POINT ( 'NONE',  ( 1.432180847299084014, -0.9397650347787239733, 6.598882878417470010 ) ) ;
#28774 = CARTESIAN_POINT ( 'NONE',  ( -30.51168605928413058, 6.759292476615653023, 16.35960578974476576 ) ) ;
#28775 = CIRCLE ( 'NONE', #105229, 2.500000000000000888 ) ;
#28776 = ORIENTED_EDGE ( 'NONE', *, *, #32006, .F. ) ;
#28777 = ORIENTED_EDGE ( 'NONE', *, *, #25610, .F. ) ;
#28778 = ADVANCED_FACE ( 'NONE', ( #54404 ), #87710, .F. ) ;
#28779 = CARTESIAN_POINT ( 'NONE',  ( 75.97959685856477563, 6.109999999999999432, 1.637169565754164280 ) ) ;
#28780 = AXIS2_PLACEMENT_3D ( 'NONE', #29907, #10296, #75584 ) ;
#28781 = VERTEX_POINT ( 'NONE', #66686 ) ;
#28782 = EDGE_CURVE ( 'NONE', #117931, #102793, #44976, .T. ) ;
#28783 = DIRECTION ( 'NONE',  ( -0.7071067811865486830, -0.7071067811865464625, 0.000000000000000000 ) ) ;
#28784 = EDGE_CURVE ( 'NONE', #104180, #62156, #110849, .T. ) ;
#28785 = CARTESIAN_POINT ( 'NONE',  ( 6.812461875839422198, -22.22500000000000142, 4.000000000000000000 ) ) ;
#28786 = CARTESIAN_POINT ( 'NONE',  ( 9.005480084712511157, 28.92564299267931816, 4.000000000000000000 ) ) ;
#28787 = ORIENTED_EDGE ( 'NONE', *, *, #116467, .T. ) ;
#28788 = EDGE_CURVE ( 'NONE', #60360, #10019, #34065, .T. ) ;
#28789 = CARTESIAN_POINT ( 'NONE',  ( -32.99999999999975842, 11.58746187583912146, 4.000000000000000000 ) ) ;
#28790 = FACE_OUTER_BOUND ( 'NONE', #27180, .T. ) ;
#28791 = ORIENTED_EDGE ( 'NONE', *, *, #54417, .F. ) ;
#28792 = ADVANCED_FACE ( 'NONE', ( #100027 ), #683, .F. ) ;
#28793 = FACE_OUTER_BOUND ( 'NONE', #8283, .T. ) ;
#28794 = CARTESIAN_POINT ( 'NONE',  ( -0.1839886062690032631, 28.73617430169787568, 5.000000000000000000 ) ) ;
#28795 = VECTOR ( 'NONE', #5655, 1000.000000000000000 ) ;
#28796 = LINE ( 'NONE', #49846, #81696 ) ;
#28797 = ORIENTED_EDGE ( 'NONE', *, *, #82655, .T. ) ;
#28798 = ORIENTED_EDGE ( 'NONE', *, *, #112598, .F. ) ;
#28799 = EDGE_CURVE ( 'NONE', #41413, #43020, #111607, .T. ) ;
#28800 = EDGE_CURVE ( 'NONE', #83105, #68726, #98579, .T. ) ;
#28801 = LINE ( 'NONE', #115040, #10677 ) ;
#28802 = PLANE ( 'NONE',  #113351 ) ;
#28803 = CARTESIAN_POINT ( 'NONE',  ( -53.99451991528749062, 28.92564299267975869, 4.000000000000000000 ) ) ;
#28804 =( NAMED_UNIT ( * ) SI_UNIT ( $, .STERADIAN. ) SOLID_ANGLE_UNIT ( ) );
#28805 = LINE ( 'NONE', #17875, #96682 ) ;
#28806 = EDGE_CURVE ( 'NONE', #111873, #81702, #62962, .T. ) ;
#28807 = DIRECTION ( 'NONE',  ( 0.2400000000000087064, -1.734723475976868478E-16, -0.9707728879609257566 ) ) ;
#28808 = VERTEX_POINT ( 'NONE', #43495 ) ;
#28809 = VERTEX_POINT ( 'NONE', #56568 ) ;
#28810 = EDGE_LOOP ( 'NONE', ( #83247, #102508, #117543, #104415 ) ) ;
#28811 = ORIENTED_EDGE ( 'NONE', *, *, #78528, .F. ) ;
#28812 = VECTOR ( 'NONE', #74474, 999.9999999999998863 ) ;
#28813 = SURFACE_STYLE_FILL_AREA ( #116523 ) ;
#28814 = DIRECTION ( 'NONE',  ( 1.000000000000000000, 0.000000000000000000, 0.000000000000000000 ) ) ;
#28815 = VERTEX_POINT ( 'NONE', #79011 ) ;
#28816 = DIRECTION ( 'NONE',  ( -0.000000000000000000, 0.000000000000000000, 1.000000000000000000 ) ) ;
#28817 = LINE ( 'NONE', #15728, #20188 ) ;
#28818 = ADVANCED_FACE ( 'NONE', ( #112329 ), #67535, .T. ) ;
#28819 = DIRECTION ( 'NONE',  ( 0.000000000000000000, -0.000000000000000000, 1.000000000000000000 ) ) ;
#28820 = CARTESIAN_POINT ( 'NONE',  ( 57.18398860626899705, 28.73617430169827358, 5.000000000000000000 ) ) ;
#28821 = ORIENTED_EDGE ( 'NONE', *, *, #80867, .T. ) ;
#28822 = CARTESIAN_POINT ( 'NONE',  ( -5.966809772938240997, -22.22500000000000142, -5.973340791029712271 ) ) ;
#28823 = FACE_OUTER_BOUND ( 'NONE', #45187, .T. ) ;
#28824 = ORIENTED_EDGE ( 'NONE', *, *, #19905, .T. ) ;
#28825 = DIRECTION ( 'NONE',  ( -0.000000000000000000, -0.3543493200069152693, 0.9351131265310292928 ) ) ;
#28826 = VERTEX_POINT ( 'NONE', #19352 ) ;
#28827 = DIRECTION ( 'NONE',  ( -1.000000000000000000, 0.000000000000000000, 0.000000000000000000 ) ) ;
#28828 = EDGE_LOOP ( 'NONE', ( #108767, #111100, #128280, #45826, #6606, #109454 ) ) ;
#28829 = ORIENTED_EDGE ( 'NONE', *, *, #89372, .T. ) ;
#28830 = CARTESIAN_POINT ( 'NONE',  ( 75.68793019189809002, 6.110000000000002984, -1.637169565754156730 ) ) ;
#28831 = VECTOR ( 'NONE', #1514, 999.9999999999998863 ) ;
#28832 = EDGE_LOOP ( 'NONE', ( #75953, #35115, #48001, #10900 ) ) ;
#28833 = EDGE_CURVE ( 'NONE', #69258, #92363, #72210, .T. ) ;
#28834 = VECTOR ( 'NONE', #81367, 1000.000000000000000 ) ;
#28835 = DIRECTION ( 'NONE',  ( -0.7071067811865486830, -0.7071067811865464625, 0.000000000000000000 ) ) ;
#28836 = CARTESIAN_POINT ( 'NONE',  ( 104.5629301918980900, 1.637169565754157174, 6.110000000000002984 ) ) ;
#28837 = FACE_OUTER_BOUND ( 'NONE', #24432, .T. ) ;
#28838 = AXIS2_PLACEMENT_3D ( 'NONE', #70668, #102568, #71357 ) ;
#28839 = EDGE_CURVE ( 'NONE', #92154, #105072, #43265, .T. ) ;
#28840 = DIRECTION ( 'NONE',  ( -0.7071067811865486830, -0.7071067811865464625, -0.000000000000000000 ) ) ;
#28841 = DIRECTION ( 'NONE',  ( -0.7071067811865486830, 0.7071067811865464625, 0.000000000000000000 ) ) ;
#28842 = FACE_OUTER_BOUND ( 'NONE', #105895, .T. ) ;
#28843 =( BOUNDED_CURVE ( )  B_SPLINE_CURVE ( 3, ( #117383, #4294, #51461, #81245 ),
 .UNSPECIFIED., .F., .F. ) 
 B_SPLINE_CURVE_WITH_KNOTS ( ( 4, 4 ),
 ( 5.106027341939290309, 6.645403452391242638 ),
 .UNSPECIFIED. ) 
 CURVE ( )  GEOMETRIC_REPRESENTATION_ITEM ( )  RATIONAL_B_SPLINE_CURVE ( ( 1.000000000000000000, 0.8120851936182307274, 0.8120851936182307274, 1.000000000000000000 ) ) 
 REPRESENTATION_ITEM ( '' )  );
#28844 = DIRECTION ( 'NONE',  ( 0.000000000000000000, 0.000000000000000000, -1.000000000000000000 ) ) ;
#28845 = VERTEX_POINT ( 'NONE', #73725 ) ;
#28847 = LINE ( 'NONE', #50595, #19746 ) ;
#28846 = VECTOR ( 'NONE', #124436, 1000.000000000000000 ) ;
#28848 = EDGE_CURVE ( 'NONE', #130662, #53059, #117906, .T. ) ;
#28849 = ORIENTED_EDGE ( 'NONE', *, *, #64145, .F. ) ;
#28850 = EDGE_LOOP ( 'NONE', ( #94622, #3550, #42579, #96495 ) ) ;
#28851 = CARTESIAN_POINT ( 'NONE',  ( -2.999999999999988898, 17.58746187583907172, 4.000000000000000000 ) ) ;
#28852 = VERTEX_POINT ( 'NONE', #95176 ) ;
#28853 =( BOUNDED_CURVE ( )  B_SPLINE_CURVE ( 3, ( #112290, #2040, #123888, #68799 ),
 .UNSPECIFIED., .F., .T. ) 
 B_SPLINE_CURVE_WITH_KNOTS ( ( 4, 4 ),
 ( 2.001653308786171426, 3.503810798801451742 ),
 .UNSPECIFIED. ) 
 CURVE ( )  GEOMETRIC_REPRESENTATION_ITEM ( )  RATIONAL_B_SPLINE_CURVE ( ( 1.000000000000000000, 0.8206354192515243895, 0.8206354192515243895, 1.000000000000000000 ) ) 
 REPRESENTATION_ITEM ( '' )  );
#28854 = CARTESIAN_POINT ( 'NONE',  ( 26.87852683662837094, -20.24070752338407075, 7.412974875817730513 ) ) ;
#28855 = PLANE ( 'NONE',  #22331 ) ;
#28856 = EDGE_CURVE ( 'NONE', #63590, #101471, #125695, .T. ) ;
#28857 = DIRECTION ( 'NONE',  ( -1.000000000000000000, 0.000000000000000000, 0.000000000000000000 ) ) ;
#28858 = CARTESIAN_POINT ( 'NONE',  ( -0.4892135623730947680, -27.52281430457055578, 5.000000000000000000 ) ) ;
#28859 = EDGE_LOOP ( 'NONE', ( #99613, #77583, #14371, #85451 ) ) ;
#28860 = CARTESIAN_POINT ( 'NONE',  ( 0.4812208760381984640, -49.11951764990644165, 40.13200514437900068 ) ) ;
#28861 = VERTEX_POINT ( 'NONE', #50270 ) ;
#28862 = VECTOR ( 'NONE', #135325, 1000.000000000000227 ) ;
#28863 = VECTOR ( 'NONE', #110770, 1000.000000000000000 ) ;
#28864 = CARTESIAN_POINT ( 'NONE',  ( 7.707903141435219929, -6.871911579029513106, -3.967499999999993587 ) ) ;
#28865 = CARTESIAN_POINT ( 'NONE',  ( -10.63753812416090483, 22.22500000000000142, 4.000000000000000000 ) ) ;
#28866 = VECTOR ( 'NONE', #2073, 1000.000000000000000 ) ;
#28867 = FACE_OUTER_BOUND ( 'NONE', #122319, .T. ) ;
#28868 = STYLED_ITEM ( 'NONE', ( #5594 ), #7398 ) ;
#28869 = CARTESIAN_POINT ( 'NONE',  ( 14.47191377450093697, -9.396605767970752865, -1.423631233415600050 ) ) ;
#28870 = ORIENTED_EDGE ( 'NONE', *, *, #20089, .F. ) ;
#28871 = ORIENTED_EDGE ( 'NONE', *, *, #134198, .F. ) ;
#28872 = ORIENTED_EDGE ( 'NONE', *, *, #87073, .F. ) ;
#28873 = LINE ( 'NONE', #139797, #62618 ) ;
#28874 =( NAMED_UNIT ( * ) PLANE_ANGLE_UNIT ( ) SI_UNIT ( $, .RADIAN. ) );
#28875 = DIRECTION ( 'NONE',  ( -0.000000000000000000, -0.3543493200069152693, 0.9351131265310292928 ) ) ;
#28876 = FACE_OUTER_BOUND ( 'NONE', #41630, .T. ) ;
#28877 = DIRECTION ( 'NONE',  ( 0.7071067811865487940, 0.7071067811865463515, 0.000000000000000000 ) ) ;
#28878 = DIRECTION ( 'NONE',  ( -0.7071067811865487940, -0.7071067811865463515, -0.000000000000000000 ) ) ;
#28879 = CARTESIAN_POINT ( 'NONE',  ( 35.99451991528749772, 28.92564299267963079, 4.000000000000000000 ) ) ;
#28880 = EDGE_CURVE ( 'NONE', #127352, #46830, #48848, .T. ) ;
#28881 = DIRECTION ( 'NONE',  ( -0.7071067811865486830, -0.7071067811865464625, -0.000000000000000000 ) ) ;
#28882 = CARTESIAN_POINT ( 'NONE',  ( -25.39999999999996305, 0.000000000000000000, 0.000000000000000000 ) ) ;
#28883 = ORIENTED_EDGE ( 'NONE', *, *, #51149, .T. ) ;
#28884 = CARTESIAN_POINT ( 'NONE',  ( 73.91666666666665719, -6.884901960086287076, -3.975000000000000977 ) ) ;
#28885 = FACE_OUTER_BOUND ( 'NONE', #140812, .T. ) ;
#28886 = ORIENTED_EDGE ( 'NONE', *, *, #85433, .F. ) ;
#28887 = DIRECTION ( 'NONE',  ( -0.7071067811865486830, 0.7071067811865464625, 0.000000000000000000 ) ) ;
#28888 = EDGE_CURVE ( 'NONE', #105446, #135400, #93048, .T. ) ;
#28890 = EDGE_LOOP ( 'NONE', ( #37027, #45275, #111744, #133617 ) ) ;
#28889 = FACE_OUTER_BOUND ( 'NONE', #15199, .T. ) ;
#28891 = EDGE_CURVE ( 'NONE', #91471, #4002, #72052, .T. ) ;
#28892 = CARTESIAN_POINT ( 'NONE',  ( -17.99999999999986855, 13.55218569542903140, 5.000000000000000000 ) ) ;
#28893 = DIRECTION ( 'NONE',  ( 0.000000000000000000, -1.000000000000000000, 0.000000000000000000 ) ) ;
#28894 = EDGE_LOOP ( 'NONE', ( #52789, #105573, #41649, #63845 ) ) ;
#28895 = DIRECTION ( 'NONE',  ( -0.7071067811865486830, -0.7071067811865464625, -0.000000000000000000 ) ) ;
#28896 = UNCERTAINTY_MEASURE_WITH_UNIT (LENGTH_MEASURE( 1.000000000000000082E-05 ), #13627, 'distance_accuracy_value', 'NONE');
#28897 = ORIENTED_EDGE ( 'NONE', *, *, #66392, .F. ) ;
#28898 = CARTESIAN_POINT ( 'NONE',  ( -12.70000000000000462, -22.26999999999999247, -39.50000000000000000 ) ) ;
#28899 = CARTESIAN_POINT ( 'NONE',  ( 126.2250270504628986, 5.819803920172573086, -5.819803920172572198 ) ) ;
#28900 = PLANE ( 'NONE',  #23011 ) ;
#28901 = CARTESIAN_POINT ( 'NONE',  ( 57.18398860626899705, 28.73617430169827358, 5.000000000000000000 ) ) ;
#28902 = DIRECTION ( 'NONE',  ( 1.248002500702738701E-15, 1.000000000000000000, -0.000000000000000000 ) ) ;
#28903 = DIRECTION ( 'NONE',  ( -0.6830127018922181881, 0.6830127018922202975, -0.2588190451025214056 ) ) ;
#28904 = CARTESIAN_POINT ( 'NONE',  ( 20.99999999999985079, -6.033600742197678279, 5.000000000000000000 ) ) ;
#28905 = CARTESIAN_POINT ( 'NONE',  ( 27.10373647476855652, 5.808823158059036373, 5.808823158059032821 ) ) ;
#28906 = CARTESIAN_POINT ( 'NONE',  ( 8.437069808101885116, 2.126176841940952134, -7.934999999999992504 ) ) ;
#28907 = DIRECTION ( 'NONE',  ( -1.000000000000000000, -0.000000000000000000, -0.000000000000000000 ) ) ;
#28908 = CARTESIAN_POINT ( 'NONE',  ( 6.328169399223488867, -12.74070752338414891, 4.000000000000000000 ) ) ;
#28909 = LINE ( 'NONE', #39814, #84847 ) ;
#28910 = ORIENTED_EDGE ( 'NONE', *, *, #75838, .T. ) ;
#28911 = ADVANCED_FACE ( 'NONE', ( #50979 ), #105340, .F. ) ;
#28912 = AXIS2_PLACEMENT_3D ( 'NONE', #98532, #142758, #42035 ) ;
#28913 = ORIENTED_EDGE ( 'NONE', *, *, #40905, .T. ) ;
#28914 = CARTESIAN_POINT ( 'NONE',  ( 82.08333333333334281, 6.884901960086290629, -3.974999999999994316 ) ) ;
#28915 = PRESENTATION_STYLE_ASSIGNMENT (( #6384 ) ) ;
#28916 = ORIENTED_EDGE ( 'NONE', *, *, #11523, .F. ) ;
#28917 = CARTESIAN_POINT ( 'NONE',  ( 92.39169371712955581, 2.130196079827421762, 7.950000000000000178 ) ) ;
#28918 = CARTESIAN_POINT ( 'NONE',  ( -51.18398860626899705, 28.73617430169823095, 5.000000000000000000 ) ) ;
#28919 = ORIENTED_EDGE ( 'NONE', *, *, #77214, .T. ) ;
#28920 = CARTESIAN_POINT ( 'NONE',  ( -23.03457404400602115, 22.22500000000000142, 0.4942731178105737033 ) ) ;
#28921 = FACE_OUTER_BOUND ( 'NONE', #53055, .T. ) ;
#28922 = CARTESIAN_POINT ( 'NONE',  ( 15.52000000000000135, 9.521314400968980422E-16, 0.000000000000000000 ) ) ;
#28923 = DIRECTION ( 'NONE',  ( -1.000000000000000000, -1.224606353822377258E-16, -0.000000000000000000 ) ) ;
#28924 = FACE_OUTER_BOUND ( 'NONE', #44545, .T. ) ;
#28925 = DIRECTION ( 'NONE',  ( -0.000000000000000000, 0.3543493200069153248, 0.9351131265310292928 ) ) ;
#28926 = PLANE ( 'NONE',  #119745 ) ;
#28927 = DIRECTION ( 'NONE',  ( 0.7071067811865487940, -0.7071067811865463515, 0.000000000000000000 ) ) ;
#28928 = DIRECTION ( 'NONE',  ( 0.6830127018922181881, 0.6830127018922202975, -0.2588190451025214056 ) ) ;
#28929 = CARTESIAN_POINT ( 'NONE',  ( -72.48921356237309510, -27.52281430457106026, 5.000000000000000000 ) ) ;
#28930 = DIRECTION ( 'NONE',  ( -0.7071067811865486830, -0.7071067811865464625, -0.000000000000000000 ) ) ;
#28931 = DIRECTION ( 'NONE',  ( -0.000000000000000000, 0.3543493200069153248, 0.9351131265310292928 ) ) ;
#28932 = ADVANCED_FACE ( 'NONE', ( #61872 ), #103199, .F. ) ;
#28933 = VECTOR ( 'NONE', #23763, 1000.000000000000000 ) ;
#28934 = ORIENTED_EDGE ( 'NONE', *, *, #18742, .F. ) ;
#28935 = ORIENTED_EDGE ( 'NONE', *, *, #137551, .T. ) ;
#28936 = ADVANCED_FACE ( 'NONE', ( #61190 ), #40133, .F. ) ;
#28937 = CARTESIAN_POINT ( 'NONE',  ( 100.0420968585647756, 5.291415217122923842, -3.054999999999996163 ) ) ;
#28938 = ORIENTED_EDGE ( 'NONE', *, *, #25508, .T. ) ;
#28939 = ADVANCED_FACE ( 'NONE', ( #82208 ), #116228, .T. ) ;
#28940 = VECTOR ( 'NONE', #82446, 1000.000000000000000 ) ;
#28941 = DIRECTION ( 'NONE',  ( -0.7071067811865487940, 0.7071067811865463515, 0.000000000000000000 ) ) ;
#28942 = CARTESIAN_POINT ( 'NONE',  ( 7.875000000000000000, -6.094999999999989981, 3.732111120401553285E-16 ) ) ;
#28943 = ORIENTED_EDGE ( 'NONE', *, *, #111896, .T. ) ;
#28944 = ADVANCED_FACE ( 'NONE', ( #15442 ), #115469, .F. ) ;
#28945 = ADVANCED_FACE ( 'NONE', ( #114084 ), #38673, .F. ) ;
#28946 = CARTESIAN_POINT ( 'NONE',  ( -16.78678096696630817, 12.75929247661558996, 10.29404684609031406 ) ) ;
#28947 = CARTESIAN_POINT ( 'NONE',  ( 13.18000000000000149, 9.521314400968980422E-16, 0.000000000000000000 ) ) ;
#28948 = CARTESIAN_POINT ( 'NONE',  ( 97.62043019189812298, 3.055000000000001936, -5.291415217122916737 ) ) ;
#28949 = VECTOR ( 'NONE', #138368, 1000.000000000000000 ) ;
#28950 = ORIENTED_EDGE ( 'NONE', *, *, #29725, .F. ) ;
#28951 = DIRECTION ( 'NONE',  ( -0.3543493200069162685, -0.000000000000000000, -0.9351131265310288487 ) ) ;
#28952 = ORIENTED_EDGE ( 'NONE', *, *, #127623, .T. ) ;
#28953 = LINE ( 'NONE', #18762, #66199 ) ;
#28954 = LINE ( 'NONE', #85446, #102487 ) ;
#28955 = FACE_OUTER_BOUND ( 'NONE', #6408, .T. ) ;
#28956 = ORIENTED_EDGE ( 'NONE', *, *, #14225, .T. ) ;
#28957 = VERTEX_POINT ( 'NONE', #27785 ) ;
#28958 = EDGE_CURVE ( 'NONE', #132946, #18156, #59048, .T. ) ;
#28959 = VERTEX_POINT ( 'NONE', #71313 ) ;
#28960 = PLANE ( 'NONE',  #2820 ) ;
#28961 = EDGE_CURVE ( 'NONE', #63922, #17176, #3846, .T. ) ;
#28962 = DIRECTION ( 'NONE',  ( 0.7071067811865487940, 0.7071067811865463515, -0.000000000000000000 ) ) ;
#28963 = CARTESIAN_POINT ( 'NONE',  ( 4.442069808101886785, 7.934999999999992504, 2.126176841940951689 ) ) ;
#28964 = CARTESIAN_POINT ( 'NONE',  ( 0.000000000000000000, 0.000000000000000000, 5.000000000000000000 ) ) ;
#28965 = EDGE_CURVE ( 'NONE', #36826, #96824, #92311, .T. ) ;
#28966 = AXIS2_PLACEMENT_3D ( 'NONE', #129839, #8032, #108049 ) ;
#28967 = AXIS2_PLACEMENT_3D ( 'NONE', #88775, #45987, #22739 ) ;
#28968 = VECTOR ( 'NONE', #117238, 1000.000000000000000 ) ;
#28969 = ORIENTED_EDGE ( 'NONE', *, *, #475, .F. ) ;
#28971 = ORIENTED_EDGE ( 'NONE', *, *, #116301, .T. ) ;
#28970 = VECTOR ( 'NONE', #83226, 1000.000000000000000 ) ;
#28972 = CARTESIAN_POINT ( 'NONE',  ( -16.49999999999988276, -16.53360074219757792, 5.000000000000000000 ) ) ;
#28973 = EDGE_LOOP ( 'NONE', ( #136955, #58489, #56650, #14898 ) ) ;
#28974 = ORIENTED_EDGE ( 'NONE', *, *, #38437, .F. ) ;
#28975 = ADVANCED_FACE ( 'NONE', ( #16159 ), #72781, .F. ) ;
#28976 = CARTESIAN_POINT ( 'NONE',  ( 113.6620968585647944, -5.291415217122919401, 3.054999999999997939 ) ) ;
#28977 = CYLINDRICAL_SURFACE ( 'NONE', #60545, 4.749999999999997335 ) ;
#28978 = CARTESIAN_POINT ( 'NONE',  ( 27.70710678118635428, 20.25929247661551003, 5.000000000000000000 ) ) ;
#28979 = ORIENTED_EDGE ( 'NONE', *, *, #81092, .T. ) ;
#28980 = CARTESIAN_POINT ( 'NONE',  ( 6.416666666666666963, 5.278424836066147208, 3.047499999999990550 ) ) ;
#28981 = DIRECTION ( 'NONE',  ( 0.7071067811865487940, 0.7071067811865463515, -0.000000000000000000 ) ) ;
#28982 = ADVANCED_FACE ( 'NONE', ( #137991 ), #82903, .T. ) ;
#28983 = FACE_OUTER_BOUND ( 'NONE', #102915, .T. ) ;
#28984 = DIRECTION ( 'NONE',  ( -1.000000000000000000, -1.224606353822377258E-16, -0.000000000000000000 ) ) ;
#28985 = ORIENTED_EDGE ( 'NONE', *, *, #45474, .T. ) ;
#28986 = CARTESIAN_POINT ( 'NONE',  ( -24.87485380690750958, -14.24070752338413470, 9.401115078912718914 ) ) ;
#28987 = DIRECTION ( 'NONE',  ( -0.6830127018922180770, -0.6830127018922204085, -0.2588190451025213501 ) ) ;
#28988 = EDGE_LOOP ( 'NONE', ( #95949, #27343, #59455, #103944 ) ) ;
#28989 = DIRECTION ( 'NONE',  ( -0.7071067811865487940, 0.7071067811865463515, -0.000000000000000000 ) ) ;
#28990 = DIRECTION ( 'NONE',  ( -0.000000000000000000, 0.000000000000000000, 1.000000000000000000 ) ) ;
#28991 = DIRECTION ( 'NONE',  ( 1.000000000000000000, 0.000000000000000000, 0.000000000000000000 ) ) ;
#28992 = EDGE_LOOP ( 'NONE', ( #140431, #65810, #50911, #116049 ) ) ;
#28993 = EDGE_CURVE ( 'NONE', #15118, #23170, #44446, .T. ) ;
#28994 = CARTESIAN_POINT ( 'NONE',  ( -6.005480084712508493, 28.92564299267933947, 4.000000000000000000 ) ) ;
#28995 = VERTEX_POINT ( 'NONE', #140811 ) ;
#28996 = ORIENTED_EDGE ( 'NONE', *, *, #68249, .F. ) ;
#28997 = VERTEX_POINT ( 'NONE', #131393 ) ;
#28998 = EDGE_CURVE ( 'NONE', #59037, #122865, #64708, .T. ) ;
#28999 = CARTESIAN_POINT ( 'NONE',  ( 31.12043019189811233, 3.055000000000001936, -5.291415217122916737 ) ) ;
#29000 = B_SPLINE_CURVE_WITH_KNOTS ( 'NONE', 3,
 ( #117250, #65635, #49912, #84664 ),
 .UNSPECIFIED., .F., .F.,
 ( 4, 4 ),
 ( 0.000000000000000000, 0.001824211539880447918 ),
 .UNSPECIFIED. ) ;
#29001 = DIRECTION ( 'NONE',  ( 0.000000000000000000, -1.000000000000000000, 0.000000000000000000 ) ) ;
#29002 = LINE ( 'NONE', #140598, #93540 ) ;
#29003 = DIRECTION ( 'NONE',  ( 0.000000000000000000, -1.000000000000000000, 0.000000000000000000 ) ) ;
#29004 = CARTESIAN_POINT ( 'NONE',  ( 3.469446951953614189E-15, -10.44781430457072169, 5.000000000000000000 ) ) ;
#29005 = CARTESIAN_POINT ( 'NONE',  ( -15.32816939922342137, -18.74070752338409562, 4.000000000000000000 ) ) ;
#29006 = CARTESIAN_POINT ( 'NONE',  ( 33.48921356237309510, -27.52281430457078670, 5.000000000000000000 ) ) ;
#29007 = CARTESIAN_POINT ( 'NONE',  ( -11.99451991528749417, 28.92564299267946382, 4.000000000000000000 ) ) ;
#29008 = CARTESIAN_POINT ( 'NONE',  ( 21.75860074219781382, 21.72500000000000142, 5.000000000000000000 ) ) ;
#29009 = CARTESIAN_POINT ( 'NONE',  ( -66.18398860626901126, 28.73617430169833753, 5.000000000000000000 ) ) ;
#29010 = PLANE ( 'NONE',  #742 ) ;
#29011 = EDGE_CURVE ( 'NONE', #39017, #86313, #22176, .T. ) ;
#29012 = EDGE_LOOP ( 'NONE', ( #37244, #13283, #85090, #13761 ) ) ;
#29013 = ORIENTED_EDGE ( 'NONE', *, *, #143542, .F. ) ;
#29014 = VERTEX_POINT ( 'NONE', #119069 ) ;
#29015 = ORIENTED_EDGE ( 'NONE', *, *, #126649, .F. ) ;
#29016 = CARTESIAN_POINT ( 'NONE',  ( -1.311990357131797014, 0.1751088764723762181, 3.778756969498452634 ) ) ;
#29017 = ORIENTED_EDGE ( 'NONE', *, *, #44256, .T. ) ;
#29018 = ORIENTED_EDGE ( 'NONE', *, *, #56853, .F. ) ;
#29019 = CARTESIAN_POINT ( 'NONE',  ( 13.49159235450332162, 2.500000000000001776, 0.000000000000000000 ) ) ;
#29020 = CARTESIAN_POINT ( 'NONE',  ( 6.489213562373093325, -27.52281430457059841, 5.000000000000000000 ) ) ;
#29021 = ADVANCED_FACE ( 'NONE', ( #63995 ), #49094, .T. ) ;
#29022 = DIRECTION ( 'NONE',  ( 0.7071067811865487940, -0.7071067811865463515, 0.000000000000000000 ) ) ;
#29023 = ORIENTED_EDGE ( 'NONE', *, *, #86749, .F. ) ;
#29024 = FACE_OUTER_BOUND ( 'NONE', #130903, .T. ) ;
#29025 = ORIENTED_EDGE ( 'NONE', *, *, #58671, .F. ) ;
#29026 =( BOUNDED_CURVE ( )  B_SPLINE_CURVE ( 2, ( #3832, #94448, #127078, #27055, #70616, #103878, #104619, #92298, #17590 ),
 .UNSPECIFIED., .F., .T. ) 
 B_SPLINE_CURVE_WITH_KNOTS ( ( 3, 2, 2, 2, 3 ),
 ( 0.7000000000000000666, 0.7083333333333334814, 0.7166666666666666741, 0.7249999999999999778, 0.7257331639278409297 ),
 .UNSPECIFIED. ) 
 CURVE ( )  GEOMETRIC_REPRESENTATION_ITEM ( )  RATIONAL_B_SPLINE_CURVE ( ( 0.9999999999999995559, 0.9659258262890687563, 1.000000000000000000, 0.9659258262890683122, 1.000000000000000000, 0.9659258262890683122, 1.000000000000000000, 0.9970021653956989693, 0.9945318277978396626 ) ) 
 REPRESENTATION_ITEM ( '' )  );
#29027 = CARTESIAN_POINT ( 'NONE',  ( -33.48921356237309510, -27.52281430457078670, 5.000000000000000000 ) ) ;
#29028 = AXIS2_PLACEMENT_3D ( 'NONE', #35588, #143051, #110398 ) ;
#29029 = LINE ( 'NONE', #63814, #82094 ) ;
#29030 = CARTESIAN_POINT ( 'NONE',  ( 13.04623647476855375, -7.934999999999990727, 4.858786175617117713E-16 ) ) ;
#29031 = ORIENTED_EDGE ( 'NONE', *, *, #79683, .T. ) ;
#29032 = CARTESIAN_POINT ( 'NONE',  ( 102.1412635252314232, 4.472830434245837594, 4.472830434245841147 ) ) ;
#29033 = TOROIDAL_SURFACE ( 'NONE', #128592, 4.000000000000000000, 1.000000000000000000 ) ;
#29034 = FACE_OUTER_BOUND ( 'NONE', #70638, .T. ) ;
#29035 = CARTESIAN_POINT ( 'NONE',  ( -20.99451991528748707, 28.92564299267952777, 4.000000000000000000 ) ) ;
#29036 = ORIENTED_EDGE ( 'NONE', *, *, #25073, .T. ) ;
#29037 = VERTEX_POINT ( 'NONE', #73451 ) ;
#29038 = LINE ( 'NONE', #119581, #81974 ) ;
#29039 = ORIENTED_EDGE ( 'NONE', *, *, #51281, .F. ) ;
#29040 =( NAMED_UNIT ( * ) PLANE_ANGLE_UNIT ( ) SI_UNIT ( $, .RADIAN. ) );
#29041 = LINE ( 'NONE', #74713, #90484 ) ;
#29042 = CARTESIAN_POINT ( 'NONE',  ( 0.000000000000000000, -30.18000000000009564, -15.92500000000064375 ) ) ;
#29043 = DIRECTION ( 'NONE',  ( -0.000000000000000000, -0.3543493200069152693, 0.9351131265310292928 ) ) ;
#29044 = ORIENTED_EDGE ( 'NONE', *, *, #116994, .F. ) ;
#29045 = LINE ( 'NONE', #70463, #82958 ) ;
#29046 = VECTOR ( 'NONE', #113575, 999.9999999999998863 ) ;
#29047 = EDGE_CURVE ( 'NONE', #132587, #24646, #108165, .T. ) ;
#29048 = LINE ( 'NONE', #51531, #9537 ) ;
#29049 = DIRECTION ( 'NONE',  ( -0.3543493200069162685, -0.000000000000000000, -0.9351131265310288487 ) ) ;
#29050 = ORIENTED_EDGE ( 'NONE', *, *, #127103, .T. ) ;
#29051 = CARTESIAN_POINT ( 'NONE',  ( 15.52000000000000135, 9.521314400968980422E-16, 0.000000000000000000 ) ) ;
#29052 = LINE ( 'NONE', #94296, #128071 ) ;
#29053 = ORIENTED_EDGE ( 'NONE', *, *, #118928, .T. ) ;
#29054 = EDGE_CURVE ( 'NONE', #2836, #94406, #119761, .T. ) ;
#29056 = ORIENTED_EDGE ( 'NONE', *, *, #131077, .F. ) ;
#29055 = CARTESIAN_POINT ( 'NONE',  ( 4.969723521325230209, -2.055000000000000160, 0.000000000000000000 ) ) ;
#29058 = VERTEX_POINT ( 'NONE', #29915 ) ;
#29057 = ADVANCED_FACE ( 'NONE', ( #87165 ), #10302, .F. ) ;
#29059 = DIRECTION ( 'NONE',  ( -0.3543493200069162685, -0.000000000000000000, -0.9351131265310288487 ) ) ;
#29060 = DIRECTION ( 'NONE',  ( -0.7071067811865487940, 0.7071067811865463515, 0.000000000000000000 ) ) ;
#29061 = VERTEX_POINT ( 'NONE', #9577 ) ;
#29062 = CARTESIAN_POINT ( 'NONE',  ( 29.99999999999979750, 4.552185695429124657, 5.000000000000000000 ) ) ;
#29063 = AXIS2_PLACEMENT_3D ( 'NONE', #139857, #15856, #28927 ) ;
#29064 = DIRECTION ( 'NONE',  ( 0.7071067811865486830, -0.7071067811865464625, -0.000000000000000000 ) ) ;
#29065 = AXIS2_PLACEMENT_3D ( 'NONE', #79799, #134141, #58788 ) ;
#29066 = LINE ( 'NONE', #37823, #41452 ) ;
#29068 = EDGE_CURVE ( 'NONE', #18156, #133583, #62022, .T. ) ;
#29067 = AXIS2_PLACEMENT_3D ( 'NONE', #117941, #7769, #129558 ) ;
#29069 = LINE ( 'NONE', #62428, #39225 ) ;
#29070 = DIRECTION ( 'NONE',  ( 0.6830127018922181881, 0.6830127018922202975, -0.2588190451025214056 ) ) ;
#29071 = DIRECTION ( 'NONE',  ( 0.7071067811865486830, -0.7071067811865464625, -0.000000000000000000 ) ) ;
#29072 = LINE ( 'NONE', #95015, #132766 ) ;
#29073 = LINE ( 'NONE', #85572, #51215 ) ;
#29074 = CARTESIAN_POINT ( 'NONE',  ( -35.99451991528749772, 28.92564299267963079, 4.000000000000000000 ) ) ;
#29075 = LINE ( 'NONE', #18153, #39117 ) ;
#29076 =( GEOMETRIC_REPRESENTATION_CONTEXT ( 3 ) GLOBAL_UNCERTAINTY_ASSIGNED_CONTEXT ( ( #134627 ) ) GLOBAL_UNIT_ASSIGNED_CONTEXT ( ( #53307, #131601, #26927 ) ) REPRESENTATION_CONTEXT ( 'NONE', 'WORKASPACE' ) );
#29077 = DIRECTION ( 'NONE',  ( -0.7071067811865486830, -0.7071067811865464625, -0.000000000000000000 ) ) ;
#29078 = LINE ( 'NONE', #63169, #15268 ) ;
#29079 = ORIENTED_EDGE ( 'NONE', *, *, #17404, .T. ) ;
#29080 = EDGE_CURVE ( 'NONE', #25013, #109867, #5314, .T. ) ;
#29081 = ORIENTED_EDGE ( 'NONE', *, *, #37812, .F. ) ;
#29082 = ORIENTED_EDGE ( 'NONE', *, *, #82507, .T. ) ;
#29083 = CARTESIAN_POINT ( 'NONE',  ( 108.1874999999999858, -5.819803920172573086, 5.819803920172572198 ) ) ;
#29084 = ORIENTED_EDGE ( 'NONE', *, *, #24015, .T. ) ;
#29085 = ORIENTED_EDGE ( 'NONE', *, *, #63832, .T. ) ;
#29086 = EDGE_LOOP ( 'NONE', ( #48411, #142742, #1845, #112967 ) ) ;
#29087 = DIRECTION ( 'NONE',  ( -0.7071067811865486830, -0.7071067811865464625, 0.000000000000000000 ) ) ;
#29088 = PLANE ( 'NONE',  #120284 ) ;
#29089 = VERTEX_POINT ( 'NONE', #120462 ) ;
#29090 = CARTESIAN_POINT ( 'NONE',  ( -20.99451991528748707, 28.92564299267952777, 4.000000000000000000 ) ) ;
#29091 = FILL_AREA_STYLE_COLOUR ( '', #34904 ) ;
#29092 = CARTESIAN_POINT ( 'NONE',  ( -26.51078643762690845, -27.52281430457036748, 5.000000000000000000 ) ) ;
#29093 = PLANE ( 'NONE',  #136830 ) ;
#29094 = CARTESIAN_POINT ( 'NONE',  ( 101.9379301918980900, -6.110000000000001208, 1.637169565754158951 ) ) ;
#29095 = ORIENTED_EDGE ( 'NONE', *, *, #44765, .T. ) ;
#29096 = DIRECTION ( 'NONE',  ( 0.6830127018922181881, 0.6830127018922202975, -0.2588190451025214056 ) ) ;
#29097 = FILL_AREA_STYLE ('',( #129114 ) ) ;
#29098 = FACE_OUTER_BOUND ( 'NONE', #137865, .T. ) ;
#29099 = DIRECTION ( 'NONE',  ( -0.6830127018922180770, -0.6830127018922204085, -0.2588190451025213501 ) ) ;
#29100 = LINE ( 'NONE', #126967, #67743 ) ;
#29101 = LINE ( 'NONE', #83502, #45449 ) ;
#29102 = CARTESIAN_POINT ( 'NONE',  ( 38.57919371712956291, 3.975000000000002753, -6.884901960086283523 ) ) ;
#29103 = DIRECTION ( 'NONE',  ( -0.7071067811865486830, -0.7071067811865464625, 0.000000000000000000 ) ) ;
#29104 = DIRECTION ( 'NONE',  ( -0.7071067811865486830, 0.7071067811865464625, 0.000000000000000000 ) ) ;
#29105 = VERTEX_POINT ( 'NONE', #85722 ) ;
#29106 = ORIENTED_EDGE ( 'NONE', *, *, #87858, .T. ) ;
#29107 = EDGE_CURVE ( 'NONE', #100020, #39592, #69916, .T. ) ;
#29108 = CARTESIAN_POINT ( 'NONE',  ( 30.45833333333332504, 3.974999999999997424, 6.884901960086288852 ) ) ;
#29109 = EDGE_LOOP ( 'NONE', ( #124401, #25581, #27731, #135144, #122577 ) ) ;
#29110 = FACE_OUTER_BOUND ( 'NONE', #42224, .T. ) ;
#29111 = EDGE_CURVE ( 'NONE', #11920, #72701, #42258, .T. ) ;
#29112 = DIRECTION ( 'NONE',  ( -0.7071067811865487940, 0.7071067811865463515, 0.000000000000000000 ) ) ;
#29113 = FACE_OUTER_BOUND ( 'NONE', #50822, .T. ) ;
#29114 = EDGE_CURVE ( 'NONE', #74762, #36287, #53850, .T. ) ;
#29115 = EDGE_CURVE ( 'NONE', #76368, #119902, #108881, .T. ) ;
#29116 = FILL_AREA_STYLE_COLOUR ( '', #32561 ) ;
#29117 = CARTESIAN_POINT ( 'NONE',  ( 125.3287635252314516, 0.000000000000000000, -6.109999999999998543 ) ) ;
#29118 = ORIENTED_EDGE ( 'NONE', *, *, #3650, .F. ) ;
#29119 = DIRECTION ( 'NONE',  ( -0.6830127018922181881, 0.6830127018922202975, -0.2588190451025214056 ) ) ;
#29120 = ORIENTED_EDGE ( 'NONE', *, *, #53699, .F. ) ;
#29121 = CARTESIAN_POINT ( 'NONE',  ( 6.489213562373093325, -27.52281430457059841, 5.000000000000000000 ) ) ;
#29122 = ADVANCED_FACE ( 'NONE', ( #18302 ), #11712, .F. ) ;
#29123 = LINE ( 'NONE', #4439, #24502 ) ;
#29124 = FACE_OUTER_BOUND ( 'NONE', #54895, .T. ) ;
#29125 = VERTEX_POINT ( 'NONE', #46573 ) ;
#29127 = EDGE_CURVE ( 'NONE', #2713, #36832, #21902, .T. ) ;
#29126 = CARTESIAN_POINT ( 'NONE',  ( 46.95876352523143993, 0.000000000000000000, -6.110000000000001208 ) ) ;
#29128 = VERTEX_POINT ( 'NONE', #132844 ) ;
#29129 = FACE_OUTER_BOUND ( 'NONE', #100487, .T. ) ;
#29130 = EDGE_CURVE ( 'NONE', #84298, #99644, #134253, .T. ) ;
#29131 = DIRECTION ( 'NONE',  ( -1.000000000000000000, -1.224606353822377258E-16, -0.000000000000000000 ) ) ;
#29132 = DIRECTION ( 'NONE',  ( -0.000000000000000000, -0.000000000000000000, -1.000000000000000000 ) ) ;
#29133 = DIRECTION ( 'NONE',  ( 1.055184596092948005E-16, -1.000000000000000000, 0.000000000000000000 ) ) ;
#29134 = AXIS2_PLACEMENT_3D ( 'NONE', #14503, #36961, #115921 ) ;
#29135 = EDGE_CURVE ( 'NONE', #10533, #49354, #13857, .T. ) ;
#29136 = ADVANCED_FACE ( 'NONE', ( #90762 ), #55262, .F. ) ;
#29137 = CARTESIAN_POINT ( 'NONE',  ( 51.09959685856477307, -6.109999999999997655, -1.637169565754160283 ) ) ;
#29138 = ORIENTED_EDGE ( 'NONE', *, *, #1616, .F. ) ;
#29139 = VECTOR ( 'NONE', #79287, 1000.000000000000000 ) ;
#29140 = PLANE ( 'NONE',  #14105 ) ;
#29141 = CARTESIAN_POINT ( 'NONE',  ( 7.940000000000001279, -60.26999999999998892, -10.00000000000000178 ) ) ;
#29142 = EDGE_LOOP ( 'NONE', ( #18223, #129781, #58495, #9357 ) ) ;
#29143 = ORIENTED_EDGE ( 'NONE', *, *, #48732, .F. ) ;
#29144 = ADVANCED_FACE ( 'NONE', ( #34221 ), #58154, .F. ) ;
#29145 = ORIENTED_EDGE ( 'NONE', *, *, #12462, .T. ) ;
#29146 = CARTESIAN_POINT ( 'NONE',  ( 60.30836038379622011, 7.949999999999996625, 2.130196079827431088 ) ) ;
#29147 = VERTEX_POINT ( 'NONE', #35688 ) ;
#29148 = CARTESIAN_POINT ( 'NONE',  ( 43.53752705046289151, -9.735942053221456900E-16, 7.949999999999998401 ) ) ;
#29149 = ADVANCED_FACE ( 'NONE', ( #111026 ), #24760, .F. ) ;
#29150 = LINE ( 'NONE', #72718, #122926 ) ;
#29151 = FACE_BOUND ( 'NONE', #9802, .T. ) ;
#29152 = DIRECTION ( 'NONE',  ( 0.000000000000000000, 0.000000000000000000, -1.000000000000000000 ) ) ;
#29153 = EDGE_LOOP ( 'NONE', ( #83382, #22458, #141075, #139896, #84020 ) ) ;
#29154 =( NAMED_UNIT ( * ) SI_UNIT ( $, .STERADIAN. ) SOLID_ANGLE_UNIT ( ) );
#29155 = ORIENTED_EDGE ( 'NONE', *, *, #78013, .F. ) ;
#29156 = EDGE_CURVE ( 'NONE', #78146, #68546, #37499, .T. ) ;
#29157 = EDGE_LOOP ( 'NONE', ( #102316, #12140, #1136, #138097 ) ) ;
#29158 = LINE ( 'NONE', #85668, #98063 ) ;
#29159 = AXIS2_PLACEMENT_3D ( 'NONE', #43219, #142532, #65718 ) ;
#29160 = EDGE_LOOP ( 'NONE', ( #57089, #51356, #33410, #108398 ) ) ;
#29161 = ADVANCED_FACE ( 'NONE', ( #3001 ), #121908, .F. ) ;
#29162 = VECTOR ( 'NONE', #112727, 1000.000000000000000 ) ;
#29163 = CARTESIAN_POINT ( 'NONE',  ( 57.07876352523144448, -7.482591942790325086E-16, 6.109999999999998543 ) ) ;
#29164 = VERTEX_POINT ( 'NONE', #45134 ) ;
#29165 = VECTOR ( 'NONE', #117447, 1000.000000000000000 ) ;
#29166 = PLANE ( 'NONE',  #25535 ) ;
#29167 = AXIS2_PLACEMENT_3D ( 'NONE', #69613, #114493, #125400 ) ;
#29168 = CARTESIAN_POINT ( 'NONE',  ( 47.99451991528749062, 28.92564299267971251, 4.000000000000000000 ) ) ;
#29169 = VERTEX_POINT ( 'NONE', #79912 ) ;
#29170 = FACE_OUTER_BOUND ( 'NONE', #53316, .T. ) ;
#29171 = VECTOR ( 'NONE', #100055, 1000.000000000000000 ) ;
#29172 = EDGE_CURVE ( 'NONE', #74481, #127430, #89312, .T. ) ;
#29173 = CARTESIAN_POINT ( 'NONE',  ( 0.000000000000000000, 2.342191155542447500, -5.001666872980086609 ) ) ;
#29174 = CARTESIAN_POINT ( 'NONE',  ( 100.7500000000000000, -9.735942053221458872E-16, 7.950000000000000178 ) ) ;
#29175 = CARTESIAN_POINT ( 'NONE',  ( 6.183988606268994381, 28.73617430169791476, 5.000000000000000000 ) ) ;
#29176 = PLANE ( 'NONE',  #69420 ) ;
#29177 = VERTEX_POINT ( 'NONE', #123397 ) ;
#29178 = ORIENTED_EDGE ( 'NONE', *, *, #92806, .F. ) ;
#29179 = CARTESIAN_POINT ( 'NONE',  ( -26.67183060077628198, -18.74070752338408852, 4.000000000000000000 ) ) ;
#29180 = CARTESIAN_POINT ( 'NONE',  ( 8.500000000000000000, 9.521314400968980422E-16, 0.000000000000000000 ) ) ;
#29181 = ORIENTED_EDGE ( 'NONE', *, *, #89204, .F. ) ;
#29182 = ORIENTED_EDGE ( 'NONE', *, *, #107976, .F. ) ;
#29183 = ORIENTED_EDGE ( 'NONE', *, *, #129141, .T. ) ;
#29184 = DIRECTION ( 'NONE',  ( -0.6830127018922181881, 0.6830127018922202975, -0.2588190451025214056 ) ) ;
#29185 = CARTESIAN_POINT ( 'NONE',  ( 55.64169371712955581, -2.130196079827424871, -7.949999999999998401 ) ) ;
#29186 = LINE ( 'NONE', #106728, #16058 ) ;
#29187 = ORIENTED_EDGE ( 'NONE', *, *, #24514, .T. ) ;
#29188 = LINE ( 'NONE', #84998, #50948 ) ;
#29189 = CARTESIAN_POINT ( 'NONE',  ( -66.29974487139159578, -27.71228299555252406, 4.000000000000000000 ) ) ;
#29190 = CARTESIAN_POINT ( 'NONE',  ( 13.62956980810188767, -3.967499999999998028, -6.871911579029511330 ) ) ;
#29191 = FACE_OUTER_BOUND ( 'NONE', #11822, .T. ) ;
#29192 = ORIENTED_EDGE ( 'NONE', *, *, #28961, .T. ) ;
#29193 = CARTESIAN_POINT ( 'NONE',  ( 128.0995968585647802, -6.109999999999998543, -1.637169565754160727 ) ) ;
#29195 = EDGE_CURVE ( 'NONE', #23129, #54018, #45830, .T. ) ;
#29194 = LINE ( 'NONE', #95161, #109120 ) ;
#29196 = DIRECTION ( 'NONE',  ( 0.6830127018922181881, 0.6830127018922202975, -0.2588190451025214056 ) ) ;
#29198 = ORIENTED_EDGE ( 'NONE', *, *, #124363, .F. ) ;
#29197 = DIRECTION ( 'NONE',  ( -0.000000000000000000, -0.3543493200069152693, 0.9351131265310292928 ) ) ;
#29199 = VECTOR ( 'NONE', #128079, 1000.000000000000000 ) ;
#29200 = CARTESIAN_POINT ( 'NONE',  ( 10.54580628287044064, 5.278424836066143655, -3.047499999999997655 ) ) ;
#29201 = VERTEX_POINT ( 'NONE', #23310 ) ;
#29202 = CARTESIAN_POINT ( 'NONE',  ( 76.35002705046288440, -5.819803920172573086, -5.819803920172573086 ) ) ;
#29203 = CARTESIAN_POINT ( 'NONE',  ( -34.43312800248720862, -21.74070752338405299, 6.915939825044155498 ) ) ;
#29204 = CARTESIAN_POINT ( 'NONE',  ( -20.67183060077632817, 20.25929247661551003, 4.000000000000000000 ) ) ;
#29205 = ORIENTED_EDGE ( 'NONE', *, *, #119689, .F. ) ;
#29206 = PLANE ( 'NONE',  #142119 ) ;
#29207 = PLANE ( 'NONE',  #104342 ) ;
#29208 = DIRECTION ( 'NONE',  ( 0.000000000000000000, -1.000000000000000000, 0.000000000000000000 ) ) ;
#29209 = ORIENTED_EDGE ( 'NONE', *, *, #72650, .T. ) ;
#29210 = DIRECTION ( 'NONE',  ( -0.7071067811865486830, -0.7071067811865464625, 0.000000000000000000 ) ) ;
#29211 = LINE ( 'NONE', #129231, #111855 ) ;
#29212 = CARTESIAN_POINT ( 'NONE',  ( 10.94186803553636977, 3.821174125832445049E-16, 0.000000000000000000 ) ) ;
#29213 = CARTESIAN_POINT ( 'NONE',  ( -23.99999999999982947, 10.21212019023806938, -2.019456568337744340 ) ) ;
#29214 = FACE_OUTER_BOUND ( 'NONE', #79830, .T. ) ;
#29215 = EDGE_CURVE ( 'NONE', #80017, #1190, #67592, .T. ) ;
#29216 = ORIENTED_EDGE ( 'NONE', *, *, #114038, .T. ) ;
#29217 = VERTEX_POINT ( 'NONE', #24059 ) ;
#29218 = DIRECTION ( 'NONE',  ( -0.3543493200069162685, -0.000000000000000000, -0.9351131265310288487 ) ) ;
#29219 = DIRECTION ( 'NONE',  ( 0.000000000000000000, -1.000000000000000000, 0.000000000000000000 ) ) ;
#29220 = ADVANCED_FACE ( 'NONE', ( #12448 ), #79230, .T. ) ;
#29221 = ADVANCED_FACE ( 'NONE', ( #1544 ), #68317, .F. ) ;
#29222 = EDGE_CURVE ( 'NONE', #4021, #3523, #124085, .T. ) ;
#29223 = CARTESIAN_POINT ( 'NONE',  ( 14.85373647476855474, -5.808823158059035485, -5.808823158059033709 ) ) ;
#29224 = AXIS2_PLACEMENT_3D ( 'NONE', #77172, #130832, #63443 ) ;
#29225 = CARTESIAN_POINT ( 'NONE',  ( 27.29974487139158512, -27.71228299555225405, 4.000000000000000000 ) ) ;
#29226 = DIRECTION ( 'NONE',  ( 0.7071067811865487940, 0.7071067811865463515, 0.000000000000000000 ) ) ;
#29227 = CARTESIAN_POINT ( 'NONE',  ( -25.39999999999996305, 3.061616997868383141E-16, -2.500000000000000000 ) ) ;
#29228 = VECTOR ( 'NONE', #61457, 1000.000000000000000 ) ;
#29229 = ORIENTED_EDGE ( 'NONE', *, *, #33893, .T. ) ;
#29230 = EDGE_CURVE ( 'NONE', #47662, #56422, #61016, .T. ) ;
#29231 = CARTESIAN_POINT ( 'NONE',  ( 9.994118527364397764, 4.584330080086930965E-16, 0.000000000000000000 ) ) ;
#29232 = FACE_OUTER_BOUND ( 'NONE', #139304, .T. ) ;
#29233 = DIRECTION ( 'NONE',  ( -0.000000000000000000, 0.000000000000000000, 1.000000000000000000 ) ) ;
#29234 = CARTESIAN_POINT ( 'NONE',  ( 49.20376352523145158, 6.109999999999999432, 1.122388791418549108E-15 ) ) ;
#29235 = CARTESIAN_POINT ( 'NONE',  ( 33.29974487139158867, -27.71228299555229313, 4.000000000000000000 ) ) ;
#29236 = EDGE_CURVE ( 'NONE', #91335, #35930, #49411, .T. ) ;
#29237 = ORIENTED_EDGE ( 'NONE', *, *, #100509, .T. ) ;
#29238 = CARTESIAN_POINT ( 'NONE',  ( -17.20710678118642178, -17.24070752338410628, 5.000000000000000000 ) ) ;
#29239 = ORIENTED_EDGE ( 'NONE', *, *, #115112, .T. ) ;
#29240 = STYLED_ITEM ( 'NONE', ( #16645 ), #33681 ) ;
#29241 = ORIENTED_EDGE ( 'NONE', *, *, #1291, .T. ) ;
#29242 = FACE_OUTER_BOUND ( 'NONE', #46405, .T. ) ;
#29243 = EDGE_CURVE ( 'NONE', #88659, #1800, #131452, .T. ) ;
#29244 = CARTESIAN_POINT ( 'NONE',  ( -18.79289321881332242, -17.24070752338410628, 5.000000000000000000 ) ) ;
#29245 = LINE ( 'NONE', #137319, #104454 ) ;
#29246 = LINE ( 'NONE', #141597, #131972 ) ;
#29247 = VECTOR ( 'NONE', #105751, 1000.000000000000000 ) ;
#29248 = DIRECTION ( 'NONE',  ( -0.000000000000000000, 0.3543493200069153248, 0.9351131265310292928 ) ) ;
#29249 = DIRECTION ( 'NONE',  ( -1.000000000000000000, -0.000000000000000000, -0.000000000000000000 ) ) ;
#29250 = ORIENTED_EDGE ( 'NONE', *, *, #51672, .T. ) ;
#29251 = LINE ( 'NONE', #106800, #122711 ) ;
#29252 = DIRECTION ( 'NONE',  ( 0.7071067811865487940, -0.7071067811865463515, 0.000000000000000000 ) ) ;
#29253 = EDGE_CURVE ( 'NONE', #84504, #75919, #113913, .T. ) ;
#29254 = DIRECTION ( 'NONE',  ( -0.6830127018922181881, 0.6830127018922202975, -0.2588190451025214056 ) ) ;
#29255 = DIRECTION ( 'NONE',  ( -1.000000000000000000, -0.000000000000000000, -0.000000000000000000 ) ) ;
#29256 = CARTESIAN_POINT ( 'NONE',  ( -2.999999999999975131, 8.587461875839162317, 4.000000000000000000 ) ) ;
#29257 = VECTOR ( 'NONE', #95970, 999.9999999999998863 ) ;
#29258 = CARTESIAN_POINT ( 'NONE',  ( 17.99999999999986855, -16.02097659208068947, -11.96015758381212635 ) ) ;
#29259 = VECTOR ( 'NONE', #10393, 1000.000000000000000 ) ;
#29260 = CARTESIAN_POINT ( 'NONE',  ( 67.01669371712957002, 7.950000000000001066, -2.130196079827421318 ) ) ;
#29261 = AXIS2_PLACEMENT_3D ( 'NONE', #119662, #10210, #142190 ) ;
#29262 = LINE ( 'NONE', #85784, #53048 ) ;
#29263 = ORIENTED_EDGE ( 'NONE', *, *, #15031, .F. ) ;
#29264 = EDGE_LOOP ( 'NONE', ( #128488, #53735, #2650, #4408 ) ) ;
#29265 = CARTESIAN_POINT ( 'NONE',  ( 54.95833333333332860, 3.974999999999997424, 6.884901960086288852 ) ) ;
#29266 = DIRECTION ( 'NONE',  ( -0.7071067811865487940, 0.7071067811865463515, -0.000000000000000000 ) ) ;
#29267 = CARTESIAN_POINT ( 'NONE',  ( -11.99999999999991829, 15.45873954670184425, -0.03131636524291228629 ) ) ;
#29268 = EDGE_CURVE ( 'NONE', #26466, #116177, #17446, .T. ) ;
#29269 = VECTOR ( 'NONE', #123791, 999.9999999999998863 ) ;
#29270 = EDGE_LOOP ( 'NONE', ( #77679, #94603, #11526, #43728 ) ) ;
#29272 = ADVANCED_FACE ( 'NONE', ( #50100 ), #38503, .T. ) ;
#29271 = DIRECTION ( 'NONE',  ( 0.7071067811865487940, 0.7071067811865463515, 0.000000000000000000 ) ) ;
#29273 = EDGE_CURVE ( 'NONE', #106882, #35724, #126903, .T. ) ;
#29274 = CARTESIAN_POINT ( 'NONE',  ( 57.16709685856477563, -3.055000000000000160, -5.291415217122921177 ) ) ;
#29275 = ORIENTED_EDGE ( 'NONE', *, *, #99785, .T. ) ;
#29276 = PLANE ( 'NONE',  #27093 ) ;
#29277 = EDGE_LOOP ( 'NONE', ( #35352, #141861, #104013, #132838 ) ) ;
#29278 = ORIENTED_EDGE ( 'NONE', *, *, #143093, .T. ) ;
#29279 = CARTESIAN_POINT ( 'NONE',  ( -8.999999999999932498, -19.06887692260762890, 4.000000000000000000 ) ) ;
#29280 = ADVANCED_FACE ( 'NONE', ( #26201 ), #27604, .F. ) ;
#29281 = LINE ( 'NONE', #51053, #59321 ) ;
#29282 = CARTESIAN_POINT ( 'NONE',  ( 16.49999999999987921, -14.56887692260766087, 4.000000000000000000 ) ) ;
#29283 = FACE_OUTER_BOUND ( 'NONE', #102109, .T. ) ;
#29284 = EDGE_CURVE ( 'NONE', #95787, #97600, #92822, .T. ) ;
#29285 = LINE ( 'NONE', #61950, #21085 ) ;
#29287 = ORIENTED_EDGE ( 'NONE', *, *, #123795, .T. ) ;
#29286 = DIRECTION ( 'NONE',  ( 0.6830127018922180770, -0.6830127018922204085, -0.2588190451025213501 ) ) ;
#29288 = LINE ( 'NONE', #92388, #136374 ) ;
#29289 = DIRECTION ( 'NONE',  ( -0.7071067811865486830, -0.7071067811865464625, 0.000000000000000000 ) ) ;
#29290 = PLANE ( 'NONE',  #88834 ) ;
#29291 = CARTESIAN_POINT ( 'NONE',  ( 31.17183060077626067, 6.759292476615651246, 4.000000000000000000 ) ) ;
#29292 = LINE ( 'NONE', #27869, #15949 ) ;
#29293 = VERTEX_POINT ( 'NONE', #70466 ) ;
#29294 = ORIENTED_EDGE ( 'NONE', *, *, #115392, .T. ) ;
#29295 = VECTOR ( 'NONE', #106543, 1000.000000000000000 ) ;
#29296 = EDGE_CURVE ( 'NONE', #130144, #29014, #37061, .T. ) ;
#29297 = DIRECTION ( 'NONE',  ( 1.000000000000000000, 0.000000000000000000, 0.000000000000000000 ) ) ;
#29298 = CARTESIAN_POINT ( 'NONE',  ( 72.24543019189810877, -5.291415217122918513, -3.055000000000000160 ) ) ;
#29299 = FACE_OUTER_BOUND ( 'NONE', #18751, .T. ) ;
#29300 = CARTESIAN_POINT ( 'NONE',  ( 21.29159235450332233, 9.902892378096218942E-16, 0.000000000000000000 ) ) ;
#29301 = LINE ( 'NONE', #127184, #66424 ) ;
#29302 = ORIENTED_EDGE ( 'NONE', *, *, #103890, .F. ) ;
#29303 = ORIENTED_EDGE ( 'NONE', *, *, #105533, .T. ) ;
#29304 = AXIS2_PLACEMENT_3D ( 'NONE', #130587, #142178, #120355 ) ;
#29305 = LINE ( 'NONE', #139545, #114035 ) ;
#29306 = EDGE_CURVE ( 'NONE', #58487, #67480, #103042, .T. ) ;
#29307 = ORIENTED_EDGE ( 'NONE', *, *, #36295, .T. ) ;
#29308 = EDGE_LOOP ( 'NONE', ( #96162, #49571, #37612 ) ) ;
#29309 = DIRECTION ( 'NONE',  ( -0.000000000000000000, 0.000000000000000000, 1.000000000000000000 ) ) ;
#29310 = ORIENTED_EDGE ( 'NONE', *, *, #125828, .T. ) ;
#29311 = PLANE ( 'NONE',  #24808 ) ;
#29312 = VECTOR ( 'NONE', #138022, 1000.000000000000227 ) ;
#29313 = DIRECTION ( 'NONE',  ( 0.3543493200069162685, -0.000000000000000000, -0.9351131265310288487 ) ) ;
#29314 = AXIS2_PLACEMENT_3D ( 'NONE', #63766, #52152, #19522 ) ;
#29315 = FACE_BOUND ( 'NONE', #33159, .T. ) ;
#29316 = CARTESIAN_POINT ( 'NONE',  ( 3.712309939660257019, -21.73547319004780576, 4.999917730833663754 ) ) ;
#29317 = PLANE ( 'NONE',  #140593 ) ;
#29319 = ORIENTED_EDGE ( 'NONE', *, *, #84093, .F. ) ;
#29318 = FACE_OUTER_BOUND ( 'NONE', #17177, .T. ) ;
#29320 = DIRECTION ( 'NONE',  ( 0.000000000000000000, -0.000000000000000000, -1.000000000000000000 ) ) ;
#29321 = APPLICATION_PROTOCOL_DEFINITION ( 'draft international standard', 'automotive_design', 1998, #16032 ) ;
#29323 = EDGE_LOOP ( 'NONE', ( #133820, #131552, #37666, #76725 ) ) ;
#29322 = AXIS2_PLACEMENT_3D ( 'NONE', #4497, #94419, #72742 ) ;
#29324 = ORIENTED_EDGE ( 'NONE', *, *, #15251, .T. ) ;
#29325 = CARTESIAN_POINT ( 'NONE',  ( 87.41209685856478018, 5.291415217122921177, -3.054999999999994831 ) ) ;
#29326 = ORIENTED_EDGE ( 'NONE', *, *, #116199, .F. ) ;
#29327 = VECTOR ( 'NONE', #22866, 1000.000000000000000 ) ;
#29328 = FACE_OUTER_BOUND ( 'NONE', #111433, .T. ) ;
#29329 = DIRECTION ( 'NONE',  ( 0.6830127018922180770, -0.6830127018922204085, -0.2588190451025213501 ) ) ;
#29330 = CARTESIAN_POINT ( 'NONE',  ( 0.000000000000000000, 0.000000000000000000, 5.000000000000000000 ) ) ;
#29331 = LINE ( 'NONE', #4672, #19342 ) ;
#29332 = CARTESIAN_POINT ( 'NONE',  ( 0.000000000000000000, 0.000000000000000000, 5.000000000000000000 ) ) ;
#29333 = VECTOR ( 'NONE', #138281, 999.9999999999998863 ) ;
#29334 = CARTESIAN_POINT ( 'NONE',  ( 19.49999999999987566, 16.08746187583907883, 4.000000000000000000 ) ) ;
#29335 = DIRECTION ( 'NONE',  ( -0.7071067811865486830, -0.7071067811865464625, 0.000000000000000000 ) ) ;
#29336 = LINE ( 'NONE', #112963, #120999 ) ;
#29337 = PLANE ( 'NONE',  #85628 ) ;
#29338 = DIRECTION ( 'NONE',  ( -0.000000000000000000, -0.3543493200069152693, 0.9351131265310292928 ) ) ;
#29339 = EDGE_LOOP ( 'NONE', ( #90565, #23411, #67983, #100894, #80237 ) ) ;
#29340 = DIRECTION ( 'NONE',  ( -0.3543493200069162685, -0.000000000000000000, -0.9351131265310288487 ) ) ;
#29341 = CARTESIAN_POINT ( 'NONE',  ( 26.99451991528749417, 28.92564299267956685, 4.000000000000000000 ) ) ;
#29342 = VERTEX_POINT ( 'NONE', #104451 ) ;
#29344 = EDGE_LOOP ( 'NONE', ( #49264, #113481, #81724, #34504 ) ) ;
#29343 = VECTOR ( 'NONE', #56978, 999.9999999999998863 ) ;
#29345 = VERTEX_POINT ( 'NONE', #61702 ) ;
#29346 = CARTESIAN_POINT ( 'NONE',  ( 33.25043019189810423, 3.055000000000002824, -5.291415217122919401 ) ) ;
#29347 = EDGE_LOOP ( 'NONE', ( #138341, #5452, #46189, #48276 ) ) ;
#29348 = AXIS2_PLACEMENT_3D ( 'NONE', #28794, #73035, #115741 ) ;
#29349 = VECTOR ( 'NONE', #17836, 1000.000000000000227 ) ;
#29350 = CARTESIAN_POINT ( 'NONE',  ( 16.96247294953710849, -7.464222240803106570E-16, -6.094999999999989981 ) ) ;
#29351 = CARTESIAN_POINT ( 'NONE',  ( 6.205262656257519716, 11.46168650470408146, -26.04351286206016525 ) ) ;
#29352 = VERTEX_POINT ( 'NONE', #48667 ) ;
#29353 = DIRECTION ( 'NONE',  ( 0.7071067811865487940, 0.7071067811865463515, 0.000000000000000000 ) ) ;
#29354 = VECTOR ( 'NONE', #73171, 999.9999999999998863 ) ;
#29355 = ORIENTED_EDGE ( 'NONE', *, *, #48898, .T. ) ;
#29357 = EDGE_CURVE ( 'NONE', #129322, #88587, #125520, .T. ) ;
#29356 = DIRECTION ( 'NONE',  ( 0.6830127018922180770, -0.6830127018922204085, -0.2588190451025213501 ) ) ;
#29358 = VECTOR ( 'NONE', #52450, 1000.000000000000227 ) ;
#29359 = CYLINDRICAL_SURFACE ( 'NONE', #38281, 7.950000000000000178 ) ;
#29361 = VERTEX_POINT ( 'NONE', #105173 ) ;
#29360 = CARTESIAN_POINT ( 'NONE',  ( 25.49999999999982236, -12.66682484999664382, -0.6294897503863351451 ) ) ;
#29362 = ORIENTED_EDGE ( 'NONE', *, *, #125455, .F. ) ;
#29363 = DIRECTION ( 'NONE',  ( 0.6830127018922180770, -0.6830127018922204085, -0.2588190451025213501 ) ) ;
#29364 = ORIENTED_EDGE ( 'NONE', *, *, #89336, .T. ) ;
#29365 = CARTESIAN_POINT ( 'NONE',  ( -18.48921356237309510, -27.52281430457068367, 5.000000000000000000 ) ) ;
#29366 = ORIENTED_EDGE ( 'NONE', *, *, #39044, .T. ) ;
#29367 = ORIENTED_EDGE ( 'NONE', *, *, #22778, .F. ) ;
#29368 = ORIENTED_EDGE ( 'NONE', *, *, #123024, .F. ) ;
#29369 = ORIENTED_EDGE ( 'NONE', *, *, #49478, .F. ) ;
#29370 = EDGE_CURVE ( 'NONE', #40283, #34938, #114611, .T. ) ;
#29371 = EDGE_CURVE ( 'NONE', #28471, #25993, #92864, .T. ) ;
#29372 = DIRECTION ( 'NONE',  ( 0.000000000000000000, 1.000000000000000000, 0.000000000000000000 ) ) ;
#29373 = DIRECTION ( 'NONE',  ( -0.000000000000000000, 0.3543493200069153248, 0.9351131265310292928 ) ) ;
#29374 = PLANE ( 'NONE',  #83900 ) ;
#29375 = EDGE_CURVE ( 'NONE', #925, #110223, #60275, .T. ) ;
#29376 = CARTESIAN_POINT ( 'NONE',  ( 0.000000000000000000, 0.000000000000000000, 5.000000000000000000 ) ) ;
#29377 = PLANE ( 'NONE',  #76080 ) ;
#29378 = ADVANCED_FACE ( 'NONE', ( #91464 ), #39217, .T. ) ;
#29380 = ORIENTED_EDGE ( 'NONE', *, *, #46707, .T. ) ;
#29379 = EDGE_CURVE ( 'NONE', #134283, #93966, #124788, .T. ) ;
#29381 = DIRECTION ( 'NONE',  ( -0.7071067811865486830, -0.7071067811865464625, 0.000000000000000000 ) ) ;
#29382 = VERTEX_POINT ( 'NONE', #73286 ) ;
#29383 = VECTOR ( 'NONE', #66654, 1000.000000000000000 ) ;
#29384 = LINE ( 'NONE', #17778, #84158 ) ;
#29385 = ADVANCED_FACE ( 'NONE', ( #97110 ), #30484, .F. ) ;
#29386 = EDGE_CURVE ( 'NONE', #104249, #13451, #8667, .T. ) ;
#29387 = DIRECTION ( 'NONE',  ( 0.7071067811865487940, 0.7071067811865463515, 0.000000000000000000 ) ) ;
#29388 = LINE ( 'NONE', #62764, #94813 ) ;
#29389 = AXIS2_PLACEMENT_3D ( 'NONE', #26370, #89470, #111959 ) ;
#29390 = ORIENTED_EDGE ( 'NONE', *, *, #87813, .F. ) ;
#29391 = CARTESIAN_POINT ( 'NONE',  ( 96.22916666666667140, 7.950000000000001954, -2.130196079827421762 ) ) ;
#29392 =( BOUNDED_CURVE ( )  B_SPLINE_CURVE ( 3, ( #132468, #97644, #107791, #75216 ),
 .UNSPECIFIED., .F., .T. ) 
 B_SPLINE_CURVE_WITH_KNOTS ( ( 4, 4 ),
 ( 5.005968288816728951, 5.074607125596330093 ),
 .UNSPECIFIED. ) 
 CURVE ( )  GEOMETRIC_REPRESENTATION_ITEM ( )  RATIONAL_B_SPLINE_CURVE ( ( 1.000000000000000000, 0.9996074310407765395, 0.9996074310407765395, 1.000000000000000000 ) ) 
 REPRESENTATION_ITEM ( '' )  );
#29393 = SURFACE_STYLE_FILL_AREA ( #54055 ) ;
#29394 = VERTEX_POINT ( 'NONE', #9391 ) ;
#29395 = ORIENTED_EDGE ( 'NONE', *, *, #43913, .T. ) ;
#29396 = EDGE_CURVE ( 'NONE', #112859, #2047, #106572, .T. ) ;
#29397 = VERTEX_POINT ( 'NONE', #107999 ) ;
#29398 = CARTESIAN_POINT ( 'NONE',  ( 63.18398860626900415, 28.73617430169831621, 5.000000000000000000 ) ) ;
#29399 = DIRECTION ( 'NONE',  ( -0.6830127018922181881, 0.6830127018922202975, -0.2588190451025214056 ) ) ;
#29400 = DIRECTION ( 'NONE',  ( 0.3543493200069162685, -0.000000000000000000, -0.9351131265310288487 ) ) ;
#29401 = AXIS2_PLACEMENT_3D ( 'NONE', #76011, #118791, #75316 ) ;
#29402 = CARTESIAN_POINT ( 'NONE',  ( 12.71230993966019085, -21.73547319004782352, 4.999917730833663754 ) ) ;
#29403 = CARTESIAN_POINT ( 'NONE',  ( 0.3252437201535152145, -48.93522302958430004, -39.28544916627528494 ) ) ;
#29404 = CARTESIAN_POINT ( 'NONE',  ( 76.91209685856479439, 5.291415217122922066, -3.054999999999995275 ) ) ;
#29405 = DIRECTION ( 'NONE',  ( -1.000000000000000000, -1.224606353822377258E-16, -0.000000000000000000 ) ) ;
#29406 = EDGE_CURVE ( 'NONE', #38491, #137243, #52907, .T. ) ;
#29407 = DIRECTION ( 'NONE',  ( -0.000000000000000000, 0.000000000000000000, 1.000000000000000000 ) ) ;
#29408 = LINE ( 'NONE', #73643, #25657 ) ;
#29409 = DIRECTION ( 'NONE',  ( -1.000000000000000000, -1.224606353822377258E-16, -0.000000000000000000 ) ) ;
#29410 = PLANE ( 'NONE',  #139064 ) ;
#29411 = COLOUR_RGB ( '', 0.08235294, 0.09019608, 0.10196078) ;
#29412 = ORIENTED_EDGE ( 'NONE', *, *, #87590, .T. ) ;
#29413 = CARTESIAN_POINT ( 'NONE',  ( 27.48921356237309155, -27.52281430457074762, 5.000000000000000000 ) ) ;
#29414 = ORIENTED_EDGE ( 'NONE', *, *, #125989, .F. ) ;
#29415 = CARTESIAN_POINT ( 'NONE',  ( 12.82439460721831104, -2.055000000000000160, 0.000000000000000000 ) ) ;
#29417 = ORIENTED_EDGE ( 'NONE', *, *, #78563, .F. ) ;
#29416 = CARTESIAN_POINT ( 'NONE',  ( -54.48921356237310221, -27.52281430457093236, 5.000000000000000000 ) ) ;
#29418 = DIRECTION ( 'NONE',  ( -0.7071067811865486830, -0.7071067811865464625, 0.000000000000000000 ) ) ;
#29419 = DIRECTION ( 'NONE',  ( -1.000000000000000000, -0.000000000000000000, -0.000000000000000000 ) ) ;
#29420 = VERTEX_POINT ( 'NONE', #53673 ) ;
#29421 = VERTEX_POINT ( 'NONE', #107311 ) ;
#29422 = LINE ( 'NONE', #95399, #132046 ) ;
#29423 = CARTESIAN_POINT ( 'NONE',  ( 18.29974487139159223, -27.71228299555219010, 4.000000000000000000 ) ) ;
#29424 = EDGE_CURVE ( 'NONE', #17542, #37203, #18125, .T. ) ;
#29425 = LINE ( 'NONE', #85962, #12572 ) ;
#29426 = CARTESIAN_POINT ( 'NONE',  ( 96.62086038379621300, -6.884901960086286188, 3.974999999999997424 ) ) ;
#29427 = CARTESIAN_POINT ( 'NONE',  ( 57.48921356237308800, -27.52281430457095368, 5.000000000000000000 ) ) ;
#29428 = DIRECTION ( 'NONE',  ( -0.7071067811865486830, 0.7071067811865464625, -0.000000000000000000 ) ) ;
#29429 = VERTEX_POINT ( 'NONE', #86301 ) ;
#29430 = LINE ( 'NONE', #129462, #63165 ) ;
#29431 = CARTESIAN_POINT ( 'NONE',  ( 12.69999999999999574, -35.15000000000000568, -39.79289321881344677 ) ) ;
#29432 = CARTESIAN_POINT ( 'NONE',  ( 32.08333333333333570, -5.278424836066144543, 3.047499999999995879 ) ) ;
#29433 = ADVANCED_FACE ( 'NONE', ( #97877 ), #128374, .F. ) ;
#29434 = CARTESIAN_POINT ( 'NONE',  ( 32.99999999999977263, -15.03360074219758502, 5.000000000000000000 ) ) ;
#29435 = VERTEX_POINT ( 'NONE', #52222 ) ;
#29436 = DIRECTION ( 'NONE',  ( 1.000000000000000000, 0.000000000000000000, 0.000000000000000000 ) ) ;
#29437 = ADVANCED_FACE ( 'NONE', ( #96408 ), #7982, .F. ) ;
#29438 = EDGE_LOOP ( 'NONE', ( #79816, #11326, #93145, #119497 ) ) ;
#29439 = CARTESIAN_POINT ( 'NONE',  ( 83.27126352523143282, 4.472830434245839371, 4.472830434245842035 ) ) ;
#29440 = EDGE_CURVE ( 'NONE', #28258, #34677, #7258, .T. ) ;
#29441 = CARTESIAN_POINT ( 'NONE',  ( -66.18398860626901126, 28.73617430169833753, 5.000000000000000000 ) ) ;
#29442 = PLANE ( 'NONE',  #128080 ) ;
#29443 = ORIENTED_EDGE ( 'NONE', *, *, #27435, .F. ) ;
#29444 = CARTESIAN_POINT ( 'NONE',  ( 0.000000000000000000, 0.000000000000000000, 5.000000000000000000 ) ) ;
#29445 = ADVANCED_FACE ( 'NONE', ( #84854 ), #85547, .T. ) ;
#29446 = EDGE_CURVE ( 'NONE', #125983, #4875, #118899, .T. ) ;
#29447 = FACE_OUTER_BOUND ( 'NONE', #89601, .T. ) ;
#29448 = AXIS2_PLACEMENT_3D ( 'NONE', #105086, #128285, #73201 ) ;
#29449 = DIRECTION ( 'NONE',  ( 0.6830127018922180770, -0.6830127018922204085, -0.2588190451025213501 ) ) ;
#29451 = ORIENTED_EDGE ( 'NONE', *, *, #54693, .F. ) ;
#29450 = FACE_OUTER_BOUND ( 'NONE', #66709, .T. ) ;
#29452 = CARTESIAN_POINT ( 'NONE',  ( 13.56250000000000178, 4.461849672132300881, 4.461849672132299105 ) ) ;
#29453 = DIRECTION ( 'NONE',  ( -1.000000000000000000, -1.224606353822377258E-16, -0.000000000000000000 ) ) ;
#29454 = FACE_OUTER_BOUND ( 'NONE', #123258, .T. ) ;
#29455 = EDGE_CURVE ( 'NONE', #19220, #77121, #131216, .T. ) ;
#29456 = VECTOR ( 'NONE', #74265, 999.9999999999998863 ) ;
#29457 =( NAMED_UNIT ( * ) PLANE_ANGLE_UNIT ( ) SI_UNIT ( $, .RADIAN. ) );
#29458 = AXIS2_PLACEMENT_3D ( 'NONE', #20202, #20926, #108627 ) ;
#29459 = ORIENTED_EDGE ( 'NONE', *, *, #104302, .T. ) ;
#29460 = ORIENTED_EDGE ( 'NONE', *, *, #86165, .T. ) ;
#29461 =( GEOMETRIC_REPRESENTATION_CONTEXT ( 3 ) GLOBAL_UNCERTAINTY_ASSIGNED_CONTEXT ( ( #35895 ) ) GLOBAL_UNIT_ASSIGNED_CONTEXT ( ( #35580, #112392, #79810 ) ) REPRESENTATION_CONTEXT ( 'NONE', 'WORKASPACE' ) );
#29462 = CARTESIAN_POINT ( 'NONE',  ( 71.89626352523144703, 4.472830434245840259, -4.472830434245839371 ) ) ;
#29463 = ORIENTED_EDGE ( 'NONE', *, *, #81058, .T. ) ;
#29464 = ADVANCED_FACE ( 'NONE', ( #73984 ), #40651, .F. ) ;
#29465 = LINE ( 'NONE', #19317, #137916 ) ;
#29467 = LINE ( 'NONE', #64989, #20242 ) ;
#29466 = AXIS2_PLACEMENT_3D ( 'NONE', #89568, #123659, #21466 ) ;
#29468 = CARTESIAN_POINT ( 'NONE',  ( 13.49999999999991473, 10.46639925780215918, 5.000000000000000000 ) ) ;
#29469 = ORIENTED_EDGE ( 'NONE', *, *, #54246, .T. ) ;
#29470 = PLANE ( 'NONE',  #125437 ) ;
#29471 = DIRECTION ( 'NONE',  ( 0.7071067811865486830, -0.7071067811865464625, -0.000000000000000000 ) ) ;
#29472 = VERTEX_POINT ( 'NONE', #19591 ) ;
#29473 = FACE_OUTER_BOUND ( 'NONE', #100522, .T. ) ;
#29474 = CARTESIAN_POINT ( 'NONE',  ( 29.99999999999979039, 2.966399257802232459, 5.000000000000000000 ) ) ;
#29475 = CARTESIAN_POINT ( 'NONE',  ( 19.56363873141800624, -2.772201803466310288, 4.368625942145807350 ) ) ;
#29476 = ORIENTED_EDGE ( 'NONE', *, *, #108014, .F. ) ;
#29477 = VERTEX_POINT ( 'NONE', #120293 ) ;
#29478 = ADVANCED_FACE ( 'NONE', ( #20288 ), #64527, .F. ) ;
#29479 = CARTESIAN_POINT ( 'NONE',  ( 34.49999999999976552, 3.431123077392151277, 4.000000000000000000 ) ) ;
#29480 = LINE ( 'NONE', #6983, #18432 ) ;
#29481 = CARTESIAN_POINT ( 'NONE',  ( -21.48921356237309155, -27.52281430457070499, 5.000000000000000000 ) ) ;
#29482 = LINE ( 'NONE', #73717, #30155 ) ;
#29483 = VECTOR ( 'NONE', #78594, 999.9999999999998863 ) ;
#29484 = DIRECTION ( 'NONE',  ( 0.000000000000000000, -1.000000000000000000, 0.000000000000000000 ) ) ;
#29485 = CARTESIAN_POINT ( 'NONE',  ( -17.99999999999986855, -19.06887692260762179, 4.000000000000000000 ) ) ;
#29486 = ORIENTED_EDGE ( 'NONE', *, *, #140798, .T. ) ;
#29487 = EDGE_CURVE ( 'NONE', #138729, #13798, #94989, .T. ) ;
#29488 = ORIENTED_EDGE ( 'NONE', *, *, #125044, .T. ) ;
#29489 = ORIENTED_EDGE ( 'NONE', *, *, #51248, .T. ) ;
#29490 = ORIENTED_EDGE ( 'NONE', *, *, #106636, .F. ) ;
#29491 = AXIS2_PLACEMENT_3D ( 'NONE', #1795, #46837, #56278 ) ;
#29492 = CARTESIAN_POINT ( 'NONE',  ( 183.4813685602585167, -52.14999999947626463, 41.03936837847149377 ) ) ;
#29493 = ADVANCED_FACE ( 'NONE', ( #65993 ), #12280, .F. ) ;
#29494 = DIRECTION ( 'NONE',  ( 0.6830127018922180770, -0.6830127018922204085, -0.2588190451025213501 ) ) ;
#29496 = ADVANCED_FACE ( 'NONE', ( #46392 ), #123295, .T. ) ;
#29495 =( LENGTH_UNIT ( ) NAMED_UNIT ( * ) SI_UNIT ( .MILLI., .METRE. ) );
#29497 = VERTEX_POINT ( 'NONE', #77575 ) ;
#29498 = LINE ( 'NONE', #117912, #27463 ) ;
#29499 = DIRECTION ( 'NONE',  ( -1.000000000000000000, -1.224606353822377258E-16, -0.000000000000000000 ) ) ;
#29500 = LINE ( 'NONE', #50557, #3917 ) ;
#29501 = VECTOR ( 'NONE', #143551, 1000.000000000000227 ) ;
#29502 = CARTESIAN_POINT ( 'NONE',  ( -19.49999999999986144, -20.53675388469232388, 2.352720554255848473 ) ) ;
#29503 = CARTESIAN_POINT ( 'NONE',  ( 26.99999999999999289, -4.294289084967417125, -4.784050195499812475 ) ) ;
#29504 = ORIENTED_EDGE ( 'NONE', *, *, #36629, .F. ) ;
#29505 = CARTESIAN_POINT ( 'NONE',  ( -0.4892135623730947680, -27.52281430457055578, 5.000000000000000000 ) ) ;
#29506 = LINE ( 'NONE', #87485, #27991 ) ;
#29508 = ORIENTED_EDGE ( 'NONE', *, *, #14514, .T. ) ;
#29507 = VECTOR ( 'NONE', #3456, 1000.000000000000000 ) ;
#29509 = CARTESIAN_POINT ( 'NONE',  ( -9.707106781186462641, -15.74070752338412760, 5.000000000000000000 ) ) ;
#29510 = ORIENTED_EDGE ( 'NONE', *, *, #137017, .F. ) ;
#29511 = ADVANCED_FACE ( 'NONE', ( #10830 ), #35513, .F. ) ;
#29512 = DIRECTION ( 'NONE',  ( -1.000000000000000000, -1.224606353822377258E-16, -0.000000000000000000 ) ) ;
#29513 = ORIENTED_EDGE ( 'NONE', *, *, #107815, .F. ) ;
#29514 = CARTESIAN_POINT ( 'NONE',  ( 71.60459685856476142, 1.637169565754164946, -6.109999999999999432 ) ) ;
#29515 = ORIENTED_EDGE ( 'NONE', *, *, #58435, .F. ) ;
#29516 = VERTEX_POINT ( 'NONE', #78276 ) ;
#29517 = DIRECTION ( 'NONE',  ( -0.7071067811865487940, 0.7071067811865463515, -0.000000000000000000 ) ) ;
#29518 = CARTESIAN_POINT ( 'NONE',  ( 8.212472949537106715, 0.000000000000000000, 6.094999999999989981 ) ) ;
#29519 = VECTOR ( 'NONE', #105796, 1000.000000000000000 ) ;
#29520 = CARTESIAN_POINT ( 'NONE',  ( 113.6045968585647614, 1.637169565754164946, -6.109999999999999432 ) ) ;
#29521 = CARTESIAN_POINT ( 'NONE',  ( -24.48921356237309510, -27.52281430457072631, 5.000000000000000000 ) ) ;
#29522 = FACE_OUTER_BOUND ( 'NONE', #48888, .T. ) ;
#29523 = FACE_OUTER_BOUND ( 'NONE', #62583, .T. ) ;
#29524 = CARTESIAN_POINT ( 'NONE',  ( -34.92500000000001137, 3.701285051063773146, 12.01932804697901069 ) ) ;
#29525 = CARTESIAN_POINT ( 'NONE',  ( 39.18398860626899705, 28.73617430169814568, 5.000000000000000000 ) ) ;
#29526 = DIRECTION ( 'NONE',  ( -0.000000000000000000, 0.000000000000000000, 1.000000000000000000 ) ) ;
#29527 = CARTESIAN_POINT ( 'NONE',  ( 77.37086038379622721, 6.884901960086289741, -3.974999999999993427 ) ) ;
#29528 = ORIENTED_EDGE ( 'NONE', *, *, #73192, .F. ) ;
#29529 = DIRECTION ( 'NONE',  ( -0.000000000000000000, 0.000000000000000000, 1.000000000000000000 ) ) ;
#29530 = FACE_OUTER_BOUND ( 'NONE', #110773, .T. ) ;
#29531 = ORIENTED_EDGE ( 'NONE', *, *, #26154, .T. ) ;
#29532 = ORIENTED_EDGE ( 'NONE', *, *, #4445, .T. ) ;
#29533 = VERTEX_POINT ( 'NONE', #44974 ) ;
#29534 = EDGE_CURVE ( 'NONE', #5176, #16100, #34062, .T. ) ;
#29535 = ORIENTED_EDGE ( 'NONE', *, *, #2538, .T. ) ;
#29536 = COLOUR_RGB ( '', 0.40784314, 0.44705882, 0.49803922) ;
#29537 = EDGE_CURVE ( 'NONE', #15997, #123054, #67412, .T. ) ;
#29538 = PLANE ( 'NONE',  #39959 ) ;
#29539 = LINE ( 'NONE', #111202, #73299 ) ;
#29540 = VECTOR ( 'NONE', #52672, 1000.000000000000000 ) ;
#29541 = CARTESIAN_POINT ( 'NONE',  ( 29.29289321881325137, -15.74070752338412049, 5.000000000000000000 ) ) ;
#29542 = ADVANCED_FACE ( 'NONE', ( #44228 ), #90579, .F. ) ;
#29543 = ORIENTED_EDGE ( 'NONE', *, *, #101901, .F. ) ;
#29544 = CARTESIAN_POINT ( 'NONE',  ( -2.554855379167821863E-16, -50.22575108204303973, 35.38524182944719598 ) ) ;
#29545 = ORIENTED_EDGE ( 'NONE', *, *, #70339, .T. ) ;
#29546 = VECTOR ( 'NONE', #138470, 1000.000000000000227 ) ;
#29547 = VECTOR ( 'NONE', #10936, 1000.000000000000000 ) ;
#29548 = EDGE_CURVE ( 'NONE', #5611, #2635, #681, .T. ) ;
#29549 = EDGE_CURVE ( 'NONE', #78241, #123918, #43493, .T. ) ;
#29550 = CARTESIAN_POINT ( 'NONE',  ( 1.291236474768552966, -9.717572351234235426E-16, -7.934999999999990727 ) ) ;
#29551 = CARTESIAN_POINT ( 'NONE',  ( 34.49999999999975842, 1.464255608400477415, 4.994342998332161443 ) ) ;
#29552 = EDGE_CURVE ( 'NONE', #131572, #138628, #56566, .T. ) ;
#29553 = DIRECTION ( 'NONE',  ( 0.6830127018922181881, 0.6830127018922202975, -0.2588190451025214056 ) ) ;
#29554 = CARTESIAN_POINT ( 'NONE',  ( 32.99999999999977973, 7.588810512006247677, -3.013526669885301601 ) ) ;
#29555 = ORIENTED_EDGE ( 'NONE', *, *, #74468, .T. ) ;
#29556 = VERTEX_POINT ( 'NONE', #111605 ) ;
#29557 = ADVANCED_FACE ( 'NONE', ( #24585 ), #89149, .T. ) ;
#29558 = ORIENTED_EDGE ( 'NONE', *, *, #131646, .F. ) ;
#29559 = LINE ( 'NONE', #73797, #23248 ) ;
#29560 = DIRECTION ( 'NONE',  ( 1.000000000000000000, 0.000000000000000000, 0.000000000000000000 ) ) ;
#29561 = ADVANCED_FACE ( 'NONE', ( #12979 ), #110846, .T. ) ;
#29562 = DIRECTION ( 'NONE',  ( -0.000000000000000000, -0.3543493200069152693, 0.9351131265310292928 ) ) ;
#29563 = DIRECTION ( 'NONE',  ( 1.000000000000000000, 0.000000000000000000, 0.000000000000000000 ) ) ;
#29564 = CARTESIAN_POINT ( 'NONE',  ( 3.250000000000000000, -4.999999999999999112, -7.627214432543508948 ) ) ;
#29565 = DIRECTION ( 'NONE',  ( 0.7071067811865486830, -0.7071067811865464625, -0.000000000000000000 ) ) ;
#29566 = LINE ( 'NONE', #98926, #69635 ) ;
#29567 = EDGE_CURVE ( 'NONE', #56571, #136567, #122459, .T. ) ;
#29568 = LINE ( 'NONE', #15113, #108719 ) ;
#29569 = CARTESIAN_POINT ( 'NONE',  ( 28.87543019189810067, -5.291415217122920289, -3.055000000000001492 ) ) ;
#29570 = CARTESIAN_POINT ( 'NONE',  ( -12.71757738642558877, -21.73023691814493219, 5.000000000000000888 ) ) ;
#29571 = CARTESIAN_POINT ( 'NONE',  ( -15.29974487139158867, -27.71228299555216879, 4.000000000000000000 ) ) ;
#29572 = ORIENTED_EDGE ( 'NONE', *, *, #112869, .T. ) ;
#29573 = CARTESIAN_POINT ( 'NONE',  ( 26.45376352523144803, -6.109999999999998543, -3.741295971395162543E-16 ) ) ;
#29574 = PLANE ( 'NONE',  #91031 ) ;
#29575 = ORIENTED_EDGE ( 'NONE', *, *, #109785, .F. ) ;
#29576 = EDGE_CURVE ( 'NONE', #123638, #120212, #141811, .T. ) ;
#29577 = CARTESIAN_POINT ( 'NONE',  ( 24.70612307739177638, 22.22500000000000142, 4.000000000000000000 ) ) ;
#29579 = VERTEX_POINT ( 'NONE', #89836 ) ;
#29578 = DIRECTION ( 'NONE',  ( -1.000000000000000000, -1.224606353822377258E-16, -0.000000000000000000 ) ) ;
#29580 = EDGE_CURVE ( 'NONE', #20842, #137446, #134079, .T. ) ;
#29581 = CARTESIAN_POINT ( 'NONE',  ( -33.29974487139158867, -27.71228299555229313, 4.000000000000000000 ) ) ;
#29583 = AXIS2_PLACEMENT_3D ( 'NONE', #106525, #74670, #20963 ) ;
#29582 = CARTESIAN_POINT ( 'NONE',  ( 18.18398860626898994, 28.73617430169800002, 5.000000000000000000 ) ) ;
#29584 = ORIENTED_EDGE ( 'NONE', *, *, #53389, .T. ) ;
#29585 = CARTESIAN_POINT ( 'NONE',  ( 36.48921356237310221, -27.52281430457080802, 5.000000000000000000 ) ) ;
#29586 = VERTEX_POINT ( 'NONE', #79007 ) ;
#29587 = EDGE_CURVE ( 'NONE', #94208, #83589, #49193, .T. ) ;
#29588 = FILL_AREA_STYLE_COLOUR ( '', #8106 ) ;
#29589 = CARTESIAN_POINT ( 'NONE',  ( 120.5375270504628844, -9.735942053221456900E-16, 7.949999999999998401 ) ) ;
#29590 = CARTESIAN_POINT ( 'NONE',  ( 75.18398860626899705, 28.73617430169839793, 5.000000000000000000 ) ) ;
#29591 = DIRECTION ( 'NONE',  ( -0.3543493200069162685, -0.000000000000000000, -0.9351131265310288487 ) ) ;
#29592 = PLANE ( 'NONE',  #35227 ) ;
#29593 =( NAMED_UNIT ( * ) SI_UNIT ( $, .STERADIAN. ) SOLID_ANGLE_UNIT ( ) );
#29594 = DIRECTION ( 'NONE',  ( 0.6830127018922181881, 0.6830127018922202975, -0.2588190451025214056 ) ) ;
#29595 = CARTESIAN_POINT ( 'NONE',  ( 2.916666666666666963, 5.278424836066147208, 3.047499999999990550 ) ) ;
#29596 = CARTESIAN_POINT ( 'NONE',  ( 5.082903141435219041, 3.967499999999992699, -6.871911579029513994 ) ) ;
#29597 = CARTESIAN_POINT ( 'NONE',  ( -10.49999999999992895, -2.568876922607790103, 4.000000000000000000 ) ) ;
#29598 = CARTESIAN_POINT ( 'NONE',  ( -51.18398860626899705, 28.73617430169823095, 5.000000000000000000 ) ) ;
#29599 = ORIENTED_EDGE ( 'NONE', *, *, #7723, .F. ) ;
#29600 = EDGE_LOOP ( 'NONE', ( #19892, #75067, #117680, #49657 ) ) ;
#29601 = CARTESIAN_POINT ( 'NONE',  ( 85.14583333333334281, 2.130196079827431976, -7.949999999999999289 ) ) ;
#29602 = ORIENTED_EDGE ( 'NONE', *, *, #59534, .F. ) ;
#29603 = PRODUCT_DEFINITION_SHAPE ( 'NONE', 'NONE',  #143574 ) ;
#29604 = EDGE_CURVE ( 'NONE', #17816, #134787, #123927, .T. ) ;
#29605 = DIRECTION ( 'NONE',  ( 0.7071067811865487940, 0.7071067811865463515, 0.000000000000000000 ) ) ;
#29606 = DIRECTION ( 'NONE',  ( 0.7071067811865486830, -0.7071067811865464625, -0.000000000000000000 ) ) ;
#29607 = FACE_OUTER_BOUND ( 'NONE', #44374, .T. ) ;
#29608 = PLANE ( 'NONE',  #68616 ) ;
#29609 = VERTEX_POINT ( 'NONE', #71676 ) ;
#29610 = PLANE ( 'NONE',  #88084 ) ;
#29612 = AXIS2_PLACEMENT_3D ( 'NONE', #30971, #119356, #42571 ) ;
#29611 = CARTESIAN_POINT ( 'NONE',  ( 20.66840764549667497, 2.499999999999998224, 3.061616997868380183E-16 ) ) ;
#29613 = CARTESIAN_POINT ( 'NONE',  ( 7.637717201596474048, 4.584330080086930965E-16, 0.000000000000000000 ) ) ;
#29615 = ORIENTED_EDGE ( 'NONE', *, *, #8612, .F. ) ;
#29614 = PLANE ( 'NONE',  #31316 ) ;
#29616 = PLANE ( 'NONE',  #44334 ) ;
#29617 =( NAMED_UNIT ( * ) PLANE_ANGLE_UNIT ( ) SI_UNIT ( $, .RADIAN. ) );
#29618 = CARTESIAN_POINT ( 'NONE',  ( -39.18398860626899705, 28.73617430169814568, 5.000000000000000000 ) ) ;
#29619 = LINE ( 'NONE', #5717, #57040 ) ;
#29620 = CARTESIAN_POINT ( 'NONE',  ( 22.49999999999985789, 16.08746187583907883, 4.000000000000000000 ) ) ;
#29621 = EDGE_CURVE ( 'NONE', #667, #79851, #4929, .T. ) ;
#29622 = CARTESIAN_POINT ( 'NONE',  ( 60.07317433568704246, -45.23984008851418537, 35.04755940937982217 ) ) ;
#29623 = ORIENTED_EDGE ( 'NONE', *, *, #79236, .F. ) ;
#29624 = ORIENTED_EDGE ( 'NONE', *, *, #48464, .T. ) ;
#29625 = CARTESIAN_POINT ( 'NONE',  ( 105.8754301918981042, -5.291415217122920289, -3.055000000000001492 ) ) ;
#29626 = AXIS2_PLACEMENT_3D ( 'NONE', #42218, #65406, #109586 ) ;
#29627 = ORIENTED_EDGE ( 'NONE', *, *, #112761, .F. ) ;
#29628 = EDGE_CURVE ( 'NONE', #136197, #43029, #49933, .T. ) ;
#29629 = PLANE ( 'NONE',  #29401 ) ;
#29630 = CARTESIAN_POINT ( 'NONE',  ( 8.458333333333333925, -3.047499999999997211, -5.278424836066143655 ) ) ;
#29631 = ORIENTED_EDGE ( 'NONE', *, *, #89192, .F. ) ;
#29632 = CARTESIAN_POINT ( 'NONE',  ( 54.18398860626899705, 28.73617430169825226, 5.000000000000000000 ) ) ;
#29633 = DIRECTION ( 'NONE',  ( 0.6830127018922181881, 0.6830127018922202975, -0.2588190451025214056 ) ) ;
#29634 = CARTESIAN_POINT ( 'NONE',  ( 93.82876352523145158, 0.000000000000000000, -6.109999999999998543 ) ) ;
#29635 = ORIENTED_EDGE ( 'NONE', *, *, #121073, .T. ) ;
#29636 = ADVANCED_FACE ( 'NONE', ( #2828 ), #115843, .F. ) ;
#29637 = LINE ( 'NONE', #28240, #81348 ) ;
#29638 = ORIENTED_EDGE ( 'NONE', *, *, #29580, .F. ) ;
#29639 = FACE_OUTER_BOUND ( 'NONE', #137114, .T. ) ;
#29640 = CARTESIAN_POINT ( 'NONE',  ( 4.499999999999968914, 10.94296225409027379, -9.576120664313247488 ) ) ;
#29641 = VECTOR ( 'NONE', #121379, 1000.000000000000000 ) ;
#29642 = CARTESIAN_POINT ( 'NONE',  ( 19.05000000000000071, 3.174999999999997158, 5.000000000000000000 ) ) ;
#29643 = ORIENTED_EDGE ( 'NONE', *, *, #17224, .T. ) ;
#29644 = EDGE_LOOP ( 'NONE', ( #83248, #47634, #77261, #73022 ) ) ;
#29645 = VECTOR ( 'NONE', #20576, 1000.000000000000000 ) ;
#29646 = ADVANCED_FACE ( 'NONE', ( #91307 ), #15115, .T. ) ;
#29647 = ORIENTED_EDGE ( 'NONE', *, *, #75452, .T. ) ;
#29648 = FACE_OUTER_BOUND ( 'NONE', #8610, .T. ) ;
#29649 = LINE ( 'NONE', #113276, #59294 ) ;
#29650 = CARTESIAN_POINT ( 'NONE',  ( 13.33790314143522160, -6.871911579029513106, -3.967499999999993587 ) ) ;
#29651 = VECTOR ( 'NONE', #37938, 1000.000000000000000 ) ;
#29652 = VECTOR ( 'NONE', #76067, 1000.000000000000000 ) ;
#29653 = CARTESIAN_POINT ( 'NONE',  ( 7.408407645496676963, 9.139736423841732040E-16, 0.000000000000000000 ) ) ;
#29654 = ADVANCED_FACE ( 'NONE', ( #39035 ), #38330, .F. ) ;
#29655 = ORIENTED_EDGE ( 'NONE', *, *, #23138, .T. ) ;
#29656 = ORIENTED_EDGE ( 'NONE', *, *, #41416, .T. ) ;
#29657 = EDGE_CURVE ( 'NONE', #100403, #57736, #49228, .T. ) ;
#29658 = DIRECTION ( 'NONE',  ( -0.7071067811865487940, 0.7071067811865463515, 0.000000000000000000 ) ) ;
#29659 = ORIENTED_EDGE ( 'NONE', *, *, #108528, .F. ) ;
#29660 = ORIENTED_EDGE ( 'NONE', *, *, #100978, .F. ) ;
#29661 = EDGE_CURVE ( 'NONE', #8834, #130638, #136203, .T. ) ;
#29662 = CARTESIAN_POINT ( 'NONE',  ( -24.29974487139158867, -27.71228299555223273, 4.000000000000000000 ) ) ;
#29664 = EDGE_CURVE ( 'NONE', #54301, #86260, #136093, .T. ) ;
#29663 = CARTESIAN_POINT ( 'NONE',  ( 2.671830600776457398, 17.25929247661554911, 4.000000000000000000 ) ) ;
#29665 = ORIENTED_EDGE ( 'NONE', *, *, #111905, .F. ) ;
#29666 = CARTESIAN_POINT ( 'NONE',  ( 5.833333333333333925, 5.278424836066143655, -3.047499999999997655 ) ) ;
#29667 = CARTESIAN_POINT ( 'NONE',  ( -32.24139925780183091, 21.72499999999999432, 5.000000000000000000 ) ) ;
#29668 = CARTESIAN_POINT ( 'NONE',  ( 50.99451991528749062, 28.92564299267973738, 4.000000000000000000 ) ) ;
#29669 = VECTOR ( 'NONE', #68869, 1000.000000000000000 ) ;
#29670 =( BOUNDED_CURVE ( )  B_SPLINE_CURVE ( 3, ( #62515, #106683, #128478, #7376 ),
 .UNSPECIFIED., .F., .T. ) 
 B_SPLINE_CURVE_WITH_KNOTS ( ( 4, 4 ),
 ( 3.141592653589793116, 4.712388980384689674 ),
 .UNSPECIFIED. ) 
 CURVE ( )  GEOMETRIC_REPRESENTATION_ITEM ( )  RATIONAL_B_SPLINE_CURVE ( ( 1.000000000000000000, 0.8047378541243649375, 0.8047378541243649375, 1.000000000000000000 ) ) 
 REPRESENTATION_ITEM ( '' )  );
#29671 = CARTESIAN_POINT ( 'NONE',  ( -34.92500000000001137, 7.512461875839426817, 4.000000000000000000 ) ) ;
#29672 = ORIENTED_EDGE ( 'NONE', *, *, #99791, .T. ) ;
#29673 = VECTOR ( 'NONE', #24245, 1000.000000000000000 ) ;
#29674 = CARTESIAN_POINT ( 'NONE',  ( -59.99451991528749772, 28.92564299267980132, 4.000000000000000000 ) ) ;
#29675 = FACE_BOUND ( 'NONE', #105958, .T. ) ;
#29676 = VERTEX_POINT ( 'NONE', #81135 ) ;
#29677 = LINE ( 'NONE', #84115, #117568 ) ;
#29678 = DIRECTION ( 'NONE',  ( 1.000000000000000000, 0.000000000000000000, 0.000000000000000000 ) ) ;
#29679 = LINE ( 'NONE', #74655, #127872 ) ;
#29680 = ADVANCED_FACE ( 'NONE', ( #125341 ), #47122, .F. ) ;
#29681 = EDGE_LOOP ( 'NONE', ( #63230, #32959, #135557, #123872 ) ) ;
#29682 = DIRECTION ( 'NONE',  ( 0.7071067811865486830, -0.7071067811865464625, -0.000000000000000000 ) ) ;
#29683 = ORIENTED_EDGE ( 'NONE', *, *, #66553, .F. ) ;
#29684 = AXIS2_PLACEMENT_3D ( 'NONE', #68105, #10786, #98535 ) ;
#29685 = VERTEX_POINT ( 'NONE', #83258 ) ;
#29686 = ORIENTED_EDGE ( 'NONE', *, *, #7806, .T. ) ;
#29687 = CARTESIAN_POINT ( 'NONE',  ( 60.18398860626900415, 28.73617430169829490, 5.000000000000000000 ) ) ;
#29688 = DIRECTION ( 'NONE',  ( 0.7071067811865487940, 0.7071067811865463515, -0.000000000000000000 ) ) ;
#29689 = FACE_OUTER_BOUND ( 'NONE', #48567, .T. ) ;
#29690 = CARTESIAN_POINT ( 'NONE',  ( -14.99999999999989519, -7.447814304570749222, 5.000000000000000000 ) ) ;
#29691 = DIRECTION ( 'NONE',  ( 0.000000000000000000, 0.000000000000000000, -1.000000000000000000 ) ) ;
#29692 = CARTESIAN_POINT ( 'NONE',  ( -1.828169399223514624, -14.24070752338414181, 4.000000000000000000 ) ) ;
#29693 = DIRECTION ( 'NONE',  ( -0.7071067811865486830, -0.7071067811865464625, -0.000000000000000000 ) ) ;
#29694 = CONICAL_SURFACE ( 'NONE', #119916, 2.055000000000001048, 0.9599310885968758145 ) ;
#29695 = DIRECTION ( 'NONE',  ( 0.6830127018922180770, -0.6830127018922204085, -0.2588190451025213501 ) ) ;
#29696 = DIRECTION ( 'NONE',  ( -0.000000000000000000, -0.000000000000000000, -1.000000000000000000 ) ) ;
#29697 = CARTESIAN_POINT ( 'NONE',  ( 60.48921356237309510, -27.52281430457097500, 5.000000000000000000 ) ) ;
#29698 = LINE ( 'NONE', #63797, #114179 ) ;
#29699 = EDGE_LOOP ( 'NONE', ( #37946, #79610, #31482, #87488 ) ) ;
#29700 = ORIENTED_EDGE ( 'NONE', *, *, #42088, .F. ) ;
#29701 = ORIENTED_EDGE ( 'NONE', *, *, #101511, .T. ) ;
#29702 = ORIENTED_EDGE ( 'NONE', *, *, #55511, .F. ) ;
#29703 = DIRECTION ( 'NONE',  ( 0.7071067811865487940, -0.7071067811865463515, 0.000000000000000000 ) ) ;
#29704 = ORIENTED_EDGE ( 'NONE', *, *, #124796, .T. ) ;
#29705 = ORIENTED_EDGE ( 'NONE', *, *, #53335, .T. ) ;
#29706 = CARTESIAN_POINT ( 'NONE',  ( 26.90840764549667696, -3.851859888774471706E-31, 2.500000000000001332 ) ) ;
#29707 = LINE ( 'NONE', #118133, #50114 ) ;
#29708 = DIRECTION ( 'NONE',  ( 0.7071067811865486830, -0.7071067811865464625, -0.000000000000000000 ) ) ;
#29709 = LINE ( 'NONE', #128349, #39399 ) ;
#29710 = ORIENTED_EDGE ( 'NONE', *, *, #47432, .F. ) ;
#29711 = DIRECTION ( 'NONE',  ( -0.7071067811865486830, -0.7071067811865464625, 0.000000000000000000 ) ) ;
#29712 = ORIENTED_EDGE ( 'NONE', *, *, #69198, .T. ) ;
#29713 = LINE ( 'NONE', #118140, #79141 ) ;
#29714 = DIRECTION ( 'NONE',  ( 1.000000000000000000, 0.000000000000000000, -0.000000000000000000 ) ) ;
#29715 = ADVANCED_FACE ( 'NONE', ( #25290 ), #47812, .T. ) ;
#29716 = CARTESIAN_POINT ( 'NONE',  ( 14.06706980810188412, 2.126176841940952134, -7.934999999999993392 ) ) ;
#29717 = ORIENTED_EDGE ( 'NONE', *, *, #9965, .F. ) ;
#29718 = CARTESIAN_POINT ( 'NONE',  ( 88.57876352523145158, -7.482591942790327058E-16, 6.109999999999999432 ) ) ;
#29719 = DIRECTION ( 'NONE',  ( -0.000000000000000000, -0.000000000000000000, 1.000000000000000000 ) ) ;
#29720 = EDGE_CURVE ( 'NONE', #6499, #20344, #124618, .T. ) ;
#29721 = DIRECTION ( 'NONE',  ( 0.000000000000000000, 0.000000000000000000, -1.000000000000000000 ) ) ;
#29722 = DIRECTION ( 'NONE',  ( -0.000000000000000000, 0.3543493200069153248, 0.9351131265310292928 ) ) ;
#29723 = ORIENTED_EDGE ( 'NONE', *, *, #2416, .F. ) ;
#29724 = ORIENTED_EDGE ( 'NONE', *, *, #82626, .T. ) ;
#29725 = EDGE_CURVE ( 'NONE', #142121, #110593, #57975, .T. ) ;
#29726 = CARTESIAN_POINT ( 'NONE',  ( 131.5423521607622774, -49.05583548141699168, -39.86617647058817226 ) ) ;
#29727 = ORIENTED_EDGE ( 'NONE', *, *, #122540, .T. ) ;
#29728 = DIRECTION ( 'NONE',  ( -0.7071067811865486830, 0.7071067811865464625, 0.000000000000000000 ) ) ;
#29729 = CARTESIAN_POINT ( 'NONE',  ( 12.03892749862900402, 4.202752102959690472E-16, 0.000000000000000000 ) ) ;
#29730 = DIRECTION ( 'NONE',  ( -0.7071067811865486830, -0.7071067811865464625, -0.000000000000000000 ) ) ;
#29731 = EDGE_CURVE ( 'NONE', #70701, #86413, #13682, .T. ) ;
#29732 = DIRECTION ( 'NONE',  ( 0.3543493200069162685, -0.000000000000000000, -0.9351131265310288487 ) ) ;
#29733 = ORIENTED_EDGE ( 'NONE', *, *, #32369, .F. ) ;
#29734 = FACE_OUTER_BOUND ( 'NONE', #129030, .T. ) ;
#29735 = DIRECTION ( 'NONE',  ( -0.000000000000000000, -0.000000000000000000, 1.000000000000000000 ) ) ;
#29736 = CARTESIAN_POINT ( 'NONE',  ( -6.098435806082331823, 11.25929247661560240, 10.79108189686405872 ) ) ;
#29737 = ORIENTED_EDGE ( 'NONE', *, *, #125407, .T. ) ;
#29738 = CARTESIAN_POINT ( 'NONE',  ( 9.682526172861077640, 2.055000000000001048, 0.000000000000000000 ) ) ;
#29739 = AXIS2_PLACEMENT_3D ( 'NONE', #123859, #24517, #135449 ) ;
#29740 = VECTOR ( 'NONE', #25277, 1000.000000000000000 ) ;
#29741 = VECTOR ( 'NONE', #85651, 1000.000000000000000 ) ;
#29742 = DIRECTION ( 'NONE',  ( 0.7071067811865487940, 0.7071067811865463515, 0.000000000000000000 ) ) ;
#29743 = VERTEX_POINT ( 'NONE', #103555 ) ;
#29744 = VECTOR ( 'NONE', #96508, 999.9999999999998863 ) ;
#29745 = EDGE_CURVE ( 'NONE', #54925, #47459, #48481, .T. ) ;
#29747 = VERTEX_POINT ( 'NONE', #26729 ) ;
#29746 = CARTESIAN_POINT ( 'NONE',  ( 10.32500000000000107, -8.432637487761466488, 4.375000000000001776 ) ) ;
#29748 = ORIENTED_EDGE ( 'NONE', *, *, #39053, .T. ) ;
#29749 = ADVANCED_FACE ( 'NONE', ( #60838 ), #115127, .F. ) ;
#29750 = AXIS2_PLACEMENT_3D ( 'NONE', #105682, #50623, #28877 ) ;
#29751 = LINE ( 'NONE', #64539, #139628 ) ;
#29752 = FACE_OUTER_BOUND ( 'NONE', #35387, .T. ) ;
#29753 = STYLED_ITEM ( 'NONE', ( #57379 ), #124337 ) ;
#29754 = ORIENTED_EDGE ( 'NONE', *, *, #102088, .T. ) ;
#29755 = CARTESIAN_POINT ( 'NONE',  ( -8.510786437626906675, -27.52281430457049183, 5.000000000000000000 ) ) ;
#29756 = ADVANCED_FACE ( 'NONE', ( #117978 ), #52748, .T. ) ;
#29757 = FACE_OUTER_BOUND ( 'NONE', #109019, .T. ) ;
#29758 = FACE_OUTER_BOUND ( 'NONE', #78666, .T. ) ;
#29759 = CARTESIAN_POINT ( 'NONE',  ( 0.1600000000000011691, -7.097592117162074388, -3.612066091894396092 ) ) ;
#29760 = DIRECTION ( 'NONE',  ( 0.7071067811865486830, -0.7071067811865464625, -0.000000000000000000 ) ) ;
#29761 = LINE ( 'NONE', #50829, #63330 ) ;
#29762 = CARTESIAN_POINT ( 'NONE',  ( -60.18398860626900415, 28.73617430169829490, 5.000000000000000000 ) ) ;
#29763 = EDGE_CURVE ( 'NONE', #30212, #126336, #86116, .T. ) ;
#29764 = DIRECTION ( 'NONE',  ( 0.6830127018922180770, -0.6830127018922204085, -0.2588190451025213501 ) ) ;
#29765 = DIRECTION ( 'NONE',  ( -0.7071067811865486830, -0.7071067811865464625, 0.000000000000000000 ) ) ;
#29766 = LINE ( 'NONE', #63866, #83635 ) ;
#29767 = CARTESIAN_POINT ( 'NONE',  ( -69.18398860626899705, 28.73617430169835529, 5.000000000000000000 ) ) ;
#29768 = VERTEX_POINT ( 'NONE', #84686 ) ;
#29769 = VERTEX_POINT ( 'NONE', #51354 ) ;
#29770 = ORIENTED_EDGE ( 'NONE', *, *, #54833, .F. ) ;
#29771 = CARTESIAN_POINT ( 'NONE',  ( 110.9583333333333286, 3.974999999999997424, 6.884901960086288852 ) ) ;
#29772 = VECTOR ( 'NONE', #126427, 1000.000000000000227 ) ;
#29773 = ORIENTED_EDGE ( 'NONE', *, *, #92959, .T. ) ;
#29774 = EDGE_LOOP ( 'NONE', ( #79820, #110728, #46331, #79855, #45116, #43925 ) ) ;
#29775 = ORIENTED_EDGE ( 'NONE', *, *, #102783, .T. ) ;
#29776 = EDGE_CURVE ( 'NONE', #140087, #3810, #128889, .T. ) ;
#29777 = FACE_OUTER_BOUND ( 'NONE', #94969, .T. ) ;
#29778 = VECTOR ( 'NONE', #45000, 1000.000000000000000 ) ;
#29779 = LINE ( 'NONE', #18915, #71710 ) ;
#29780 = ORIENTED_EDGE ( 'NONE', *, *, #124531, .T. ) ;
#29781 = AXIS2_PLACEMENT_3D ( 'NONE', #106638, #118963, #125218 ) ;
#29782 = FACE_OUTER_BOUND ( 'NONE', #27020, .T. ) ;
#29783 = VECTOR ( 'NONE', #123765, 1000.000000000000000 ) ;
#29784 = DIRECTION ( 'NONE',  ( -0.7071067811865486830, -0.7071067811865464625, 0.000000000000000000 ) ) ;
#29785 = VECTOR ( 'NONE', #139935, 1000.000000000000000 ) ;
#29786 = CARTESIAN_POINT ( 'NONE',  ( 34.92499999999998295, 22.22500000000000142, 4.000000000000000000 ) ) ;
#29787 = CARTESIAN_POINT ( 'NONE',  ( 28.00000000000000355, 2.500000000000000000, 0.000000000000000000 ) ) ;
#29788 = CARTESIAN_POINT ( 'NONE',  ( 104.1254301918981184, 5.291415217122919401, 3.055000000000002824 ) ) ;
#29789 = EDGE_LOOP ( 'NONE', ( #11365, #116060, #127389, #135017 ) ) ;
#29790 = CARTESIAN_POINT ( 'NONE',  ( -12.54203964395424009, 7.284662239043824705, -30.67748158611714970 ) ) ;
#29791 = PRESENTATION_STYLE_ASSIGNMENT (( #61749 ) ) ;
#29792 = PLANE ( 'NONE',  #89074 ) ;
#29793 = DIRECTION ( 'NONE',  ( 0.000000000000000000, -1.000000000000000000, 0.000000000000000000 ) ) ;
#29794 = AXIS2_PLACEMENT_3D ( 'NONE', #24611, #47151, #57281 ) ;
#29795 = LINE ( 'NONE', #69231, #54454 ) ;
#29796 = LINE ( 'NONE', #50856, #77046 ) ;
#29797 = DIRECTION ( 'NONE',  ( 0.7071067811865487940, 0.7071067811865463515, 0.000000000000000000 ) ) ;
#29798 = VECTOR ( 'NONE', #12223, 999.9999999999998863 ) ;
#29799 = CARTESIAN_POINT ( 'NONE',  ( 28.00000000000002487, -52.14999999999999147, 34.92500000000003268 ) ) ;
#29800 = EDGE_CURVE ( 'NONE', #127400, #22127, #116595, .T. ) ;
#29801 = DIRECTION ( 'NONE',  ( 6.938893903907221278E-15, -0.000000000000000000, -1.000000000000000000 ) ) ;
#29802 = FACE_OUTER_BOUND ( 'NONE', #110504, .T. ) ;
#29803 = EDGE_LOOP ( 'NONE', ( #97232, #4158, #123686, #47357 ) ) ;
#29804 = EDGE_LOOP ( 'NONE', ( #91972, #74213, #29, #84468 ) ) ;
#29805 = CARTESIAN_POINT ( 'NONE',  ( 126.0004301918981042, -3.055000000000002380, 5.291415217122920289 ) ) ;
#29806 = ORIENTED_EDGE ( 'NONE', *, *, #83858, .T. ) ;
#29807 = DIRECTION ( 'NONE',  ( -0.000000000000000000, 1.000000000000000000, -0.000000000000000000 ) ) ;
#29808 = EDGE_CURVE ( 'NONE', #52143, #47310, #67512, .T. ) ;
#29809 = CARTESIAN_POINT ( 'NONE',  ( 6.160000000000001030, -2.055000000000000160, 0.000000000000000000 ) ) ;
#29810 = CIRCLE ( 'NONE', #15903, 1.142820323027522456 ) ;
#29811 = CARTESIAN_POINT ( 'NONE',  ( -14.81601139373099585, 28.73617430169776910, 5.000000000000000000 ) ) ;
#29812 = FACE_OUTER_BOUND ( 'NONE', #58803, .T. ) ;
#29813 = FACE_OUTER_BOUND ( 'NONE', #125283, .T. ) ;
#29814 = CARTESIAN_POINT ( 'NONE',  ( 126.4954301918981230, 5.291415217122916737, 3.055000000000001936 ) ) ;
#29815 = ORIENTED_EDGE ( 'NONE', *, *, #31125, .F. ) ;
#29816 = EDGE_CURVE ( 'NONE', #93380, #111380, #7074, .T. ) ;
#29817 = LINE ( 'NONE', #61095, #66442 ) ;
#29818 = VERTEX_POINT ( 'NONE', #41903 ) ;
#29819 = PLANE ( 'NONE',  #139903 ) ;
#29820 = DIRECTION ( 'NONE',  ( -0.7071067811865487940, 0.7071067811865463515, -0.000000000000000000 ) ) ;
#29821 = CARTESIAN_POINT ( 'NONE',  ( 4.288407645496676857, 9.139736423841732040E-16, 0.000000000000000000 ) ) ;
#29822 = DIRECTION ( 'NONE',  ( -0.6830127018922180770, -0.6830127018922204085, -0.2588190451025213501 ) ) ;
#29823 = ORIENTED_EDGE ( 'NONE', *, *, #36955, .F. ) ;
#29824 = CARTESIAN_POINT ( 'NONE',  ( 49.58376352523144703, -6.110000000000001208, -3.741295971395164515E-16 ) ) ;
#29825 = ADVANCED_FACE ( 'NONE', ( #119420 ), #96236, .T. ) ;
#29826 = EDGE_LOOP ( 'NONE', ( #89341, #114798, #140031, #3116 ) ) ;
#29827 = CARTESIAN_POINT ( 'NONE',  ( -6.489213562373093325, -27.52281430457059841, 5.000000000000000000 ) ) ;
#29828 = FACE_OUTER_BOUND ( 'NONE', #94057, .T. ) ;
#29829 = FACE_OUTER_BOUND ( 'NONE', #57834, .T. ) ;
#29830 = CARTESIAN_POINT ( 'NONE',  ( 1.042387978378689573, 4.202752102959690472E-16, 0.000000000000000000 ) ) ;
#29831 = CARTESIAN_POINT ( 'NONE',  ( 42.20376352523144448, 6.109999999999998543, 1.122388791418548911E-15 ) ) ;
#29832 = ORIENTED_EDGE ( 'NONE', *, *, #30345, .T. ) ;
#29833 = EDGE_CURVE ( 'NONE', #42879, #24873, #72079, .T. ) ;
#29834 = DIRECTION ( 'NONE',  ( -1.000000000000000000, -1.224606353822377258E-16, -0.000000000000000000 ) ) ;
#29835 = VERTEX_POINT ( 'NONE', #73118 ) ;
#29836 = EDGE_LOOP ( 'NONE', ( #117612, #57748, #93565, #108450 ) ) ;
#29837 = ORIENTED_EDGE ( 'NONE', *, *, #8883, .F. ) ;
#29838 = CARTESIAN_POINT ( 'NONE',  ( -20.99999999999985079, -9.033600742197641864, 5.000000000000000000 ) ) ;
#29839 = EDGE_CURVE ( 'NONE', #94364, #13154, #141947, .T. ) ;
#29840 = ORIENTED_EDGE ( 'NONE', *, *, #58485, .F. ) ;
#29841 = CARTESIAN_POINT ( 'NONE',  ( -36.18398860626899705, 28.73617430169812437, 5.000000000000000000 ) ) ;
#29842 = VECTOR ( 'NONE', #142888, 1000.000000000000000 ) ;
#29843 = CARTESIAN_POINT ( 'NONE',  ( 6.473360963642107890, -5.240707523384232402, 16.25846745537497284 ) ) ;
#29844 = AXIS2_PLACEMENT_3D ( 'NONE', #9718, #120609, #20593 ) ;
#29845 = AXIS2_PLACEMENT_3D ( 'NONE', #49033, #136722, #37436 ) ;
#29846 = PRESENTATION_LAYER_ASSIGNMENT (  '', '', ( #92345 ) ) ;
#29847 = CARTESIAN_POINT ( 'NONE',  ( -0.2997448713915885632, -27.71228299555206220, 4.000000000000000000 ) ) ;
#29848 = TOROIDAL_SURFACE ( 'NONE', #62278, 5.000000000000000000, 1.000000000000000000 ) ;
#29849 = EDGE_CURVE ( 'NONE', #83015, #81768, #63673, .T. ) ;
#29850 = FACE_BOUND ( 'NONE', #59290, .T. ) ;
#29851 = ORIENTED_EDGE ( 'NONE', *, *, #15382, .F. ) ;
#29852 = DIRECTION ( 'NONE',  ( -0.000000000000000000, 1.000000000000000000, -0.000000000000000000 ) ) ;
#29853 = CARTESIAN_POINT ( 'NONE',  ( 25.17183060077629619, -17.24070752338410273, 4.000000000000000000 ) ) ;
#29855 = EDGE_CURVE ( 'NONE', #15784, #39873, #20114, .T. ) ;
#29854 = DIRECTION ( 'NONE',  ( -0.7071067811865487940, 0.7071067811865463515, -0.000000000000000000 ) ) ;
#29856 = EDGE_LOOP ( 'NONE', ( #24170, #22059, #134906, #117188 ) ) ;
#29857 = ORIENTED_EDGE ( 'NONE', *, *, #16307, .F. ) ;
#29858 = VERTEX_POINT ( 'NONE', #28165 ) ;
#29859 = VECTOR ( 'NONE', #51548, 1000.000000000000000 ) ;
#29860 = DIRECTION ( 'NONE',  ( -0.7071067811865486830, -0.7071067811865464625, 0.000000000000000000 ) ) ;
#29861 = VERTEX_POINT ( 'NONE', #72427 ) ;
#29862 = CARTESIAN_POINT ( 'NONE',  ( 59.26626352523145869, 4.472830434245838482, -4.472830434245837594 ) ) ;
#29863 = VERTEX_POINT ( 'NONE', #117281 ) ;
#29864 = CARTESIAN_POINT ( 'NONE',  ( 17.99999999999986855, -19.22509904557634997, 1.855685503482220833 ) ) ;
#29865 = DIRECTION ( 'NONE',  ( 0.6830127018922180770, -0.6830127018922204085, -0.2588190451025213501 ) ) ;
#29866 = ORIENTED_EDGE ( 'NONE', *, *, #37929, .F. ) ;
#29867 = CYLINDRICAL_SURFACE ( 'NONE', #137113, 1.000000000000000888 ) ;
#29868 = AXIS2_PLACEMENT_3D ( 'NONE', #57265, #87723, #57988 ) ;
#29869 = ADVANCED_FACE ( 'NONE', ( #62235 ), #43328, .T. ) ;
#29870 = VECTOR ( 'NONE', #113970, 1000.000000000000227 ) ;
#29871 = DIRECTION ( 'NONE',  ( -0.6830127018922180770, -0.6830127018922204085, -0.2588190451025213501 ) ) ;
#29872 = CARTESIAN_POINT ( 'NONE',  ( 2.700255128608413990, -27.71228299555204089, 4.000000000000000000 ) ) ;
#29873 = CYLINDRICAL_SURFACE ( 'NONE', #117592, 2.500000000000000444 ) ;
#29874 = DIRECTION ( 'NONE',  ( 0.3543493200069162685, -0.000000000000000000, -0.9351131265310288487 ) ) ;
#29875 = PLANE ( 'NONE',  #57840 ) ;
#29876 = ORIENTED_EDGE ( 'NONE', *, *, #44927, .F. ) ;
#29877 = ORIENTED_EDGE ( 'NONE', *, *, #60246, .T. ) ;
#29878 = LINE ( 'NONE', #105997, #70574 ) ;
#29879 = FACE_OUTER_BOUND ( 'NONE', #4712, .T. ) ;
#29880 = VERTEX_POINT ( 'NONE', #99837 ) ;
#29881 = VECTOR ( 'NONE', #12654, 1000.000000000000000 ) ;
#29882 = EDGE_LOOP ( 'NONE', ( #37739, #56506, #120323, #82621 ) ) ;
#29883 = VECTOR ( 'NONE', #47645, 999.9999999999998863 ) ;
#29884 = VERTEX_POINT ( 'NONE', #112162 ) ;
#29885 = DIRECTION ( 'NONE',  ( -1.000000000000000000, -0.000000000000000000, -0.000000000000000000 ) ) ;
#29886 = CARTESIAN_POINT ( 'NONE',  ( 54.18336038379622721, -2.130196079827426203, 7.949999999999996625 ) ) ;
#29887 = LINE ( 'NONE', #74132, #131804 ) ;
#29888 = ORIENTED_EDGE ( 'NONE', *, *, #95606, .T. ) ;
#29889 = AXIS2_PLACEMENT_3D ( 'NONE', #31599, #141050, #30896 ) ;
#29890 = CARTESIAN_POINT ( 'NONE',  ( 7.171830600776424092, 6.759292476615643253, 4.000000000000000000 ) ) ;
#29891 = VECTOR ( 'NONE', #122619, 1000.000000000000000 ) ;
#29893 = ADVANCED_FACE ( 'NONE', ( #44799 ), #75949, .F. ) ;
#29892 =( NAMED_UNIT ( * ) SI_UNIT ( $, .STERADIAN. ) SOLID_ANGLE_UNIT ( ) );
#29894 = CARTESIAN_POINT ( 'NONE',  ( 21.06706980810188412, 2.126176841940952134, -7.934999999999993392 ) ) ;
#29895 = EDGE_CURVE ( 'NONE', #90863, #52679, #65831, .T. ) ;
#29896 = FACE_OUTER_BOUND ( 'NONE', #109259, .T. ) ;
#29897 = EDGE_LOOP ( 'NONE', ( #125378, #27506, #98502, #17422 ) ) ;
#29898 = CARTESIAN_POINT ( 'NONE',  ( 118.1829301918981372, -1.637169565754159173, -6.109999999999999432 ) ) ;
#29899 = EDGE_CURVE ( 'NONE', #109693, #77035, #46642, .T. ) ;
#29900 = DIRECTION ( 'NONE',  ( 0.6830127018922180770, -0.6830127018922204085, -0.2588190451025213501 ) ) ;
#29901 = LINE ( 'NONE', #87154, #100477 ) ;
#29902 =( GEOMETRIC_REPRESENTATION_CONTEXT ( 3 ) GLOBAL_UNCERTAINTY_ASSIGNED_CONTEXT ( ( #69573 ) ) GLOBAL_UNIT_ASSIGNED_CONTEXT ( ( #63765, #142046, #31830 ) ) REPRESENTATION_CONTEXT ( 'NONE', 'WORKASPACE' ) );
#29904 = ORIENTED_EDGE ( 'NONE', *, *, #41684, .F. ) ;
#29903 = LINE ( 'NONE', #21891, #84243 ) ;
#29905 = CARTESIAN_POINT ( 'NONE',  ( 24.48921356237309510, -27.52281430457072631, 5.000000000000000000 ) ) ;
#29906 = VERTEX_POINT ( 'NONE', #78103 ) ;
#29907 = CARTESIAN_POINT ( 'NONE',  ( -57.48921356237308800, -27.52281430457095368, 5.000000000000000000 ) ) ;
#29908 = LINE ( 'NONE', #19756, #77062 ) ;
#29909 = EDGE_CURVE ( 'NONE', #26438, #60276, #98418, .T. ) ;
#29910 = EDGE_CURVE ( 'NONE', #72227, #18068, #86007, .T. ) ;
#29911 = PLANE ( 'NONE',  #10100 ) ;
#29912 = ORIENTED_EDGE ( 'NONE', *, *, #134037, .F. ) ;
#29913 = DIRECTION ( 'NONE',  ( -0.000000000000000000, -0.3543493200069152693, 0.9351131265310292928 ) ) ;
#29914 = DIRECTION ( 'NONE',  ( -0.6830127018922181881, 0.6830127018922202975, -0.2588190451025214056 ) ) ;
#29915 = CARTESIAN_POINT ( 'NONE',  ( -18.70710678118641468, -18.74070752338409562, 5.000000000000000000 ) ) ;
#29916 = ORIENTED_EDGE ( 'NONE', *, *, #14799, .T. ) ;
#29917 = LINE ( 'NONE', #28526, #97091 ) ;
#29918 = DIRECTION ( 'NONE',  ( -0.3543493200069162685, -0.000000000000000000, -0.9351131265310288487 ) ) ;
#29919 = CYLINDRICAL_SURFACE ( 'NONE', #139816, 0.5000000000000004441 ) ;
#29920 = EDGE_CURVE ( 'NONE', #124115, #118128, #76691, .T. ) ;
#29921 = CARTESIAN_POINT ( 'NONE',  ( 16.58990935480158413, 9.759292476615621936, 11.28811694763782469 ) ) ;
#29922 = VERTEX_POINT ( 'NONE', #33884 ) ;
#29923 = EDGE_CURVE ( 'NONE', #130643, #117951, #10657, .T. ) ;
#29924 = ORIENTED_EDGE ( 'NONE', *, *, #12723, .F. ) ;
#29925 = LINE ( 'NONE', #74169, #5544 ) ;
#29926 = DIRECTION ( 'NONE',  ( 0.7071067811865487940, 0.7071067811865463515, 0.000000000000000000 ) ) ;
#29927 = EDGE_CURVE ( 'NONE', #143369, #122228, #54924, .T. ) ;
#29928 = CARTESIAN_POINT ( 'NONE',  ( 12.37456980810188512, 6.871911579029510442, -3.967499999999998916 ) ) ;
#29929 = DIRECTION ( 'NONE',  ( 1.000000000000000000, 0.000000000000000000, 0.000000000000000000 ) ) ;
#29930 = CARTESIAN_POINT ( 'NONE',  ( -3.643187427517367905, -20.24070752338407786, 21.22881796311212099 ) ) ;
#29931 = EDGE_CURVE ( 'NONE', #115930, #81209, #88263, .T. ) ;
#29932 = CARTESIAN_POINT ( 'NONE',  ( -69.48921356237309510, -27.52281430457103895, 5.000000000000000000 ) ) ;
#29933 = ORIENTED_EDGE ( 'NONE', *, *, #39907, .F. ) ;
#29934 = LINE ( 'NONE', #115488, #27933 ) ;
#29935 = CARTESIAN_POINT ( 'NONE',  ( -27.29974487139158512, -27.71228299555225405, 4.000000000000000000 ) ) ;
#29936 = CARTESIAN_POINT ( 'NONE',  ( 6.489213562373093325, -27.52281430457059841, 5.000000000000000000 ) ) ;
#29937 = EDGE_CURVE ( 'NONE', #113570, #89814, #54234, .T. ) ;
#29938 = PLANE ( 'NONE',  #62228 ) ;
#29939 = CARTESIAN_POINT ( 'NONE',  ( 35.49543019189811588, 5.291415217122917625, 3.055000000000002380 ) ) ;
#29940 = CARTESIAN_POINT ( 'NONE',  ( -11.70025512860841133, -27.71228299555198049, 4.000000000000000000 ) ) ;
#29941 = EDGE_LOOP ( 'NONE', ( #128404, #42915, #139373, #5272 ) ) ;
#29942 = CARTESIAN_POINT ( 'NONE',  ( -18.71757738642554258, -21.73023691814492864, 5.000000000000000888 ) ) ;
#29943 = EDGE_LOOP ( 'NONE', ( #63941, #34095, #1419, #135090 ) ) ;
#29944 = ORIENTED_EDGE ( 'NONE', *, *, #94014, .F. ) ;
#29945 = ADVANCED_FACE ( 'NONE', ( #12101 ), #77412, .F. ) ;
#29946 = CARTESIAN_POINT ( 'NONE',  ( 32.99999999999977263, -21.41253812416053393, 4.000000000000000000 ) ) ;
#29947 = CARTESIAN_POINT ( 'NONE',  ( 28.49999999999980815, 10.46639925780215563, 5.000000000000000000 ) ) ;
#29948 = AXIS2_PLACEMENT_3D ( 'NONE', #33328, #55051, #43447 ) ;
#29949 = VECTOR ( 'NONE', #35619, 1000.000000000000000 ) ;
#29950 = VECTOR ( 'NONE', #122731, 999.9999999999998863 ) ;
#29951 = DIRECTION ( 'NONE',  ( -0.7071067811865486830, 0.7071067811865464625, 0.000000000000000000 ) ) ;
#29952 = VECTOR ( 'NONE', #15729, 1000.000000000000227 ) ;
#29953 = CARTESIAN_POINT ( 'NONE',  ( -45.48921356237309510, -27.52281430457087197, 5.000000000000000000 ) ) ;
#29954 = FACE_OUTER_BOUND ( 'NONE', #9019, .T. ) ;
#29955 = DIRECTION ( 'NONE',  ( 0.7071067811865486830, -0.7071067811865464625, -0.000000000000000000 ) ) ;
#29956 = ORIENTED_EDGE ( 'NONE', *, *, #2424, .T. ) ;
#29957 = EDGE_CURVE ( 'NONE', #117951, #107684, #110676, .T. ) ;
#29958 = LINE ( 'NONE', #16206, #55677 ) ;
#29959 = DIRECTION ( 'NONE',  ( -0.000000000000000000, -5.782411586589356455E-15, -1.000000000000000000 ) ) ;
#29960 = ADVANCED_FACE ( 'NONE', ( #56386 ), #65095, .F. ) ;
#29961 = DIRECTION ( 'NONE',  ( -0.000000000000000000, 0.000000000000000000, 1.000000000000000000 ) ) ;
#29962 = VECTOR ( 'NONE', #140498, 1000.000000000000000 ) ;
#29963 = PLANE ( 'NONE',  #55487 ) ;
#29964 = DIRECTION ( 'NONE',  ( 0.7071067811865487940, 0.7071067811865463515, -0.000000000000000000 ) ) ;
#29965 = CARTESIAN_POINT ( 'NONE',  ( -32.99999999999977263, 20.70535890316558536, 1.956823837851992209 ) ) ;
#29966 = CARTESIAN_POINT ( 'NONE',  ( 55.49586038379622721, -3.974999999999998312, -6.884901960086286188 ) ) ;
#29967 = ADVANCED_FACE ( 'NONE', ( #34591 ), #142635, .F. ) ;
#29968 = PLANE ( 'NONE',  #41465 ) ;
#29969 = VECTOR ( 'NONE', #54564, 999.9999999999998863 ) ;
#29970 = ORIENTED_EDGE ( 'NONE', *, *, #82602, .T. ) ;
#29971 = ORIENTED_EDGE ( 'NONE', *, *, #17517, .F. ) ;
#29972 = CARTESIAN_POINT ( 'NONE',  ( 56.41666666666665719, -6.884901960086287076, -3.975000000000000977 ) ) ;
#29973 = CARTESIAN_POINT ( 'NONE',  ( 3.707106781186524369, -12.74070752338415602, 5.000000000000000000 ) ) ;
#29974 = DIRECTION ( 'NONE',  ( 1.000000000000000000, 0.000000000000000000, 0.000000000000000000 ) ) ;
#29975 = PRESENTATION_LAYER_ASSIGNMENT (  '', '', ( #13711 ) ) ;
#29976 = VECTOR ( 'NONE', #121384, 1000.000000000000000 ) ;
#29977 = CARTESIAN_POINT ( 'NONE',  ( 8.292893218813407685, -6.740707523384214639, 5.000000000000000000 ) ) ;
#29978 = ORIENTED_EDGE ( 'NONE', *, *, #95909, .F. ) ;
#29979 = CARTESIAN_POINT ( 'NONE',  ( 127.0544956184052552, -3.708120683632985859, -5.191463943825122662 ) ) ;
#29980 =( BOUNDED_CURVE ( )  B_SPLINE_CURVE ( 3, ( #4546, #84353, #26382, #16925 ),
 .UNSPECIFIED., .F., .T. ) 
 B_SPLINE_CURVE_WITH_KNOTS ( ( 4, 4 ),
 ( 1.739935637444958383, 1.766022064991929819 ),
 .UNSPECIFIED. ) 
 CURVE ( )  GEOMETRIC_REPRESENTATION_ITEM ( )  RATIONAL_B_SPLINE_CURVE ( ( 1.000000000000000000, 0.9999432923287778774, 0.9999432923287778774, 1.000000000000000000 ) ) 
 REPRESENTATION_ITEM ( '' )  );
#29981 =( GEOMETRIC_REPRESENTATION_CONTEXT ( 3 ) GLOBAL_UNCERTAINTY_ASSIGNED_CONTEXT ( ( #109849 ) ) GLOBAL_UNIT_ASSIGNED_CONTEXT ( ( #121620, #140029, #77457 ) ) REPRESENTATION_CONTEXT ( 'NONE', 'WORKASPACE' ) );
#29982 = CARTESIAN_POINT ( 'NONE',  ( 46.66709685856476852, -3.055000000000000160, -5.291415217122921177 ) ) ;
#29983 = ORIENTED_EDGE ( 'NONE', *, *, #110630, .F. ) ;
#29984 = LINE ( 'NONE', #141626, #54854 ) ;
#29985 = ORIENTED_EDGE ( 'NONE', *, *, #32400, .F. ) ;
#29986 = VERTEX_POINT ( 'NONE', #46212 ) ;
#29987 = CARTESIAN_POINT ( 'NONE',  ( -34.49999999999975842, -11.94567065516892690, 4.994342998332167660 ) ) ;
#29988 = VECTOR ( 'NONE', #24140, 1000.000000000000000 ) ;
#29989 = AXIS2_PLACEMENT_3D ( 'NONE', #60489, #51017, #72090 ) ;
#29990 = DIRECTION ( 'NONE',  ( -0.000000000000000000, 1.000000000000000000, 0.000000000000000000 ) ) ;
#29991 = DIRECTION ( 'NONE',  ( -0.6830127018922181881, 0.6830127018922202975, -0.2588190451025214056 ) ) ;
#29992 = CIRCLE ( 'NONE', #122607, 9.000000000000001776 ) ;
#29993 = SURFACE_SIDE_STYLE ('',( #19827 ) ) ;
#29994 = ORIENTED_EDGE ( 'NONE', *, *, #73352, .F. ) ;
#29995 = PLANE ( 'NONE',  #111315 ) ;
#29997 = ORIENTED_EDGE ( 'NONE', *, *, #118909, .T. ) ;
#29996 = FACE_OUTER_BOUND ( 'NONE', #7422, .T. ) ;
#29998 = AXIS2_PLACEMENT_3D ( 'NONE', #119661, #21090, #76943 ) ;
#29999 = LINE ( 'NONE', #108974, #27715 ) ;
#30000 = DIRECTION ( 'NONE',  ( 0.7071067811865487940, 0.7071067811865463515, -0.000000000000000000 ) ) ;
#30001 = FACE_OUTER_BOUND ( 'NONE', #129859, .T. ) ;
#30002 = VECTOR ( 'NONE', #128594, 1000.000000000000000 ) ;
#30003 = DIRECTION ( 'NONE',  ( -0.7071067811865487940, 0.7071067811865463515, -0.000000000000000000 ) ) ;
#30004 = CARTESIAN_POINT ( 'NONE',  ( -45.29974487139158867, -27.71228299555237840, 4.000000000000000000 ) ) ;
#30005 = ORIENTED_EDGE ( 'NONE', *, *, #73537, .T. ) ;
#30006 = EDGE_LOOP ( 'NONE', ( #136910, #81331, #128308, #55274 ) ) ;
#30007 = CARTESIAN_POINT ( 'NONE',  ( 67.57876352523145158, -7.482591942790325086E-16, 6.109999999999998543 ) ) ;
#30008 = DIRECTION ( 'NONE',  ( -0.7071067811865486830, -0.7071067811865464625, 0.000000000000000000 ) ) ;
#30009 = DIRECTION ( 'NONE',  ( -0.6830127018922180770, -0.6830127018922204085, -0.2588190451025213501 ) ) ;
#30010 = PLANE ( 'NONE',  #68707 ) ;
#30011 = ORIENTED_EDGE ( 'NONE', *, *, #51678, .F. ) ;
#30012 = ORIENTED_EDGE ( 'NONE', *, *, #63536, .F. ) ;
#30013 = CARTESIAN_POINT ( 'NONE',  ( -81.48921356237309510, -27.52281430457112066, 5.000000000000000000 ) ) ;
#30014 = LINE ( 'NONE', #120568, #111610 ) ;
#30015 = VERTEX_POINT ( 'NONE', #87539 ) ;
#30016 = EDGE_LOOP ( 'NONE', ( #47138, #47136, #73099, #55870 ) ) ;
#30017 = CARTESIAN_POINT ( 'NONE',  ( 34.49999999999975131, 13.46425560840035196, 4.994342998332160555 ) ) ;
#30018 = ORIENTED_EDGE ( 'NONE', *, *, #49575, .T. ) ;
#30019 = CARTESIAN_POINT ( 'NONE',  ( 64.00000000000000000, 0.000000000000000000, -7.950000000000000178 ) ) ;
#30020 = DIRECTION ( 'NONE',  ( -1.000000000000000000, 0.000000000000000000, -0.000000000000000000 ) ) ;
#30021 = LINE ( 'NONE', #64824, #76591 ) ;
#30022 = EDGE_CURVE ( 'NONE', #138721, #75295, #131047, .T. ) ;
#30023 = FACE_BOUND ( 'NONE', #103043, .T. ) ;
#30024 =( LENGTH_UNIT ( ) NAMED_UNIT ( * ) SI_UNIT ( .MILLI., .METRE. ) );
#30025 = APPLICATION_CONTEXT ( 'automotive_design' ) ;
#30026 = CARTESIAN_POINT ( 'NONE',  ( 40.03752705046288440, -9.735942053221456900E-16, 7.949999999999998401 ) ) ;
#30027 = EDGE_CURVE ( 'NONE', #20459, #100121, #20834, .T. ) ;
#30028 = CARTESIAN_POINT ( 'NONE',  ( -11.99999999999991296, -15.03360074219758502, 5.000000000000000000 ) ) ;
#30030 = ORIENTED_EDGE ( 'NONE', *, *, #79683, .F. ) ;
#30029 = PLANE ( 'NONE',  #133875 ) ;
#30031 = CARTESIAN_POINT ( 'NONE',  ( 26.40000000000000568, -16.48000000000005016, 33.92499999999998295 ) ) ;
#30032 = ITEM_DEFINED_TRANSFORMATION ( 'NONE', 'NONE', #49340,  #127880 ) ;
#30033 = ORIENTED_EDGE ( 'NONE', *, *, #29047, .T. ) ;
#30034 = ORIENTED_EDGE ( 'NONE', *, *, #130710, .T. ) ;
#30035 = CARTESIAN_POINT ( 'NONE',  ( 81.57876352523143737, -7.482591942790325086E-16, 6.109999999999998543 ) ) ;
#30036 = ORIENTED_EDGE ( 'NONE', *, *, #647, .T. ) ;
#30037 = CARTESIAN_POINT ( 'NONE',  ( -22.88982677111772901, -22.22499999999999787, 4.785647885939354751 ) ) ;
#30038 = EDGE_CURVE ( 'NONE', #35605, #114108, #47648, .T. ) ;
#30039 = PLANE ( 'NONE',  #18781 ) ;
#30040 = DIRECTION ( 'NONE',  ( 4.681814790819592407E-17, 0.3543493200069153248, 0.9351131265310292928 ) ) ;
#30041 = EDGE_CURVE ( 'NONE', #138878, #32128, #73473, .T. ) ;
#30042 = CARTESIAN_POINT ( 'NONE',  ( 9.489213562373095101, -27.52281430457062328, 5.000000000000000000 ) ) ;
#30043 = DIRECTION ( 'NONE',  ( -0.6830127018922180770, -0.6830127018922204085, -0.2588190451025213501 ) ) ;
#30044 = PLANE ( 'NONE',  #33905 ) ;
#30045 = CARTESIAN_POINT ( 'NONE',  ( 42.48921356237308800, -27.52281430457085065, 5.000000000000000000 ) ) ;
#30046 = FACE_OUTER_BOUND ( 'NONE', #12072, .T. ) ;
#30047 = CARTESIAN_POINT ( 'NONE',  ( 180.9587832221919257, -48.83231052142030393, -38.98973348322097365 ) ) ;
#30048 = AXIS2_PLACEMENT_3D ( 'NONE', #27695, #18968, #116133 ) ;
#30050 = ADVANCED_FACE ( 'NONE', ( #16941 ), #101982, .F. ) ;
#30049 = VECTOR ( 'NONE', #113886, 1000.000000000000000 ) ;
#30051 = AXIS2_PLACEMENT_3D ( 'NONE', #77394, #103363, #102693 ) ;
#30052 = DIRECTION ( 'NONE',  ( 1.000000000000000000, 0.000000000000000000, 0.000000000000000000 ) ) ;
#30053 = VECTOR ( 'NONE', #119153, 1000.000000000000000 ) ;
#30054 = ORIENTED_EDGE ( 'NONE', *, *, #50418, .F. ) ;
#30055 = DIRECTION ( 'NONE',  ( -0.000000000000000000, -0.3543493200069152693, 0.9351131265310292928 ) ) ;
#30056 = CARTESIAN_POINT ( 'NONE',  ( -30.79333936457826226, 21.75929247661549581, 4.998822639870701856 ) ) ;
#30057 = CIRCLE ( 'NONE', #129607, 2.500000000000000888 ) ;
#30058 = ORIENTED_EDGE ( 'NONE', *, *, #114485, .T. ) ;
#30059 = ORIENTED_EDGE ( 'NONE', *, *, #25553, .F. ) ;
#30060 = VERTEX_POINT ( 'NONE', #61216 ) ;
#30061 = CARTESIAN_POINT ( 'NONE',  ( 36.60459685856475431, 1.637169565754164946, -6.109999999999999432 ) ) ;
#30062 = EDGE_CURVE ( 'NONE', #40404, #106314, #6719, .T. ) ;
#30063 = ORIENTED_EDGE ( 'NONE', *, *, #103061, .T. ) ;
#30064 = AXIS2_PLACEMENT_3D ( 'NONE', #101110, #22804, #35900 ) ;
#30065 = DIRECTION ( 'NONE',  ( -0.7071067811865486830, -0.7071067811865464625, 0.000000000000000000 ) ) ;
#30066 = CARTESIAN_POINT ( 'NONE',  ( 28.48330628287044064, 6.094999999999991758, 1.633150327867687102 ) ) ;
#30067 = CARTESIAN_POINT ( 'NONE',  ( 10.90130741741065101, 8.797424235802401071, -29.72726348083716630 ) ) ;
#30068 = ORIENTED_EDGE ( 'NONE', *, *, #86285, .F. ) ;
#30069 = PLANE ( 'NONE',  #36263 ) ;
#30070 = EDGE_CURVE ( 'NONE', #57200, #79351, #124446, .T. ) ;
#30071 = EDGE_LOOP ( 'NONE', ( #109433, #100101, #126354, #123816 ) ) ;
#30072 = DIRECTION ( 'NONE',  ( 0.7071067811865486830, -0.7071067811865464625, -0.000000000000000000 ) ) ;
#30073 = VECTOR ( 'NONE', #137142, 1000.000000000000000 ) ;
#30074 = FACE_OUTER_BOUND ( 'NONE', #52212, .T. ) ;
#30076 = ORIENTED_EDGE ( 'NONE', *, *, #136145, .F. ) ;
#30075 = LINE ( 'NONE', #137437, #44832 ) ;
#30077 = ORIENTED_EDGE ( 'NONE', *, *, #37347, .F. ) ;
#30078 = LINE ( 'NONE', #40290, #63093 ) ;
#30079 = EDGE_CURVE ( 'NONE', #52416, #122791, #122953, .T. ) ;
#30080 = EDGE_CURVE ( 'NONE', #20632, #71393, #139469, .T. ) ;
#30081 = CARTESIAN_POINT ( 'NONE',  ( -66.18398860626901126, 28.73617430169833753, 5.000000000000000000 ) ) ;
#30082 = ORIENTED_EDGE ( 'NONE', *, *, #127279, .T. ) ;
#30083 = COLOUR_RGB ( '', 0.31764706, 0.68627451, 0.89019608) ;
#30084 = CARTESIAN_POINT ( 'NONE',  ( 23.99451991528749062, 28.92564299267954908, 4.000000000000000000 ) ) ;
#30085 = ORIENTED_EDGE ( 'NONE', *, *, #47495, .F. ) ;
#30086 = ORIENTED_EDGE ( 'NONE', *, *, #37862, .F. ) ;
#30087 = EDGE_LOOP ( 'NONE', ( #28291, #131831, #121480, #57427 ) ) ;
#30088 = PLANE ( 'NONE',  #86542 ) ;
#30090 = EDGE_CURVE ( 'NONE', #94326, #8586, #2648, .T. ) ;
#30089 = VECTOR ( 'NONE', #57300, 1000.000000000000000 ) ;
#30091 = DIRECTION ( 'NONE',  ( -0.000000000000000000, -0.3543493200069152693, 0.9351131265310292928 ) ) ;
#30092 = PLANE ( 'NONE',  #26019 ) ;
#30093 = LINE ( 'NONE', #74343, #125834 ) ;
#30094 = EDGE_CURVE ( 'NONE', #14737, #29556, #7210, .T. ) ;
#30095 = CARTESIAN_POINT ( 'NONE',  ( 152.4000000000000057, 7.919999999999947526, 19.12499999999998224 ) ) ;
#30096 = ORIENTED_EDGE ( 'NONE', *, *, #45474, .F. ) ;
#30097 = VECTOR ( 'NONE', #24017, 1000.000000000000000 ) ;
#30098 = EDGE_CURVE ( 'NONE', #5240, #113523, #143452, .T. ) ;
#30099 = DIRECTION ( 'NONE',  ( -0.7071067811865487940, 0.7071067811865463515, 0.000000000000000000 ) ) ;
#30100 = ORIENTED_EDGE ( 'NONE', *, *, #127846, .T. ) ;
#30101 = VECTOR ( 'NONE', #92203, 1000.000000000000000 ) ;
#30102 = DIRECTION ( 'NONE',  ( 0.3543493200069162685, -0.000000000000000000, -0.9351131265310288487 ) ) ;
#30103 = CARTESIAN_POINT ( 'NONE',  ( 31.04123647476855297, 0.000000000000000000, 7.934999999999990727 ) ) ;
#30104 = ORIENTED_EDGE ( 'NONE', *, *, #6554, .F. ) ;
#30105 = CARTESIAN_POINT ( 'NONE',  ( 22.49999999999984723, 10.46639925780215563, 5.000000000000000000 ) ) ;
#30106 = EDGE_CURVE ( 'NONE', #130990, #70483, #125333, .T. ) ;
#30107 = CARTESIAN_POINT ( 'NONE',  ( -6.183988606268994381, 28.73617430169791476, 5.000000000000000000 ) ) ;
#30108 = ORIENTED_EDGE ( 'NONE', *, *, #39052, .T. ) ;
#30109 = ORIENTED_EDGE ( 'NONE', *, *, #38660, .F. ) ;
#30110 = LINE ( 'NONE', #128035, #53274 ) ;
#30111 = CARTESIAN_POINT ( 'NONE',  ( 34.92499999999998295, -15.15525166281332581, -9.164774702225022551 ) ) ;
#30112 = VECTOR ( 'NONE', #32854, 1000.000000000000227 ) ;
#30113 = FACE_OUTER_BOUND ( 'NONE', #129613, .T. ) ;
#30114 = DIRECTION ( 'NONE',  ( 0.7071067811865486830, -0.7071067811865464625, -0.000000000000000000 ) ) ;
#30115 = EDGE_CURVE ( 'NONE', #142404, #50417, #51003, .T. ) ;
#30116 = CARTESIAN_POINT ( 'NONE',  ( 0.06788206741517728571, -51.13011358081256219, -36.94363806876511802 ) ) ;
#30117 = CARTESIAN_POINT ( 'NONE',  ( 64.37043019189810877, -3.055000000000001936, 5.291415217122918513 ) ) ;
#30118 = LINE ( 'NONE', #118555, #44089 ) ;
#30119 = CARTESIAN_POINT ( 'NONE',  ( 3.183988606268992161, 28.73617430169789699, 5.000000000000000000 ) ) ;
#30120 = DIRECTION ( 'NONE',  ( -0.7071067811865486830, -0.7071067811865464625, 0.000000000000000000 ) ) ;
#30121 = CARTESIAN_POINT ( 'NONE',  ( 184.1500000000000057, -57.15000000000003411, -15.92500000000064730 ) ) ;
#30122 = ORIENTED_EDGE ( 'NONE', *, *, #115981, .F. ) ;
#30123 = CARTESIAN_POINT ( 'NONE',  ( -2.000000000000000000, 2.375000000000000000, 1.069999999999998508 ) ) ;
#30124 = ORIENTED_EDGE ( 'NONE', *, *, #30767, .F. ) ;
#30125 = VECTOR ( 'NONE', #84, 1000.000000000000227 ) ;
#30126 = CARTESIAN_POINT ( 'NONE',  ( 15.96626304157554266, 4.202752102959690472E-16, 0.000000000000000000 ) ) ;
#30127 = CARTESIAN_POINT ( 'NONE',  ( -39.29974487139159578, -27.71228299555233576, 4.000000000000000000 ) ) ;
#30128 = ORIENTED_EDGE ( 'NONE', *, *, #33259, .F. ) ;
#30129 = CARTESIAN_POINT ( 'NONE',  ( 5.999999999999967137, 1.552185695429152856, 5.000000000000000000 ) ) ;
#30131 = ORIENTED_EDGE ( 'NONE', *, *, #46163, .T. ) ;
#30130 = FACE_OUTER_BOUND ( 'NONE', #103171, .T. ) ;
#30132 = CARTESIAN_POINT ( 'NONE',  ( -14.99999999999990230, 14.58746187583910192, 4.000000000000000000 ) ) ;
#30133 = FACE_OUTER_BOUND ( 'NONE', #114522, .T. ) ;
#30134 = DIRECTION ( 'NONE',  ( -0.7071067811865486830, -0.7071067811865464625, -0.000000000000000000 ) ) ;
#30135 = ORIENTED_EDGE ( 'NONE', *, *, #7920, .T. ) ;
#30136 = ORIENTED_EDGE ( 'NONE', *, *, #47998, .T. ) ;
#30137 = CARTESIAN_POINT ( 'NONE',  ( 18.79289321881333663, -8.240707523384195099, 5.000000000000000000 ) ) ;
#30138 = CARTESIAN_POINT ( 'NONE',  ( 7.251592354503322291, -2.500000000000000444, 3.061616997868384620E-16 ) ) ;
#30139 = UNCERTAINTY_MEASURE_WITH_UNIT (LENGTH_MEASURE( 1.000000000000000082E-05 ), #121693, 'distance_accuracy_value', 'NONE');
#30140 = VECTOR ( 'NONE', #513, 999.9999999999998863 ) ;
#30141 = FACE_OUTER_BOUND ( 'NONE', #41374, .T. ) ;
#30142 = EDGE_CURVE ( 'NONE', #49004, #28681, #33267, .T. ) ;
#30143 = CARTESIAN_POINT ( 'NONE',  ( 97.35002705046287019, -5.819803920172572198, -5.819803920172572198 ) ) ;
#30145 = EDGE_CURVE ( 'NONE', #119189, #83353, #61895, .T. ) ;
#30144 = DIRECTION ( 'NONE',  ( -0.3543493200069162685, -0.000000000000000000, -0.9351131265310288487 ) ) ;
#30146 = CARTESIAN_POINT ( 'NONE',  ( 28.21321903303341472, 12.75929247661558996, 10.29404684609041887 ) ) ;
#30147 = ORIENTED_EDGE ( 'NONE', *, *, #127884, .F. ) ;
#30148 = DIRECTION ( 'NONE',  ( -1.000000000000000000, -0.000000000000000000, -0.000000000000000000 ) ) ;
#30149 = DIRECTION ( 'NONE',  ( 1.000000000000000000, 0.000000000000000000, 0.000000000000000000 ) ) ;
#30150 = CARTESIAN_POINT ( 'NONE',  ( 31.64583333333333925, -1.633150327867689988, 6.094999999999989981 ) ) ;
#30151 = ORIENTED_EDGE ( 'NONE', *, *, #52827, .T. ) ;
#30153 = EDGE_CURVE ( 'NONE', #55970, #22881, #58540, .T. ) ;
#30152 = AXIS2_PLACEMENT_3D ( 'NONE', #73117, #50627, #9205 ) ;
#30154 = DIRECTION ( 'NONE',  ( -0.000000000000000000, -0.3543493200069152693, 0.9351131265310292928 ) ) ;
#30155 = VECTOR ( 'NONE', #94030, 1000.000000000000000 ) ;
#30156 = ORIENTED_EDGE ( 'NONE', *, *, #47773, .T. ) ;
#30157 = VECTOR ( 'NONE', #30273, 1000.000000000000000 ) ;
#30158 = CARTESIAN_POINT ( 'NONE',  ( 75.83376352523144703, 6.110000000000001208, 1.122388791418549305E-15 ) ) ;
#30159 = CARTESIAN_POINT ( 'NONE',  ( 5.999999999999961808, -6.412538124160692909, 4.000000000000000000 ) ) ;
#30160 = VECTOR ( 'NONE', #105952, 999.9999999999998863 ) ;
#30161 = CARTESIAN_POINT ( 'NONE',  ( -34.92499999999997584, -6.270000000000012896, -37.00000000000000000 ) ) ;
#30162 = ORIENTED_EDGE ( 'NONE', *, *, #32571, .F. ) ;
#30163 = VECTOR ( 'NONE', #69171, 1000.000000000000000 ) ;
#30164 = AXIS2_PLACEMENT_3D ( 'NONE', #131402, #120, #122645 ) ;
#30165 =( GEOMETRIC_REPRESENTATION_CONTEXT ( 3 ) GLOBAL_UNCERTAINTY_ASSIGNED_CONTEXT ( ( #121592 ) ) GLOBAL_UNIT_ASSIGNED_CONTEXT ( ( #83434, #29040, #4355 ) ) REPRESENTATION_CONTEXT ( 'NONE', 'WORKASPACE' ) );
#30166 = DIRECTION ( 'NONE',  ( -0.7071067811865486830, 0.7071067811865464625, 0.000000000000000000 ) ) ;
#30167 = VECTOR ( 'NONE', #40446, 1000.000000000000000 ) ;
#30168 = CARTESIAN_POINT ( 'NONE',  ( -42.18398860626899705, 28.73617430169816700, 5.000000000000000000 ) ) ;
#30169 = CARTESIAN_POINT ( 'NONE',  ( -17.70025512860841488, -27.71228299555193786, 4.000000000000000000 ) ) ;
#30170 = CARTESIAN_POINT ( 'NONE',  ( 0.000000000000000000, 0.000000000000000000, 5.000000000000000000 ) ) ;
#30172 = VERTEX_POINT ( 'NONE', #17624 ) ;
#30171 = CARTESIAN_POINT ( 'NONE',  ( -32.99999999999976552, -3.412538124160721331, 4.000000000000000000 ) ) ;
#30173 =( NAMED_UNIT ( * ) SI_UNIT ( $, .STERADIAN. ) SOLID_ANGLE_UNIT ( ) );
#30174 = CARTESIAN_POINT ( 'NONE',  ( -39.13499573751598604, 3.759292476615678336, 15.36553568819735283 ) ) ;
#30175 = CARTESIAN_POINT ( 'NONE',  ( 36.27825451568550363, 8.259292476615637923, 11.78515199841158889 ) ) ;
#30176 = VECTOR ( 'NONE', #44277, 1000.000000000000000 ) ;
#30177 = LINE ( 'NONE', #83146, #56225 ) ;
#30178 = VERTEX_POINT ( 'NONE', #90388 ) ;
#30179 = ORIENTED_EDGE ( 'NONE', *, *, #101361, .T. ) ;
#30180 = CARTESIAN_POINT ( 'NONE',  ( 72.04209685856477563, 5.291415217122923842, -3.054999999999996163 ) ) ;
#30181 = ORIENTED_EDGE ( 'NONE', *, *, #79482, .F. ) ;
#30182 = CARTESIAN_POINT ( 'NONE',  ( -0.005480084712502889671, 28.92564299267938210, 4.000000000000000000 ) ) ;
#30183 = LINE ( 'NONE', #20730, #140638 ) ;
#30184 = VECTOR ( 'NONE', #7077, 1000.000000000000000 ) ;
#30185 = CARTESIAN_POINT ( 'NONE',  ( 20.99999999999985079, 8.816494571476654940, 4.604407763760433703 ) ) ;
#30186 = FACE_OUTER_BOUND ( 'NONE', #92557, .T. ) ;
#30187 = EDGE_LOOP ( 'NONE', ( #88104, #124106, #63772, #83031 ) ) ;
#30188 = CARTESIAN_POINT ( 'NONE',  ( -3.793339364578453665, 21.75929247661549581, 4.998822639870701856 ) ) ;
#30189 = PRESENTATION_STYLE_ASSIGNMENT (( #99008 ) ) ;
#30190 = AXIS2_PLACEMENT_3D ( 'NONE', #142720, #43410, #87624 ) ;
#30191 = EDGE_LOOP ( 'NONE', ( #131873, #127723, #104674, #49357 ) ) ;
#30192 = AXIS2_PLACEMENT_3D ( 'NONE', #21139, #57371, #797 ) ;
#30193 = DIRECTION ( 'NONE',  ( 0.7071067811865487940, 0.7071067811865463515, 0.000000000000000000 ) ) ;
#30194 = VECTOR ( 'NONE', #94501, 1000.000000000000000 ) ;
#30195 = CARTESIAN_POINT ( 'NONE',  ( -34.92500000000001137, 22.22500000000000142, 4.000000000000000000 ) ) ;
#30196 = DIRECTION ( 'NONE',  ( 0.3543493200069162685, -0.000000000000000000, -0.9351131265310288487 ) ) ;
#30197 = VECTOR ( 'NONE', #109832, 1000.000000000000000 ) ;
#30198 = EDGE_LOOP ( 'NONE', ( #130326, #60135, #61341, #92830 ) ) ;
#30199 = ORIENTED_EDGE ( 'NONE', *, *, #71808, .F. ) ;
#30200 = EDGE_CURVE ( 'NONE', #109338, #119169, #3357, .T. ) ;
#30201 = EDGE_CURVE ( 'NONE', #103076, #128927, #118374, .T. ) ;
#30202 = EDGE_CURVE ( 'NONE', #50573, #93784, #24419, .T. ) ;
#30203 = FACE_BOUND ( 'NONE', #48664, .T. ) ;
#30204 = COLOUR_RGB ( '', 0.66274510, 0.83137255, 0.94901961) ;
#30205 = CARTESIAN_POINT ( 'NONE',  ( -17.20710678118642178, 12.75929247661558641, 5.000000000000000000 ) ) ;
#30206 = CARTESIAN_POINT ( 'NONE',  ( -29.99999999999979039, 19.93112307739198386, 4.000000000000000000 ) ) ;
#30207 =( LENGTH_UNIT ( ) NAMED_UNIT ( * ) SI_UNIT ( .MILLI., .METRE. ) );
#30208 = LINE ( 'NONE', #6987, #50374 ) ;
#30209 = ADVANCED_FACE ( 'NONE', ( #8168 ), #129984, .F. ) ;
#30210 = EDGE_CURVE ( 'NONE', #6460, #67219, #41524, .T. ) ;
#30211 = DIRECTION ( 'NONE',  ( 0.7071067811865487940, 0.7071067811865463515, 0.000000000000000000 ) ) ;
#30212 = VERTEX_POINT ( 'NONE', #86491 ) ;
#30213 = VECTOR ( 'NONE', #36714, 1000.000000000000000 ) ;
#30214 = ORIENTED_EDGE ( 'NONE', *, *, #101187, .F. ) ;
#30215 = VERTEX_POINT ( 'NONE', #52407 ) ;
#30216 = EDGE_CURVE ( 'NONE', #94223, #123054, #141580, .T. ) ;
#30217 = ORIENTED_EDGE ( 'NONE', *, *, #29156, .T. ) ;
#30218 = CIRCLE ( 'NONE', #53402, 1.000000000000000000 ) ;
#30219 = CARTESIAN_POINT ( 'NONE',  ( 180.9625229943972613, -48.82538788374357352, 38.96958855984509995 ) ) ;
#30220 = LINE ( 'NONE', #75884, #45532 ) ;
#30221 = EDGE_CURVE ( 'NONE', #17057, #28238, #30686, .T. ) ;
#30222 = CARTESIAN_POINT ( 'NONE',  ( 9.489213562373095101, -27.52281430457062328, 5.000000000000000000 ) ) ;
#30223 = ORIENTED_EDGE ( 'NONE', *, *, #7454, .T. ) ;
#30224 = DIRECTION ( 'NONE',  ( 0.000000000000000000, 0.000000000000000000, 1.000000000000000000 ) ) ;
#30225 = DIRECTION ( 'NONE',  ( 0.3543493200069162685, -0.000000000000000000, -0.9351131265310288487 ) ) ;
#30226 = CARTESIAN_POINT ( 'NONE',  ( 58.70419371712954870, -6.884901960086285300, -3.975000000000000089 ) ) ;
#30227 = CARTESIAN_POINT ( 'NONE',  ( -16.82816939922341959, 9.759292476615618384, 4.000000000000000000 ) ) ;
#30228 = VECTOR ( 'NONE', #28325, 1000.000000000000000 ) ;
#30229 = EDGE_CURVE ( 'NONE', #79128, #118195, #132142, .T. ) ;
#30230 = DIRECTION ( 'NONE',  ( -0.000000000000000000, 0.000000000000000000, 1.000000000000000000 ) ) ;
#30231 = ORIENTED_EDGE ( 'NONE', *, *, #7298, .T. ) ;
#30232 = DIRECTION ( 'NONE',  ( 0.7071067811865487940, -0.7071067811865463515, 0.000000000000000000 ) ) ;
#30233 = CARTESIAN_POINT ( 'NONE',  ( 51.16666666666666430, 6.884901960086285300, 3.975000000000003642 ) ) ;
#30234 = ORIENTED_EDGE ( 'NONE', *, *, #4315, .F. ) ;
#30235 = DIRECTION ( 'NONE',  ( -1.000000000000000000, -1.224606353822377258E-16, -0.000000000000000000 ) ) ;
#30236 = VERTEX_POINT ( 'NONE', #130722 ) ;
#30237 = CARTESIAN_POINT ( 'NONE',  ( 21.76000000000000156, 9.521314400968980422E-16, 0.000000000000000000 ) ) ;
#30238 = ORIENTED_EDGE ( 'NONE', *, *, #114508, .T. ) ;
#30239 = CARTESIAN_POINT ( 'NONE',  ( 61.25043019189810423, 3.055000000000002824, -5.291415217122919401 ) ) ;
#30240 = EDGE_CURVE ( 'NONE', #7595, #100121, #40835, .T. ) ;
#30242 = VERTEX_POINT ( 'NONE', #119095 ) ;
#30241 = VECTOR ( 'NONE', #116972, 1000.000000000000000 ) ;
#30243 = VERTEX_POINT ( 'NONE', #129247 ) ;
#30244 = CARTESIAN_POINT ( 'NONE',  ( -75.18398860626899705, 28.73617430169839793, 5.000000000000000000 ) ) ;
#30245 = CARTESIAN_POINT ( 'NONE',  ( 39.48921356237310221, -27.52281430457082934, 5.000000000000000000 ) ) ;
#30247 =( BOUNDED_CURVE ( )  B_SPLINE_CURVE ( 3, ( #18611, #104189, #62888, #107072 ),
 .UNSPECIFIED., .F., .T. ) 
 B_SPLINE_CURVE_WITH_KNOTS ( ( 4, 4 ),
 ( 1.964434688349477875, 3.503810798801451742 ),
 .UNSPECIFIED. ) 
 CURVE ( )  GEOMETRIC_REPRESENTATION_ITEM ( )  RATIONAL_B_SPLINE_CURVE ( ( 1.000000000000000000, 0.8120851936182257313, 0.8120851936182257313, 1.000000000000000000 ) ) 
 REPRESENTATION_ITEM ( '' )  );
#30246 = CARTESIAN_POINT ( 'NONE',  ( 95.22959685856476142, -6.110000000000000320, -1.637169565754161393 ) ) ;
#30248 = FACE_OUTER_BOUND ( 'NONE', #47921, .T. ) ;
#30249 = DIRECTION ( 'NONE',  ( 0.7071067811865487940, 0.7071067811865463515, -0.000000000000000000 ) ) ;
#30250 = EDGE_CURVE ( 'NONE', #7430, #99882, #97310, .T. ) ;
#30251 = DIRECTION ( 'NONE',  ( 0.6830127018922181881, 0.6830127018922202975, -0.2588190451025214056 ) ) ;
#30252 = CONICAL_SURFACE ( 'NONE', #16358, 2.055000000000000604, 0.9599310885968764806 ) ;
#30253 = DIRECTION ( 'NONE',  ( 0.6830127018922180770, -0.6830127018922204085, -0.2588190451025213501 ) ) ;
#30254 = LINE ( 'NONE', #67182, #39817 ) ;
#30257 = EDGE_CURVE ( 'NONE', #65878, #112121, #65469, .T. ) ;
#30256 = FACE_OUTER_BOUND ( 'NONE', #74097, .T. ) ;
#30255 = MECHANICAL_DESIGN_GEOMETRIC_PRESENTATION_REPRESENTATION (  '', ( #97283 ), #60405 ) ;
#30259 = VERTEX_POINT ( 'NONE', #19071 ) ;
#30258 = VECTOR ( 'NONE', #85818, 1000.000000000000000 ) ;
#30260 = ORIENTED_EDGE ( 'NONE', *, *, #30376, .F. ) ;
#30261 = ADVANCED_FACE ( 'NONE', ( #85043 ), #63336, .F. ) ;
#30262 = EDGE_LOOP ( 'NONE', ( #132774, #100673, #80151, #133707 ) ) ;
#30263 = EDGE_LOOP ( 'NONE', ( #24774, #26928, #36095, #648, #93530 ) ) ;
#30264 = VECTOR ( 'NONE', #85721, 1000.000000000000000 ) ;
#30265 = VECTOR ( 'NONE', #104841, 1000.000000000000000 ) ;
#30266 = EDGE_LOOP ( 'NONE', ( #30199, #15116, #123405, #93984 ) ) ;
#30267 = CIRCLE ( 'NONE', #32560, 2.500000000000000444 ) ;
#30268 = VECTOR ( 'NONE', #117276, 1000.000000000000000 ) ;
#30269 = EDGE_CURVE ( 'NONE', #77866, #88432, #108187, .T. ) ;
#30270 = VECTOR ( 'NONE', #1003, 1000.000000000000227 ) ;
#30271 = LINE ( 'NONE', #128861, #37671 ) ;
#30272 = CARTESIAN_POINT ( 'NONE',  ( -6.183988606268994381, 28.73617430169791476, 5.000000000000000000 ) ) ;
#30273 = DIRECTION ( 'NONE',  ( 0.7071067811865486830, -0.7071067811865464625, -0.000000000000000000 ) ) ;
#30274 = ORIENTED_EDGE ( 'NONE', *, *, #20549, .F. ) ;
#30275 = CARTESIAN_POINT ( 'NONE',  ( 3.596992905810010743, -49.14999999999999147, 40.56450646617209799 ) ) ;
#30277 = EDGE_LOOP ( 'NONE', ( #98612, #45760, #3287, #44104, #134024 ) ) ;
#30276 = AXIS2_PLACEMENT_3D ( 'NONE', #20879, #32501, #21618 ) ;
#30278 = CARTESIAN_POINT ( 'NONE',  ( 6.832903141435220817, -3.967499999999994476, 6.871911579029513106 ) ) ;
#30279 =( NAMED_UNIT ( * ) PLANE_ANGLE_UNIT ( ) SI_UNIT ( $, .RADIAN. ) );
#30280 = LINE ( 'NONE', #87524, #8898 ) ;
#30282 = ADVANCED_FACE ( 'NONE', ( #142306 ), #121231, .F. ) ;
#30281 = VECTOR ( 'NONE', #47219, 1000.000000000000000 ) ;
#30283 = CARTESIAN_POINT ( 'NONE',  ( 27.48921356237309155, -27.52281430457074762, 5.000000000000000000 ) ) ;
#30284 = ORIENTED_EDGE ( 'NONE', *, *, #97366, .T. ) ;
#30285 = ORIENTED_EDGE ( 'NONE', *, *, #120026, .T. ) ;
#30286 = VERTEX_POINT ( 'NONE', #32096 ) ;
#30288 = VECTOR ( 'NONE', #43171, 999.9999999999998863 ) ;
#30287 = CARTESIAN_POINT ( 'NONE',  ( -33.18398860626899705, 28.73617430169810305, 5.000000000000000000 ) ) ;
#30289 = DIRECTION ( 'NONE',  ( 0.3543493200069162685, -0.000000000000000000, -0.9351131265310288487 ) ) ;
#30290 = DIRECTION ( 'NONE',  ( -0.7071067811865486830, -0.7071067811865464625, 0.000000000000000000 ) ) ;
#30291 = EDGE_CURVE ( 'NONE', #32044, #37569, #20478, .T. ) ;
#30292 = DIRECTION ( 'NONE',  ( 0.7071067811865487940, 0.7071067811865463515, 0.000000000000000000 ) ) ;
#30293 = DIRECTION ( 'NONE',  ( 1.000000000000000000, 0.000000000000000000, 0.000000000000000000 ) ) ;
#30294 = VECTOR ( 'NONE', #62482, 1000.000000000000227 ) ;
#30295 = VECTOR ( 'NONE', #51058, 1000.000000000000000 ) ;
#30296 = CARTESIAN_POINT ( 'NONE',  ( 21.48921356237309155, -27.52281430457070499, 5.000000000000000000 ) ) ;
#30297 = CARTESIAN_POINT ( 'NONE',  ( 26.83376352523143993, 6.110000000000001208, 1.122388791418549305E-15 ) ) ;
#30298 = CARTESIAN_POINT ( 'NONE',  ( 15.18398860626900237, 28.73617430169797871, 5.000000000000000000 ) ) ;
#30299 = CARTESIAN_POINT ( 'NONE',  ( 26.43999999999999773, 9.521314400968980422E-16, 0.000000000000000000 ) ) ;
#30300 = VECTOR ( 'NONE', #121956, 1000.000000000000000 ) ;
#30301 = ORIENTED_EDGE ( 'NONE', *, *, #79405, .F. ) ;
#30302 = LINE ( 'NONE', #88266, #39527 ) ;
#30304 = AXIS2_PLACEMENT_3D ( 'NONE', #65474, #109655, #121236 ) ;
#30303 = CARTESIAN_POINT ( 'NONE',  ( -1.998069433179001653, -22.22500000000000142, 4.500000000000000888 ) ) ;
#30305 = VERTEX_POINT ( 'NONE', #21923 ) ;
#30306 = FACE_OUTER_BOUND ( 'NONE', #16805, .T. ) ;
#30309 = EDGE_CURVE ( 'NONE', #2772, #89301, #9596, .T. ) ;
#30308 = ORIENTED_EDGE ( 'NONE', *, *, #31646, .T. ) ;
#30307 = CARTESIAN_POINT ( 'NONE',  ( 11.11162361894751882, 9.759292476615614831, 17.35367589129210231 ) ) ;
#30310 = PRESENTATION_LAYER_ASSIGNMENT (  '', '', ( #127479 ) ) ;
#30311 = CARTESIAN_POINT ( 'NONE',  ( -39.29974487139159578, -27.71228299555233576, 4.000000000000000000 ) ) ;
#30312 = ADVANCED_FACE ( 'NONE', ( #42990 ), #87191, .F. ) ;
#30313 = CARTESIAN_POINT ( 'NONE',  ( -32.67183060077623935, 20.25929247661551358, 4.000000000000000000 ) ) ;
#30314 = EDGE_LOOP ( 'NONE', ( #117087, #111486 ) ) ;
#30315 = CARTESIAN_POINT ( 'NONE',  ( 26.67183060077628198, -15.74070752338412049, 4.000000000000000000 ) ) ;
#30316 = EDGE_LOOP ( 'NONE', ( #9835, #44963, #107168, #24596 ) ) ;
#30317 = FACE_OUTER_BOUND ( 'NONE', #55606, .T. ) ;
#30318 = ADVANCED_FACE ( 'NONE', ( #98759 ), #142995, .T. ) ;
#30319 = CARTESIAN_POINT ( 'NONE',  ( 118.4958603837962272, -3.974999999999998312, -6.884901960086286188 ) ) ;
#30320 = CARTESIAN_POINT ( 'NONE',  ( 49.80836038379622721, 7.949999999999996625, 2.130196079827431088 ) ) ;
#30321 = AXIS2_PLACEMENT_3D ( 'NONE', #48397, #28807, #61461 ) ;
#30322 = DIRECTION ( 'NONE',  ( 0.3543493200069162685, -0.000000000000000000, -0.9351131265310288487 ) ) ;
#30323 = CARTESIAN_POINT ( 'NONE',  ( 153.6500000000000057, 4.749999999999997335, 0.000000000000000000 ) ) ;
#30324 = LINE ( 'NONE', #61563, #132860 ) ;
#30325 = CARTESIAN_POINT ( 'NONE',  ( -32.58838509405146056, 22.22499999999999787, 4.777194822843818578 ) ) ;
#30327 = VECTOR ( 'NONE', #91180, 999.9999999999998863 ) ;
#30326 = CARTESIAN_POINT ( 'NONE',  ( 8.750000000000000000, -7.464222240803106570E-16, -6.094999999999989981 ) ) ;
#30328 = CARTESIAN_POINT ( 'NONE',  ( 19.22873647476855297, 5.808823158059031044, -5.808823158059037262 ) ) ;
#30330 = VECTOR ( 'NONE', #92142, 1000.000000000000000 ) ;
#30329 = DIRECTION ( 'NONE',  ( 0.6830127018922181881, 0.6830127018922202975, -0.2588190451025214056 ) ) ;
#30331 = CARTESIAN_POINT ( 'NONE',  ( -9.328169399223460445, 20.25929247661551713, 4.000000000000000000 ) ) ;
#30332 = ORIENTED_EDGE ( 'NONE', *, *, #92720, .F. ) ;
#30333 = EDGE_LOOP ( 'NONE', ( #66601, #40217, #134746, #92970, #58067, #43008, #20687, #23654, #99188, #78265, #37941, #127504, #43278, #38706, #67509, #90815, #103730, #75937, #138150, #24575, #22036, #55368, #12312, #87179, #24723, #60701, #130271, #40, #51909, #17582, #9423, #7730, #119512, #24430, #67627, #80583, #136633, #30516, #83471, #89120, #30054, #143307, #9524, #616, #50263, #122269, #131584, #21605, #38702, #64985, #3773, #130649, #88809, #86840, #45796, #115478, #4312, #9714, #67609, #9806, #115323, #83551, #12484, #124848, #121043, #125042, #100714, #20062, #130702, #124562, #31841, #141452, #14599, #141679, #96768, #52414, #113346, #139167, #126005, #51299, #128412, #84795, #43930, #4518, #17347, #115905 ) ) ;
#30334 = EDGE_CURVE ( 'NONE', #55557, #14445, #51724, .T. ) ;
#30335 = ORIENTED_EDGE ( 'NONE', *, *, #39113, .F. ) ;
#30336 = CARTESIAN_POINT ( 'NONE',  ( -32.99451991528749062, 28.92564299267960948, 4.000000000000000000 ) ) ;
#30337 = LINE ( 'NONE', #31771, #120286 ) ;
#30338 = CYLINDRICAL_SURFACE ( 'NONE', #34869, 17.46000000000000085 ) ;
#30339 = VECTOR ( 'NONE', #82365, 1000.000000000000000 ) ;
#30340 = LINE ( 'NONE', #74580, #22400 ) ;
#30341 = VERTEX_POINT ( 'NONE', #864 ) ;
#30342 = DIRECTION ( 'NONE',  ( 0.7071067811865486830, -0.7071067811865464625, -0.000000000000000000 ) ) ;
#30343 = CARTESIAN_POINT ( 'NONE',  ( 92.43749999999998579, 5.819803920172574863, -5.819803920172573086 ) ) ;
#30344 = LINE ( 'NONE', #118772, #41955 ) ;
#30345 = EDGE_CURVE ( 'NONE', #88659, #46696, #90779, .T. ) ;
#30347 = ORIENTED_EDGE ( 'NONE', *, *, #28374, .T. ) ;
#30346 = CARTESIAN_POINT ( 'NONE',  ( -27.28001967989386856, 0.7592924766157104211, 14.27032725228002619 ) ) ;
#30348 = DIRECTION ( 'NONE',  ( -0.000000000000000000, 0.3543493200069153248, 0.9351131265310292928 ) ) ;
#30349 = FACE_OUTER_BOUND ( 'NONE', #12906, .T. ) ;
#30350 = CONICAL_SURFACE ( 'NONE', #134583, 2.055000000000001048, 0.9599310885968758145 ) ;
#30351 = DIRECTION ( 'NONE',  ( 0.3543493200069163240, 0.000000000000000000, -0.9351131265310288487 ) ) ;
#30352 = LINE ( 'NONE', #118780, #133603 ) ;
#30353 = CARTESIAN_POINT ( 'NONE',  ( -34.82334089840005475, 5.259292476615665457, 15.86257073897106018 ) ) ;
#30354 = VERTEX_POINT ( 'NONE', #135697 ) ;
#30355 = ORIENTED_EDGE ( 'NONE', *, *, #106751, .F. ) ;
#30356 = ORIENTED_EDGE ( 'NONE', *, *, #50898, .T. ) ;
#30357 = CARTESIAN_POINT ( 'NONE',  ( 101.6462635252314186, -4.472830434245840259, 4.472830434245839371 ) ) ;
#30358 = ORIENTED_EDGE ( 'NONE', *, *, #24451, .F. ) ;
#30359 = CARTESIAN_POINT ( 'NONE',  ( 128.6723146206077502, -49.13871568196919526, 40.16438383193056438 ) ) ;
#30360 = CARTESIAN_POINT ( 'NONE',  ( 7.291666666666667851, -3.047499999999994547, 5.278424836066145431 ) ) ;
#30361 = ORIENTED_EDGE ( 'NONE', *, *, #48026, .F. ) ;
#30362 = MECHANICAL_DESIGN_GEOMETRIC_PRESENTATION_REPRESENTATION (  '', ( #127648 ), #44255 ) ;
#30363 = DIRECTION ( 'NONE',  ( -0.000000000000000000, 0.000000000000000000, 1.000000000000000000 ) ) ;
#30364 = LINE ( 'NONE', #118796, #16475 ) ;
#30365 = VECTOR ( 'NONE', #59174, 1000.000000000000000 ) ;
#30366 = VECTOR ( 'NONE', #33971, 1000.000000000000000 ) ;
#30367 = CARTESIAN_POINT ( 'NONE',  ( 94.41209685856478018, 5.291415217122921177, -3.054999999999994831 ) ) ;
#30368 = ORIENTED_EDGE ( 'NONE', *, *, #126407, .F. ) ;
#30369 = DIRECTION ( 'NONE',  ( 0.7071067811865487940, 0.7071067811865463515, 0.000000000000000000 ) ) ;
#30370 = CARTESIAN_POINT ( 'NONE',  ( 23.81601139373100295, 28.73617430169770870, 5.000000000000000000 ) ) ;
#30371 = AXIS2_PLACEMENT_3D ( 'NONE', #63523, #42480, #65680 ) ;
#30372 = DIRECTION ( 'NONE',  ( -0.000000000000000000, -1.000000000000000000, -0.000000000000000000 ) ) ;
#30373 = VECTOR ( 'NONE', #62424, 1000.000000000000000 ) ;
#30374 = AXIS2_PLACEMENT_3D ( 'NONE', #90654, #48560, #134151 ) ;
#30375 = LINE ( 'NONE', #141266, #104025 ) ;
#30376 = EDGE_CURVE ( 'NONE', #129025, #135430, #104623, .T. ) ;
#30377 = VECTOR ( 'NONE', #111766, 1000.000000000000000 ) ;
#30378 = VERTEX_POINT ( 'NONE', #45852 ) ;
#30379 = ORIENTED_EDGE ( 'NONE', *, *, #69185, .T. ) ;
#30380 = ORIENTED_EDGE ( 'NONE', *, *, #125426, .F. ) ;
#30381 = DIRECTION ( 'NONE',  ( 0.7071067811865487940, 0.7071067811865463515, 0.000000000000000000 ) ) ;
#30382 = EDGE_CURVE ( 'NONE', #131612, #135054, #111801, .T. ) ;
#30383 = EDGE_CURVE ( 'NONE', #104648, #98113, #13166, .T. ) ;
#30384 = LINE ( 'NONE', #63748, #61762 ) ;
#30385 = VECTOR ( 'NONE', #6773, 1000.000000000000000 ) ;
#30386 = CARTESIAN_POINT ( 'NONE',  ( 28.49999999999981171, 19.08746187583904330, 4.000000000000000000 ) ) ;
#30387 = CARTESIAN_POINT ( 'NONE',  ( 25.22674160717818737, -11.24070752338416490, 18.24660765846988397 ) ) ;
#30388 = EDGE_CURVE ( 'NONE', #88279, #5941, #68338, .T. ) ;
#30389 = EDGE_CURVE ( 'NONE', #13547, #11670, #134271, .T. ) ;
#30390 = ADVANCED_FACE ( 'NONE', ( #69756 ), #90028, .F. ) ;
#30391 = ORIENTED_EDGE ( 'NONE', *, *, #142652, .T. ) ;
#30392 = ORIENTED_EDGE ( 'NONE', *, *, #139454, .F. ) ;
#30393 = AXIS2_PLACEMENT_3D ( 'NONE', #15560, #4667, #48970 ) ;
#30395 = EDGE_CURVE ( 'NONE', #124122, #110313, #2276, .T. ) ;
#30394 = CARTESIAN_POINT ( 'NONE',  ( -13.20450575203696886, 4.382956123802139281, 4.000000000000000000 ) ) ;
#30396 = EDGE_LOOP ( 'NONE', ( #1100, #102297, #75487, #115073 ) ) ;
#30397 = ORIENTED_EDGE ( 'NONE', *, *, #56587, .F. ) ;
#30398 = EDGE_CURVE ( 'NONE', #65672, #73773, #91484, .T. ) ;
#30399 = VECTOR ( 'NONE', #73554, 1000.000000000000227 ) ;
#30400 = EDGE_CURVE ( 'NONE', #15104, #127807, #78465, .T. ) ;
#30401 = VECTOR ( 'NONE', #81036, 1000.000000000000000 ) ;
#30402 = LINE ( 'NONE', #88916, #104470 ) ;
#30403 = DIRECTION ( 'NONE',  ( -0.7071067811865487940, 0.7071067811865463515, 0.000000000000000000 ) ) ;
#30404 = ORIENTED_EDGE ( 'NONE', *, *, #49724, .F. ) ;
#30405 = DIRECTION ( 'NONE',  ( 0.7071067811865487940, -0.7071067811865463515, 0.000000000000000000 ) ) ;
#30406 = FILL_AREA_STYLE ('',( #10757 ) ) ;
#30407 = VECTOR ( 'NONE', #55047, 1000.000000000000000 ) ;
#30408 = CARTESIAN_POINT ( 'NONE',  ( -32.21837311707484020, 21.74787736706806385, 4.999607392498048419 ) ) ;
#30409 = DIRECTION ( 'NONE',  ( 0.6830127018922181881, 0.6830127018922202975, -0.2588190451025214056 ) ) ;
#30410 = AXIS2_PLACEMENT_3D ( 'NONE', #46978, #124478, #123062 ) ;
#30411 = FACE_OUTER_BOUND ( 'NONE', #123866, .T. ) ;
#30412 = ORIENTED_EDGE ( 'NONE', *, *, #132692, .T. ) ;
#30413 = EDGE_CURVE ( 'NONE', #123966, #84757, #13876, .T. ) ;
#30414 = LINE ( 'NONE', #64463, #67328 ) ;
#30415 = DIRECTION ( 'NONE',  ( -0.7071067811865486830, -0.7071067811865463515, 0.000000000000000000 ) ) ;
#30416 = ORIENTED_EDGE ( 'NONE', *, *, #7527, .F. ) ;
#30417 = CARTESIAN_POINT ( 'NONE',  ( 25.40000000000001634, 3.638354173706144667, -7.063344996420134692 ) ) ;
#30418 = CARTESIAN_POINT ( 'NONE',  ( 34.92499999999998295, -3.183345613589516621, 4.500000000000000888 ) ) ;
#30419 = AXIS2_PLACEMENT_3D ( 'NONE', #62087, #17133, #47838 ) ;
#30420 = CARTESIAN_POINT ( 'NONE',  ( -45.48921356237309510, -27.52281430457087197, 5.000000000000000000 ) ) ;
#30421 = EDGE_LOOP ( 'NONE', ( #46758, #11253, #54806, #94232 ) ) ;
#30422 = LINE ( 'NONE', #28994, #55149 ) ;
#30423 = ORIENTED_EDGE ( 'NONE', *, *, #67938, .F. ) ;
#30424 = VERTEX_POINT ( 'NONE', #22605 ) ;
#30425 = ADVANCED_FACE ( 'NONE', ( #79214 ), #24079, .F. ) ;
#30426 = ORIENTED_EDGE ( 'NONE', *, *, #106156, .F. ) ;
#30427 = FACE_OUTER_BOUND ( 'NONE', #93039, .T. ) ;
#30428 = CARTESIAN_POINT ( 'NONE',  ( -15.79289321881333841, -2.240707523384262601, 5.000000000000000000 ) ) ;
#30429 = PRESENTATION_LAYER_ASSIGNMENT (  '', '', ( #11873 ) ) ;
#30430 = SURFACE_STYLE_USAGE ( .BOTH. , #129722 ) ;
#30431 = CARTESIAN_POINT ( 'NONE',  ( 34.92499999999998295, -0.1833456135895417671, 4.500000000000000888 ) ) ;
#30432 = CARTESIAN_POINT ( 'NONE',  ( 126.1462635252314186, -4.472830434245840259, 4.472830434245838482 ) ) ;
#30433 = CARTESIAN_POINT ( 'NONE',  ( 149.2199999999997999, -3.180000000000061444, -31.92499999999998295 ) ) ;
#30434 = CARTESIAN_POINT ( 'NONE',  ( -30.18398860626900060, 28.73617430169808173, 5.000000000000000000 ) ) ;
#30436 = LINE ( 'NONE', #97824, #52760 ) ;
#30435 = VECTOR ( 'NONE', #31271, 1000.000000000000000 ) ;
#30437 = LINE ( 'NONE', #50759, #97765 ) ;
#30439 = EDGE_CURVE ( 'NONE', #51050, #19388, #135009, .T. ) ;
#30438 = CARTESIAN_POINT ( 'NONE',  ( 26.67183060077627843, -12.74070752338415069, 4.000000000000000000 ) ) ;
#30440 = DIRECTION ( 'NONE',  ( -0.7071067811865486830, 0.7071067811865464625, 0.000000000000000000 ) ) ;
#30441 = CARTESIAN_POINT ( 'NONE',  ( -39.29974487139159578, -27.71228299555233576, 4.000000000000000000 ) ) ;
#30442 = ORIENTED_EDGE ( 'NONE', *, *, #46463, .T. ) ;
#30443 = EDGE_CURVE ( 'NONE', #42434, #48695, #58178, .T. ) ;
#30444 = ORIENTED_EDGE ( 'NONE', *, *, #15363, .T. ) ;
#30445 = ORIENTED_EDGE ( 'NONE', *, *, #116835, .T. ) ;
#30446 = AXIS2_PLACEMENT_3D ( 'NONE', #15278, #92144, #59565 ) ;
#30447 = VERTEX_POINT ( 'NONE', #3020 ) ;
#30448 = PLANE ( 'NONE',  #84268 ) ;
#30449 = ORIENTED_EDGE ( 'NONE', *, *, #114762, .T. ) ;
#30450 = ADVANCED_FACE ( 'NONE', ( #88633 ), #36384, .T. ) ;
#30451 = ORIENTED_EDGE ( 'NONE', *, *, #71120, .F. ) ;
#30452 = FACE_OUTER_BOUND ( 'NONE', #74976, .T. ) ;
#30453 = LINE ( 'NONE', #96376, #29295 ) ;
#30454 = DIRECTION ( 'NONE',  ( -0.000000000000000000, 0.000000000000000000, 1.000000000000000000 ) ) ;
#30455 = ORIENTED_EDGE ( 'NONE', *, *, #49638, .F. ) ;
#30456 = CARTESIAN_POINT ( 'NONE',  ( -42.48921356237308800, -27.52281430457085065, 5.000000000000000000 ) ) ;
#30457 = CONICAL_SURFACE ( 'NONE', #116134, 2.500000000000000444, 0.9599310885968830309 ) ;
#30458 = ORIENTED_EDGE ( 'NONE', *, *, #54658, .F. ) ;
#30459 = EDGE_CURVE ( 'NONE', #50406, #46947, #11737, .T. ) ;
#30460 = DIRECTION ( 'NONE',  ( -0.6830127018922180770, -0.6830127018922204085, -0.2588190451025213501 ) ) ;
#30461 = CARTESIAN_POINT ( 'NONE',  ( 7.796236474768553748, 7.934999999999990727, -1.457635852685135314E-15 ) ) ;
#30462 = ORIENTED_EDGE ( 'NONE', *, *, #141396, .T. ) ;
#30463 = CARTESIAN_POINT ( 'NONE',  ( 87.70376352523146579, 6.109999999999999432, 1.122388791418549108E-15 ) ) ;
#30464 = CARTESIAN_POINT ( 'NONE',  ( 74.50000000000000000, 0.000000000000000000, -7.950000000000000178 ) ) ;
#30466 = EDGE_CURVE ( 'NONE', #136170, #51392, #132, .T. ) ;
#30465 = CARTESIAN_POINT ( 'NONE',  ( -24.18398860626899705, 28.73617430169804265, 5.000000000000000000 ) ) ;
#30467 = LINE ( 'NONE', #77561, #4848 ) ;
#30468 = ORIENTED_EDGE ( 'NONE', *, *, #48772, .F. ) ;
#30469 = ORIENTED_EDGE ( 'NONE', *, *, #49074, .T. ) ;
#30470 = DIRECTION ( 'NONE',  ( 1.000000000000000000, 0.000000000000000000, 0.000000000000000000 ) ) ;
#30471 = ORIENTED_EDGE ( 'NONE', *, *, #70739, .T. ) ;
#30472 = DIRECTION ( 'NONE',  ( 0.000000000000000000, 1.000000000000000000, 0.000000000000000000 ) ) ;
#30473 = CARTESIAN_POINT ( 'NONE',  ( -11.81601139373100651, 28.73617430169779041, 5.000000000000000000 ) ) ;
#30474 = VECTOR ( 'NONE', #74355, 1000.000000000000000 ) ;
#30476 = PLANE ( 'NONE',  #59029 ) ;
#30475 = VECTOR ( 'NONE', #132284, 1000.000000000000227 ) ;
#30477 = DIRECTION ( 'NONE',  ( 0.000000000000000000, 1.000000000000000000, 0.000000000000000000 ) ) ;
#30478 = ORIENTED_EDGE ( 'NONE', *, *, #130568, .F. ) ;
#30479 = AXIS2_PLACEMENT_3D ( 'NONE', #19022, #139413, #40102 ) ;
#30480 = DIRECTION ( 'NONE',  ( -1.000000000000000000, -1.224606353822377258E-16, -0.000000000000000000 ) ) ;
#30481 = VECTOR ( 'NONE', #140930, 1000.000000000000000 ) ;
#30482 = EDGE_CURVE ( 'NONE', #3140, #121198, #16761, .T. ) ;
#30483 = CARTESIAN_POINT ( 'NONE',  ( -1.320799999999990870, 0.000000000000000000, 9.407735506486140764 ) ) ;
#30484 = PLANE ( 'NONE',  #137140 ) ;
#30485 = EDGE_LOOP ( 'NONE', ( #120391, #49834, #90834, #67399 ) ) ;
#30486 = FACE_OUTER_BOUND ( 'NONE', #101849, .T. ) ;
#30487 = VECTOR ( 'NONE', #130177, 1000.000000000000000 ) ;
#30488 = AXIS2_PLACEMENT_3D ( 'NONE', #122312, #133242, #12139 ) ;
#30489 = VECTOR ( 'NONE', #70305, 1000.000000000000000 ) ;
#30490 = AXIS2_PLACEMENT_3D ( 'NONE', #45395, #101874, #56982 ) ;
#30491 = CARTESIAN_POINT ( 'NONE',  ( -34.92500000000001137, -22.22500000000000142, 4.000000000000000000 ) ) ;
#30493 = ORIENTED_EDGE ( 'NONE', *, *, #129266, .T. ) ;
#30492 = AXIS2_PLACEMENT_3D ( 'NONE', #140400, #93330, #40401 ) ;
#30496 = EDGE_CURVE ( 'NONE', #77145, #65454, #17468, .T. ) ;
#30495 = VERTEX_POINT ( 'NONE', #137852 ) ;
#30494 = CARTESIAN_POINT ( 'NONE',  ( 33.48921356237309510, -27.52281430457078670, 5.000000000000000000 ) ) ;
#30497 = ORIENTED_EDGE ( 'NONE', *, *, #64943, .F. ) ;
#30498 = DIRECTION ( 'NONE',  ( 0.6830127018922181881, 0.6830127018922202975, -0.2588190451025214056 ) ) ;
#30499 = CARTESIAN_POINT ( 'NONE',  ( 10.49999999999992895, 6.277155672890280869, -3.510561720658966323 ) ) ;
#30500 = ORIENTED_EDGE ( 'NONE', *, *, #30210, .F. ) ;
#30501 = LINE ( 'NONE', #65289, #18766 ) ;
#30502 = UNCERTAINTY_MEASURE_WITH_UNIT (LENGTH_MEASURE( 1.000000000000000082E-05 ), #103757, 'distance_accuracy_value', 'NONE');
#30503 = CARTESIAN_POINT ( 'NONE',  ( 14.22995720542196985, 21.73644205237998150, 5.000000000000000888 ) ) ;
#30504 = ADVANCED_FACE ( 'NONE', ( #139288 ), #14623, .F. ) ;
#30505 = LINE ( 'NONE', #52928, #34537 ) ;
#30506 = CARTESIAN_POINT ( 'NONE',  ( 57.18398860626899705, 28.73617430169827358, 5.000000000000000000 ) ) ;
#30507 = CARTESIAN_POINT ( 'NONE',  ( 0.1600000000000023348, -7.836308044950259344, 1.291832889770243353 ) ) ;
#30508 = DIRECTION ( 'NONE',  ( -0.6830127018922181881, 0.6830127018922202975, -0.2588190451025214056 ) ) ;
#30509 = LINE ( 'NONE', #94318, #49358 ) ;
#30510 = DIRECTION ( 'NONE',  ( 1.000000000000000000, -0.000000000000000000, 0.000000000000000000 ) ) ;
#30511 = LINE ( 'NONE', #75443, #87435 ) ;
#30512 = CARTESIAN_POINT ( 'NONE',  ( 9.489213562373095101, -27.52281430457062328, 5.000000000000000000 ) ) ;
#30513 = DIRECTION ( 'NONE',  ( 0.7071067811865487940, 0.7071067811865463515, 0.000000000000000000 ) ) ;
#30514 = CARTESIAN_POINT ( 'NONE',  ( 5.691592354503320905, 2.500000000000001776, 0.000000000000000000 ) ) ;
#30515 = PRESENTATION_STYLE_ASSIGNMENT (( #129090 ) ) ;
#30516 = ORIENTED_EDGE ( 'NONE', *, *, #90259, .F. ) ;
#30517 = EDGE_CURVE ( 'NONE', #94326, #7871, #84199, .T. ) ;
#30518 = PRESENTATION_LAYER_ASSIGNMENT (  '', '', ( #53591 ) ) ;
#30519 = ORIENTED_EDGE ( 'NONE', *, *, #94457, .T. ) ;
#30520 = ORIENTED_EDGE ( 'NONE', *, *, #127956, .F. ) ;
#30521 = CARTESIAN_POINT ( 'NONE',  ( 110.0833333333333428, 6.884901960086290629, -3.974999999999994316 ) ) ;
#30522 = VECTOR ( 'NONE', #94557, 1000.000000000000227 ) ;
#30523 = ADVANCED_FACE ( 'NONE', ( #105883 ), #92891, .F. ) ;
#30524 = ORIENTED_EDGE ( 'NONE', *, *, #113442, .T. ) ;
#30525 = ORIENTED_EDGE ( 'NONE', *, *, #25432, .F. ) ;
#30526 = AXIS2_PLACEMENT_3D ( 'NONE', #132821, #46542, #111002 ) ;
#30527 = ORIENTED_EDGE ( 'NONE', *, *, #103245, .F. ) ;
#30528 = CARTESIAN_POINT ( 'NONE',  ( -62.99451991528749772, 28.92564299267982264, 4.000000000000000000 ) ) ;
#30529 = LINE ( 'NONE', #141414, #127244 ) ;
#30530 = AXIS2_PLACEMENT_3D ( 'NONE', #86357, #129123, #130576 ) ;
#30531 = EDGE_LOOP ( 'NONE', ( #28979, #127911, #131746, #31189 ) ) ;
#30532 = LINE ( 'NONE', #21783, #23132 ) ;
#30533 = CARTESIAN_POINT ( 'NONE',  ( -19.64175702458847894, 15.75929247661555088, 19.34181609438704186 ) ) ;
#30534 = CARTESIAN_POINT ( 'NONE',  ( 3.060110710440185233, -9.740707523384184441, 10.89222023123380190 ) ) ;
#30535 = CARTESIAN_POINT ( 'NONE',  ( 99.75043019189810423, 3.055000000000002824, -5.291415217122919401 ) ) ;
#30536 = ORIENTED_EDGE ( 'NONE', *, *, #111769, .T. ) ;
#30537 = EDGE_CURVE ( 'NONE', #138203, #11420, #92164, .T. ) ;
#30538 = CARTESIAN_POINT ( 'NONE',  ( -39.48921356237310221, -27.52281430457082934, 5.000000000000000000 ) ) ;
#30539 = SURFACE_SIDE_STYLE ('',( #75469 ) ) ;
#30541 = VECTOR ( 'NONE', #59006, 1000.000000000000000 ) ;
#30540 = LINE ( 'NONE', #44284, #117016 ) ;
#30542 = DIRECTION ( 'NONE',  ( 0.7071067811865487940, 0.7071067811865463515, 0.000000000000000000 ) ) ;
#30543 = DIRECTION ( 'NONE',  ( -0.7071067811865486830, -0.7071067811865464625, 0.000000000000000000 ) ) ;
#30544 = DIRECTION ( 'NONE',  ( 0.000000000000000000, -1.000000000000000000, 0.000000000000000000 ) ) ;
#30545 = FACE_OUTER_BOUND ( 'NONE', #43147, .T. ) ;
#30546 = VERTEX_POINT ( 'NONE', #82064 ) ;
#30547 = ORIENTED_EDGE ( 'NONE', *, *, #116657, .T. ) ;
#30548 = CARTESIAN_POINT ( 'NONE',  ( 30.16666666666666075, 6.884901960086285300, 3.975000000000003642 ) ) ;
#30549 = ORIENTED_EDGE ( 'NONE', *, *, #142147, .F. ) ;
#30550 = CARTESIAN_POINT ( 'NONE',  ( -34.42499999999997584, 22.27000000000000668, -0.5000000000000000000 ) ) ;
#30551 = CIRCLE ( 'NONE', #141685, 2.500000000000000444 ) ;
#30552 = LINE ( 'NONE', #21805, #38631 ) ;
#30553 = B_SPLINE_CURVE_WITH_KNOTS ( 'NONE', 3,
 ( #45932, #134364, #77150, #35067 ),
 .UNSPECIFIED., .F., .F.,
 ( 4, 4 ),
 ( 0.003615568590623272072, 0.004164643302645765210 ),
 .UNSPECIFIED. ) ;
#30554 = AXIS2_PLACEMENT_3D ( 'NONE', #52244, #8003, #118923 ) ;
#30555 = CARTESIAN_POINT ( 'NONE',  ( 20.81601139373100295, 28.73617430169773002, 5.000000000000000000 ) ) ;
#30556 = CARTESIAN_POINT ( 'NONE',  ( 5.380000000000000782, -2.055000000000000160, 0.000000000000000000 ) ) ;
#30557 = CARTESIAN_POINT ( 'NONE',  ( 25.39999999999999858, -30.18000000000009564, -15.92500000000064375 ) ) ;
#30558 = CARTESIAN_POINT ( 'NONE',  ( 26.99999999999981526, 1.761378380278708855, -6.096875308897192980 ) ) ;
#30559 = CARTESIAN_POINT ( 'NONE',  ( 121.5370968585647802, -3.054999999999998828, -5.291415217122919401 ) ) ;
#30560 = ORIENTED_EDGE ( 'NONE', *, *, #76104, .T. ) ;
#30561 = LINE ( 'NONE', #62474, #138250 ) ;
#30562 = EDGE_CURVE ( 'NONE', #98330, #137557, #93621, .T. ) ;
#30563 = ORIENTED_EDGE ( 'NONE', *, *, #79415, .F. ) ;
#30564 = AXIS2_PLACEMENT_3D ( 'NONE', #129965, #98050, #29208 ) ;
#30565 = CARTESIAN_POINT ( 'NONE',  ( 71.10002705046289861, 5.819803920172570422, 5.819803920172575751 ) ) ;
#30566 = CARTESIAN_POINT ( 'NONE',  ( -57.18398860626899705, 28.73617430169827358, 5.000000000000000000 ) ) ;
#30568 =( BOUNDED_CURVE ( )  B_SPLINE_CURVE ( 3, ( #67075, #142500, #109851, #143196 ),
 .UNSPECIFIED., .F., .T. ) 
 B_SPLINE_CURVE_WITH_KNOTS ( ( 4, 4 ),
 ( 0.1773996044403691741, 1.570796326794896558 ),
 .UNSPECIFIED. ) 
 CURVE ( )  GEOMETRIC_REPRESENTATION_ITEM ( )  RATIONAL_B_SPLINE_CURVE ( ( 1.000000000000000000, 0.8446433258982466441, 0.8446433258982466441, 1.000000000000000000 ) ) 
 REPRESENTATION_ITEM ( '' )  );
#30567 = CARTESIAN_POINT ( 'NONE',  ( -33.52400138585426248, 22.03583458319438648, 4.979811245910084061 ) ) ;
#30569 = DIRECTION ( 'NONE',  ( -0.7071067811865486830, -0.7071067811865464625, 0.000000000000000000 ) ) ;
#30570 = ORIENTED_EDGE ( 'NONE', *, *, #21397, .F. ) ;
#30571 = CARTESIAN_POINT ( 'NONE',  ( 42.00043019189809712, -3.055000000000002380, 5.291415217122920289 ) ) ;
#30572 = EDGE_LOOP ( 'NONE', ( #142808, #27349, #88938, #107415 ) ) ;
#30573 = FACE_OUTER_BOUND ( 'NONE', #62930, .T. ) ;
#30574 = DIRECTION ( 'NONE',  ( -0.3543493200069162685, -0.000000000000000000, -0.9351131265310288487 ) ) ;
#30575 = FACE_OUTER_BOUND ( 'NONE', #53674, .T. ) ;
#30576 = LINE ( 'NONE', #127002, #117877 ) ;
#30577 = PRESENTATION_LAYER_ASSIGNMENT (  '', '', ( #97709 ) ) ;
#30578 = EDGE_CURVE ( 'NONE', #103011, #83238, #5134, .T. ) ;
#30579 = CARTESIAN_POINT ( 'NONE',  ( 41.76626352523145158, 4.472830434245839371, -4.472830434245838482 ) ) ;
#30580 = EDGE_CURVE ( 'NONE', #32788, #13363, #128394, .T. ) ;
#30581 = ORIENTED_EDGE ( 'NONE', *, *, #48898, .F. ) ;
#30583 = EDGE_CURVE ( 'NONE', #39610, #71573, #125543, .T. ) ;
#30582 = CARTESIAN_POINT ( 'NONE',  ( -5.510786437626906675, -27.52281430457051314, 5.000000000000000000 ) ) ;
#30584 = ORIENTED_EDGE ( 'NONE', *, *, #106011, .F. ) ;
#30585 = ORIENTED_EDGE ( 'NONE', *, *, #136983, .F. ) ;
#30586 = CIRCLE ( 'NONE', #16687, 2.500000000000000888 ) ;
#30587 = AXIS2_PLACEMENT_3D ( 'NONE', #22562, #132827, #86451 ) ;
#30588 = ORIENTED_EDGE ( 'NONE', *, *, #96211, .T. ) ;
#30589 = VECTOR ( 'NONE', #46476, 1000.000000000000000 ) ;
#30590 = EDGE_CURVE ( 'NONE', #79833, #121192, #126247, .T. ) ;
#30591 = STYLED_ITEM ( 'NONE', ( #51313 ), #118172 ) ;
#30592 = PRESENTATION_LAYER_ASSIGNMENT (  '', '', ( #93081 ) ) ;
#30593 = CARTESIAN_POINT ( 'NONE',  ( -2.999999999999981792, 4.384688058510565867, -7.090945410444692953 ) ) ;
#30594 = ORIENTED_EDGE ( 'NONE', *, *, #111520, .F. ) ;
#30595 = CARTESIAN_POINT ( 'NONE',  ( -34.47516574401892342, 6.028067341115762368, 4.998110765256835286 ) ) ;
#30596 = EDGE_CURVE ( 'NONE', #104186, #86287, #47994, .T. ) ;
#30597 = CIRCLE ( 'NONE', #56078, 2.500000000000000444 ) ;
#30598 = VECTOR ( 'NONE', #84551, 999.9999999999998863 ) ;
#30599 = AXIS2_PLACEMENT_3D ( 'NONE', #109727, #95986, #119855 ) ;
#30600 = LINE ( 'NONE', #42905, #106100 ) ;
#30601 = LINE ( 'NONE', #8079, #14141 ) ;
#30602 = EDGE_CURVE ( 'NONE', #39158, #91753, #82748, .T. ) ;
#30603 = FACE_BOUND ( 'NONE', #52370, .T. ) ;
#30604 = ORIENTED_EDGE ( 'NONE', *, *, #72724, .F. ) ;
#30605 = EDGE_CURVE ( 'NONE', #49793, #108166, #103067, .T. ) ;
#30606 = PLANE ( 'NONE',  #71166 ) ;
#30607 = CARTESIAN_POINT ( 'NONE',  ( 3.600192512601675610, -49.14999999999999858, 40.57313449935462302 ) ) ;
#30608 = DIRECTION ( 'NONE',  ( -1.000000000000000000, -0.000000000000000000, -0.000000000000000000 ) ) ;
#30609 = VERTEX_POINT ( 'NONE', #136393 ) ;
#30610 = LINE ( 'NONE', #74838, #73562 ) ;
#30611 = EDGE_LOOP ( 'NONE', ( #105141, #39756, #3899, #42420 ) ) ;
#30612 = VERTEX_POINT ( 'NONE', #16011 ) ;
#30613 = DIRECTION ( 'NONE',  ( 0.7071067811865486830, -0.7071067811865464625, -0.000000000000000000 ) ) ;
#30614 = ADVANCED_FACE ( 'NONE', ( #71891 ), #3700, .F. ) ;
#30615 = EDGE_LOOP ( 'NONE', ( #24656, #64141, #116118, #26932, #116258 ) ) ;
#30616 = CARTESIAN_POINT ( 'NONE',  ( 56.78709685856478728, 3.054999999999997495, 5.291415217122919401 ) ) ;
#30617 = ORIENTED_EDGE ( 'NONE', *, *, #20192, .F. ) ;
#30618 = CARTESIAN_POINT ( 'NONE',  ( 0.000000000000000000, 0.000000000000000000, 5.000000000000000000 ) ) ;
#30619 = LINE ( 'NONE', #116179, #7881 ) ;
#30620 = ORIENTED_EDGE ( 'NONE', *, *, #44494, .T. ) ;
#30621 = DIRECTION ( 'NONE',  ( 0.7071067811865487940, 0.7071067811865463515, 0.000000000000000000 ) ) ;
#30622 = PLANE ( 'NONE',  #4082 ) ;
#30623 = VECTOR ( 'NONE', #129530, 1000.000000000000000 ) ;
#30624 = VECTOR ( 'NONE', #16850, 1000.000000000000227 ) ;
#30625 = CARTESIAN_POINT ( 'NONE',  ( 7.720000000000001528, 2.055000000000001492, 0.000000000000000000 ) ) ;
#30626 = CARTESIAN_POINT ( 'NONE',  ( 18.81246187583933960, -22.22500000000000142, 4.000000000000000000 ) ) ;
#30627 = LINE ( 'NONE', #119034, #11108 ) ;
#30628 = VECTOR ( 'NONE', #10109, 1000.000000000000227 ) ;
#30629 = LINE ( 'NONE', #97246, #84004 ) ;
#30630 = LINE ( 'NONE', #19017, #20944 ) ;
#30631 = ORIENTED_EDGE ( 'NONE', *, *, #101805, .F. ) ;
#30632 = EDGE_CURVE ( 'NONE', #140063, #26733, #12868, .T. ) ;
#30633 = ORIENTED_EDGE ( 'NONE', *, *, #7110, .F. ) ;
#30634 = VECTOR ( 'NONE', #17333, 1000.000000000000000 ) ;
#30635 = CARTESIAN_POINT ( 'NONE',  ( 0.000000000000000000, 0.000000000000000000, 5.000000000000000000 ) ) ;
#30636 = LINE ( 'NONE', #61161, #324 ) ;
#30637 = ORIENTED_EDGE ( 'NONE', *, *, #9673, .T. ) ;
#30638 = EDGE_LOOP ( 'NONE', ( #63307, #125669, #48548, #22363 ) ) ;
#30639 = ORIENTED_EDGE ( 'NONE', *, *, #139427, .T. ) ;
#30640 = CARTESIAN_POINT ( 'NONE',  ( -26.48334561358936412, 22.22500000000000142, 4.500000000000000888 ) ) ;
#30641 = FACE_OUTER_BOUND ( 'NONE', #127278, .T. ) ;
#30642 = DIRECTION ( 'NONE',  ( 0.7071067811865486830, -0.7071067811865464625, -0.000000000000000000 ) ) ;
#30643 = ORIENTED_EDGE ( 'NONE', *, *, #108072, .T. ) ;
#30644 = CARTESIAN_POINT ( 'NONE',  ( 0.000000000000000000, 9.913515839097813477E-16, -8.094999999999991758 ) ) ;
#30645 = AXIS2_PLACEMENT_3D ( 'NONE', #77690, #88571, #132807 ) ;
#30646 = CARTESIAN_POINT ( 'NONE',  ( -24.48921356237309510, -27.52281430457072631, 5.000000000000000000 ) ) ;
#30647 = CARTESIAN_POINT ( 'NONE',  ( 17.85873647476854842, 5.808823158059031044, -5.808823158059038150 ) ) ;
#30648 = ORIENTED_EDGE ( 'NONE', *, *, #46026, .F. ) ;
#30649 = CARTESIAN_POINT ( 'NONE',  ( 120.5162635252314374, -4.472830434245839371, 4.472830434245839371 ) ) ;
#30651 = ADVANCED_FACE ( 'NONE', ( #18895 ), #42110, .F. ) ;
#30650 = CARTESIAN_POINT ( 'NONE',  ( 24.87999999999999901, 9.521314400968980422E-16, 0.000000000000000000 ) ) ;
#30652 = AXIS2_PLACEMENT_3D ( 'NONE', #93853, #140229, #16252 ) ;
#30653 = CARTESIAN_POINT ( 'NONE',  ( 0.000000000000000000, 0.000000000000000000, 5.000000000000000000 ) ) ;
#30655 = ORIENTED_EDGE ( 'NONE', *, *, #26284, .T. ) ;
#30654 = DIRECTION ( 'NONE',  ( 0.000000000000000000, 0.000000000000000000, 1.000000000000000000 ) ) ;
#30657 = VECTOR ( 'NONE', #35535, 1000.000000000000000 ) ;
#30656 = DIRECTION ( 'NONE',  ( -0.000000000000000000, 0.000000000000000000, 1.000000000000000000 ) ) ;
#30658 = ORIENTED_EDGE ( 'NONE', *, *, #143300, .T. ) ;
#30659 = LINE ( 'NONE', #53842, #91290 ) ;
#30660 = LINE ( 'NONE', #72774, #35468 ) ;
#30661 = LINE ( 'NONE', #20454, #137514 ) ;
#30662 = VERTEX_POINT ( 'NONE', #84874 ) ;
#30663 = ADVANCED_FACE ( 'NONE', ( #54422 ), #9411, .F. ) ;
#30664 = CARTESIAN_POINT ( 'NONE',  ( 10.15640092694706453, 3.061616997868383634E-16, -2.500000000000000444 ) ) ;
#30665 = DIRECTION ( 'NONE',  ( 0.000000000000000000, 5.782411586589356455E-15, -1.000000000000000000 ) ) ;
#30666 = VECTOR ( 'NONE', #116037, 1000.000000000000000 ) ;
#30667 = EDGE_LOOP ( 'NONE', ( #58525, #43132, #92873, #44340, #125708 ) ) ;
#30668 = VECTOR ( 'NONE', #55353, 1000.000000000000000 ) ;
#30669 = CARTESIAN_POINT ( 'NONE',  ( -2.510786437626908008, -27.52281430457053446, 5.000000000000000000 ) ) ;
#30670 = CARTESIAN_POINT ( 'NONE',  ( -6.299744871391586898, -27.71228299555210484, 4.000000000000000000 ) ) ;
#30671 = ORIENTED_EDGE ( 'NONE', *, *, #127501, .T. ) ;
#30672 = CARTESIAN_POINT ( 'NONE',  ( 34.42499999999998295, 0.000000000000000000, 4.500000000000000888 ) ) ;
#30673 = LINE ( 'NONE', #63321, #4388 ) ;
#30675 = EDGE_CURVE ( 'NONE', #102238, #85157, #7286, .T. ) ;
#30674 = ORIENTED_EDGE ( 'NONE', *, *, #131131, .F. ) ;
#30676 = ORIENTED_EDGE ( 'NONE', *, *, #57465, .F. ) ;
#30677 = VECTOR ( 'NONE', #90808, 999.9999999999998863 ) ;
#30678 = LINE ( 'NONE', #85737, #40268 ) ;
#30679 = LINE ( 'NONE', #65460, #11224 ) ;
#30680 = CARTESIAN_POINT ( 'NONE',  ( 12.95790314143521904, 6.871911579029515771, 3.967499999999989146 ) ) ;
#30681 = DIRECTION ( 'NONE',  ( -0.000000000000000000, -0.000000000000000000, 1.000000000000000000 ) ) ;
#30682 = PLANE ( 'NONE',  #43751 ) ;
#30683 = LINE ( 'NONE', #119090, #100014 ) ;
#30684 = ORIENTED_EDGE ( 'NONE', *, *, #92398, .T. ) ;
#30685 = CARTESIAN_POINT ( 'NONE',  ( -12.69999999999998153, 0.000000000000000000, 2.500000000000000444 ) ) ;
#30686 = LINE ( 'NONE', #32834, #5031 ) ;
#30687 = CARTESIAN_POINT ( 'NONE',  ( 72.18398860626899705, 28.73617430169837661, 5.000000000000000000 ) ) ;
#30688 = AXIS2_PLACEMENT_3D ( 'NONE', #34240, #110334, #78462 ) ;
#30689 = VECTOR ( 'NONE', #60459, 1000.000000000000227 ) ;
#30690 = AXIS2_PLACEMENT_3D ( 'NONE', #113288, #24863, #45928 ) ;
#30691 = DIRECTION ( 'NONE',  ( 0.7071067811865487940, 0.7071067811865463515, -0.000000000000000000 ) ) ;
#30692 = CARTESIAN_POINT ( 'NONE',  ( 41.47459685856477307, 1.637169565754164280, -6.109999999999997655 ) ) ;
#30693 = CARTESIAN_POINT ( 'NONE',  ( 25.49999999999982592, -2.947814304570800736, 5.000000000000000000 ) ) ;
#30694 = AXIS2_PLACEMENT_3D ( 'NONE', #78068, #22915, #1176 ) ;
#30695 = AXIS2_PLACEMENT_3D ( 'NONE', #59500, #49350, #58821 ) ;
#30696 = ORIENTED_EDGE ( 'NONE', *, *, #68411, .F. ) ;
#30697 = CARTESIAN_POINT ( 'NONE',  ( -10.49999999999992006, 18.05218569542898521, 5.000000000000000000 ) ) ;
#30698 = EDGE_CURVE ( 'NONE', #85690, #22619, #41356, .T. ) ;
#30699 = ORIENTED_EDGE ( 'NONE', *, *, #93774, .F. ) ;
#30700 = ADVANCED_FACE ( 'NONE', ( #95747 ), #21029, .F. ) ;
#30701 = VERTEX_POINT ( 'NONE', #20307 ) ;
#30702 = AXIS2_PLACEMENT_3D ( 'NONE', #102399, #82775, #59610 ) ;
#30703 = LINE ( 'NONE', #43000, #66385 ) ;
#30704 =( GEOMETRIC_REPRESENTATION_CONTEXT ( 3 ) GLOBAL_UNCERTAINTY_ASSIGNED_CONTEXT ( ( #140315 ) ) GLOBAL_UNIT_ASSIGNED_CONTEXT ( ( #121660, #109372, #98496 ) ) REPRESENTATION_CONTEXT ( 'NONE', 'WORKASPACE' ) );
#30705 = DIRECTION ( 'NONE',  ( 0.7071067811865487940, -0.7071067811865463515, 0.000000000000000000 ) ) ;
#30706 = VERTEX_POINT ( 'NONE', #142137 ) ;
#30707 = PLANE ( 'NONE',  #29989 ) ;
#30708 = LINE ( 'NONE', #8860, #127548 ) ;
#30709 = CARTESIAN_POINT ( 'NONE',  ( -6.183988606268994381, 28.73617430169791476, 5.000000000000000000 ) ) ;
#30710 = EDGE_CURVE ( 'NONE', #57071, #115637, #108730, .T. ) ;
#30711 = DIRECTION ( 'NONE',  ( -0.7071067811865486830, -0.7071067811865464625, 0.000000000000000000 ) ) ;
#30712 = FACE_OUTER_BOUND ( 'NONE', #35950, .T. ) ;
#30713 = ORIENTED_EDGE ( 'NONE', *, *, #6966, .F. ) ;
#30714 = ADVANCED_FACE ( 'NONE', ( #109483 ), #75439, .F. ) ;
#30715 = CARTESIAN_POINT ( 'NONE',  ( -34.92500000000001137, 7.800094516027127334, 4.759050581649336920 ) ) ;
#30716 = FACE_OUTER_BOUND ( 'NONE', #14335, .T. ) ;
#30717 = DIRECTION ( 'NONE',  ( -0.7071067811865486830, -0.7071067811865464625, 0.000000000000000000 ) ) ;
#30718 = DIRECTION ( 'NONE',  ( -0.7071067811865487940, 0.7071067811865463515, -0.000000000000000000 ) ) ;
#30719 = FACE_OUTER_BOUND ( 'NONE', #47089, .T. ) ;
#30720 = CARTESIAN_POINT ( 'NONE',  ( -11.29289321881337571, 11.25929247661560240, 5.000000000000000000 ) ) ;
#30721 = CARTESIAN_POINT ( 'NONE',  ( 53.74586038379622011, 3.974999999999996980, 6.884901960086287964 ) ) ;
#30723 = DIRECTION ( 'NONE',  ( 0.7071067811865487940, -0.7071067811865463515, 0.000000000000000000 ) ) ;
#30722 = VECTOR ( 'NONE', #86666, 1000.000000000000000 ) ;
#30724 = ORIENTED_EDGE ( 'NONE', *, *, #118909, .F. ) ;
#30725 = EDGE_LOOP ( 'NONE', ( #110577, #291, #91112, #100513 ) ) ;
#30726 = CARTESIAN_POINT ( 'NONE',  ( 56.27083333333332860, -7.949999999999999289, -2.130196079827426203 ) ) ;
#30727 = CARTESIAN_POINT ( 'NONE',  ( 13.64840764549667540, 9.139736423841732040E-16, 0.000000000000000000 ) ) ;
#30728 = LINE ( 'NONE', #42320, #134229 ) ;
#30729 = DIRECTION ( 'NONE',  ( -0.6830127018922180770, -0.6830127018922204085, -0.2588190451025213501 ) ) ;
#30730 = VERTEX_POINT ( 'NONE', #10160 ) ;
#30731 = ADVANCED_FACE ( 'NONE', ( #74741 ), #64550, .T. ) ;
#30732 = DIRECTION ( 'NONE',  ( 1.000000000000000000, 0.000000000000000000, 0.000000000000000000 ) ) ;
#30733 = CARTESIAN_POINT ( 'NONE',  ( 51.18793019189810423, 6.110000000000002984, -1.637169565754156730 ) ) ;
#30734 = VECTOR ( 'NONE', #118701, 1000.000000000000227 ) ;
#30735 = ORIENTED_EDGE ( 'NONE', *, *, #49253, .T. ) ;
#30736 = LINE ( 'NONE', #95245, #110381 ) ;
#30737 = EDGE_LOOP ( 'NONE', ( #124482, #29239, #8505, #80392 ) ) ;
#30738 = ORIENTED_EDGE ( 'NONE', *, *, #16234, .F. ) ;
#30739 = CIRCLE ( 'NONE', #63139, 0.5000000000000004441 ) ;
#30740 = CARTESIAN_POINT ( 'NONE',  ( 8.188407645496676324, 2.500000000000000888, 3.061616997868383141E-16 ) ) ;
#30741 = FACE_OUTER_BOUND ( 'NONE', #128290, .T. ) ;
#30742 = DIRECTION ( 'NONE',  ( -0.7071067811865486830, -0.7071067811865464625, -0.000000000000000000 ) ) ;
#30743 = CARTESIAN_POINT ( 'NONE',  ( 53.99451991528749062, 28.92564299267975869, 4.000000000000000000 ) ) ;
#30744 = ORIENTED_EDGE ( 'NONE', *, *, #55680, .T. ) ;
#30745 = CARTESIAN_POINT ( 'NONE',  ( -23.27718569542924243, -21.72500000000000142, 5.000000000000000000 ) ) ;
#30746 = DIRECTION ( 'NONE',  ( -0.7071067811865486830, 0.7071067811865464625, 0.000000000000000000 ) ) ;
#30748 = ORIENTED_EDGE ( 'NONE', *, *, #143065, .F. ) ;
#30747 = CARTESIAN_POINT ( 'NONE',  ( 9.962472949537104938, -7.464222240803106570E-16, -6.094999999999989981 ) ) ;
#30749 = CARTESIAN_POINT ( 'NONE',  ( 85.16709685856477563, -3.055000000000000160, -5.291415217122921177 ) ) ;
#30750 = DIRECTION ( 'NONE',  ( 0.000000000000000000, 0.000000000000000000, 1.000000000000000000 ) ) ;
#30751 = PLANE ( 'NONE',  #50079 ) ;
#30752 = SURFACE_STYLE_USAGE ( .BOTH. , #100279 ) ;
#30753 = EDGE_CURVE ( 'NONE', #89800, #75311, #40670, .T. ) ;
#30754 = ORIENTED_EDGE ( 'NONE', *, *, #24203, .F. ) ;
#30755 = CARTESIAN_POINT ( 'NONE',  ( 66.70376352523143737, 6.109999999999998543, 1.122388791418548911E-15 ) ) ;
#30756 = EDGE_CURVE ( 'NONE', #8995, #85957, #129083, .T. ) ;
#30757 = DIRECTION ( 'NONE',  ( -0.000000000000000000, 0.000000000000000000, 1.000000000000000000 ) ) ;
#30758 = VECTOR ( 'NONE', #38601, 1000.000000000000000 ) ;
#30759 = DIRECTION ( 'NONE',  ( 0.7071067811865486830, -0.7071067811865464625, -0.000000000000000000 ) ) ;
#30760 = DIRECTION ( 'NONE',  ( -0.7071067811865486830, -0.7071067811865464625, 0.000000000000000000 ) ) ;
#30761 = EDGE_LOOP ( 'NONE', ( #110782, #56873, #1665, #61034 ) ) ;
#30762 = ORIENTED_EDGE ( 'NONE', *, *, #58617, .T. ) ;
#30763 = AXIS2_PLACEMENT_3D ( 'NONE', #75821, #66375, #133764 ) ;
#30764 = DIRECTION ( 'NONE',  ( -0.7071067811865486830, 0.7071067811865464625, 0.000000000000000000 ) ) ;
#30765 = VERTEX_POINT ( 'NONE', #65296 ) ;
#30766 = EDGE_CURVE ( 'NONE', #92260, #57761, #131968, .T. ) ;
#30767 = EDGE_CURVE ( 'NONE', #52339, #15589, #108019, .T. ) ;
#30768 = VERTEX_POINT ( 'NONE', #73304 ) ;
#30769 = PLANE ( 'NONE',  #9691 ) ;
#30770 = ORIENTED_EDGE ( 'NONE', *, *, #96517, .F. ) ;
#30771 = DIRECTION ( 'NONE',  ( -0.7071067811865486830, -0.7071067811865464625, 0.000000000000000000 ) ) ;
#30772 = CARTESIAN_POINT ( 'NONE',  ( 34.92499999999998295, 11.57121408575943633, 9.037117742336738146 ) ) ;
#30773 = VECTOR ( 'NONE', #2734, 1000.000000000000000 ) ;
#30774 = CARTESIAN_POINT ( 'NONE',  ( 12.18398860626900060, 28.73617430169795739, 5.000000000000000000 ) ) ;
#30775 = EDGE_CURVE ( 'NONE', #47321, #51992, #117474, .T. ) ;
#30776 = FACE_BOUND ( 'NONE', #33476, .T. ) ;
#30777 = EDGE_CURVE ( 'NONE', #105009, #94334, #87021, .T. ) ;
#30778 = CARTESIAN_POINT ( 'NONE',  ( 20.97999999999999687, 9.521314400968980422E-16, 0.000000000000000000 ) ) ;
#30779 = DIRECTION ( 'NONE',  ( 0.3543493200069162685, -0.000000000000000000, -0.9351131265310288487 ) ) ;
#30780 = AXIS2_PLACEMENT_3D ( 'NONE', #71741, #6400, #7864 ) ;
#30781 = FACE_OUTER_BOUND ( 'NONE', #28859, .T. ) ;
#30783 = VERTEX_POINT ( 'NONE', #31926 ) ;
#30782 = DIRECTION ( 'NONE',  ( -0.000000000000000000, 0.3543493200069153248, 0.9351131265310292928 ) ) ;
#30784 = EDGE_CURVE ( 'NONE', #106288, #75799, #2849, .T. ) ;
#30785 = ORIENTED_EDGE ( 'NONE', *, *, #69741, .F. ) ;
#30786 = EDGE_LOOP ( 'NONE', ( #54811, #121210, #17896, #67181 ) ) ;
#30787 = CARTESIAN_POINT ( 'NONE',  ( 82.59959685856476597, -6.109999999999997655, -1.637169565754160283 ) ) ;
#30788 = ORIENTED_EDGE ( 'NONE', *, *, #39080, .T. ) ;
#30789 = CARTESIAN_POINT ( 'NONE',  ( -69.48921356237309510, -27.52281430457103895, 5.000000000000000000 ) ) ;
#30790 = ORIENTED_EDGE ( 'NONE', *, *, #96919, .F. ) ;
#30791 = DIRECTION ( 'NONE',  ( -1.000000000000000000, -1.224606353822377258E-16, -0.000000000000000000 ) ) ;
#30792 = EDGE_CURVE ( 'NONE', #41256, #139718, #55841, .T. ) ;
#30793 = VECTOR ( 'NONE', #57421, 1000.000000000000000 ) ;
#30794 = VECTOR ( 'NONE', #32068, 1000.000000000000000 ) ;
#30795 = AXIS2_PLACEMENT_3D ( 'NONE', #93728, #70591, #82170 ) ;
#30796 = DIRECTION ( 'NONE',  ( -0.000000000000000000, 0.3543493200069153248, 0.9351131265310292928 ) ) ;
#30797 = LINE ( 'NONE', #66983, #134082 ) ;
#30798 = CARTESIAN_POINT ( 'NONE',  ( -10.49999999999992184, -13.53360074219759746, 5.000000000000000000 ) ) ;
#30799 = LINE ( 'NONE', #32955, #94413 ) ;
#30800 = CARTESIAN_POINT ( 'NONE',  ( 16.49999999999988987, -10.53360074219763121, 5.000000000000000000 ) ) ;
#30801 = DIRECTION ( 'NONE',  ( -0.7071067811865486830, -0.7071067811865464625, 0.000000000000000000 ) ) ;
#30802 = CARTESIAN_POINT ( 'NONE',  ( 12.29974487139158512, -27.71228299555214747, 4.000000000000000000 ) ) ;
#30803 = ORIENTED_EDGE ( 'NONE', *, *, #38592, .F. ) ;
#30804 = VECTOR ( 'NONE', #82187, 1000.000000000000227 ) ;
#30805 = ADVANCED_FACE ( 'NONE', ( #89859 ), #57999, .F. ) ;
#30806 = AXIS2_PLACEMENT_3D ( 'NONE', #34628, #3395, #122317 ) ;
#30807 = CARTESIAN_POINT ( 'NONE',  ( 26.67183060077628198, -6.740707523384212863, 4.000000000000000000 ) ) ;
#30808 = ORIENTED_EDGE ( 'NONE', *, *, #104179, .T. ) ;
#30809 = CARTESIAN_POINT ( 'NONE',  ( 5.999999999999960032, -4.447814304570786526, 5.000000000000000000 ) ) ;
#30810 = CARTESIAN_POINT ( 'NONE',  ( 45.18398860626900415, 28.73617430169818832, 5.000000000000000000 ) ) ;
#30811 = ORIENTED_EDGE ( 'NONE', *, *, #55753, .T. ) ;
#30812 = ORIENTED_EDGE ( 'NONE', *, *, #92233, .T. ) ;
#30813 = ORIENTED_EDGE ( 'NONE', *, *, #88857, .F. ) ;
#30814 = ADVANCED_FACE ( 'NONE', ( #121766 ), #49183, .T. ) ;
#30815 = CARTESIAN_POINT ( 'NONE',  ( 37.18793019189810423, 6.110000000000002984, -1.637169565754156730 ) ) ;
#30816 = EDGE_CURVE ( 'NONE', #140054, #31371, #110176, .T. ) ;
#30817 = VECTOR ( 'NONE', #65329, 1000.000000000000000 ) ;
#30818 = ORIENTED_EDGE ( 'NONE', *, *, #83119, .T. ) ;
#30819 = CARTESIAN_POINT ( 'NONE',  ( 22.49999999999984368, -19.91253812416055169, 4.000000000000000000 ) ) ;
#30820 = EDGE_CURVE ( 'NONE', #86975, #102218, #99290, .T. ) ;
#30821 = AXIS2_PLACEMENT_3D ( 'NONE', #62431, #108731, #52933 ) ;
#30822 = CARTESIAN_POINT ( 'NONE',  ( 26.58747294953710494, -6.094999999999989981, 3.732111120401553285E-16 ) ) ;
#30823 = CARTESIAN_POINT ( 'NONE',  ( -1.027788732625423807, 12.58765678330771287, -25.27074045886576670 ) ) ;
#30824 = ORIENTED_EDGE ( 'NONE', *, *, #134853, .T. ) ;
#30825 = CARTESIAN_POINT ( 'NONE',  ( -18.70710678118640402, -9.740707523384182664, 5.000000000000000000 ) ) ;
#30826 = ORIENTED_EDGE ( 'NONE', *, *, #35186, .T. ) ;
#30827 = CARTESIAN_POINT ( 'NONE',  ( 2.878526836628512164, -20.24070752338406720, 7.412974875817785581 ) ) ;
#30828 = CARTESIAN_POINT ( 'NONE',  ( -21.48921356237309155, -27.52281430457070499, 5.000000000000000000 ) ) ;
#30830 = VERTEX_POINT ( 'NONE', #34085 ) ;
#30829 = CARTESIAN_POINT ( 'NONE',  ( 34.47516574401891631, 18.02806734111562292, 4.998110765256834398 ) ) ;
#30831 = ORIENTED_EDGE ( 'NONE', *, *, #133584, .F. ) ;
#30832 = DIRECTION ( 'NONE',  ( -1.000000000000000000, -0.000000000000000000, -0.000000000000000000 ) ) ;
#30833 = CONICAL_SURFACE ( 'NONE', #79399, 2.500000000000000888, 0.9599310885968822538 ) ;
#30834 = LINE ( 'NONE', #55428, #130481 ) ;
#30835 = ORIENTED_EDGE ( 'NONE', *, *, #129795, .T. ) ;
#30836 = DIRECTION ( 'NONE',  ( -0.7071067811865486830, -0.7071067811865464625, 0.000000000000000000 ) ) ;
#30837 = ORIENTED_EDGE ( 'NONE', *, *, #59729, .T. ) ;
#30838 = VERTEX_POINT ( 'NONE', #1403 ) ;
#30839 = VECTOR ( 'NONE', #58343, 1000.000000000000000 ) ;
#30840 = VERTEX_POINT ( 'NONE', #77596 ) ;
#30841 = FACE_OUTER_BOUND ( 'NONE', #131458, .T. ) ;
#30842 = LINE ( 'NONE', #67024, #57751 ) ;
#30843 = FACE_OUTER_BOUND ( 'NONE', #103134, .T. ) ;
#30844 = CARTESIAN_POINT ( 'NONE',  ( 19.49999999999986855, 22.01701374228156993, 2.453858888625586321 ) ) ;
#30845 = CARTESIAN_POINT ( 'NONE',  ( -24.32816939922335919, -18.74070752338409207, 4.000000000000000000 ) ) ;
#30846 = CARTESIAN_POINT ( 'NONE',  ( 8.000000000000007105, 0.000000000000000000, 0.000000000000000000 ) ) ;
#30848 = EDGE_CURVE ( 'NONE', #38978, #116079, #24608, .T. ) ;
#30847 = EDGE_LOOP ( 'NONE', ( #87110, #16425, #59019, #35641 ) ) ;
#30849 = CARTESIAN_POINT ( 'NONE',  ( 0.2569208697893814453, 4.202752102959690472E-16, 0.000000000000000000 ) ) ;
#30850 = ORIENTED_EDGE ( 'NONE', *, *, #64758, .T. ) ;
#30851 = LINE ( 'NONE', #75080, #100385 ) ;
#30852 = CONICAL_SURFACE ( 'NONE', #12293, 1.749999999999999778, 0.7853981633974480570 ) ;
#30853 = DIRECTION ( 'NONE',  ( 0.000000000000000000, -1.000000000000000000, 0.000000000000000000 ) ) ;
#30855 = ORIENTED_EDGE ( 'NONE', *, *, #43677, .F. ) ;
#30854 = VECTOR ( 'NONE', #18486, 1000.000000000000227 ) ;
#30856 = DIRECTION ( 'NONE',  ( 0.7071067811865487940, 0.7071067811865463515, -0.000000000000000000 ) ) ;
#30857 = DIRECTION ( 'NONE',  ( -0.000000000000000000, 0.000000000000000000, 1.000000000000000000 ) ) ;
#30858 = EDGE_LOOP ( 'NONE', ( #12749, #26761, #112447, #73702, #41499, #32142 ) ) ;
#30859 = VERTEX_POINT ( 'NONE', #134104 ) ;
#30860 = ADVANCED_FACE ( 'NONE', ( #133396 ), #32652, .F. ) ;
#30861 = DIRECTION ( 'NONE',  ( 0.3543493200069162685, -0.000000000000000000, -0.9351131265310288487 ) ) ;
#30862 = CARTESIAN_POINT ( 'NONE',  ( 8.999999999999937828, -21.41253812416053748, 4.000000000000000000 ) ) ;
#30863 = DIRECTION ( 'NONE',  ( -0.000000000000000000, 0.000000000000000000, 1.000000000000000000 ) ) ;
#30864 = VECTOR ( 'NONE', #27844, 1000.000000000000227 ) ;
#30865 = LINE ( 'NONE', #63507, #89084 ) ;
#30866 = CARTESIAN_POINT ( 'NONE',  ( 66.55793019189812298, 6.110000000000001208, -1.637169565754156286 ) ) ;
#30867 = LINE ( 'NONE', #95380, #11642 ) ;
#30868 = LINE ( 'NONE', #51184, #4695 ) ;
#30869 = DIRECTION ( 'NONE',  ( 0.3543493200069162685, -0.000000000000000000, -0.9351131265310288487 ) ) ;
#30870 = ORIENTED_EDGE ( 'NONE', *, *, #129401, .T. ) ;
#30871 = CARTESIAN_POINT ( 'NONE',  ( 24.70710678118637205, -18.74070752338408852, 5.000000000000000000 ) ) ;
#30872 = ORIENTED_EDGE ( 'NONE', *, *, #65201, .F. ) ;
#30873 = AXIS2_PLACEMENT_3D ( 'NONE', #93213, #72232, #129398 ) ;
#30874 = PLANE ( 'NONE',  #138089 ) ;
#30875 = CARTESIAN_POINT ( 'NONE',  ( -31.92499999999997584, -21.76999999999999247, -37.00000000000000000 ) ) ;
#30876 = ORIENTED_EDGE ( 'NONE', *, *, #29135, .F. ) ;
#30877 = PLANE ( 'NONE',  #41381 ) ;
#30879 = ORIENTED_EDGE ( 'NONE', *, *, #139111, .T. ) ;
#30878 = DIRECTION ( 'NONE',  ( 0.7071067811865486830, -0.7071067811865464625, -0.000000000000000000 ) ) ;
#30880 = LINE ( 'NONE', #70996, #71752 ) ;
#30881 = ADVANCED_FACE ( 'NONE', ( #123949 ), #79767, .F. ) ;
#30882 = DIRECTION ( 'NONE',  ( -0.6830127018922180770, -0.6830127018922204085, -0.2588190451025213501 ) ) ;
#30883 = PLANE ( 'NONE',  #103229 ) ;
#30884 = ORIENTED_EDGE ( 'NONE', *, *, #79615, .F. ) ;
#30885 = EDGE_CURVE ( 'NONE', #16391, #63562, #122480, .T. ) ;
#30887 = ORIENTED_EDGE ( 'NONE', *, *, #50871, .T. ) ;
#30886 = AXIS2_PLACEMENT_3D ( 'NONE', #100445, #68549, #3246 ) ;
#30888 = DIRECTION ( 'NONE',  ( -0.000000000000000000, -0.3543493200069152693, 0.9351131265310292928 ) ) ;
#30889 = LINE ( 'NONE', #53318, #25932 ) ;
#30890 = CARTESIAN_POINT ( 'NONE',  ( 80.57919371712955581, 3.975000000000002753, -6.884901960086283523 ) ) ;
#30891 = CARTESIAN_POINT ( 'NONE',  ( -54.18398860626899705, 28.73617430169825226, 5.000000000000000000 ) ) ;
#30892 = CARTESIAN_POINT ( 'NONE',  ( -5.999999999999956479, -13.06887692260767508, 4.000000000000000000 ) ) ;
#30893 = ORIENTED_EDGE ( 'NONE', *, *, #36598, .F. ) ;
#30894 = ADVANCED_FACE ( 'NONE', ( #111631 ), #123240, .F. ) ;
#30895 = PLANE ( 'NONE',  #37698 ) ;
#30896 = DIRECTION ( 'NONE',  ( 0.7071067811865487940, 0.7071067811865463515, 0.000000000000000000 ) ) ;
#30897 = CARTESIAN_POINT ( 'NONE',  ( 34.85416666666666430, 1.633150327867695095, 6.094999999999988205 ) ) ;
#30898 = VECTOR ( 'NONE', #8670, 999.9999999999998863 ) ;
#30899 = VERTEX_POINT ( 'NONE', #78295 ) ;
#30900 = EDGE_CURVE ( 'NONE', #8157, #24024, #45689, .T. ) ;
#30901 = VECTOR ( 'NONE', #95857, 1000.000000000000227 ) ;
#30902 = CARTESIAN_POINT ( 'NONE',  ( -72.48921356237309510, -27.52281430457106026, 5.000000000000000000 ) ) ;
#30903 = EDGE_LOOP ( 'NONE', ( #116344, #80020, #85796, #74555 ) ) ;
#30904 = CARTESIAN_POINT ( 'NONE',  ( 72.62543019189810423, 5.291415217122919401, 3.055000000000002824 ) ) ;
#30905 = LINE ( 'NONE', #107006, #84778 ) ;
#30907 = CARTESIAN_POINT ( 'NONE',  ( 45.48921356237309510, -27.52281430457087197, 5.000000000000000000 ) ) ;
#30906 = VECTOR ( 'NONE', #45212, 1000.000000000000227 ) ;
#30908 = ORIENTED_EDGE ( 'NONE', *, *, #57740, .F. ) ;
#30909 = EDGE_CURVE ( 'NONE', #130020, #91987, #143536, .T. ) ;
#30910 = CARTESIAN_POINT ( 'NONE',  ( -11.51078643762690490, -27.52281430457047406, 5.000000000000000000 ) ) ;
#30911 = DIRECTION ( 'NONE',  ( -0.7071067811865487940, -0.7071067811865463515, -0.000000000000000000 ) ) ;
#30912 = CARTESIAN_POINT ( 'NONE',  ( -53.99451991528749062, 28.92564299267975869, 4.000000000000000000 ) ) ;
#30913 = CARTESIAN_POINT ( 'NONE',  ( 0.000000000000000000, 0.000000000000000000, 5.000000000000000000 ) ) ;
#30915 = ORIENTED_EDGE ( 'NONE', *, *, #88710, .T. ) ;
#30914 = DIRECTION ( 'NONE',  ( -0.7071067811865486830, -0.7071067811865464625, 0.000000000000000000 ) ) ;
#30916 = DIRECTION ( 'NONE',  ( -0.7071067811865486830, -0.7071067811865464625, 0.000000000000000000 ) ) ;
#30917 = CARTESIAN_POINT ( 'NONE',  ( -10.49999999999992362, -17.91344420646043289, 1.358650452708439538 ) ) ;
#30918 = DIRECTION ( 'NONE',  ( -0.7071067811865486830, -0.7071067811865464625, 0.000000000000000000 ) ) ;
#30919 = CIRCLE ( 'NONE', #23971, 2.055000000000000604 ) ;
#30920 = LINE ( 'NONE', #72316, #72468 ) ;
#30921 = VERTEX_POINT ( 'NONE', #2101 ) ;
#30922 = EDGE_LOOP ( 'NONE', ( #33891, #27227, #111118, #131288 ) ) ;
#30923 = CARTESIAN_POINT ( 'NONE',  ( 60.95876352523143993, 0.000000000000000000, -6.110000000000001208 ) ) ;
#30924 = AXIS2_PLACEMENT_3D ( 'NONE', #116787, #139998, #17469 ) ;
#30925 = VERTEX_POINT ( 'NONE', #68863 ) ;
#30926 = CARTESIAN_POINT ( 'NONE',  ( 0.000000000000000000, 0.000000000000000000, 0.000000000000000000 ) ) ;
#30927 = EDGE_CURVE ( 'NONE', #119366, #116312, #132705, .T. ) ;
#30928 = DIRECTION ( 'NONE',  ( 0.3543493200069162685, -0.000000000000000000, -0.9351131265310288487 ) ) ;
#30929 = LINE ( 'NONE', #119323, #98895 ) ;
#30930 = CARTESIAN_POINT ( 'NONE',  ( -42.18398860626899705, 28.73617430169816700, 5.000000000000000000 ) ) ;
#30931 = EDGE_LOOP ( 'NONE', ( #38694, #19122, #36948, #58121, #142640 ) ) ;
#30932 = LINE ( 'NONE', #20013, #88603 ) ;
#30933 = CARTESIAN_POINT ( 'NONE',  ( 35.99451991528749772, 28.92564299267963079, 4.000000000000000000 ) ) ;
#30934 = VECTOR ( 'NONE', #79357, 1000.000000000000227 ) ;
#30935 = ADVANCED_FACE ( 'NONE', ( #23915 ), #68176, .T. ) ;
#30936 = ADVANCED_FACE ( 'NONE', ( #101453 ), #26752, .T. ) ;
#30937 = VERTEX_POINT ( 'NONE', #83282 ) ;
#30938 = AXIS2_PLACEMENT_3D ( 'NONE', #57586, #58331, #88782 ) ;
#30939 = FACE_OUTER_BOUND ( 'NONE', #87273, .T. ) ;
#30940 = CARTESIAN_POINT ( 'NONE',  ( 1.042387978378689573, -0.3999999999999998002, -2.015694669338588429 ) ) ;
#30941 = CARTESIAN_POINT ( 'NONE',  ( 42.18398860626899705, 28.73617430169816700, 5.000000000000000000 ) ) ;
#30942 = EDGE_CURVE ( 'NONE', #41501, #105119, #94136, .T. ) ;
#30943 = VERTEX_POINT ( 'NONE', #36907 ) ;
#30945 = ORIENTED_EDGE ( 'NONE', *, *, #48524, .F. ) ;
#30944 = VECTOR ( 'NONE', #138886, 1000.000000000000000 ) ;
#30946 = EDGE_CURVE ( 'NONE', #20788, #112121, #105711, .T. ) ;
#30947 = FACE_BOUND ( 'NONE', #72021, .T. ) ;
#30948 = EDGE_CURVE ( 'NONE', #78047, #59514, #49955, .T. ) ;
#30949 = CARTESIAN_POINT ( 'NONE',  ( -24.31657961132774304, -6.740707523384216415, 11.88629033278130009 ) ) ;
#30950 = LINE ( 'NONE', #31649, #42085 ) ;
#30951 = CARTESIAN_POINT ( 'NONE',  ( 62.25000000000000000, -9.735942053221458872E-16, 7.950000000000000178 ) ) ;
#30952 = FILL_AREA_STYLE_COLOUR ( '', #94338 ) ;
#30953 = VECTOR ( 'NONE', #97610, 1000.000000000000000 ) ;
#30954 = LINE ( 'NONE', #120036, #113723 ) ;
#30955 = EDGE_LOOP ( 'NONE', ( #103017, #111021, #41742 ) ) ;
#30956 = ADVANCED_FACE ( 'NONE', ( #114463 ), #92710, .F. ) ;
#30957 = AXIS2_PLACEMENT_3D ( 'NONE', #7949, #118127, #18834 ) ;
#30958 = VERTEX_POINT ( 'NONE', #50647 ) ;
#30959 = ORIENTED_EDGE ( 'NONE', *, *, #34919, .F. ) ;
#30960 = EDGE_CURVE ( 'NONE', #45624, #28995, #38354, .T. ) ;
#30961 = EDGE_LOOP ( 'NONE', ( #60954, #15373, #65312, #124943 ) ) ;
#30962 = VECTOR ( 'NONE', #133256, 1000.000000000000000 ) ;
#30963 = CARTESIAN_POINT ( 'NONE',  ( 184.1173099067358123, -47.89015928896270680, 37.22465919495247988 ) ) ;
#30964 = EDGE_CURVE ( 'NONE', #89868, #114456, #72449, .T. ) ;
#30965 =( BOUNDED_CURVE ( )  B_SPLINE_CURVE ( 2, ( #126438, #29979, #115530, #38735, #118413 ),
 .UNSPECIFIED., .F., .F. ) 
 B_SPLINE_CURVE_WITH_KNOTS ( ( 3, 2, 3 ),
 ( 0.9711948811556444516, 0.9722222222222222099, 0.9749999999999999778 ),
 .UNSPECIFIED. ) 
 CURVE ( )  GEOMETRIC_REPRESENTATION_ITEM ( )  RATIONAL_B_SPLINE_CURVE ( ( 0.9841174075436982527, 0.9873979127333399886, 1.000000000000000000, 0.9659258262890683122, 1.000000000000000000 ) ) 
 REPRESENTATION_ITEM ( '' )  );
#30966 = DIRECTION ( 'NONE',  ( -0.6830127018922180770, -0.6830127018922204085, -0.2588190451025213501 ) ) ;
#30967 = DIRECTION ( 'NONE',  ( 0.6830127018922181881, 0.6830127018922202975, -0.2588190451025214056 ) ) ;
#30968 = ORIENTED_EDGE ( 'NONE', *, *, #99413, .T. ) ;
#30969 = FACE_OUTER_BOUND ( 'NONE', #99228, .T. ) ;
#30970 = CARTESIAN_POINT ( 'NONE',  ( -33.48921356237309510, -27.52281430457078670, 5.000000000000000000 ) ) ;
#30971 = CARTESIAN_POINT ( 'NONE',  ( -36.18398860626899705, 28.73617430169812437, 5.000000000000000000 ) ) ;
#30972 = DIRECTION ( 'NONE',  ( 0.6830127018922180770, -0.6830127018922204085, -0.2588190451025213501 ) ) ;
#30973 = VECTOR ( 'NONE', #138881, 1000.000000000000000 ) ;
#30974 = DIRECTION ( 'NONE',  ( -1.000000000000000000, 0.000000000000000000, 0.000000000000000000 ) ) ;
#30975 = VERTEX_POINT ( 'NONE', #26052 ) ;
#30976 = DIRECTION ( 'NONE',  ( 0.7071067811865487940, 0.7071067811865463515, -0.000000000000000000 ) ) ;
#30977 = CARTESIAN_POINT ( 'NONE',  ( -9.489213562373095101, -27.52281430457062328, 5.000000000000000000 ) ) ;
#30978 = ORIENTED_EDGE ( 'NONE', *, *, #29396, .T. ) ;
#30979 = CARTESIAN_POINT ( 'NONE',  ( 29.99999999999999645, -2.375000000000000000, 4.319999999999998508 ) ) ;
#30980 = ORIENTED_EDGE ( 'NONE', *, *, #29487, .F. ) ;
#30981 = ORIENTED_EDGE ( 'NONE', *, *, #29424, .F. ) ;
#30982 = EDGE_LOOP ( 'NONE', ( #39881, #77380, #114725 ) ) ;
#30983 =( GEOMETRIC_REPRESENTATION_CONTEXT ( 3 ) GLOBAL_UNCERTAINTY_ASSIGNED_CONTEXT ( ( #121432 ) ) GLOBAL_UNIT_ASSIGNED_CONTEXT ( ( #1627, #38405, #77812 ) ) REPRESENTATION_CONTEXT ( 'NONE', 'WORKASPACE' ) );
#30984 = CARTESIAN_POINT ( 'NONE',  ( 61.68793019189811844, 6.110000000000002984, -1.637169565754156730 ) ) ;
#30985 = EDGE_CURVE ( 'NONE', #51277, #27734, #9716, .T. ) ;
#30986 = ORIENTED_EDGE ( 'NONE', *, *, #97063, .F. ) ;
#30987 = EDGE_LOOP ( 'NONE', ( #119462, #27613, #18962, #69536 ) ) ;
#30988 = ADVANCED_FACE ( 'NONE', ( #71001 ), #59421, .F. ) ;
#30989 = LINE ( 'NONE', #33153, #9471 ) ;
#30990 = ADVANCED_FACE ( 'NONE', ( #138374 ), #25313, .F. ) ;
#30991 = VECTOR ( 'NONE', #67750, 1000.000000000000000 ) ;
#30992 = CARTESIAN_POINT ( 'NONE',  ( 96.97959685856477563, 6.109999999999999432, 1.637169565754164280 ) ) ;
#30993 = LINE ( 'NONE', #9919, #58772 ) ;
#30994 = CARTESIAN_POINT ( 'NONE',  ( -32.99451991528749062, 28.92564299267960948, 4.000000000000000000 ) ) ;
#30995 = VERTEX_POINT ( 'NONE', #126085 ) ;
#30996 = CARTESIAN_POINT ( 'NONE',  ( -23.56319896779156409, -12.74070752338415069, 9.898150129686429821 ) ) ;
#30997 = EDGE_CURVE ( 'NONE', #115411, #100841, #104287, .T. ) ;
#30998 = FACE_OUTER_BOUND ( 'NONE', #126996, .T. ) ;
#30999 = VECTOR ( 'NONE', #2004, 999.9999999999998863 ) ;
#31000 = CARTESIAN_POINT ( 'NONE',  ( 90.39583333333335702, -2.130196079827389344, 7.950000000000021494 ) ) ;
#31001 = CARTESIAN_POINT ( 'NONE',  ( -14.81601139373099585, 28.73617430169776910, 5.000000000000000000 ) ) ;
#31002 = ORIENTED_EDGE ( 'NONE', *, *, #93401, .T. ) ;
#31003 = CARTESIAN_POINT ( 'NONE',  ( 30.51665438641024153, 22.22500000000000142, 4.500000000000000888 ) ) ;
#31004 = VERTEX_POINT ( 'NONE', #103581 ) ;
#31005 = EDGE_LOOP ( 'NONE', ( #38274, #105064, #132855, #73659 ) ) ;
#31006 = VERTEX_POINT ( 'NONE', #70314 ) ;
#31007 = CARTESIAN_POINT ( 'NONE',  ( 118.4745968585647944, 1.637169565754164280, -6.109999999999996767 ) ) ;
#31008 = ORIENTED_EDGE ( 'NONE', *, *, #38366, .F. ) ;
#31009 = CARTESIAN_POINT ( 'NONE',  ( -33.52781275693359220, 22.22500000000000142, 4.470553524000289158 ) ) ;
#31010 = CARTESIAN_POINT ( 'NONE',  ( 5.161706124526165951, -6.740707523384212863, 16.75550250614868730 ) ) ;
#31011 = DIRECTION ( 'NONE',  ( -0.6830127018922181881, 0.6830127018922202975, -0.2588190451025214056 ) ) ;
#31012 = ORIENTED_EDGE ( 'NONE', *, *, #7701, .F. ) ;
#31013 = SURFACE_STYLE_FILL_AREA ( #95520 ) ;
#31014 = ORIENTED_EDGE ( 'NONE', *, *, #10048, .F. ) ;
#31015 = VECTOR ( 'NONE', #86777, 1000.000000000000000 ) ;
#31016 = AXIS2_PLACEMENT_3D ( 'NONE', #10348, #40859, #43011 ) ;
#31017 = CARTESIAN_POINT ( 'NONE',  ( 3.332903141435219929, -3.967499999999994476, 6.871911579029513106 ) ) ;
#31018 = LINE ( 'NONE', #22232, #62375 ) ;
#31019 = DIRECTION ( 'NONE',  ( 0.000000000000000000, -1.000000000000000000, 0.000000000000000000 ) ) ;
#31020 = CARTESIAN_POINT ( 'NONE',  ( 38.62499999999999289, -7.950000000000000178, -4.867971026610729436E-16 ) ) ;
#31021 = ORIENTED_EDGE ( 'NONE', *, *, #30334, .F. ) ;
#31022 = ORIENTED_EDGE ( 'NONE', *, *, #58409, .F. ) ;
#31023 = ADVANCED_FACE ( 'NONE', ( #36221 ), #5688, .F. ) ;
#31024 = EDGE_LOOP ( 'NONE', ( #51172, #9490, #4090, #24710 ) ) ;
#31025 = DIRECTION ( 'NONE',  ( 1.000000000000000000, 0.000000000000000000, 0.000000000000000000 ) ) ;
#31026 = DIRECTION ( 'NONE',  ( 1.000000000000000000, 0.000000000000000000, 0.000000000000000000 ) ) ;
#31027 = AXIS2_PLACEMENT_3D ( 'NONE', #134416, #111949, #12609 ) ;
#31028 = DIRECTION ( 'NONE',  ( -0.000000000000000000, 0.000000000000000000, 1.000000000000000000 ) ) ;
#31029 = LINE ( 'NONE', #85373, #82826 ) ;
#31030 = DIRECTION ( 'NONE',  ( 0.6830127018922180770, -0.6830127018922204085, -0.2588190451025213501 ) ) ;
#31031 = CONICAL_SURFACE ( 'NONE', #17156, 2.055000000000000604, 0.9599310885968764806 ) ;
#31032 = CARTESIAN_POINT ( 'NONE',  ( 29.89626352523142927, 4.472830434245840259, -4.472830434245839371 ) ) ;
#31033 = LINE ( 'NONE', #75259, #49019 ) ;
#31034 = DIRECTION ( 'NONE',  ( -1.000000000000000000, -1.224606353822377258E-16, -0.000000000000000000 ) ) ;
#31035 = EDGE_LOOP ( 'NONE', ( #105093, #31507, #131905, #42861 ) ) ;
#31036 = LINE ( 'NONE', #9208, #46597 ) ;
#31037 = CARTESIAN_POINT ( 'NONE',  ( -21.87889065874226091, 8.431076354171498366, 5.000000000000000000 ) ) ;
#31038 = EDGE_LOOP ( 'NONE', ( #75847, #70624, #141419, #108708 ) ) ;
#31039 = VECTOR ( 'NONE', #85732, 1000.000000000000000 ) ;
#31040 = EDGE_CURVE ( 'NONE', #90453, #28286, #139438, .T. ) ;
#31041 = DIRECTION ( 'NONE',  ( 0.7071067811865487940, 0.7071067811865463515, -0.000000000000000000 ) ) ;
#31043 = ORIENTED_EDGE ( 'NONE', *, *, #138129, .T. ) ;
#31042 = FACE_OUTER_BOUND ( 'NONE', #56364, .T. ) ;
#31044 = VECTOR ( 'NONE', #89990, 1000.000000000000000 ) ;
#31045 = EDGE_CURVE ( 'NONE', #115828, #45804, #27443, .T. ) ;
#31046 = DIRECTION ( 'NONE',  ( -1.000000000000000000, -1.224606353822377258E-16, -0.000000000000000000 ) ) ;
#31047 = ORIENTED_EDGE ( 'NONE', *, *, #126142, .F. ) ;
#31048 = ORIENTED_EDGE ( 'NONE', *, *, #94457, .F. ) ;
#31049 = DIRECTION ( 'NONE',  ( 0.7071067811865486830, -0.7071067811865464625, -0.000000000000000000 ) ) ;
#31050 = ORIENTED_EDGE ( 'NONE', *, *, #82453, .F. ) ;
#31052 = EDGE_CURVE ( 'NONE', #35520, #21301, #49254, .T. ) ;
#31051 = VECTOR ( 'NONE', #118108, 1000.000000000000114 ) ;
#31053 = EDGE_CURVE ( 'NONE', #107783, #73971, #136222, .T. ) ;
#31054 =( LENGTH_UNIT ( ) NAMED_UNIT ( * ) SI_UNIT ( .MILLI., .METRE. ) );
#31055 = CARTESIAN_POINT ( 'NONE',  ( 109.3083603837961988, 7.949999999999997513, 2.130196079827431088 ) ) ;
#31057 = MECHANICAL_DESIGN_GEOMETRIC_PRESENTATION_REPRESENTATION (  '', ( #95913 ), #56647 ) ;
#31056 = CARTESIAN_POINT ( 'NONE',  ( 49.66252705046289861, 7.949999999999998401, 1.460391307983218338E-15 ) ) ;
#31058 = CARTESIAN_POINT ( 'NONE',  ( 14.29289321881335795, 14.25929247661557397, 5.000000000000000000 ) ) ;
#31059 = ADVANCED_FACE ( 'NONE', ( #40506 ), #19443, .F. ) ;
#31060 = DIRECTION ( 'NONE',  ( 0.000000000000000000, 0.000000000000000000, -1.000000000000000000 ) ) ;
#31061 = DIRECTION ( 'NONE',  ( -0.000000000000000000, -1.000000000000000000, -0.000000000000000000 ) ) ;
#31062 = LINE ( 'NONE', #119446, #101724 ) ;
#31063 = CARTESIAN_POINT ( 'NONE',  ( 5.541666666666666963, 3.047499999999993214, -5.278424836066146320 ) ) ;
#31064 = CARTESIAN_POINT ( 'NONE',  ( 21.56206980810188867, -7.934999999999990727, -2.126176841940955242 ) ) ;
#31065 = VECTOR ( 'NONE', #122824, 1000.000000000000000 ) ;
#31066 = DIRECTION ( 'NONE',  ( -1.000000000000000000, 0.000000000000000000, -0.000000000000000000 ) ) ;
#31067 = DIRECTION ( 'NONE',  ( -0.7071067811865486830, -0.7071067811865464625, -0.000000000000000000 ) ) ;
#31068 = EDGE_LOOP ( 'NONE', ( #59240, #80088, #117285, #35405 ) ) ;
#31069 = ORIENTED_EDGE ( 'NONE', *, *, #19558, .T. ) ;
#31070 = ADVANCED_FACE ( 'NONE', ( #64381 ), #73141, .F. ) ;
#31071 = AXIS2_PLACEMENT_3D ( 'NONE', #131892, #32586, #119544 ) ;
#31072 = FACE_OUTER_BOUND ( 'NONE', #40731, .T. ) ;
#31073 = VERTEX_POINT ( 'NONE', #128915 ) ;
#31074 = PLANE ( 'NONE',  #136005 ) ;
#31075 = AXIS2_PLACEMENT_3D ( 'NONE', #68832, #26016, #137644 ) ;
#31076 = CARTESIAN_POINT ( 'NONE',  ( 127.4973405139118228, -50.37061236291009436, -37.32649486623493829 ) ) ;
#31077 = EDGE_LOOP ( 'NONE', ( #95927, #28829, #84910, #6426 ) ) ;
#31078 = EDGE_CURVE ( 'NONE', #15191, #97431, #56136, .T. ) ;
#31079 = CARTESIAN_POINT ( 'NONE',  ( 10.49999999999993605, -20.94781430457060623, 5.000000000000000000 ) ) ;
#31080 = DIRECTION ( 'NONE',  ( -0.7071067811865486830, -0.7071067811865464625, 0.000000000000000000 ) ) ;
#31081 = CARTESIAN_POINT ( 'NONE',  ( 66.48921356237309510, -27.52281430457101763, 5.000000000000000000 ) ) ;
#31083 = VERTEX_POINT ( 'NONE', #51375 ) ;
#31082 = DIRECTION ( 'NONE',  ( 0.6830127018922180770, -0.6830127018922204085, -0.2588190451025213501 ) ) ;
#31084 = CARTESIAN_POINT ( 'NONE',  ( 19.49999999999986855, -10.53360074219763121, 5.000000000000000000 ) ) ;
#31085 = ADVANCED_FACE ( 'NONE', ( #130368, #18704 ), #8519, .F. ) ;
#31086 = CARTESIAN_POINT ( 'NONE',  ( 0.000000000000000000, 0.000000000000000000, 5.000000000000000000 ) ) ;
#31087 = CARTESIAN_POINT ( 'NONE',  ( 25.97159235450331849, 2.500000000000001776, 0.000000000000000000 ) ) ;
#31088 = CARTESIAN_POINT ( 'NONE',  ( 14.08373646989360317, 3.821174125832445049E-16, 0.000000000000000000 ) ) ;
#31089 = CARTESIAN_POINT ( 'NONE',  ( 58.77385498567259958, -47.18881911353556546, 35.55177538329026277 ) ) ;
#31090 = ORIENTED_EDGE ( 'NONE', *, *, #72203, .T. ) ;
#31091 = ORIENTED_EDGE ( 'NONE', *, *, #7019, .F. ) ;
#31092 = ORIENTED_EDGE ( 'NONE', *, *, #18427, .T. ) ;
#31093 = CARTESIAN_POINT ( 'NONE',  ( 102.6670968585647756, -3.055000000000000160, -5.291415217122921177 ) ) ;
#31094 = VERTEX_POINT ( 'NONE', #62254 ) ;
#31095 = ADVANCED_FACE ( 'NONE', ( #84707 ), #29592, .F. ) ;
#31096 = CARTESIAN_POINT ( 'NONE',  ( 128.5065401839287631, -48.97294124528377779, 39.12804664298170820 ) ) ;
#31097 = DIRECTION ( 'NONE',  ( -0.000000000000000000, 0.3543493200069153248, 0.9351131265310292928 ) ) ;
#31098 = VERTEX_POINT ( 'NONE', #119444 ) ;
#31099 = LINE ( 'NONE', #121640, #16652 ) ;
#31101 = VECTOR ( 'NONE', #21855, 999.9999999999998863 ) ;
#31100 = DIRECTION ( 'NONE',  ( 0.3543493200069162685, -0.000000000000000000, -0.9351131265310288487 ) ) ;
#31102 = EDGE_CURVE ( 'NONE', #46563, #114228, #65121, .T. ) ;
#31103 = CARTESIAN_POINT ( 'NONE',  ( 99.95376352523145158, -6.109999999999998543, -3.741295971395162543E-16 ) ) ;
#31104 = ORIENTED_EDGE ( 'NONE', *, *, #135501, .F. ) ;
#31105 = EDGE_CURVE ( 'NONE', #105446, #54652, #74560, .T. ) ;
#31106 = CARTESIAN_POINT ( 'NONE',  ( 48.18398860626899705, 28.73617430169820608, 5.000000000000000000 ) ) ;
#31107 = CARTESIAN_POINT ( 'NONE',  ( 28.00000000000002487, -49.14999999999999147, 40.92499999999998295 ) ) ;
#31108 = CARTESIAN_POINT ( 'NONE',  ( 115.1874999999999858, -5.819803920172573974, 5.819803920172573086 ) ) ;
#31109 = CARTESIAN_POINT ( 'NONE',  ( -45.48921356237309510, -27.52281430457087197, 5.000000000000000000 ) ) ;
#31110 = EDGE_CURVE ( 'NONE', #47599, #45624, #131068, .T. ) ;
#31111 = EDGE_LOOP ( 'NONE', ( #82253, #89209 ) ) ;
#31112 = ORIENTED_EDGE ( 'NONE', *, *, #81751, .T. ) ;
#31113 = ORIENTED_EDGE ( 'NONE', *, *, #35551, .T. ) ;
#31114 = DIRECTION ( 'NONE',  ( 1.000000000000000000, 0.000000000000000000, 0.000000000000000000 ) ) ;
#31115 = LINE ( 'NONE', #8574, #68688 ) ;
#31116 = CARTESIAN_POINT ( 'NONE',  ( 19.75456980810189123, -6.871911579029512218, 3.967499999999996252 ) ) ;
#31117 = VECTOR ( 'NONE', #66118, 1000.000000000000000 ) ;
#31118 = CARTESIAN_POINT ( 'NONE',  ( -8.510786437626906675, -27.52281430457049183, 5.000000000000000000 ) ) ;
#31119 = DIRECTION ( 'NONE',  ( -0.6830127018922181881, 0.6830127018922202975, -0.2588190451025214056 ) ) ;
#31120 = SHAPE_REPRESENTATION_RELATIONSHIP ( 'NONE' , 'NONE' ,  #104156, #50002 ) ;
#31121 = AXIS2_PLACEMENT_3D ( 'NONE', #111445, #143362, #20141 ) ;
#31122 = VERTEX_POINT ( 'NONE', #41929 ) ;
#31123 =( BOUNDED_CURVE ( )  B_SPLINE_CURVE ( 3, ( #105872, #126234, #95001, #82050 ),
 .UNSPECIFIED., .F., .T. ) 
 B_SPLINE_CURVE_WITH_KNOTS ( ( 4, 4 ),
 ( 5.920967161967926273, 7.341195215986587641 ),
 .UNSPECIFIED. ) 
 CURVE ( )  GEOMETRIC_REPRESENTATION_ITEM ( )  RATIONAL_B_SPLINE_CURVE ( ( 1.000000000000000000, 0.8388583629366720418, 0.8388583629366720418, 1.000000000000000000 ) ) 
 REPRESENTATION_ITEM ( '' )  );
#31124 = ORIENTED_EDGE ( 'NONE', *, *, #116696, .F. ) ;
#31125 = EDGE_CURVE ( 'NONE', #65367, #88773, #7100, .T. ) ;
#31126 = DIRECTION ( 'NONE',  ( 0.6830127018922181881, 0.6830127018922202975, -0.2588190451025214056 ) ) ;
#31127 = ORIENTED_EDGE ( 'NONE', *, *, #35558, .T. ) ;
#31128 = ORIENTED_EDGE ( 'NONE', *, *, #118076, .F. ) ;
#31129 = ADVANCED_FACE ( 'NONE', ( #31757 ), #96961, .F. ) ;
#31130 = SURFACE_STYLE_FILL_AREA ( #422 ) ;
#31131 = DIRECTION ( 'NONE',  ( -0.7071067811865487940, 0.7071067811865463515, 0.000000000000000000 ) ) ;
#31132 = ORIENTED_EDGE ( 'NONE', *, *, #100401, .T. ) ;
#31133 = AXIS2_PLACEMENT_3D ( 'NONE', #121570, #45488, #89665 ) ;
#31134 = CARTESIAN_POINT ( 'NONE',  ( 55.68749999999999289, -5.819803920172573974, 5.819803920172573086 ) ) ;
#31135 = PRESENTATION_STYLE_ASSIGNMENT (( #120967 ) ) ;
#31136 = VECTOR ( 'NONE', #18205, 1000.000000000000000 ) ;
#31137 = DIRECTION ( 'NONE',  ( -0.7071067811865487940, 0.7071067811865463515, 0.000000000000000000 ) ) ;
#31138 = CARTESIAN_POINT ( 'NONE',  ( -34.92500000000001137, 8.816654386410331057, 4.500000000000000888 ) ) ;
#31139 = DIRECTION ( 'NONE',  ( -0.7071067811865487940, 0.7071067811865463515, 0.000000000000000000 ) ) ;
#31140 = VERTEX_POINT ( 'NONE', #75974 ) ;
#31141 = FILL_AREA_STYLE ('',( #63770 ) ) ;
#31143 = ORIENTED_EDGE ( 'NONE', *, *, #38419, .F. ) ;
#31142 = VECTOR ( 'NONE', #31191, 999.9999999999998863 ) ;
#31144 = CARTESIAN_POINT ( 'NONE',  ( 25.39999999999999147, 4.335470510665683896, -6.649025316336889091 ) ) ;
#31145 = LINE ( 'NONE', #75359, #96689 ) ;
#31146 = VERTEX_POINT ( 'NONE', #53512 ) ;
#31147 =( NAMED_UNIT ( * ) SI_UNIT ( $, .STERADIAN. ) SOLID_ANGLE_UNIT ( ) );
#31148 = VERTEX_POINT ( 'NONE', #109308 ) ;
#31149 = DIRECTION ( 'NONE',  ( -0.000000000000000000, 0.3543493200069153248, 0.9351131265310292928 ) ) ;
#31150 = EDGE_LOOP ( 'NONE', ( #104924, #54101, #43377, #134158 ) ) ;
#31151 = ORIENTED_EDGE ( 'NONE', *, *, #19232, .F. ) ;
#31152 =( BOUNDED_CURVE ( )  B_SPLINE_CURVE ( 2, ( #79676, #1316, #55740, #69480, #58644, #101363, #123144, #57899, #78932, #68767, #133307, #45597, #99945 ),
 .UNSPECIFIED., .F., .T. ) 
 B_SPLINE_CURVE_WITH_KNOTS ( ( 3, 2, 2, 2, 2, 2, 3 ),
 ( 0.6833333333333333481, 0.6861111111111111160, 0.6888888888888888840, 0.6916666666666666519, 0.6944444444444444198, 0.6972222222222221877, 0.6999999999999999556 ),
 .UNSPECIFIED. ) 
 CURVE ( )  GEOMETRIC_REPRESENTATION_ITEM ( )  RATIONAL_B_SPLINE_CURVE ( ( 1.000000000000000000, 0.9659258262890683122, 1.000000000000000000, 0.9659258262890683122, 1.000000000000000000, 0.9659258262890683122, 1.000000000000000000, 0.9659258262890683122, 1.000000000000000000, 0.9659258262890683122, 1.000000000000000000, 0.9659258262890683122, 1.000000000000000000 ) ) 
 REPRESENTATION_ITEM ( '' )  );
#31153 = ORIENTED_EDGE ( 'NONE', *, *, #66417, .T. ) ;
#31154 = VECTOR ( 'NONE', #27371, 1000.000000000000227 ) ;
#31155 = CARTESIAN_POINT ( 'NONE',  ( 28.05793019189811233, 6.110000000000000320, -1.637169565754156064 ) ) ;
#31156 = FACE_OUTER_BOUND ( 'NONE', #60647, .T. ) ;
#31157 = MECHANICAL_DESIGN_GEOMETRIC_PRESENTATION_REPRESENTATION (  '', ( #119088 ), #130717 ) ;
#31158 = CARTESIAN_POINT ( 'NONE',  ( 6.792893218813416567, -14.24070752338413826, 5.000000000000000000 ) ) ;
#31159 = DIRECTION ( 'NONE',  ( -0.000000000000000000, 0.000000000000000000, 1.000000000000000000 ) ) ;
#31160 = LINE ( 'NONE', #75369, #11401 ) ;
#31161 = CARTESIAN_POINT ( 'NONE',  ( -22.17183060077631396, 12.75929247661558996, 4.000000000000000000 ) ) ;
#31162 = DIRECTION ( 'NONE',  ( -0.000000000000000000, 0.000000000000000000, 1.000000000000000000 ) ) ;
#31163 = PLANE ( 'NONE',  #110600 ) ;
#31164 = LINE ( 'NONE', #141325, #58500 ) ;
#31165 = DIRECTION ( 'NONE',  ( 0.6830127018922180770, -0.6830127018922204085, -0.2588190451025213501 ) ) ;
#31166 = LINE ( 'NONE', #31864, #99177 ) ;
#31167 = LINE ( 'NONE', #30441, #12346 ) ;
#31168 = ORIENTED_EDGE ( 'NONE', *, *, #65388, .T. ) ;
#31169 = VERTEX_POINT ( 'NONE', #120145 ) ;
#31170 = ORIENTED_EDGE ( 'NONE', *, *, #99427, .T. ) ;
#31171 = ORIENTED_EDGE ( 'NONE', *, *, #59376, .F. ) ;
#31172 = PLANE ( 'NONE',  #132903 ) ;
#31173 = VERTEX_POINT ( 'NONE', #86139 ) ;
#31174 = ORIENTED_EDGE ( 'NONE', *, *, #126256, .T. ) ;
#31175 = CARTESIAN_POINT ( 'NONE',  ( 21.18398860626899349, 28.73617430169802134, 5.000000000000000000 ) ) ;
#31176 = DIRECTION ( 'NONE',  ( -1.000000000000000000, 0.000000000000000000, -0.000000000000000000 ) ) ;
#31177 = DIRECTION ( 'NONE',  ( 0.7071067811865486830, -0.7071067811865464625, -0.000000000000000000 ) ) ;
#31178 = ORIENTED_EDGE ( 'NONE', *, *, #23028, .F. ) ;
#31179 = CARTESIAN_POINT ( 'NONE',  ( 11.99999999999991651, -12.41253812416062985, 4.000000000000000000 ) ) ;
#31180 = ORIENTED_EDGE ( 'NONE', *, *, #40698, .T. ) ;
#31181 = DIRECTION ( 'NONE',  ( 0.7071067811865487940, 0.7071067811865463515, -0.000000000000000000 ) ) ;
#31182 = DIRECTION ( 'NONE',  ( 0.7071067811865487940, -0.7071067811865463515, 0.000000000000000000 ) ) ;
#31183 = CARTESIAN_POINT ( 'NONE',  ( 10.71290314143521982, 3.967499999999992699, -6.871911579029513994 ) ) ;
#31184 = ORIENTED_EDGE ( 'NONE', *, *, #71887, .F. ) ;
#31185 = CARTESIAN_POINT ( 'NONE',  ( 93.68293019189812298, -1.637169565754159173, -6.109999999999999432 ) ) ;
#31186 = CARTESIAN_POINT ( 'NONE',  ( 8.900575677527392315, -8.548178872310858267, -4.146506754080105495 ) ) ;
#31187 = DIRECTION ( 'NONE',  ( -0.7071067811865486830, 0.7071067811865464625, 0.000000000000000000 ) ) ;
#31188 = LINE ( 'NONE', #75405, #79042 ) ;
#31189 = ORIENTED_EDGE ( 'NONE', *, *, #68640, .F. ) ;
#31190 = ORIENTED_EDGE ( 'NONE', *, *, #30250, .T. ) ;
#31191 = DIRECTION ( 'NONE',  ( 0.5735764363510448272, -0.8191520442889927978, 1.003171929053526103E-16 ) ) ;
#31192 = ORIENTED_EDGE ( 'NONE', *, *, #119877, .T. ) ;
#31193 = LINE ( 'NONE', #62401, #25500 ) ;
#31194 = DIRECTION ( 'NONE',  ( 0.000000000000000000, 0.3543493200069153248, 0.9351131265310291818 ) ) ;
#31195 = FACE_OUTER_BOUND ( 'NONE', #25236, .T. ) ;
#31196 = CARTESIAN_POINT ( 'NONE',  ( 20.99451991528748707, 28.92564299267952777, 4.000000000000000000 ) ) ;
#31198 = ORIENTED_EDGE ( 'NONE', *, *, #142652, .F. ) ;
#31197 = AXIS2_PLACEMENT_3D ( 'NONE', #99969, #55767, #108656 ) ;
#31199 = CARTESIAN_POINT ( 'NONE',  ( 34.92500000000001847, 0.4299755680430066840, -27.68972139052992532 ) ) ;
#31200 = DIRECTION ( 'NONE',  ( -0.3543493200069162685, -0.000000000000000000, -0.9351131265310288487 ) ) ;
#31202 = ADVANCED_FACE ( 'NONE', ( #63693 ), #84029, .F. ) ;
#31201 = CARTESIAN_POINT ( 'NONE',  ( 0.000000000000000000, 0.000000000000000000, 0.000000000000000000 ) ) ;
#31203 = VERTEX_POINT ( 'NONE', #108552 ) ;
#31204 = LINE ( 'NONE', #139267, #79117 ) ;
#31205 = DIRECTION ( 'NONE',  ( 0.7071067811865487940, 0.7071067811865463515, 0.000000000000000000 ) ) ;
#31206 = EDGE_LOOP ( 'NONE', ( #39720, #60784, #101843, #7307 ) ) ;
#31208 = ORIENTED_EDGE ( 'NONE', *, *, #35306, .F. ) ;
#31207 = CARTESIAN_POINT ( 'NONE',  ( -12.69326993309591245, -3.740707523384244837, 12.88036043432870592 ) ) ;
#31209 = VERTEX_POINT ( 'NONE', #95572 ) ;
#31210 = EDGE_CURVE ( 'NONE', #86264, #53831, #9993, .T. ) ;
#31211 = EDGE_CURVE ( 'NONE', #141704, #67140, #117306, .T. ) ;
#31212 = LINE ( 'NONE', #40659, #28470 ) ;
#31213 = LINE ( 'NONE', #75429, #22912 ) ;
#31214 = ORIENTED_EDGE ( 'NONE', *, *, #56724, .T. ) ;
#31215 = DIRECTION ( 'NONE',  ( -0.000000000000000000, 0.3543493200069153248, 0.9351131265310292928 ) ) ;
#31216 = EDGE_CURVE ( 'NONE', #21579, #15722, #46232, .T. ) ;
#31217 = EDGE_CURVE ( 'NONE', #38500, #44746, #132535, .T. ) ;
#31218 = DIRECTION ( 'NONE',  ( 0.7071067811865487940, 0.7071067811865463515, 0.000000000000000000 ) ) ;
#31219 = VECTOR ( 'NONE', #102400, 999.9999999999998863 ) ;
#31220 = CARTESIAN_POINT ( 'NONE',  ( -16.17183060077635659, -11.24070752338416135, 4.000000000000000000 ) ) ;
#31221 = PLANE ( 'NONE',  #13731 ) ;
#31223 = CARTESIAN_POINT ( 'NONE',  ( 31.18749999999998934, -5.819803920172573974, 5.819803920172573086 ) ) ;
#31222 = AXIS2_PLACEMENT_3D ( 'NONE', #34269, #77780, #122687 ) ;
#31224 = ADVANCED_FACE ( 'NONE', ( #111444 ), #53742, .T. ) ;
#31225 = CARTESIAN_POINT ( 'NONE',  ( 78.18398860626899705, 28.73617430169841924, 5.000000000000000000 ) ) ;
#31226 = CARTESIAN_POINT ( 'NONE',  ( -31.17183060077625356, -20.24070752338407075, 4.000000000000000000 ) ) ;
#31227 = CARTESIAN_POINT ( 'NONE',  ( -6.489213562373093325, -27.52281430457059841, 5.000000000000000000 ) ) ;
#31228 = CARTESIAN_POINT ( 'NONE',  ( 22.17183060077631040, -14.24070752338414358, 4.000000000000000000 ) ) ;
#31229 = CARTESIAN_POINT ( 'NONE',  ( 32.99999999999977263, -21.03360074219752107, 5.000000000000000000 ) ) ;
#31230 = CARTESIAN_POINT ( 'NONE',  ( -24.29974487139158867, -27.71228299555223273, 4.000000000000000000 ) ) ;
#31231 = ADVANCED_FACE ( 'NONE', ( #56411 ), #45520, .F. ) ;
#31232 = DIRECTION ( 'NONE',  ( 1.000000000000000000, 0.000000000000000000, 0.000000000000000000 ) ) ;
#31233 = DIRECTION ( 'NONE',  ( 0.7071067811865487940, -0.7071067811865463515, 0.000000000000000000 ) ) ;
#31234 = ORIENTED_EDGE ( 'NONE', *, *, #26639, .F. ) ;
#31235 = ORIENTED_EDGE ( 'NONE', *, *, #12518, .T. ) ;
#31236 = VERTEX_POINT ( 'NONE', #23731 ) ;
#31238 = EDGE_CURVE ( 'NONE', #35758, #98113, #68003, .T. ) ;
#31237 = CARTESIAN_POINT ( 'NONE',  ( 114.0208333333333144, 7.949999999999999289, 2.130196079827431532 ) ) ;
#31239 = EDGE_LOOP ( 'NONE', ( #5840, #125113, #91338, #128733 ) ) ;
#31240 = VECTOR ( 'NONE', #30114, 1000.000000000000000 ) ;
#31241 = ORIENTED_EDGE ( 'NONE', *, *, #60422, .T. ) ;
#31242 = VERTEX_POINT ( 'NONE', #100594 ) ;
#31243 = CARTESIAN_POINT ( 'NONE',  ( 20.51078643762690490, -27.52281430457041012, 5.000000000000000000 ) ) ;
#31244 = CARTESIAN_POINT ( 'NONE',  ( -21.18398860626899349, 28.73617430169802134, 5.000000000000000000 ) ) ;
#31245 = ORIENTED_EDGE ( 'NONE', *, *, #24979, .F. ) ;
#31246 = DIRECTION ( 'NONE',  ( -0.7071067811865486830, -0.7071067811865464625, -0.000000000000000000 ) ) ;
#31247 = EDGE_CURVE ( 'NONE', #82012, #52856, #112187, .T. ) ;
#31248 = CARTESIAN_POINT ( 'NONE',  ( 34.92499999999998295, -21.72500000000000142, 5.000000000000000000 ) ) ;
#31249 = CARTESIAN_POINT ( 'NONE',  ( 2.999999999999985345, -0.8619312979531966734, -5.102805207349819128 ) ) ;
#31250 = CARTESIAN_POINT ( 'NONE',  ( 104.4170968585647756, 3.054999999999998828, 5.291415217122922066 ) ) ;
#31251 = VERTEX_POINT ( 'NONE', #11380 ) ;
#31252 = DIRECTION ( 'NONE',  ( -0.7071067811865486830, -0.7071067811865464625, -0.000000000000000000 ) ) ;
#31253 = DIRECTION ( 'NONE',  ( 0.6830127018922181881, 0.6830127018922202975, -0.2588190451025214056 ) ) ;
#31254 = DIRECTION ( 'NONE',  ( -1.000000000000000000, -1.224606353822377258E-16, -0.000000000000000000 ) ) ;
#31255 = EDGE_CURVE ( 'NONE', #141655, #93537, #44067, .T. ) ;
#31256 = CARTESIAN_POINT ( 'NONE',  ( -32.99999999999977263, -13.06887692260767686, 4.000000000000000000 ) ) ;
#31257 = DIRECTION ( 'NONE',  ( -0.000000000000000000, -0.3543493200069152693, 0.9351131265310292928 ) ) ;
#31258 = CARTESIAN_POINT ( 'NONE',  ( 0.2262162651715141914, -0.5999999999999993117, -3.877538419241203904 ) ) ;
#31259 = CARTESIAN_POINT ( 'NONE',  ( 29.97502705046288796, -5.819803920172572198, 5.819803920172572198 ) ) ;
#31260 = VECTOR ( 'NONE', #92367, 1000.000000000000000 ) ;
#31261 = VECTOR ( 'NONE', #64875, 1000.000000000000000 ) ;
#31262 = ORIENTED_EDGE ( 'NONE', *, *, #115277, .T. ) ;
#31263 = ORIENTED_EDGE ( 'NONE', *, *, #83477, .F. ) ;
#31264 = AXIS2_PLACEMENT_3D ( 'NONE', #32692, #140026, #52274 ) ;
#31265 = CARTESIAN_POINT ( 'NONE',  ( 27.39583333333332149, -2.130196079827427091, 7.949999999999999289 ) ) ;
#31266 = ORIENTED_EDGE ( 'NONE', *, *, #2129, .T. ) ;
#31267 = DIRECTION ( 'NONE',  ( -1.000000000000000000, -1.224606353822377258E-16, -0.000000000000000000 ) ) ;
#31268 = ADVANCED_FACE ( 'NONE', ( #76717 ), #134661, .F. ) ;
#31269 = CARTESIAN_POINT ( 'NONE',  ( 0.000000000000000000, -9.500000000000000000, 4.000000000000000000 ) ) ;
#31270 = DIRECTION ( 'NONE',  ( 0.000000000000000000, -1.000000000000000000, 0.000000000000000000 ) ) ;
#31271 = DIRECTION ( 'NONE',  ( 0.7071067811865487940, 0.7071067811865463515, -0.000000000000000000 ) ) ;
#31272 = CARTESIAN_POINT ( 'NONE',  ( -0.4892135623730947680, -27.52281430457055578, 5.000000000000000000 ) ) ;
#31273 = ADVANCED_FACE ( 'NONE', ( #89698 ), #98437, .T. ) ;
#31274 = CARTESIAN_POINT ( 'NONE',  ( 123.7245968585647660, -1.637169565754160949, 6.109999999999997655 ) ) ;
#31275 = ORIENTED_EDGE ( 'NONE', *, *, #60532, .T. ) ;
#31276 = EDGE_CURVE ( 'NONE', #24394, #135463, #123055, .T. ) ;
#31277 = CARTESIAN_POINT ( 'NONE',  ( 69.18398860626899705, 28.73617430169835529, 5.000000000000000000 ) ) ;
#31278 = ORIENTED_EDGE ( 'NONE', *, *, #50510, .F. ) ;
#31279 = DIRECTION ( 'NONE',  ( -0.7071067811865486830, -0.7071067811865464625, 0.000000000000000000 ) ) ;
#31280 = DIRECTION ( 'NONE',  ( -0.000000000000000000, -0.3543493200069152693, 0.9351131265310292928 ) ) ;
#31282 = ADVANCED_FACE ( 'NONE', ( #43351 ), #87563, .F. ) ;
#31281 = CARTESIAN_POINT ( 'NONE',  ( 13.29826936130429260, 3.061616997868383634E-16, -2.500000000000000444 ) ) ;
#31283 = EDGE_CURVE ( 'NONE', #56496, #39354, #143361, .T. ) ;
#31284 = LINE ( 'NONE', #74807, #95069 ) ;
#31285 = ORIENTED_EDGE ( 'NONE', *, *, #103521, .T. ) ;
#31286 = CARTESIAN_POINT ( 'NONE',  ( 47.83376352523143993, 6.110000000000001208, 1.122388791418549305E-15 ) ) ;
#31287 = ORIENTED_EDGE ( 'NONE', *, *, #63632, .T. ) ;
#31288 = LINE ( 'NONE', #129872, #19296 ) ;
#31289 = CARTESIAN_POINT ( 'NONE',  ( -34.92500000000001137, -22.22500000000000142, 4.000000000000000000 ) ) ;
#31290 = DIRECTION ( 'NONE',  ( -0.7071067811865486830, -0.7071067811865464625, -0.000000000000000000 ) ) ;
#31291 = DIRECTION ( 'NONE',  ( 0.000000000000000000, 0.000000000000000000, -1.000000000000000000 ) ) ;
#31292 = CARTESIAN_POINT ( 'NONE',  ( 35.93293019189811588, 1.637169565754156508, 6.110000000000000320 ) ) ;
#31293 = ORIENTED_EDGE ( 'NONE', *, *, #80129, .T. ) ;
#31294 = ADVANCED_FACE ( 'NONE', ( #71537 ), #21437, .T. ) ;
#31295 = DIRECTION ( 'NONE',  ( 0.000000000000000000, 0.000000000000000000, -1.000000000000000000 ) ) ;
#31296 = ORIENTED_EDGE ( 'NONE', *, *, #110303, .F. ) ;
#31297 = ORIENTED_EDGE ( 'NONE', *, *, #53998, .T. ) ;
#31298 = ORIENTED_EDGE ( 'NONE', *, *, #35385, .T. ) ;
#31299 = DIRECTION ( 'NONE',  ( -0.6830127018922180770, -0.6830127018922204085, -0.2588190451025213501 ) ) ;
#31300 = ORIENTED_EDGE ( 'NONE', *, *, #17370, .F. ) ;
#31301 = LINE ( 'NONE', #100122, #55341 ) ;
#31302 = LINE ( 'NONE', #47224, #128863 ) ;
#31303 = DIRECTION ( 'NONE',  ( -1.000000000000000000, 0.000000000000000000, 0.000000000000000000 ) ) ;
#31304 = DIRECTION ( 'NONE',  ( -0.7071067811865486830, 0.7071067811865464625, 0.000000000000000000 ) ) ;
#31305 = FACE_BOUND ( 'NONE', #15595, .T. ) ;
#31306 = ORIENTED_EDGE ( 'NONE', *, *, #44972, .F. ) ;
#31307 =( LENGTH_UNIT ( ) NAMED_UNIT ( * ) SI_UNIT ( .MILLI., .METRE. ) );
#31308 = CARTESIAN_POINT ( 'NONE',  ( -23.70025512860841133, -27.71228299555189523, 4.000000000000000000 ) ) ;
#31309 = CARTESIAN_POINT ( 'NONE',  ( -34.42500000000001137, -21.72500000000000142, 0.4999999999999995559 ) ) ;
#31310 = VERTEX_POINT ( 'NONE', #14982 ) ;
#31311 = DIRECTION ( 'NONE',  ( 0.6830127018922181881, 0.6830127018922202975, -0.2588190451025214056 ) ) ;
#31312 = ORIENTED_EDGE ( 'NONE', *, *, #81716, .T. ) ;
#31313 = ORIENTED_EDGE ( 'NONE', *, *, #45875, .F. ) ;
#31314 = DIRECTION ( 'NONE',  ( -1.000000000000000000, 0.000000000000000000, 0.000000000000000000 ) ) ;
#31315 = ORIENTED_EDGE ( 'NONE', *, *, #128570, .T. ) ;
#31316 = AXIS2_PLACEMENT_3D ( 'NONE', #73858, #130392, #96279 ) ;
#31317 = CARTESIAN_POINT ( 'NONE',  ( 54.16209685856478018, -5.291415217122919401, 3.054999999999997939 ) ) ;
#31318 = ORIENTED_EDGE ( 'NONE', *, *, #84969, .T. ) ;
#31319 = DIRECTION ( 'NONE',  ( 0.7071067811865486830, -0.7071067811865464625, -0.000000000000000000 ) ) ;
#31320 = ORIENTED_EDGE ( 'NONE', *, *, #30960, .T. ) ;
#31321 = VECTOR ( 'NONE', #34633, 1000.000000000000000 ) ;
#31322 = DIRECTION ( 'NONE',  ( -0.000000000000000000, 0.000000000000000000, 1.000000000000000000 ) ) ;
#31323 = ORIENTED_EDGE ( 'NONE', *, *, #42, .T. ) ;
#31324 =( NAMED_UNIT ( * ) SI_UNIT ( $, .STERADIAN. ) SOLID_ANGLE_UNIT ( ) );
#31325 = DIRECTION ( 'NONE',  ( -0.6830127018922181881, 0.6830127018922202975, -0.2588190451025214056 ) ) ;
#31326 = ADVANCED_FACE ( 'NONE', ( #91158 ), #25143, .F. ) ;
#31327 = EDGE_CURVE ( 'NONE', #6816, #100625, #36741, .T. ) ;
#31328 = FACE_OUTER_BOUND ( 'NONE', #142482, .T. ) ;
#31329 = VECTOR ( 'NONE', #42106, 1000.000000000000000 ) ;
#31330 = CARTESIAN_POINT ( 'NONE',  ( 24.29974487139158867, -27.71228299555223273, 4.000000000000000000 ) ) ;
#31331 = CARTESIAN_POINT ( 'NONE',  ( -3.489213562373097322, -27.52281430457057709, 5.000000000000000000 ) ) ;
#31332 = FACE_OUTER_BOUND ( 'NONE', #117730, .T. ) ;
#31333 = ORIENTED_EDGE ( 'NONE', *, *, #131492, .F. ) ;
#31334 = ORIENTED_EDGE ( 'NONE', *, *, #21381, .F. ) ;
#31335 = ORIENTED_EDGE ( 'NONE', *, *, #90529, .T. ) ;
#31336 = CARTESIAN_POINT ( 'NONE',  ( 19.00413961620377279, -3.047499999999994547, 5.278424836066145431 ) ) ;
#31337 = PLANE ( 'NONE',  #99909 ) ;
#31338 = ORIENTED_EDGE ( 'NONE', *, *, #17825, .F. ) ;
#31339 = ORIENTED_EDGE ( 'NONE', *, *, #80533, .T. ) ;
#31340 = VERTEX_POINT ( 'NONE', #138211 ) ;
#31341 = CARTESIAN_POINT ( 'NONE',  ( -26.67183060077628198, -21.74070752338406010, 4.000000000000000000 ) ) ;
#31342 = CARTESIAN_POINT ( 'NONE',  ( -3.328169399223505742, 11.25929247661559707, 4.000000000000000000 ) ) ;
#31343 = EDGE_CURVE ( 'NONE', #84739, #66605, #4057, .T. ) ;
#31344 = LINE ( 'NONE', #8805, #90183 ) ;
#31345 = EDGE_LOOP ( 'NONE', ( #90755, #38748, #129004, #89095 ) ) ;
#31346 = CARTESIAN_POINT ( 'NONE',  ( 14.81601139373099585, 28.73617430169776910, 5.000000000000000000 ) ) ;
#31347 = VECTOR ( 'NONE', #67472, 1000.000000000000000 ) ;
#31348 = CARTESIAN_POINT ( 'NONE',  ( -15.79076468313838433, 8.175634574663693144, 5.000000000000000000 ) ) ;
#31349 = VECTOR ( 'NONE', #111948, 1000.000000000000227 ) ;
#31351 = CARTESIAN_POINT ( 'NONE',  ( 18.58790314143521982, 6.871911579029515771, 3.967499999999989146 ) ) ;
#31350 = B_SPLINE_CURVE_WITH_KNOTS ( 'NONE', 3,
 ( #89717, #136791, #14999, #25893 ),
 .UNSPECIFIED., .F., .F.,
 ( 4, 4 ),
 ( 0.003615568590623256459, 0.004164643302645746996 ),
 .UNSPECIFIED. ) ;
#31352 = AXIS2_PLACEMENT_3D ( 'NONE', #123976, #45024, #88499 ) ;
#31353 = CYLINDRICAL_SURFACE ( 'NONE', #60043, 7.950000000000000178 ) ;
#31354 = ORIENTED_EDGE ( 'NONE', *, *, #46441, .T. ) ;
#31355 = CARTESIAN_POINT ( 'NONE',  ( 118.9120968585647802, 5.291415217122922066, -3.054999999999995275 ) ) ;
#31356 = DIRECTION ( 'NONE',  ( 0.6830127018922180770, -0.6830127018922204085, -0.2588190451025213501 ) ) ;
#31357 = DIRECTION ( 'NONE',  ( -0.000000000000000000, -0.3543493200069153248, -0.9351131265310291818 ) ) ;
#31359 = VERTEX_POINT ( 'NONE', #92532 ) ;
#31358 = CARTESIAN_POINT ( 'NONE',  ( 28.49999999999980460, 13.08746187583912146, 4.000000000000000000 ) ) ;
#31360 = CARTESIAN_POINT ( 'NONE',  ( 67.74586038379622721, 3.974999999999996980, 6.884901960086287964 ) ) ;
#31361 = EDGE_LOOP ( 'NONE', ( #86868, #49523, #41157, #11995 ) ) ;
#31362 = CARTESIAN_POINT ( 'NONE',  ( 0.4892135623730947680, -27.52281430457055578, 5.000000000000000000 ) ) ;
#31363 = DIRECTION ( 'NONE',  ( 0.5735764363510453823, -0.8191520442889923537, 1.003171929053525486E-16 ) ) ;
#31364 = DIRECTION ( 'NONE',  ( 0.6830127018922181881, 0.6830127018922202975, -0.2588190451025214056 ) ) ;
#31365 = VERTEX_POINT ( 'NONE', #60694 ) ;
#31366 = CARTESIAN_POINT ( 'NONE',  ( -25.39999999999996305, 0.000000000000000000, 0.000000000000000000 ) ) ;
#31367 = DIRECTION ( 'NONE',  ( 0.7071067811865486830, -0.7071067811865464625, -0.000000000000000000 ) ) ;
#31368 = EDGE_LOOP ( 'NONE', ( #114126, #134418, #69377, #7732 ) ) ;
#31369 = DIRECTION ( 'NONE',  ( 1.000000000000000000, 0.000000000000000000, 0.000000000000000000 ) ) ;
#31370 = DIRECTION ( 'NONE',  ( -0.000000000000000000, 0.3543493200069153248, 0.9351131265310292928 ) ) ;
#31371 = VERTEX_POINT ( 'NONE', #83118 ) ;
#31372 = LINE ( 'NONE', #75597, #123579 ) ;
#31373 = DIRECTION ( 'NONE',  ( -1.000000000000000000, 0.000000000000000000, -0.000000000000000000 ) ) ;
#31374 = ORIENTED_EDGE ( 'NONE', *, *, #143083, .T. ) ;
#31375 = EDGE_CURVE ( 'NONE', #126278, #137809, #48342, .T. ) ;
#31376 = ORIENTED_EDGE ( 'NONE', *, *, #111669, .F. ) ;
#31377 = FACE_OUTER_BOUND ( 'NONE', #105668, .T. ) ;
#31378 = CARTESIAN_POINT ( 'NONE',  ( 125.5000000000000000, 0.000000000000000000, 0.000000000000000000 ) ) ;
#31379 = EDGE_CURVE ( 'NONE', #88226, #878, #136768, .T. ) ;
#31380 = EDGE_CURVE ( 'NONE', #50767, #126713, #70143, .T. ) ;
#31381 = CARTESIAN_POINT ( 'NONE',  ( 39.48921356237310221, -27.52281430457082934, 5.000000000000000000 ) ) ;
#31382 = DIRECTION ( 'NONE',  ( 0.000000000000000000, 0.000000000000000000, -1.000000000000000000 ) ) ;
#31383 = EDGE_CURVE ( 'NONE', #36965, #68527, #127319, .T. ) ;
#31384 = VERTEX_POINT ( 'NONE', #16393 ) ;
#31385 = DIRECTION ( 'NONE',  ( 0.000000000000000000, 0.000000000000000000, 1.000000000000000000 ) ) ;
#31386 = ADVANCED_FACE ( 'NONE', ( #38897 ), #38199, .F. ) ;
#31387 = DIRECTION ( 'NONE',  ( -0.6830127018922180770, -0.6830127018922202975, -0.2588190451025213501 ) ) ;
#31388 = CARTESIAN_POINT ( 'NONE',  ( 5.587472949537105826, -6.094999999999989981, 3.732111120401553285E-16 ) ) ;
#31389 = CARTESIAN_POINT ( 'NONE',  ( 126.6604541630265999, -6.146688740034715437, -2.899546345087764543 ) ) ;
#31390 = ADVANCED_FACE ( 'NONE', ( #36059 ), #80981, .F. ) ;
#31391 = CARTESIAN_POINT ( 'NONE',  ( 40.01626352523144448, -4.472830434245839371, 4.472830434245839371 ) ) ;
#31392 = LINE ( 'NONE', #106786, #78871 ) ;
#31393 = ORIENTED_EDGE ( 'NONE', *, *, #23006, .F. ) ;
#31394 = ORIENTED_EDGE ( 'NONE', *, *, #140645, .F. ) ;
#31396 = EDGE_CURVE ( 'NONE', #89130, #35044, #16680, .T. ) ;
#31395 = SURFACE_SIDE_STYLE ('',( #140841 ) ) ;
#31397 = ORIENTED_EDGE ( 'NONE', *, *, #63475, .F. ) ;
#31398 = EDGE_CURVE ( 'NONE', #11989, #93367, #134885, .T. ) ;
#31399 = ORIENTED_EDGE ( 'NONE', *, *, #136704, .F. ) ;
#31400 = PLANE ( 'NONE',  #117355 ) ;
#31401 = DIRECTION ( 'NONE',  ( -0.3543493200069162685, -0.000000000000000000, -0.9351131265310288487 ) ) ;
#31402 = ORIENTED_EDGE ( 'NONE', *, *, #80290, .T. ) ;
#31403 =( BOUNDED_CURVE ( )  B_SPLINE_CURVE ( 2, ( #79183, #80590, #841, #56726, #46567, #21898, #100887, #1540, #99438, #90754, #45129, #35682, #89307 ),
 .UNSPECIFIED., .F., .T. ) 
 B_SPLINE_CURVE_WITH_KNOTS ( ( 3, 2, 2, 2, 2, 2, 3 ),
 ( 0.05000000000000004441, 0.05277777777777781926, 0.05555555555555560104, 0.05833333333333338283, 0.06111111111111115768, 0.06388888888888893947, 0.06666666666666672125 ),
 .UNSPECIFIED. ) 
 CURVE ( )  GEOMETRIC_REPRESENTATION_ITEM ( )  RATIONAL_B_SPLINE_CURVE ( ( 0.9999999999999994449, 0.9659258262890688673, 1.000000000000000000, 0.9659258262890683122, 1.000000000000000000, 0.9659258262890683122, 1.000000000000000000, 0.9659258262890683122, 1.000000000000000000, 0.9659258262890683122, 1.000000000000000000, 0.9659258262890676461, 1.000000000000000666 ) ) 
 REPRESENTATION_ITEM ( '' )  );
#31404 = DIRECTION ( 'NONE',  ( -0.7071067811865486830, -0.7071067811865464625, -0.000000000000000000 ) ) ;
#31405 = LINE ( 'NONE', #9616, #141519 ) ;
#31406 = EDGE_CURVE ( 'NONE', #90585, #87703, #5523, .T. ) ;
#31407 = DIRECTION ( 'NONE',  ( -0.3543493200069162685, -0.000000000000000000, -0.9351131265310288487 ) ) ;
#31408 = ADVANCED_FACE ( 'NONE', ( #136058 ), #28022, .F. ) ;
#31409 = DIRECTION ( 'NONE',  ( 1.000000000000000000, 0.000000000000000000, 0.000000000000000000 ) ) ;
#31410 = FACE_OUTER_BOUND ( 'NONE', #33600, .T. ) ;
#31411 = ORIENTED_EDGE ( 'NONE', *, *, #98008, .T. ) ;
#31412 = LINE ( 'NONE', #98780, #125204 ) ;
#31413 = DIRECTION ( 'NONE',  ( -0.6830127018922180770, -0.6830127018922204085, -0.2588190451025213501 ) ) ;
#31414 = CARTESIAN_POINT ( 'NONE',  ( 79.31250000000000000, 5.819803920172571310, 5.819803920172576639 ) ) ;
#31415 = PLANE ( 'NONE',  #71071 ) ;
#31416 = CARTESIAN_POINT ( 'NONE',  ( 20.20710678118640402, -17.24070752338410628, 5.000000000000000000 ) ) ;
#31417 = ADVANCED_FACE ( 'NONE', ( #13539 ), #2671, .F. ) ;
#31418 = CARTESIAN_POINT ( 'NONE',  ( 153.4000000000000057, -1.600000000000086020, -33.92499999999998295 ) ) ;
#31419 = LINE ( 'NONE', #43014, #13382 ) ;
#31420 = CARTESIAN_POINT ( 'NONE',  ( 52.28752705046288440, 0.000000000000000000, -7.949999999999998401 ) ) ;
#31421 = AXIS2_PLACEMENT_3D ( 'NONE', #123994, #70363, #47884 ) ;
#31422 = CYLINDRICAL_SURFACE ( 'NONE', #103955, 2.500000000000000444 ) ;
#31423 = ORIENTED_EDGE ( 'NONE', *, *, #56638, .T. ) ;
#31424 = ORIENTED_EDGE ( 'NONE', *, *, #104853, .F. ) ;
#31425 = CARTESIAN_POINT ( 'NONE',  ( 53.35416666666666430, -2.130196079827425315, -7.950000000000001066 ) ) ;
#31426 = DIRECTION ( 'NONE',  ( -1.000000000000000000, -1.224606353822377258E-16, -0.000000000000000000 ) ) ;
#31427 = VECTOR ( 'NONE', #141829, 1000.000000000000000 ) ;
#31428 = CARTESIAN_POINT ( 'NONE',  ( -0.4892135623730947680, -27.52281430457055578, 5.000000000000000000 ) ) ;
#31429 = FACE_OUTER_BOUND ( 'NONE', #82038, .T. ) ;
#31430 = ORIENTED_EDGE ( 'NONE', *, *, #67597, .T. ) ;
#31431 = CARTESIAN_POINT ( 'NONE',  ( 0.4892135623730947680, -27.52281430457055578, 5.000000000000000000 ) ) ;
#31432 = CARTESIAN_POINT ( 'NONE',  ( 13.22578070446010301, 4.485909045323550615, 4.327832195654622183 ) ) ;
#31433 = CARTESIAN_POINT ( 'NONE',  ( 43.16709685856477563, -3.055000000000000160, -5.291415217122921177 ) ) ;
#31434 = ORIENTED_EDGE ( 'NONE', *, *, #1438, .T. ) ;
#31435 = EDGE_CURVE ( 'NONE', #91561, #128706, #29430, .T. ) ;
#31436 = CARTESIAN_POINT ( 'NONE',  ( -69.18398860626899705, 28.73617430169835529, 5.000000000000000000 ) ) ;
#31437 = ORIENTED_EDGE ( 'NONE', *, *, #91541, .T. ) ;
#31438 = ORIENTED_EDGE ( 'NONE', *, *, #61794, .T. ) ;
#31439 = DIRECTION ( 'NONE',  ( -0.7071067811865486830, -0.7071067811865464625, -0.000000000000000000 ) ) ;
#31440 = DIRECTION ( 'NONE',  ( 0.7071067811865486830, -0.7071067811865464625, -0.000000000000000000 ) ) ;
#31441 = CARTESIAN_POINT ( 'NONE',  ( -34.92500000000001137, 11.07784511950552897, 0.7759263132492092430 ) ) ;
#31442 = DIRECTION ( 'NONE',  ( -0.7071067811865486830, -0.7071067811865464625, 0.000000000000000000 ) ) ;
#31443 = ORIENTED_EDGE ( 'NONE', *, *, #27144, .F. ) ;
#31444 = CARTESIAN_POINT ( 'NONE',  ( 18.98155265364318822, 18.75929247661551713, 20.33588619593438551 ) ) ;
#31446 = ORIENTED_EDGE ( 'NONE', *, *, #137756, .T. ) ;
#31445 = CARTESIAN_POINT ( 'NONE',  ( -12.20000000000000284, -39.92999999999999261, 19.45086547876359617 ) ) ;
#31447 = CARTESIAN_POINT ( 'NONE',  ( 81.37543019189810423, -5.291415217122920289, -3.055000000000001492 ) ) ;
#31448 = DIRECTION ( 'NONE',  ( -0.3543493200069162685, -0.000000000000000000, -0.9351131265310288487 ) ) ;
#31449 = DIRECTION ( 'NONE',  ( 0.7071067811865486830, -0.7071067811865464625, -0.000000000000000000 ) ) ;
#31450 = LINE ( 'NONE', #64797, #74874 ) ;
#31451 = CARTESIAN_POINT ( 'NONE',  ( 30.32816939922332011, 8.259292476615630818, 4.000000000000000000 ) ) ;
#31452 =( NAMED_UNIT ( * ) PLANE_ANGLE_UNIT ( ) SI_UNIT ( $, .RADIAN. ) );
#31453 = EDGE_CURVE ( 'NONE', #117034, #3157, #19284, .T. ) ;
#31454 = AXIS2_PLACEMENT_3D ( 'NONE', #1096, #45380, #89554 ) ;
#31455 = VECTOR ( 'NONE', #86544, 1000.000000000000000 ) ;
#31456 = ORIENTED_EDGE ( 'NONE', *, *, #49280, .T. ) ;
#31457 = DIRECTION ( 'NONE',  ( -0.000000000000000000, 0.000000000000000000, 1.000000000000000000 ) ) ;
#31458 = CARTESIAN_POINT ( 'NONE',  ( 70.20376352523143737, 6.109999999999998543, 1.122388791418548911E-15 ) ) ;
#31459 = CARTESIAN_POINT ( 'NONE',  ( 0.000000000000000000, 0.000000000000000000, 5.000000000000000000 ) ) ;
#31460 = EDGE_CURVE ( 'NONE', #53079, #119580, #83863, .T. ) ;
#31461 = DIRECTION ( 'NONE',  ( 1.000000000000000000, 1.224606353822377258E-16, 0.000000000000000000 ) ) ;
#31462 = CARTESIAN_POINT ( 'NONE',  ( -18.48921356237309510, -27.52281430457068367, 5.000000000000000000 ) ) ;
#31463 = EDGE_LOOP ( 'NONE', ( #21275, #26737, #73452, #129064 ) ) ;
#31464 = VERTEX_POINT ( 'NONE', #108386 ) ;
#31465 = MECHANICAL_DESIGN_GEOMETRIC_PRESENTATION_REPRESENTATION (  '', ( #12908 ), #123987 ) ;
#31466 = DIRECTION ( 'NONE',  ( -0.7071067811865487940, 0.7071067811865463515, -0.000000000000000000 ) ) ;
#31467 = CARTESIAN_POINT ( 'NONE',  ( -6.812461875839420422, -22.22500000000000142, 4.000000000000000000 ) ) ;
#31468 = VERTEX_POINT ( 'NONE', #117846 ) ;
#31469 = VERTEX_POINT ( 'NONE', #42496 ) ;
#31470 = EDGE_CURVE ( 'NONE', #91708, #75295, #119295, .T. ) ;
#31471 = DIRECTION ( 'NONE',  ( 1.000000000000000000, 0.000000000000000000, 0.000000000000000000 ) ) ;
#31472 = VERTEX_POINT ( 'NONE', #85970 ) ;
#31473 = DIRECTION ( 'NONE',  ( 0.3543493200069163240, 0.000000000000000000, 0.9351131265310288487 ) ) ;
#31474 = CARTESIAN_POINT ( 'NONE',  ( 1.030267906253082177, 0.5999999999999988676, 4.508336184329993834 ) ) ;
#31475 = PLANE ( 'NONE',  #48945 ) ;
#31476 = EDGE_CURVE ( 'NONE', #105871, #24821, #128068, .T. ) ;
#31477 = FACE_BOUND ( 'NONE', #137789, .T. ) ;
#31478 = LINE ( 'NONE', #109006, #138210 ) ;
#31479 = LINE ( 'NONE', #19165, #120685 ) ;
#31480 = LINE ( 'NONE', #107594, #36414 ) ;
#31482 = ORIENTED_EDGE ( 'NONE', *, *, #77391, .T. ) ;
#31481 = CARTESIAN_POINT ( 'NONE',  ( 50.82919371712955581, -3.975000000000001865, 6.884901960086284411 ) ) ;
#31483 = DIRECTION ( 'NONE',  ( -0.000000000000000000, -0.3543493200069152693, 0.9351131265310292928 ) ) ;
#31484 = ITEM_DEFINED_TRANSFORMATION ( 'NONE', 'NONE', #137283,  #127880 ) ;
#31485 = ORIENTED_EDGE ( 'NONE', *, *, #124808, .F. ) ;
#31486 = EDGE_LOOP ( 'NONE', ( #6829, #73942, #82691, #12660 ) ) ;
#31487 = CARTESIAN_POINT ( 'NONE',  ( 86.24543019189812298, -5.291415217122918513, -3.055000000000000160 ) ) ;
#31488 = VERTEX_POINT ( 'NONE', #53327 ) ;
#31489 = CARTESIAN_POINT ( 'NONE',  ( -14.99999999999989875, -4.447814304570775867, 5.000000000000000000 ) ) ;
#31490 = DIRECTION ( 'NONE',  ( -0.7071067811865486830, -0.7071067811865464625, 0.000000000000000000 ) ) ;
#31491 = ORIENTED_EDGE ( 'NONE', *, *, #89506, .T. ) ;
#31492 = DIRECTION ( 'NONE',  ( 0.7071067811865487940, 0.7071067811865463515, -0.000000000000000000 ) ) ;
#31493 = DIRECTION ( 'NONE',  ( -1.000000000000000000, 0.000000000000000000, 0.000000000000000000 ) ) ;
#31494 = CARTESIAN_POINT ( 'NONE',  ( -8.749659869322266218E-15, -4.870000000000014317, -4.276802603762487998 ) ) ;
#31495 = EDGE_CURVE ( 'NONE', #14271, #107195, #107707, .T. ) ;
#31496 = CARTESIAN_POINT ( 'NONE',  ( -27.79289321881325492, 18.75929247661552068, 5.000000000000000000 ) ) ;
#31497 = LINE ( 'NONE', #120612, #6407 ) ;
#31498 = DIRECTION ( 'NONE',  ( 0.3543493200069162685, -0.000000000000000000, -0.9351131265310288487 ) ) ;
#31499 = CARTESIAN_POINT ( 'NONE',  ( 24.48921356237309510, -27.52281430457072631, 5.000000000000000000 ) ) ;
#31500 = CARTESIAN_POINT ( 'NONE',  ( 12.18398860626900060, 28.73617430169795739, 5.000000000000000000 ) ) ;
#31501 = ORIENTED_EDGE ( 'NONE', *, *, #138147, .T. ) ;
#31502 = CARTESIAN_POINT ( 'NONE',  ( 34.49999999999976552, -10.91253812416064584, 4.000000000000000000 ) ) ;
#31503 = ORIENTED_EDGE ( 'NONE', *, *, #88518, .F. ) ;
#31504 = CARTESIAN_POINT ( 'NONE',  ( 122.4333603837967530, 2.130196079833805989, -7.949999999996317790 ) ) ;
#31505 = FACE_OUTER_BOUND ( 'NONE', #19792, .T. ) ;
#31506 = ORIENTED_EDGE ( 'NONE', *, *, #19855, .T. ) ;
#31507 = ORIENTED_EDGE ( 'NONE', *, *, #112468, .F. ) ;
#31508 = ADVANCED_FACE ( 'NONE', ( #9069 ), #30895, .F. ) ;
#31509 = ORIENTED_EDGE ( 'NONE', *, *, #31476, .F. ) ;
#31510 = CARTESIAN_POINT ( 'NONE',  ( 35.87543019189811133, -5.291415217122920289, -3.055000000000001492 ) ) ;
#31511 = ORIENTED_EDGE ( 'NONE', *, *, #112131, .F. ) ;
#31512 = DIRECTION ( 'NONE',  ( 0.7071067811865487940, 0.7071067811865463515, -0.000000000000000000 ) ) ;
#31513 = CIRCLE ( 'NONE', #24567, 2.055000000000001048 ) ;
#31514 = DIRECTION ( 'NONE',  ( -0.7071067811865486830, -0.7071067811865464625, 0.000000000000000000 ) ) ;
#31515 = CARTESIAN_POINT ( 'NONE',  ( 24.98330628287043709, 6.094999999999991758, 1.633150327867687102 ) ) ;
#31516 =( BOUNDED_CURVE ( )  B_SPLINE_CURVE ( 3, ( #36761, #125937, #104135, #92555 ),
 .UNSPECIFIED., .F., .T. ) 
 B_SPLINE_CURVE_WITH_KNOTS ( ( 4, 4 ),
 ( 5.143245962375977420, 6.645403452391244414 ),
 .UNSPECIFIED. ) 
 CURVE ( )  GEOMETRIC_REPRESENTATION_ITEM ( )  RATIONAL_B_SPLINE_CURVE ( ( 1.000000000000000000, 0.8206354192515272761, 0.8206354192515272761, 1.000000000000000000 ) ) 
 REPRESENTATION_ITEM ( '' )  );
#31517 = CARTESIAN_POINT ( 'NONE',  ( 1.043401249077450688, 13.72784592288353345, -24.38207966554766060 ) ) ;
#31518 = ORIENTED_EDGE ( 'NONE', *, *, #109343, .T. ) ;
#31519 = AXIS2_PLACEMENT_3D ( 'NONE', #18393, #76397, #29297 ) ;
#31520 = DIRECTION ( 'NONE',  ( 0.000000000000000000, -1.000000000000000000, 0.000000000000000000 ) ) ;
#31521 = EDGE_LOOP ( 'NONE', ( #89807, #86270, #71657, #128982 ) ) ;
#31522 = SURFACE_SIDE_STYLE ('',( #87333 ) ) ;
#31523 = LINE ( 'NONE', #20621, #31261 ) ;
#31525 = VERTEX_POINT ( 'NONE', #72996 ) ;
#31524 = CARTESIAN_POINT ( 'NONE',  ( 54.48921356237310221, -27.52281430457093236, 5.000000000000000000 ) ) ;
#31526 = VERTEX_POINT ( 'NONE', #40351 ) ;
#31528 = EDGE_CURVE ( 'NONE', #85826, #98772, #50491, .T. ) ;
#31527 = CARTESIAN_POINT ( 'NONE',  ( 2.700255128608413990, -27.71228299555204089, 4.000000000000000000 ) ) ;
#31529 = LINE ( 'NONE', #62033, #70043 ) ;
#31530 = DIRECTION ( 'NONE',  ( 0.7071067811865486830, -0.7071067811865464625, -0.000000000000000000 ) ) ;
#31531 = ORIENTED_EDGE ( 'NONE', *, *, #132767, .T. ) ;
#31532 = CARTESIAN_POINT ( 'NONE',  ( 109.0166937171295416, 7.950000000000000178, -2.130196079827421318 ) ) ;
#31533 = ORIENTED_EDGE ( 'NONE', *, *, #79005, .F. ) ;
#31534 = ORIENTED_EDGE ( 'NONE', *, *, #99759, .F. ) ;
#31535 = ORIENTED_EDGE ( 'NONE', *, *, #2100, .T. ) ;
#31536 = PRESENTATION_LAYER_ASSIGNMENT (  '', '', ( #38462 ) ) ;
#31537 = CARTESIAN_POINT ( 'NONE',  ( -34.92500000000001137, -20.24070752338407786, 4.255531930566252896 ) ) ;
#31538 = CARTESIAN_POINT ( 'NONE',  ( 34.92499999999998295, 11.71849043720414052, 4.759050581649325373 ) ) ;
#31539 = CARTESIAN_POINT ( 'NONE',  ( 10.06000000000000050, 9.521314400968980422E-16, 0.000000000000000000 ) ) ;
#31540 = LINE ( 'NONE', #98911, #116397 ) ;
#31541 = CARTESIAN_POINT ( 'NONE',  ( 45.48921356237309510, -27.52281430457087197, 5.000000000000000000 ) ) ;
#31542 = LINE ( 'NONE', #85911, #104910 ) ;
#31543 = VECTOR ( 'NONE', #18570, 999.9999999999998863 ) ;
#31544 = DIRECTION ( 'NONE',  ( 0.000000000000000000, -1.000000000000000000, 0.000000000000000000 ) ) ;
#31545 = VERTEX_POINT ( 'NONE', #41037 ) ;
#31546 = DIRECTION ( 'NONE',  ( 1.318980745116185161E-16, -1.000000000000000000, 0.000000000000000000 ) ) ;
#31547 = VERTEX_POINT ( 'NONE', #51211 ) ;
#31548 = CARTESIAN_POINT ( 'NONE',  ( 25.39999999999999858, 7.464222240803104598E-16, -6.094999999999989093 ) ) ;
#31549 = AXIS2_PLACEMENT_3D ( 'NONE', #36594, #80846, #126452 ) ;
#31550 = VECTOR ( 'NONE', #101697, 1000.000000000000114 ) ;
#31551 = LINE ( 'NONE', #10484, #127175 ) ;
#31553 = EDGE_CURVE ( 'NONE', #69963, #98666, #105553, .T. ) ;
#31552 = VECTOR ( 'NONE', #101470, 1000.000000000000000 ) ;
#31554 = ORIENTED_EDGE ( 'NONE', *, *, #120691, .T. ) ;
#31555 = LINE ( 'NONE', #88076, #59997 ) ;
#31556 = CARTESIAN_POINT ( 'NONE',  ( 0.000000000000000000, 0.000000000000000000, 7.950000000000000178 ) ) ;
#31557 = ORIENTED_EDGE ( 'NONE', *, *, #86218, .T. ) ;
#31558 = EDGE_CURVE ( 'NONE', #77143, #3030, #84561, .T. ) ;
#31559 = ORIENTED_EDGE ( 'NONE', *, *, #59723, .T. ) ;
#31560 = FACE_OUTER_BOUND ( 'NONE', #121639, .T. ) ;
#31561 = LINE ( 'NONE', #18498, #60416 ) ;
#31562 = EDGE_CURVE ( 'NONE', #14666, #47923, #6217, .T. ) ;
#31563 = DIRECTION ( 'NONE',  ( -0.7071067811865486830, -0.7071067811865464625, -0.000000000000000000 ) ) ;
#31564 = AXIS2_PLACEMENT_3D ( 'NONE', #8691, #116070, #118930 ) ;
#31565 = LINE ( 'NONE', #22090, #78366 ) ;
#31566 = ADVANCED_FACE ( 'NONE', ( #86702 ), #39637, .F. ) ;
#31567 = CARTESIAN_POINT ( 'NONE',  ( 63.78709685856477307, 3.054999999999997939, 5.291415217122920289 ) ) ;
#31568 = CARTESIAN_POINT ( 'NONE',  ( -1.734723475976807094E-15, 13.93112307739203715, 4.000000000000000000 ) ) ;
#31569 = CARTESIAN_POINT ( 'NONE',  ( 0.4892135623730947680, -27.52281430457055578, 5.000000000000000000 ) ) ;
#31570 = CARTESIAN_POINT ( 'NONE',  ( -13.71003237941630104, 5.842153316012715258, 5.000000000000000000 ) ) ;
#31571 = DIRECTION ( 'NONE',  ( 0.3543493200069162685, -0.000000000000000000, -0.9351131265310288487 ) ) ;
#31572 = VERTEX_POINT ( 'NONE', #106993 ) ;
#31573 = LINE ( 'NONE', #108362, #2422 ) ;
#31574 = ORIENTED_EDGE ( 'NONE', *, *, #122229, .F. ) ;
#31575 = DIRECTION ( 'NONE',  ( -0.6830127018922180770, -0.6830127018922204085, -0.2588190451025213501 ) ) ;
#31576 = PLANE ( 'NONE',  #10530 ) ;
#31577 = ORIENTED_EDGE ( 'NONE', *, *, #49407, .T. ) ;
#31578 = CARTESIAN_POINT ( 'NONE',  ( 184.1500000000000057, -43.14999999999999147, 31.92499999999998295 ) ) ;
#31580 = ORIENTED_EDGE ( 'NONE', *, *, #126471, .T. ) ;
#31579 = CARTESIAN_POINT ( 'NONE',  ( 39.18398860626899705, 28.73617430169814568, 5.000000000000000000 ) ) ;
#31581 = EDGE_CURVE ( 'NONE', #87749, #12285, #96113, .T. ) ;
#31582 = DIRECTION ( 'NONE',  ( -0.7071067811865486830, -0.7071067811865464625, 0.000000000000000000 ) ) ;
#31583 = EDGE_CURVE ( 'NONE', #66284, #74755, #116454, .T. ) ;
#31584 = LINE ( 'NONE', #143189, #122758 ) ;
#31585 = DIRECTION ( 'NONE',  ( 1.000000000000000000, 0.000000000000000000, 0.000000000000000000 ) ) ;
#31586 = ORIENTED_EDGE ( 'NONE', *, *, #73150, .T. ) ;
#31587 = ORIENTED_EDGE ( 'NONE', *, *, #48955, .T. ) ;
#31588 = CARTESIAN_POINT ( 'NONE',  ( 14.99999999999989519, 20.70535890316562444, 1.956823837851882297 ) ) ;
#31589 = LINE ( 'NONE', #41027, #111609 ) ;
#31590 = CARTESIAN_POINT ( 'NONE',  ( -29.29289321881324426, 20.25929247661551713, 5.000000000000000000 ) ) ;
#31591 = EDGE_CURVE ( 'NONE', #134245, #61213, #109380, .T. ) ;
#31592 = FACE_OUTER_BOUND ( 'NONE', #19694, .T. ) ;
#31593 = CARTESIAN_POINT ( 'NONE',  ( 85.39169371712957002, 2.130196079827421762, 7.950000000000001066 ) ) ;
#31594 = DIRECTION ( 'NONE',  ( 0.3543493200069162685, -0.000000000000000000, -0.9351131265310288487 ) ) ;
#31595 = VECTOR ( 'NONE', #73095, 1000.000000000000000 ) ;
#31596 = LINE ( 'NONE', #142506, #13616 ) ;
#31597 = VERTEX_POINT ( 'NONE', #62097 ) ;
#31598 = DIRECTION ( 'NONE',  ( -0.7071067811865486830, -0.7071067811865464625, -0.000000000000000000 ) ) ;
#31599 = CARTESIAN_POINT ( 'NONE',  ( 3.183988606268992161, 28.73617430169789699, 5.000000000000000000 ) ) ;
#31600 = DIRECTION ( 'NONE',  ( -0.000000000000000000, 1.000000000000000000, -0.000000000000000000 ) ) ;
#31601 = ADVANCED_FACE ( 'NONE', ( #106255 ), #6928, .T. ) ;
#31602 = VECTOR ( 'NONE', #133087, 1000.000000000000000 ) ;
#31603 = ORIENTED_EDGE ( 'NONE', *, *, #25455, .T. ) ;
#31604 = CARTESIAN_POINT ( 'NONE',  ( 11.99999999999991651, -21.84840872380823384, 2.849755605029635763 ) ) ;
#31605 = VERTEX_POINT ( 'NONE', #110547 ) ;
#31606 = CARTESIAN_POINT ( 'NONE',  ( 75.25043019189811844, 3.055000000000002824, -5.291415217122919401 ) ) ;
#31607 = SURFACE_STYLE_USAGE ( .BOTH. , #130938 ) ;
#31608 = ADVANCED_FACE ( 'NONE', ( #1763 ), #78669, .T. ) ;
#31609 = CIRCLE ( 'NONE', #91811, 1.000000000000000888 ) ;
#31610 = DIRECTION ( 'NONE',  ( -0.000000000000000000, 0.3543493200069153248, 0.9351131265310292928 ) ) ;
#31611 = EDGE_LOOP ( 'NONE', ( #113018, #91438, #46919, #21385 ) ) ;
#31612 = DIRECTION ( 'NONE',  ( 1.000000000000000000, 1.224606353822377258E-16, 0.000000000000000000 ) ) ;
#31613 = DIRECTION ( 'NONE',  ( 0.7071067811865487940, 0.7071067811865463515, 0.000000000000000000 ) ) ;
#31614 = CARTESIAN_POINT ( 'NONE',  ( 25.49999999999983658, 1.087461875839234038, 4.000000000000000000 ) ) ;
#31615 = PLANE ( 'NONE',  #94859 ) ;
#31617 = ORIENTED_EDGE ( 'NONE', *, *, #78578, .T. ) ;
#31616 = DIRECTION ( 'NONE',  ( -0.7071067811865486830, -0.7071067811865464625, 0.000000000000000000 ) ) ;
#31618 = FACE_OUTER_BOUND ( 'NONE', #90644, .T. ) ;
#31619 = CARTESIAN_POINT ( 'NONE',  ( 5.588385094051650626, 22.22500000000000497, 4.777194822843813249 ) ) ;
#31620 = PLANE ( 'NONE',  #77260 ) ;
#31621 = CARTESIAN_POINT ( 'NONE',  ( 51.29974487139158867, -27.71228299555242103, 4.000000000000000000 ) ) ;
#31622 = EDGE_LOOP ( 'NONE', ( #101616, #104554, #66695, #64591 ) ) ;
#31623 = EDGE_CURVE ( 'NONE', #17366, #109623, #101115, .T. ) ;
#31624 = AXIS2_PLACEMENT_3D ( 'NONE', #40259, #17050, #84470 ) ;
#31625 = VERTEX_POINT ( 'NONE', #98284 ) ;
#31626 = CARTESIAN_POINT ( 'NONE',  ( 67.52126352523141861, -4.472830434245839371, -4.472830434245840259 ) ) ;
#31627 = ORIENTED_EDGE ( 'NONE', *, *, #13014, .T. ) ;
#31628 = AXIS2_PLACEMENT_3D ( 'NONE', #86916, #129682, #120204 ) ;
#31629 = LINE ( 'NONE', #75161, #123947 ) ;
#31630 = CARTESIAN_POINT ( 'NONE',  ( -5.999999999999956479, -0.2811185226894372113, -5.995736974527501317 ) ) ;
#31631 = VECTOR ( 'NONE', #74941, 1000.000000000000000 ) ;
#31632 = PLANE ( 'NONE',  #131419 ) ;
#31633 = LINE ( 'NONE', #30930, #47911 ) ;
#31634 = ORIENTED_EDGE ( 'NONE', *, *, #124940, .F. ) ;
#31635 = LINE ( 'NONE', #141083, #46935 ) ;
#31636 = CARTESIAN_POINT ( 'NONE',  ( -33.29974487139158867, -27.71228299555229313, 4.000000000000000000 ) ) ;
#31637 = EDGE_LOOP ( 'NONE', ( #120709, #76788, #46091, #67187 ) ) ;
#31638 = VECTOR ( 'NONE', #9890, 1000.000000000000000 ) ;
#31639 = ADVANCED_FACE ( 'NONE', ( #33759 ), #43196, .F. ) ;
#31640 = CARTESIAN_POINT ( 'NONE',  ( -75.18398860626899705, 28.73617430169839793, 5.000000000000000000 ) ) ;
#31641 = DIRECTION ( 'NONE',  ( -0.6830127018922181881, 0.6830127018922202975, -0.2588190451025214056 ) ) ;
#31642 = CARTESIAN_POINT ( 'NONE',  ( -39.18398860626899705, 28.73617430169814568, 5.000000000000000000 ) ) ;
#31643 = ORIENTED_EDGE ( 'NONE', *, *, #26858, .T. ) ;
#31644 = VERTEX_POINT ( 'NONE', #45359 ) ;
#31645 = AXIS2_PLACEMENT_3D ( 'NONE', #120564, #10394, #85113 ) ;
#31646 = EDGE_CURVE ( 'NONE', #73943, #123539, #67083, .T. ) ;
#31647 = FACE_BOUND ( 'NONE', #73290, .T. ) ;
#31648 = CARTESIAN_POINT ( 'NONE',  ( 54.48921356237310221, -27.52281430457093236, 5.000000000000000000 ) ) ;
#31649 = CARTESIAN_POINT ( 'NONE',  ( -71.99451991528749772, 28.92564299267988304, 4.000000000000000000 ) ) ;
#31650 = PLANE ( 'NONE',  #55231 ) ;
#31651 = DIRECTION ( 'NONE',  ( -0.7071067811865486830, -0.7071067811865464625, 0.000000000000000000 ) ) ;
#31652 = VECTOR ( 'NONE', #136107, 1000.000000000000000 ) ;
#31653 = VECTOR ( 'NONE', #84273, 1000.000000000000000 ) ;
#31654 = DIRECTION ( 'NONE',  ( -1.000000000000000000, 0.000000000000000000, -0.000000000000000000 ) ) ;
#31655 = VERTEX_POINT ( 'NONE', #120724 ) ;
#31656 = VECTOR ( 'NONE', #26966, 1000.000000000000000 ) ;
#31657 = ORIENTED_EDGE ( 'NONE', *, *, #92233, .F. ) ;
#31658 = CARTESIAN_POINT ( 'NONE',  ( 108.8495968585647660, 6.109999999999996767, 1.637169565754163836 ) ) ;
#31659 = ORIENTED_EDGE ( 'NONE', *, *, #68731, .T. ) ;
#31660 = ADVANCED_FACE ( 'NONE', ( #88849 ), #122145, .T. ) ;
#31661 = ORIENTED_EDGE ( 'NONE', *, *, #97716, .T. ) ;
#31662 = AXIS2_PLACEMENT_3D ( 'NONE', #73519, #39469, #85797 ) ;
#31663 =( NAMED_UNIT ( * ) SI_UNIT ( $, .STERADIAN. ) SOLID_ANGLE_UNIT ( ) );
#31664 = DIRECTION ( 'NONE',  ( 0.7071067811865486830, -0.7071067811865464625, -0.000000000000000000 ) ) ;
#31665 = FACE_OUTER_BOUND ( 'NONE', #4812, .T. ) ;
#31666 = ORIENTED_EDGE ( 'NONE', *, *, #8281, .T. ) ;
#31667 = PLANE ( 'NONE',  #38968 ) ;
#31668 = CARTESIAN_POINT ( 'NONE',  ( -57.29974487139158157, -27.71228299555246011, 4.000000000000000000 ) ) ;
#31669 = EDGE_CURVE ( 'NONE', #30172, #81904, #21433, .T. ) ;
#31670 = EDGE_CURVE ( 'NONE', #136234, #44903, #130309, .T. ) ;
#31671 = LINE ( 'NONE', #110619, #38845 ) ;
#31672 = FACE_OUTER_BOUND ( 'NONE', #25370, .T. ) ;
#31673 = CARTESIAN_POINT ( 'NONE',  ( -12.70000000000000462, -25.83999999999998920, 13.17925390838734323 ) ) ;
#31674 = ORIENTED_EDGE ( 'NONE', *, *, #42391, .T. ) ;
#31675 = PLANE ( 'NONE',  #35699 ) ;
#31676 = CARTESIAN_POINT ( 'NONE',  ( 17.07999999999999829, -2.055000000000000160, 2.789133085058098087E-16 ) ) ;
#31677 = ORIENTED_EDGE ( 'NONE', *, *, #75234, .F. ) ;
#31678 = EDGE_CURVE ( 'NONE', #5588, #122297, #119984, .T. ) ;
#31679 = ORIENTED_EDGE ( 'NONE', *, *, #96963, .F. ) ;
#31680 = EDGE_CURVE ( 'NONE', #26993, #41501, #44655, .T. ) ;
#31681 = VERTEX_POINT ( 'NONE', #56246 ) ;
#31682 = CARTESIAN_POINT ( 'NONE',  ( 59.64626352523142572, -4.472830434245840259, 4.472830434245838482 ) ) ;
#31683 = VERTEX_POINT ( 'NONE', #56943 ) ;
#31684 = PLANE ( 'NONE',  #53598 ) ;
#31685 = AXIS2_PLACEMENT_3D ( 'NONE', #9361, #140618, #42056 ) ;
#31686 = CARTESIAN_POINT ( 'NONE',  ( 100.1879301918981184, 6.110000000000002984, -1.637169565754156730 ) ) ;
#31687 = DIRECTION ( 'NONE',  ( -0.7071067811865486830, -0.7071067811865464625, -0.000000000000000000 ) ) ;
#31688 = CARTESIAN_POINT ( 'NONE',  ( 51.74999999999999289, -9.735942053221458872E-16, 7.950000000000000178 ) ) ;
#31689 = ORIENTED_EDGE ( 'NONE', *, *, #94742, .T. ) ;
#31690 = CARTESIAN_POINT ( 'NONE',  ( -16.17183060077636370, -5.240707523384225297, 4.000000000000000000 ) ) ;
#31691 = VECTOR ( 'NONE', #22482, 1000.000000000000114 ) ;
#31692 = PLANE ( 'NONE',  #26157 ) ;
#31693 = ADVANCED_FACE ( 'NONE', ( #88118 ), #1073, .F. ) ;
#31694 = CARTESIAN_POINT ( 'NONE',  ( 42.18398860626899705, 28.73617430169816700, 5.000000000000000000 ) ) ;
#31695 = CARTESIAN_POINT ( 'NONE',  ( -14.99999999999988987, -9.412538124160658271, 4.000000000000000000 ) ) ;
#31696 = ORIENTED_EDGE ( 'NONE', *, *, #31528, .T. ) ;
#31697 = DIRECTION ( 'NONE',  ( 0.7071067811865487940, 0.7071067811865463515, 0.000000000000000000 ) ) ;
#31698 = EDGE_LOOP ( 'NONE', ( #28713, #38110, #141387, #73461 ) ) ;
#31699 = ORIENTED_EDGE ( 'NONE', *, *, #136759, .F. ) ;
#31700 = ORIENTED_EDGE ( 'NONE', *, *, #96700, .T. ) ;
#31702 = VECTOR ( 'NONE', #11752, 1000.000000000000000 ) ;
#31701 = CARTESIAN_POINT ( 'NONE',  ( 117.4537635252314516, -6.109999999999998543, -3.741295971395162543E-16 ) ) ;
#31703 = EDGE_LOOP ( 'NONE', ( #129102, #24569, #74600, #38447 ) ) ;
#31704 = CARTESIAN_POINT ( 'NONE',  ( 11.70025512860841133, -27.71228299555198049, 4.000000000000000000 ) ) ;
#31705 = VECTOR ( 'NONE', #72715, 1000.000000000000227 ) ;
#31706 = DIRECTION ( 'NONE',  ( -0.7071067811865486830, -0.7071067811865464625, 0.000000000000000000 ) ) ;
#31707 = VERTEX_POINT ( 'NONE', #77272 ) ;
#31708 = DIRECTION ( 'NONE',  ( 0.7071067811865487940, 0.7071067811865463515, -0.000000000000000000 ) ) ;
#31709 = ORIENTED_EDGE ( 'NONE', *, *, #21860, .T. ) ;
#31710 = VECTOR ( 'NONE', #88750, 1000.000000000000000 ) ;
#31711 = CARTESIAN_POINT ( 'NONE',  ( 10.62456980810188689, -6.871911579029512218, 3.967499999999996252 ) ) ;
#31712 = CARTESIAN_POINT ( 'NONE',  ( -39.48921356237310221, -27.52281430457082934, 5.000000000000000000 ) ) ;
#31713 = ADVANCED_FACE ( 'NONE', ( #10526 ), #121443, .F. ) ;
#31714 = LINE ( 'NONE', #63656, #83061 ) ;
#31715 = VECTOR ( 'NONE', #77836, 1000.000000000000000 ) ;
#31716 = CARTESIAN_POINT ( 'NONE',  ( 14.99999999999989875, -13.44781430457069149, 5.000000000000000000 ) ) ;
#31717 = ORIENTED_EDGE ( 'NONE', *, *, #68300, .F. ) ;
#31718 = ADVANCED_FACE ( 'NONE', ( #90241 ), #99684, .F. ) ;
#31719 = ORIENTED_EDGE ( 'NONE', *, *, #139242, .F. ) ;
#31720 = ORIENTED_EDGE ( 'NONE', *, *, #81843, .F. ) ;
#31721 = CARTESIAN_POINT ( 'NONE',  ( 11.99999999999993427, 20.58746187583903264, 4.000000000000000000 ) ) ;
#31722 = PRESENTATION_STYLE_ASSIGNMENT (( #97684 ) ) ;
#31723 = LINE ( 'NONE', #64353, #132980 ) ;
#31724 = DIRECTION ( 'NONE',  ( -0.7071067811865487940, 0.7071067811865463515, 0.000000000000000000 ) ) ;
#31725 = EDGE_CURVE ( 'NONE', #5194, #45596, #23563, .T. ) ;
#31726 = EDGE_CURVE ( 'NONE', #53276, #139884, #134485, .T. ) ;
#31727 = CARTESIAN_POINT ( 'NONE',  ( 0.000000000000000000, 0.000000000000000000, 5.000000000000000000 ) ) ;
#31728 = PLANE ( 'NONE',  #71516 ) ;
#31729 = CARTESIAN_POINT ( 'NONE',  ( 28.00043019189810067, -3.055000000000002380, 5.291415217122920289 ) ) ;
#31730 = DIRECTION ( 'NONE',  ( 0.6830127018922181881, 0.6830127018922202975, -0.2588190451025214056 ) ) ;
#31731 = CARTESIAN_POINT ( 'NONE',  ( -17.99999999999987566, 15.45873954670183359, -0.03131636524290101059 ) ) ;
#31732 = ORIENTED_EDGE ( 'NONE', *, *, #41971, .T. ) ;
#31733 = DIRECTION ( 'NONE',  ( -0.000000000000000000, -0.3543493200069152693, 0.9351131265310292928 ) ) ;
#31734 = ORIENTED_EDGE ( 'NONE', *, *, #112311, .F. ) ;
#31735 = PLANE ( 'NONE',  #42963 ) ;
#31736 = ORIENTED_EDGE ( 'NONE', *, *, #70379, .F. ) ;
#31737 = DIRECTION ( 'NONE',  ( -0.7071067811865486830, -0.7071067811865464625, -0.000000000000000000 ) ) ;
#31739 = EDGE_LOOP ( 'NONE', ( #63390, #137905, #21162, #122832, #137588, #32569, #94330, #7131 ) ) ;
#31738 = CARTESIAN_POINT ( 'NONE',  ( -34.42500000000001137, -12.02281430457044564, 5.000000000000000000 ) ) ;
#31740 = STYLED_ITEM ( 'NONE', ( #26646 ), #111891 ) ;
#31741 = ADVANCED_FACE ( 'NONE', ( #59782 ), #81549, .F. ) ;
#31742 = ADVANCED_FACE ( 'NONE', ( #69974 ), #68530, .T. ) ;
#31743 = LINE ( 'NONE', #120873, #51481 ) ;
#31744 = ORIENTED_EDGE ( 'NONE', *, *, #35215, .T. ) ;
#31745 = SURFACE_STYLE_FILL_AREA ( #95561 ) ;
#31746 = ORIENTED_EDGE ( 'NONE', *, *, #87535, .T. ) ;
#31747 = CARTESIAN_POINT ( 'NONE',  ( 16.82816939922341604, -5.240707523384228850, 4.000000000000000000 ) ) ;
#31748 = ORIENTED_EDGE ( 'NONE', *, *, #67089, .F. ) ;
#31749 = AXIS2_PLACEMENT_3D ( 'NONE', #90116, #132232, #11824 ) ;
#31750 = VECTOR ( 'NONE', #14351, 1000.000000000000000 ) ;
#31751 =( NAMED_UNIT ( * ) SI_UNIT ( $, .STERADIAN. ) SOLID_ANGLE_UNIT ( ) );
#31753 = CARTESIAN_POINT ( 'NONE',  ( 108.4333603837962272, 2.130196079827431532, -7.949999999999997513 ) ) ;
#31752 = VECTOR ( 'NONE', #18947, 1000.000000000000000 ) ;
#31754 = CARTESIAN_POINT ( 'NONE',  ( 49.95419371712955581, 6.884901960086283523, 3.975000000000002753 ) ) ;
#31755 = EDGE_CURVE ( 'NONE', #52226, #56014, #101839, .T. ) ;
#31756 = PLANE ( 'NONE',  #16092 ) ;
#31757 = FACE_OUTER_BOUND ( 'NONE', #121739, .T. ) ;
#31758 = DIRECTION ( 'NONE',  ( -1.000000000000000000, -1.224606353822377258E-16, -0.000000000000000000 ) ) ;
#31759 = DIRECTION ( 'NONE',  ( 0.000000000000000000, -0.2555582702174447052, 0.9667936545734397980 ) ) ;
#31760 = CARTESIAN_POINT ( 'NONE',  ( 1.750000000000000222, -7.464222240803106570E-16, -6.094999999999989981 ) ) ;
#31761 = CARTESIAN_POINT ( 'NONE',  ( 12.81206980810188334, 7.934999999999992504, 2.126176841940951689 ) ) ;
#31762 = VECTOR ( 'NONE', #3076, 1000.000000000000000 ) ;
#31763 = ADVANCED_FACE ( 'NONE', ( #24972 ), #21530, .T. ) ;
#31764 = CYLINDRICAL_SURFACE ( 'NONE', #35095, 7.950000000000000178 ) ;
#31765 = FACE_OUTER_BOUND ( 'NONE', #85100, .T. ) ;
#31766 = EDGE_LOOP ( 'NONE', ( #84293, #92897, #90708, #52677 ) ) ;
#31767 = ORIENTED_EDGE ( 'NONE', *, *, #84478, .F. ) ;
#31768 = PLANE ( 'NONE',  #55960 ) ;
#31769 = ORIENTED_EDGE ( 'NONE', *, *, #104864, .T. ) ;
#31770 = DIRECTION ( 'NONE',  ( 0.7071067811865487940, 0.7071067811865463515, 0.000000000000000000 ) ) ;
#31771 = CARTESIAN_POINT ( 'NONE',  ( 34.92499999999998295, -21.72500000000000142, 5.000000000000000000 ) ) ;
#31772 = LINE ( 'NONE', #96270, #141324 ) ;
#31773 = EDGE_CURVE ( 'NONE', #52437, #40456, #135897, .T. ) ;
#31774 = CARTESIAN_POINT ( 'NONE',  ( 130.2059003229214227, -48.16486758952284930, -37.61253110040706105 ) ) ;
#31775 = ORIENTED_EDGE ( 'NONE', *, *, #35334, .T. ) ;
#31776 = DIRECTION ( 'NONE',  ( 0.7071067811865487940, -0.7071067811865463515, 0.000000000000000000 ) ) ;
#31777 = LINE ( 'NONE', #75994, #78895 ) ;
#31778 = CARTESIAN_POINT ( 'NONE',  ( -36.48921356237310221, -27.52281430457080802, 5.000000000000000000 ) ) ;
#31779 =( LENGTH_UNIT ( ) NAMED_UNIT ( * ) SI_UNIT ( .MILLI., .METRE. ) );
#31782 = ORIENTED_EDGE ( 'NONE', *, *, #105571, .F. ) ;
#31781 = EDGE_CURVE ( 'NONE', #102270, #11869, #75972, .T. ) ;
#31780 = CARTESIAN_POINT ( 'NONE',  ( -7.203449814691606612, -22.22500000000000142, 15.50473165117706031 ) ) ;
#31783 = DIRECTION ( 'NONE',  ( -0.7071067811865486830, -0.7071067811865464625, 0.000000000000000000 ) ) ;
#31785 = ADVANCED_FACE ( 'NONE', ( #13375 ), #57652, .F. ) ;
#31784 = VECTOR ( 'NONE', #28320, 1000.000000000000000 ) ;
#31786 = CARTESIAN_POINT ( 'NONE',  ( 66.29974487139159578, -27.71228299555252406, 4.000000000000000000 ) ) ;
#31787 = LINE ( 'NONE', #20887, #108091 ) ;
#31788 = DIRECTION ( 'NONE',  ( 0.000000000000000000, -1.000000000000000000, 0.000000000000000000 ) ) ;
#31789 = VERTEX_POINT ( 'NONE', #114138 ) ;
#31790 = EDGE_CURVE ( 'NONE', #99307, #13986, #92365, .T. ) ;
#31791 = EDGE_LOOP ( 'NONE', ( #87983, #96046, #34525, #90373 ) ) ;
#31792 = ORIENTED_EDGE ( 'NONE', *, *, #99454, .F. ) ;
#31793 = CARTESIAN_POINT ( 'NONE',  ( 95.66709685856477563, -3.055000000000000160, -5.291415217122921177 ) ) ;
#31794 = VECTOR ( 'NONE', #112747, 999.9999999999998863 ) ;
#31795 = ORIENTED_EDGE ( 'NONE', *, *, #48712, .F. ) ;
#31796 = CARTESIAN_POINT ( 'NONE',  ( 128.5740698622001901, -49.04047092357102855, 39.41690992498948987 ) ) ;
#31797 = CIRCLE ( 'NONE', #52583, 2.247900000000000453 ) ;
#31798 = PLANE ( 'NONE',  #138336 ) ;
#31799 = ORIENTED_EDGE ( 'NONE', *, *, #106370, .F. ) ;
#31800 = ADVANCED_FACE ( 'NONE', ( #60508 ), #137339, .T. ) ;
#31801 = CARTESIAN_POINT ( 'NONE',  ( 183.7627343495647665, -51.96230815476840803, 39.57541490114646621 ) ) ;
#31803 =( BOUNDED_CURVE ( )  B_SPLINE_CURVE ( 3, ( #27457, #101642, #132885, #90798 ),
 .UNSPECIFIED., .F., .F. ) 
 B_SPLINE_CURVE_WITH_KNOTS ( ( 4, 4 ),
 ( 4.712388980384689674, 6.105785702739217946 ),
 .UNSPECIFIED. ) 
 CURVE ( )  GEOMETRIC_REPRESENTATION_ITEM ( )  RATIONAL_B_SPLINE_CURVE ( ( 1.000000000000000000, 0.8446433258982464221, 0.8446433258982464221, 1.000000000000000000 ) ) 
 REPRESENTATION_ITEM ( '' )  );
#31802 = CARTESIAN_POINT ( 'NONE',  ( 11.16170612452612865, -6.740707523384212863, 16.75550250614870151 ) ) ;
#31804 = CARTESIAN_POINT ( 'NONE',  ( 92.07876352523145158, -7.482591942790325086E-16, 6.109999999999998543 ) ) ;
#31805 = ORIENTED_EDGE ( 'NONE', *, *, #127569, .F. ) ;
#31806 = CARTESIAN_POINT ( 'NONE',  ( 1.030796516412011643, 0.5999999999999987566, -4.508445023301312027 ) ) ;
#31807 = CARTESIAN_POINT ( 'NONE',  ( 117.0375270504628986, -9.735942053221456900E-16, 7.949999999999998401 ) ) ;
#31808 = ORIENTED_EDGE ( 'NONE', *, *, #119278, .T. ) ;
#31809 = VERTEX_POINT ( 'NONE', #93817 ) ;
#31810 = AXIS2_PLACEMENT_3D ( 'NONE', #139741, #5598, #95477 ) ;
#31811 = ORIENTED_EDGE ( 'NONE', *, *, #124729, .F. ) ;
#31812 = CARTESIAN_POINT ( 'NONE',  ( 60.50000000000000000, 0.000000000000000000, -7.950000000000000178 ) ) ;
#31813 = CARTESIAN_POINT ( 'NONE',  ( -29.99999999999978328, -3.412538124160721331, 4.000000000000000000 ) ) ;
#31814 = CARTESIAN_POINT ( 'NONE',  ( 17.56706980810188767, 2.126176841940952134, -7.934999999999992504 ) ) ;
#31815 = DIRECTION ( 'NONE',  ( 0.7071067811865486830, -0.7071067811865464625, -0.000000000000000000 ) ) ;
#31816 = FACE_OUTER_BOUND ( 'NONE', #89155, .T. ) ;
#31817 = DIRECTION ( 'NONE',  ( 0.7071067811865487940, -0.7071067811865463515, 0.000000000000000000 ) ) ;
#31818 = FILL_AREA_STYLE_COLOUR ( '', #35376 ) ;
#31819 = ORIENTED_EDGE ( 'NONE', *, *, #69261, .T. ) ;
#31820 = VECTOR ( 'NONE', #1485, 1000.000000000000227 ) ;
#31821 = ORIENTED_EDGE ( 'NONE', *, *, #62878, .F. ) ;
#31822 = DIRECTION ( 'NONE',  ( 0.7071067811865486830, -0.7071067811865464625, -0.000000000000000000 ) ) ;
#31824 = EDGE_CURVE ( 'NONE', #81813, #111086, #25697, .T. ) ;
#31823 = ORIENTED_EDGE ( 'NONE', *, *, #106962, .F. ) ;
#31825 = ORIENTED_EDGE ( 'NONE', *, *, #106755, .T. ) ;
#31826 = VECTOR ( 'NONE', #90980, 1000.000000000000000 ) ;
#31827 = CARTESIAN_POINT ( 'NONE',  ( 81.49999999999998579, 0.000000000000000000, -7.950000000000000178 ) ) ;
#31828 = ORIENTED_EDGE ( 'NONE', *, *, #79321, .T. ) ;
#31829 = DIRECTION ( 'NONE',  ( 1.000000000000000000, 0.000000000000000000, 0.000000000000000000 ) ) ;
#31830 =( NAMED_UNIT ( * ) SI_UNIT ( $, .STERADIAN. ) SOLID_ANGLE_UNIT ( ) );
#31831 = LINE ( 'NONE', #42735, #131262 ) ;
#31832 = FACE_OUTER_BOUND ( 'NONE', #140725, .T. ) ;
#31833 = VECTOR ( 'NONE', #12238, 1000.000000000000000 ) ;
#31834 = CARTESIAN_POINT ( 'NONE',  ( 9.591592354503321260, 2.500000000000001332, 0.000000000000000000 ) ) ;
#31835 = ORIENTED_EDGE ( 'NONE', *, *, #72425, .T. ) ;
#31836 =( NAMED_UNIT ( * ) SI_UNIT ( $, .STERADIAN. ) SOLID_ANGLE_UNIT ( ) );
#31837 = AXIS2_PLACEMENT_3D ( 'NONE', #133815, #69284, #23617 ) ;
#31838 = ORIENTED_EDGE ( 'NONE', *, *, #62387, .T. ) ;
#31839 = EDGE_CURVE ( 'NONE', #46544, #25800, #14823, .T. ) ;
#31840 = DIRECTION ( 'NONE',  ( -1.000000000000000000, -1.224606353822377258E-16, -0.000000000000000000 ) ) ;
#31841 = ORIENTED_EDGE ( 'NONE', *, *, #40518, .F. ) ;
#31842 = ORIENTED_EDGE ( 'NONE', *, *, #30632, .F. ) ;
#31844 = ADVANCED_FACE ( 'NONE', ( #3902 ), #103947, .F. ) ;
#31843 = CARTESIAN_POINT ( 'NONE',  ( 8.999999999999946709, 1.552185695429156187, 5.000000000000000000 ) ) ;
#31845 = ORIENTED_EDGE ( 'NONE', *, *, #48101, .F. ) ;
#31846 = ORIENTED_EDGE ( 'NONE', *, *, #86079, .F. ) ;
#31847 = AXIS2_PLACEMENT_3D ( 'NONE', #99955, #45606, #89775 ) ;
#31848 = ORIENTED_EDGE ( 'NONE', *, *, #137253, .T. ) ;
#31850 = ADVANCED_FACE ( 'NONE', ( #35185 ), #48903, .F. ) ;
#31849 = AXIS2_PLACEMENT_3D ( 'NONE', #112434, #142914, #99378 ) ;
#31851 = AXIS2_PLACEMENT_3D ( 'NONE', #114350, #4094, #15700 ) ;
#31852 = LINE ( 'NONE', #109405, #118348 ) ;
#31853 = CARTESIAN_POINT ( 'NONE',  ( -9.121473163371414117, -20.24070752338407431, 7.412974875817811338 ) ) ;
#31854 = DIRECTION ( 'NONE',  ( 0.6830127018922181881, 0.6830127018922202975, -0.2588190451025214056 ) ) ;
#31855 = DIRECTION ( 'NONE',  ( 0.9425785261922230429, 0.3339846133601018230, 0.000000000000000000 ) ) ;
#31856 = FACE_OUTER_BOUND ( 'NONE', #72305, .T. ) ;
#31857 = FACE_OUTER_BOUND ( 'NONE', #113125, .T. ) ;
#31858 = EDGE_CURVE ( 'NONE', #42811, #57178, #26428, .T. ) ;
#31859 = CARTESIAN_POINT ( 'NONE',  ( 12.19999999999999574, 0.000000000000000000, -0.5000000000000004441 ) ) ;
#31860 = CIRCLE ( 'NONE', #36514, 2.500000000000000444 ) ;
#31861 = DIRECTION ( 'NONE',  ( -0.3543493200069162685, -0.000000000000000000, -0.9351131265310288487 ) ) ;
#31862 = EDGE_CURVE ( 'NONE', #119359, #132971, #126431, .T. ) ;
#31863 = CARTESIAN_POINT ( 'NONE',  ( 13.49999999999990408, -11.56887692260769995, 4.000000000000000000 ) ) ;
#31864 = CARTESIAN_POINT ( 'NONE',  ( 4.176659101599700108, 5.259292476615659240, 15.86257073897096781 ) ) ;
#31865 = PLANE ( 'NONE',  #135221 ) ;
#31866 = EDGE_LOOP ( 'NONE', ( #102173, #53537, #31112, #58674, #4807, #58060, #143398, #126352 ) ) ;
#31867 = ORIENTED_EDGE ( 'NONE', *, *, #91764, .F. ) ;
#31868 = ORIENTED_EDGE ( 'NONE', *, *, #46964, .T. ) ;
#31869 = LINE ( 'NONE', #45631, #77336 ) ;
#31870 = ADVANCED_FACE ( 'NONE', ( #27123 ), #124305, .F. ) ;
#31871 = ORIENTED_EDGE ( 'NONE', *, *, #114816, .T. ) ;
#31872 = VERTEX_POINT ( 'NONE', #107540 ) ;
#31873 = FACE_OUTER_BOUND ( 'NONE', #45211, .T. ) ;
#31874 = FILL_AREA_STYLE ('',( #54376 ) ) ;
#31875 = CARTESIAN_POINT ( 'NONE',  ( 0.000000000000000000, 60.00000000000000000, 0.000000000000000000 ) ) ;
#31876 = VERTEX_POINT ( 'NONE', #6053 ) ;
#31877 = VECTOR ( 'NONE', #23640, 1000.000000000000000 ) ;
#31878 = DIRECTION ( 'NONE',  ( 0.7071067811865487940, 0.7071067811865463515, -0.000000000000000000 ) ) ;
#31879 = EDGE_CURVE ( 'NONE', #37438, #98546, #74953, .T. ) ;
#31880 = EDGE_CURVE ( 'NONE', #130610, #75725, #61247, .T. ) ;
#31881 = ORIENTED_EDGE ( 'NONE', *, *, #75452, .F. ) ;
#31882 = CARTESIAN_POINT ( 'NONE',  ( 4.828169399223495084, 0.7592924766157104211, 4.000000000000000000 ) ) ;
#31883 = CIRCLE ( 'NONE', #103577, 2.500000000000000888 ) ;
#31884 = CARTESIAN_POINT ( 'NONE',  ( 18.15040314143522338, 7.934999999999989839, -2.126176841940961904 ) ) ;
#31885 = ORIENTED_EDGE ( 'NONE', *, *, #41238, .F. ) ;
#31886 = CARTESIAN_POINT ( 'NONE',  ( 94.70376352523145158, 6.109999999999999432, 1.122388791418549108E-15 ) ) ;
#31887 = CARTESIAN_POINT ( 'NONE',  ( 1.499999999999987566, 16.18958161055402911, -11.56426086740811066 ) ) ;
#31888 = FACE_OUTER_BOUND ( 'NONE', #38705, .T. ) ;
#31889 = CARTESIAN_POINT ( 'NONE',  ( -27.51665438641025574, 22.22500000000000142, 4.500000000000000888 ) ) ;
#31890 = ORIENTED_EDGE ( 'NONE', *, *, #86135, .F. ) ;
#31891 = EDGE_CURVE ( 'NONE', #77128, #29743, #127147, .T. ) ;
#31892 = LINE ( 'NONE', #132672, #110172 ) ;
#31893 = VERTEX_POINT ( 'NONE', #18357 ) ;
#31894 = DIRECTION ( 'NONE',  ( 0.000000000000000000, -1.000000000000000000, 0.000000000000000000 ) ) ;
#31895 = VERTEX_POINT ( 'NONE', #39461 ) ;
#31896 = DIRECTION ( 'NONE',  ( -0.7071067811865487940, 0.7071067811865463515, -0.000000000000000000 ) ) ;
#31897 = LINE ( 'NONE', #55086, #69614 ) ;
#31898 = CARTESIAN_POINT ( 'NONE',  ( 15.48921356237309510, -27.52281430457066236, 5.000000000000000000 ) ) ;
#31899 = DIRECTION ( 'NONE',  ( -0.7071067811865486830, -0.7071067811865464625, 0.000000000000000000 ) ) ;
#31900 = EDGE_LOOP ( 'NONE', ( #141173, #119598, #90106, #134579 ) ) ;
#31901 = EDGE_CURVE ( 'NONE', #18367, #59489, #50325, .T. ) ;
#31902 = EDGE_CURVE ( 'NONE', #93492, #82948, #105394, .T. ) ;
#31903 = CARTESIAN_POINT ( 'NONE',  ( -11.75830541574806531, 0.7592924766157104211, 14.37146558664985285 ) ) ;
#31904 = LINE ( 'NONE', #62408, #132342 ) ;
#31905 = CARTESIAN_POINT ( 'NONE',  ( 57.48921356237308800, -27.52281430457095368, 5.000000000000000000 ) ) ;
#31906 = VERTEX_POINT ( 'NONE', #140187 ) ;
#31907 = DIRECTION ( 'NONE',  ( 0.7071067811865487940, -0.7071067811865463515, 0.000000000000000000 ) ) ;
#31909 = EDGE_CURVE ( 'NONE', #122911, #91753, #100293, .T. ) ;
#31908 = DIRECTION ( 'NONE',  ( -0.6830127018922180770, -0.6830127018922204085, -0.2588190451025213501 ) ) ;
#31910 = VERTEX_POINT ( 'NONE', #62633 ) ;
#31912 = EDGE_LOOP ( 'NONE', ( #41478, #40331, #39933 ) ) ;
#31911 = DIRECTION ( 'NONE',  ( 1.055184596092948005E-16, -1.000000000000000000, 0.000000000000000000 ) ) ;
#31914 = ORIENTED_EDGE ( 'NONE', *, *, #61755, .T. ) ;
#31913 = EDGE_CURVE ( 'NONE', #78673, #92363, #84398, .T. ) ;
#31915 = DIRECTION ( 'NONE',  ( -0.000000000000000000, 0.3543493200069152138, -0.9351131265310292928 ) ) ;
#31916 = CARTESIAN_POINT ( 'NONE',  ( -14.20710678118643955, -17.24070752338410273, 5.000000000000000000 ) ) ;
#31917 = ORIENTED_EDGE ( 'NONE', *, *, #98467, .T. ) ;
#31918 = LINE ( 'NONE', #76143, #58270 ) ;
#31919 = UNCERTAINTY_MEASURE_WITH_UNIT (LENGTH_MEASURE( 1.000000000000000082E-05 ), #61810, 'distance_accuracy_value', 'NONE');
#31920 = LINE ( 'NONE', #129796, #98482 ) ;
#31921 = LINE ( 'NONE', #44991, #76347 ) ;
#31922 = VECTOR ( 'NONE', #97438, 1000.000000000000000 ) ;
#31923 = EDGE_CURVE ( 'NONE', #50924, #103756, #77138, .T. ) ;
#31924 = CARTESIAN_POINT ( 'NONE',  ( -54.18398860626899705, 28.73617430169825226, 5.000000000000000000 ) ) ;
#31925 = FACE_OUTER_BOUND ( 'NONE', #52554, .T. ) ;
#31926 = CARTESIAN_POINT ( 'NONE',  ( 15.67180000000000284, 3.174999999999997602, 1.444000000000000394 ) ) ;
#31927 = LINE ( 'NONE', #55117, #54125 ) ;
#31928 = SURFACE_STYLE_USAGE ( .BOTH. , #120316 ) ;
#31929 = PLANE ( 'NONE',  #9626 ) ;
#31930 = DIRECTION ( 'NONE',  ( 0.7071067811865487940, -0.7071067811865463515, 0.000000000000000000 ) ) ;
#31931 = ADVANCED_FACE ( 'NONE', ( #83689 ), #127897, .T. ) ;
#31932 = DIRECTION ( 'NONE',  ( -0.7071067811865487940, 0.7071067811865463515, 0.000000000000000000 ) ) ;
#31933 = CARTESIAN_POINT ( 'NONE',  ( 0.8134913539763841683, -15.74070752338412049, 8.904080028138940506 ) ) ;
#31934 = ORIENTED_EDGE ( 'NONE', *, *, #74960, .F. ) ;
#31935 = ORIENTED_EDGE ( 'NONE', *, *, #38426, .F. ) ;
#31936 = ORIENTED_EDGE ( 'NONE', *, *, #90049, .T. ) ;
#31937 = CARTESIAN_POINT ( 'NONE',  ( 97.83333333333332860, -6.884901960086287964, 3.974999999999998312 ) ) ;
#31938 = AXIS2_PLACEMENT_3D ( 'NONE', #90058, #13197, #103098 ) ;
#31939 = VERTEX_POINT ( 'NONE', #29973 ) ;
#31940 = ORIENTED_EDGE ( 'NONE', *, *, #106570, .F. ) ;
#31941 = ORIENTED_EDGE ( 'NONE', *, *, #38402, .T. ) ;
#31942 = CARTESIAN_POINT ( 'NONE',  ( 11.99999999999991651, 8.966399257802171618, 5.000000000000000000 ) ) ;
#31943 = DIRECTION ( 'NONE',  ( 1.000000000000000000, 1.224606353822377258E-16, 0.000000000000000000 ) ) ;
#31944 = ORIENTED_EDGE ( 'NONE', *, *, #40358, .F. ) ;
#31945 = CIRCLE ( 'NONE', #117582, 2.500000000000000888 ) ;
#31946 = CARTESIAN_POINT ( 'NONE',  ( 25.49999999999982947, 10.08746187583913922, 4.000000000000000000 ) ) ;
#31947 = CARTESIAN_POINT ( 'NONE',  ( 2.999999999999981792, -4.068876922607773672, 4.000000000000000000 ) ) ;
#31948 = AXIS2_PLACEMENT_3D ( 'NONE', #67713, #134371, #114025 ) ;
#31949 = DIRECTION ( 'NONE',  ( 1.000000000000000000, 0.000000000000000000, 0.000000000000000000 ) ) ;
#31950 = LINE ( 'NONE', #55139, #4839 ) ;
#31951 = ORIENTED_EDGE ( 'NONE', *, *, #103834, .T. ) ;
#31952 = DIRECTION ( 'NONE',  ( 0.3543493200069162685, -0.000000000000000000, -0.9351131265310288487 ) ) ;
#31953 = PRESENTATION_STYLE_ASSIGNMENT (( #142165 ) ) ;
#31955 = CARTESIAN_POINT ( 'NONE',  ( -72.29974487139158157, -27.71228299555256669, 4.000000000000000000 ) ) ;
#31954 = AXIS2_PLACEMENT_3D ( 'NONE', #113314, #135124, #26334 ) ;
#31956 = CARTESIAN_POINT ( 'NONE',  ( 2.999999999999978240, 11.96639925780213609, 5.000000000000000000 ) ) ;
#31957 = CARTESIAN_POINT ( 'NONE',  ( -22.39656807105343361, -14.24070752338413648, 19.24067776001720986 ) ) ;
#31958 = CARTESIAN_POINT ( 'NONE',  ( 32.16252705046289151, 7.949999999999998401, 1.460391307983218338E-15 ) ) ;
#31959 = PLANE ( 'NONE',  #37560 ) ;
#31960 = ADVANCED_FACE ( 'NONE', ( #51037 ), #28579, .F. ) ;
#31961 = EDGE_CURVE ( 'NONE', #133096, #131795, #72837, .T. ) ;
#31962 = ORIENTED_EDGE ( 'NONE', *, *, #15981, .T. ) ;
#31963 = VERTEX_POINT ( 'NONE', #16977 ) ;
#31964 = CARTESIAN_POINT ( 'NONE',  ( 124.3962635252314470, 4.472830434245840259, -4.472830434245839371 ) ) ;
#31965 = ORIENTED_EDGE ( 'NONE', *, *, #138090, .T. ) ;
#31966 = CARTESIAN_POINT ( 'NONE',  ( -18.48921356237309510, -27.52281430457068367, 5.000000000000000000 ) ) ;
#31967 = LINE ( 'NONE', #141445, #52481 ) ;
#31968 = DIRECTION ( 'NONE',  ( -0.000000000000000000, -0.3543493200069152693, 0.9351131265310292928 ) ) ;
#31969 = LINE ( 'NONE', #40715, #35373 ) ;
#31970 = LINE ( 'NONE', #134150, #86003 ) ;
#31971 = FACE_OUTER_BOUND ( 'NONE', #105404, .T. ) ;
#31972 = CARTESIAN_POINT ( 'NONE',  ( 118.7662635252314516, 4.472830434245839371, -4.472830434245838482 ) ) ;
#31973 = ORIENTED_EDGE ( 'NONE', *, *, #73206, .T. ) ;
#31974 = VERTEX_POINT ( 'NONE', #53149 ) ;
#31975 = PLANE ( 'NONE',  #27725 ) ;
#31976 = AXIS2_PLACEMENT_3D ( 'NONE', #132859, #121925, #142985 ) ;
#31977 = CARTESIAN_POINT ( 'NONE',  ( 4.499999999999967137, 15.05218569542901896, 5.000000000000000000 ) ) ;
#31978 = EDGE_LOOP ( 'NONE', ( #107646, #54824, #100148, #39494 ) ) ;
#31979 = CARTESIAN_POINT ( 'NONE',  ( 43.89626352523143282, 4.472830434245840259, -4.472830434245839371 ) ) ;
#31980 = VERTEX_POINT ( 'NONE', #73509 ) ;
#31981 = DIRECTION ( 'NONE',  ( -0.000000000000000000, -0.000000000000000000, 1.000000000000000000 ) ) ;
#31982 = LINE ( 'NONE', #140056, #129529 ) ;
#31983 = CARTESIAN_POINT ( 'NONE',  ( 9.994118527364397764, 3.061616997868383634E-16, -2.500000000000000444 ) ) ;
#31984 = VECTOR ( 'NONE', #124040, 1000.000000000000227 ) ;
#31985 = SURFACE_STYLE_FILL_AREA ( #98659 ) ;
#31986 =( BOUNDED_CURVE ( )  B_SPLINE_CURVE ( 3, ( #85753, #63341, #142310, #61901 ),
 .UNSPECIFIED., .F., .T. ) 
 B_SPLINE_CURVE_WITH_KNOTS ( ( 4, 4 ),
 ( 1.570796326794896558, 3.141592653589793116 ),
 .UNSPECIFIED. ) 
 CURVE ( )  GEOMETRIC_REPRESENTATION_ITEM ( )  RATIONAL_B_SPLINE_CURVE ( ( 1.000000000000000000, 0.8047378541243649375, 0.8047378541243649375, 1.000000000000000000 ) ) 
 REPRESENTATION_ITEM ( '' )  );
#31987 = CARTESIAN_POINT ( 'NONE',  ( 42.93293019189812298, 1.637169565754156508, 6.110000000000000320 ) ) ;
#31988 = ORIENTED_EDGE ( 'NONE', *, *, #49774, .F. ) ;
#31989 = DIRECTION ( 'NONE',  ( -0.7071067811865486830, -0.7071067811865464625, 0.000000000000000000 ) ) ;
#31991 = EDGE_CURVE ( 'NONE', #91335, #129128, #117672, .T. ) ;
#31990 = ORIENTED_EDGE ( 'NONE', *, *, #36450, .T. ) ;
#31992 = ORIENTED_EDGE ( 'NONE', *, *, #69206, .F. ) ;
#31993 = VECTOR ( 'NONE', #21695, 1000.000000000000000 ) ;
#31994 = ORIENTED_EDGE ( 'NONE', *, *, #46665, .T. ) ;
#31995 = AXIS2_PLACEMENT_3D ( 'NONE', #101975, #14949, #58533 ) ;
#31996 = FACE_OUTER_BOUND ( 'NONE', #13981, .T. ) ;
#31997 = LINE ( 'NONE', #10231, #9458 ) ;
#31998 = ORIENTED_EDGE ( 'NONE', *, *, #87360, .F. ) ;
#31999 = DIRECTION ( 'NONE',  ( 0.6830127018922181881, 0.6830127018922202975, -0.2588190451025214056 ) ) ;
#32000 = DIRECTION ( 'NONE',  ( 1.000000000000000000, 0.000000000000000000, 0.000000000000000000 ) ) ;
#32001 = CARTESIAN_POINT ( 'NONE',  ( -11.67183060077639567, -6.740707523384219968, 4.000000000000000000 ) ) ;
#32002 = ADVANCED_FACE ( 'NONE', ( #74215 ), #85789, .T. ) ;
#32003 = FACE_BOUND ( 'NONE', #94734, .T. ) ;
#32004 = ORIENTED_EDGE ( 'NONE', *, *, #32883, .F. ) ;
#32005 = DIRECTION ( 'NONE',  ( 0.7071067811865486830, -0.7071067811865464625, -0.000000000000000000 ) ) ;
#32006 = EDGE_CURVE ( 'NONE', #117128, #69078, #118407, .T. ) ;
#32007 = EDGE_CURVE ( 'NONE', #135296, #75313, #79532, .T. ) ;
#32008 = DIRECTION ( 'NONE',  ( 0.7071067811865486830, -0.7071067811865464625, -0.000000000000000000 ) ) ;
#32009 = PLANE ( 'NONE',  #127245 ) ;
#32010 = ORIENTED_EDGE ( 'NONE', *, *, #62036, .T. ) ;
#32011 = CARTESIAN_POINT ( 'NONE',  ( 0.000000000000000000, 21.72500000000000142, 4.500000000000000888 ) ) ;
#32012 = ORIENTED_EDGE ( 'NONE', *, *, #60602, .F. ) ;
#32013 = ORIENTED_EDGE ( 'NONE', *, *, #115441, .T. ) ;
#32014 = CARTESIAN_POINT ( 'NONE',  ( 12.48921356237309155, -27.52281430457064104, 5.000000000000000000 ) ) ;
#32015 = ORIENTED_EDGE ( 'NONE', *, *, #107521, .F. ) ;
#32016 = ADVANCED_FACE ( 'NONE', ( #112376 ), #101480, .T. ) ;
#32017 = EDGE_CURVE ( 'NONE', #110484, #114963, #124668, .T. ) ;
#32018 = CARTESIAN_POINT ( 'NONE',  ( 47.74543019189811588, -5.291415217122918513, -3.055000000000000160 ) ) ;
#32019 = VERTEX_POINT ( 'NONE', #34822 ) ;
#32020 = VECTOR ( 'NONE', #64127, 1000.000000000000000 ) ;
#32021 = DIRECTION ( 'NONE',  ( -0.6830127018922181881, 0.6830127018922202975, -0.2588190451025214056 ) ) ;
#32022 = ORIENTED_EDGE ( 'NONE', *, *, #130561, .F. ) ;
#32023 = EDGE_CURVE ( 'NONE', #53028, #41122, #102226, .T. ) ;
#32024 = DIRECTION ( 'NONE',  ( 0.7071067811865487940, 0.7071067811865463515, 0.000000000000000000 ) ) ;
#32025 = ORIENTED_EDGE ( 'NONE', *, *, #80012, .F. ) ;
#32026 = FACE_OUTER_BOUND ( 'NONE', #88600, .T. ) ;
#32027 = CARTESIAN_POINT ( 'NONE',  ( -12.69999999999998153, 3.061616997868383634E-16, -2.500000000000000444 ) ) ;
#32028 = EDGE_CURVE ( 'NONE', #122674, #31094, #57307, .T. ) ;
#32029 = CARTESIAN_POINT ( 'NONE',  ( 12.48921356237309155, -27.52281430457064104, 5.000000000000000000 ) ) ;
#32030 = VECTOR ( 'NONE', #35685, 999.9999999999998863 ) ;
#32031 = FILL_AREA_STYLE ('',( #140102 ) ) ;
#32032 = LINE ( 'NONE', #31330, #34435 ) ;
#32033 = FACE_OUTER_BOUND ( 'NONE', #93599, .T. ) ;
#32034 = CARTESIAN_POINT ( 'NONE',  ( 0.000000000000000000, 0.000000000000000000, 5.000000000000000000 ) ) ;
#32035 = ORIENTED_EDGE ( 'NONE', *, *, #90073, .F. ) ;
#32036 = ORIENTED_EDGE ( 'NONE', *, *, #5644, .T. ) ;
#32037 = ORIENTED_EDGE ( 'NONE', *, *, #96786, .F. ) ;
#32038 = DIRECTION ( 'NONE',  ( -0.7071067811865486830, -0.7071067811865464625, 0.000000000000000000 ) ) ;
#32039 = CIRCLE ( 'NONE', #29739, 2.055000000000001048 ) ;
#32041 = CARTESIAN_POINT ( 'NONE',  ( 42.29974487139158157, -27.71228299555235708, 4.000000000000000000 ) ) ;
#32040 = VECTOR ( 'NONE', #94796, 1000.000000000000000 ) ;
#32042 = ORIENTED_EDGE ( 'NONE', *, *, #71587, .T. ) ;
#32044 = VERTEX_POINT ( 'NONE', #69607 ) ;
#32043 = AXIS2_PLACEMENT_3D ( 'NONE', #87102, #63252, #32000 ) ;
#32045 = LINE ( 'NONE', #128515, #67590 ) ;
#32046 = LINE ( 'NONE', #120435, #15492 ) ;
#32047 = AXIS2_PLACEMENT_3D ( 'NONE', #110319, #119763, #10997 ) ;
#32048 = DIRECTION ( 'NONE',  ( 0.6830127018922180770, -0.6830127018922204085, -0.2588190451025213501 ) ) ;
#32049 = VERTEX_POINT ( 'NONE', #2878 ) ;
#32050 = LINE ( 'NONE', #129942, #41731 ) ;
#32051 = EDGE_CURVE ( 'NONE', #97154, #94686, #704, .T. ) ;
#32052 = CIRCLE ( 'NONE', #68916, 2.500000000000000888 ) ;
#32053 = AXIS2_PLACEMENT_3D ( 'NONE', #126168, #137038, #90698 ) ;
#32054 = LINE ( 'NONE', #32792, #100017 ) ;
#32055 = CARTESIAN_POINT ( 'NONE',  ( 19.31706980810189123, -2.126176841940956130, 7.934999999999991616 ) ) ;
#32056 = DIRECTION ( 'NONE',  ( 0.7071067811865487940, 0.7071067811865463515, 0.000000000000000000 ) ) ;
#32057 = ORIENTED_EDGE ( 'NONE', *, *, #19179, .F. ) ;
#32058 = CARTESIAN_POINT ( 'NONE',  ( 122.8495968585647518, 6.109999999999997655, 1.637169565754163836 ) ) ;
#32059 = DIRECTION ( 'NONE',  ( 0.7071067811865486830, -0.7071067811865464625, -0.000000000000000000 ) ) ;
#32060 = ADVANCED_FACE ( 'NONE', ( #25344 ), #35564, .T. ) ;
#32061 = LINE ( 'NONE', #140129, #68124 ) ;
#32063 = ORIENTED_EDGE ( 'NONE', *, *, #79145, .T. ) ;
#32062 = LINE ( 'NONE', #76295, #56519 ) ;
#32064 = VECTOR ( 'NONE', #100902, 1000.000000000000000 ) ;
#32065 = CARTESIAN_POINT ( 'NONE',  ( 12.29974487139158512, -27.71228299555214747, 4.000000000000000000 ) ) ;
#32066 = ORIENTED_EDGE ( 'NONE', *, *, #32071, .T. ) ;
#32067 = DIRECTION ( 'NONE',  ( -0.000000000000000000, -0.000000000000000000, -1.000000000000000000 ) ) ;
#32068 = DIRECTION ( 'NONE',  ( 0.7071067811865486830, -0.7071067811865464625, -0.000000000000000000 ) ) ;
#32069 = FACE_OUTER_BOUND ( 'NONE', #56395, .T. ) ;
#32070 = ORIENTED_EDGE ( 'NONE', *, *, #137943, .T. ) ;
#32071 = EDGE_CURVE ( 'NONE', #28105, #107272, #75648, .T. ) ;
#32072 = VECTOR ( 'NONE', #111629, 1000.000000000000000 ) ;
#32073 = ADVANCED_FACE ( 'NONE', ( #67469 ), #119820, .F. ) ;
#32074 = CARTESIAN_POINT ( 'NONE',  ( 33.48921356237309510, -27.52281430457078670, 5.000000000000000000 ) ) ;
#32075 = VERTEX_POINT ( 'NONE', #130755 ) ;
#32076 = LINE ( 'NONE', #21193, #29969 ) ;
#32077 = EDGE_CURVE ( 'NONE', #94490, #123567, #131454, .T. ) ;
#32080 = EDGE_CURVE ( 'NONE', #90720, #11113, #108947, .T. ) ;
#32079 = VECTOR ( 'NONE', #31041, 1000.000000000000000 ) ;
#32078 = CARTESIAN_POINT ( 'NONE',  ( -23.67183060077630685, 11.25929247661559884, 4.000000000000000000 ) ) ;
#32081 = ORIENTED_EDGE ( 'NONE', *, *, #66902, .F. ) ;
#32082 = VECTOR ( 'NONE', #53627, 1000.000000000000000 ) ;
#32083 = FACE_OUTER_BOUND ( 'NONE', #49987, .T. ) ;
#32085 = EDGE_LOOP ( 'NONE', ( #107349, #66560, #38828, #120370 ) ) ;
#32084 = DIRECTION ( 'NONE',  ( 2.781805975412905274E-17, -0.3543493200069152138, 0.9351131265310292928 ) ) ;
#32086 = EDGE_LOOP ( 'NONE', ( #118639, #119077, #3363, #19241 ) ) ;
#32087 = CARTESIAN_POINT ( 'NONE',  ( -31.49999999999977973, 18.05218569542898521, 5.000000000000000000 ) ) ;
#32088 = CARTESIAN_POINT ( 'NONE',  ( -22.49999999999984013, 10.46639925780215208, 5.000000000000000000 ) ) ;
#32089 = ORIENTED_EDGE ( 'NONE', *, *, #19935, .F. ) ;
#32090 = LINE ( 'NONE', #54575, #112987 ) ;
#32091 = CARTESIAN_POINT ( 'NONE',  ( 6.707106781186501721, 2.259292476615694323, 5.000000000000000000 ) ) ;
#32092 = CARTESIAN_POINT ( 'NONE',  ( 124.0375270504628986, -9.735942053221456900E-16, 7.949999999999998401 ) ) ;
#32093 = ORIENTED_EDGE ( 'NONE', *, *, #120742, .T. ) ;
#32094 = EDGE_CURVE ( 'NONE', #34100, #43661, #7358, .T. ) ;
#32095 = DIRECTION ( 'NONE',  ( -0.6830127018922180770, -0.6830127018922204085, -0.2588190451025213501 ) ) ;
#32096 = CARTESIAN_POINT ( 'NONE',  ( -22.49999999999983302, -17.94781430457063820, 5.000000000000000000 ) ) ;
#32097 = DIRECTION ( 'NONE',  ( 0.7071067811865486830, -0.7071067811865464625, -0.000000000000000000 ) ) ;
#32098 = VECTOR ( 'NONE', #37424, 1000.000000000000227 ) ;
#32099 = LINE ( 'NONE', #66172, #39031 ) ;
#32100 = CARTESIAN_POINT ( 'NONE',  ( 39.14126352523145869, 4.472830434245837594, 4.472830434245841147 ) ) ;
#32101 = DIRECTION ( 'NONE',  ( -1.000000000000000000, -1.224606353822377258E-16, -0.000000000000000000 ) ) ;
#32102 = EDGE_LOOP ( 'NONE', ( #85745, #27588, #7246, #3780 ) ) ;
#32103 = VERTEX_POINT ( 'NONE', #12328 ) ;
#32104 = CARTESIAN_POINT ( 'NONE',  ( 126.7083333333333428, -3.974999999999999201, -6.884901960086287964 ) ) ;
#32105 = EDGE_CURVE ( 'NONE', #139444, #114640, #100778, .T. ) ;
#32106 = ORIENTED_EDGE ( 'NONE', *, *, #29253, .T. ) ;
#32107 = EDGE_LOOP ( 'NONE', ( #27687, #74232, #123213, #54892 ) ) ;
#32108 = CARTESIAN_POINT ( 'NONE',  ( 19.05000000000000071, 3.174999999999997158, 4.000000000000000000 ) ) ;
#32109 = FACE_OUTER_BOUND ( 'NONE', #97837, .T. ) ;
#32110 = ORIENTED_EDGE ( 'NONE', *, *, #91077, .F. ) ;
#32111 = PLANE ( 'NONE',  #141124 ) ;
#32112 = LINE ( 'NONE', #85767, #60522 ) ;
#32113 = PLANE ( 'NONE',  #39463 ) ;
#32114 = EDGE_CURVE ( 'NONE', #105061, #140051, #89888, .T. ) ;
#32115 = DIRECTION ( 'NONE',  ( 0.7071067811865487940, -0.7071067811865463515, 0.000000000000000000 ) ) ;
#32116 = DIRECTION ( 'NONE',  ( 0.5735764363510451602, 0.8191520442889924647, 0.000000000000000000 ) ) ;
#32117 = VERTEX_POINT ( 'NONE', #79067 ) ;
#32118 = CARTESIAN_POINT ( 'NONE',  ( 18.18398860626898994, 28.73617430169800002, 5.000000000000000000 ) ) ;
#32119 = LINE ( 'NONE', #76345, #74684 ) ;
#32120 = LINE ( 'NONE', #18346, #19508 ) ;
#32121 = CARTESIAN_POINT ( 'NONE',  ( 15.18398860626900237, 28.73617430169797871, 5.000000000000000000 ) ) ;
#32122 = DIRECTION ( 'NONE',  ( 1.000000000000000000, 0.000000000000000000, -0.000000000000000000 ) ) ;
#32123 = DIRECTION ( 'NONE',  ( 1.734723475976806848E-16, -1.000000000000000000, 0.000000000000000000 ) ) ;
#32124 = CARTESIAN_POINT ( 'NONE',  ( 56.07919371712956291, 3.975000000000002753, -6.884901960086283523 ) ) ;
#32125 = CARTESIAN_POINT ( 'NONE',  ( 34.92499999999998295, -21.72500000000000142, 5.000000000000000000 ) ) ;
#32126 = FACE_OUTER_BOUND ( 'NONE', #48259, .T. ) ;
#32127 = ORIENTED_EDGE ( 'NONE', *, *, #117510, .T. ) ;
#32128 = VERTEX_POINT ( 'NONE', #134868 ) ;
#32129 = CARTESIAN_POINT ( 'NONE',  ( 59.47916666666666430, -7.950000000000001066, 2.130196079827424427 ) ) ;
#32130 = LINE ( 'NONE', #141616, #139641 ) ;
#32131 = DIRECTION ( 'NONE',  ( 0.6830127018922181881, 0.6830127018922202975, -0.2588190451025214056 ) ) ;
#32132 = LINE ( 'NONE', #174, #13713 ) ;
#32133 = ORIENTED_EDGE ( 'NONE', *, *, #72187, .T. ) ;
#32134 = DIRECTION ( 'NONE',  ( 0.7071067811865487940, 0.7071067811865463515, 0.000000000000000000 ) ) ;
#32135 = FACE_OUTER_BOUND ( 'NONE', #90230, .T. ) ;
#32136 = EDGE_CURVE ( 'NONE', #77708, #107149, #32130, .T. ) ;
#32137 = CIRCLE ( 'NONE', #4318, 2.500000000000000444 ) ;
#32138 = CARTESIAN_POINT ( 'NONE',  ( 47.54209685856476852, 5.291415217122923842, -3.054999999999996163 ) ) ;
#32139 = ORIENTED_EDGE ( 'NONE', *, *, #10062, .F. ) ;
#32140 = DIRECTION ( 'NONE',  ( 0.7071067811865487940, 0.7071067811865463515, 0.000000000000000000 ) ) ;
#32141 = ORIENTED_EDGE ( 'NONE', *, *, #42234, .F. ) ;
#32142 = ORIENTED_EDGE ( 'NONE', *, *, #96731, .F. ) ;
#32143 = DIRECTION ( 'NONE',  ( 0.6830127018922181881, 0.6830127018922202975, -0.2588190451025214056 ) ) ;
#32144 = VECTOR ( 'NONE', #53221, 1000.000000000000227 ) ;
#32145 = VECTOR ( 'NONE', #38854, 1000.000000000000000 ) ;
#32146 = VECTOR ( 'NONE', #134921, 1000.000000000000000 ) ;
#32147 = CARTESIAN_POINT ( 'NONE',  ( 81.74586038379622721, 3.974999999999996980, 6.884901960086287964 ) ) ;
#32148 = CARTESIAN_POINT ( 'NONE',  ( -30.48921356237309510, -27.52281430457076894, 5.000000000000000000 ) ) ;
#32149 = VECTOR ( 'NONE', #91401, 1000.000000000000000 ) ;
#32150 = CARTESIAN_POINT ( 'NONE',  ( 29.20710678118633652, -14.24070752338414181, 5.000000000000000000 ) ) ;
#32151 = ORIENTED_EDGE ( 'NONE', *, *, #87078, .F. ) ;
#32152 = EDGE_CURVE ( 'NONE', #25969, #10888, #42319, .T. ) ;
#32153 = DIRECTION ( 'NONE',  ( -1.000000000000000000, -1.224606353822377258E-16, -0.000000000000000000 ) ) ;
#32154 = ORIENTED_EDGE ( 'NONE', *, *, #105710, .F. ) ;
#32155 = CARTESIAN_POINT ( 'NONE',  ( 79.04209685856477563, 5.291415217122923842, -3.054999999999996163 ) ) ;
#32156 = DIRECTION ( 'NONE',  ( -1.000000000000000000, -1.224606353822377258E-16, -0.000000000000000000 ) ) ;
#32157 = SURFACE_SIDE_STYLE ('',( #930 ) ) ;
#32158 = CARTESIAN_POINT ( 'NONE',  ( 16.49999999999988276, -9.462702396500995761, -9.474982329943555825 ) ) ;
#32159 = LINE ( 'NONE', #77814, #11300 ) ;
#32160 = VECTOR ( 'NONE', #37314, 1000.000000000000000 ) ;
#32161 = EDGE_LOOP ( 'NONE', ( #904, #100903, #95771, #143289 ) ) ;
#32162 = CYLINDRICAL_SURFACE ( 'NONE', #43025, 5.968999999999998529 ) ;
#32163 = CARTESIAN_POINT ( 'NONE',  ( 69.62043019189812298, 3.055000000000001936, -5.291415217122916737 ) ) ;
#32164 = FACE_OUTER_BOUND ( 'NONE', #127116, .T. ) ;
#32165 = B_SPLINE_CURVE_WITH_KNOTS ( 'NONE', 3,
 ( #126700, #49189, #60799, #5627 ),
 .UNSPECIFIED., .F., .F.,
 ( 4, 4 ),
 ( 0.000000000000000000, 0.001115544020566805418 ),
 .UNSPECIFIED. ) ;
#32166 = DIRECTION ( 'NONE',  ( 0.3543493200069162685, -0.000000000000000000, -0.9351131265310288487 ) ) ;
#32167 = LINE ( 'NONE', #132944, #34034 ) ;
#32168 = ORIENTED_EDGE ( 'NONE', *, *, #130652, .F. ) ;
#32169 = VERTEX_POINT ( 'NONE', #24636 ) ;
#32170 = AXIS2_PLACEMENT_3D ( 'NONE', #116774, #105873, #70476 ) ;
#32171 = AXIS2_PLACEMENT_3D ( 'NONE', #74218, #51042, #117674 ) ;
#32172 = CYLINDRICAL_SURFACE ( 'NONE', #79322, 7.950000000000000178 ) ;
#32173 = ORIENTED_EDGE ( 'NONE', *, *, #6741, .T. ) ;
#32174 = ORIENTED_EDGE ( 'NONE', *, *, #105058, .T. ) ;
#32175 = STYLED_ITEM ( 'NONE', ( #93974 ), #95871 ) ;
#32176 = CARTESIAN_POINT ( 'NONE',  ( 17.81601139373099940, 28.73617430169775133, 5.000000000000000000 ) ) ;
#32177 = ORIENTED_EDGE ( 'NONE', *, *, #93592, .T. ) ;
#32178 = FACE_OUTER_BOUND ( 'NONE', #45309, .T. ) ;
#32179 = DIRECTION ( 'NONE',  ( -0.7071067811865487940, 0.7071067811865463515, 0.000000000000000000 ) ) ;
#32180 = EDGE_CURVE ( 'NONE', #13816, #49354, #66668, .T. ) ;
#32181 = VECTOR ( 'NONE', #30916, 1000.000000000000000 ) ;
#32182 = AXIS2_PLACEMENT_3D ( 'NONE', #65679, #77254, #54767 ) ;
#32184 = VECTOR ( 'NONE', #28725, 1000.000000000000000 ) ;
#32183 = PLANE ( 'NONE',  #41897 ) ;
#32185 = FACE_BOUND ( 'NONE', #140548, .T. ) ;
#32186 = CARTESIAN_POINT ( 'NONE',  ( 15.05159235450332034, 2.500000000000001332, 0.000000000000000000 ) ) ;
#32187 = ADVANCED_FACE ( 'NONE', ( #135563 ), #81183, .F. ) ;
#32188 = LINE ( 'NONE', #43081, #106823 ) ;
#32189 = CARTESIAN_POINT ( 'NONE',  ( 2.442822804234946688, -22.22500000000000142, 19.16006494309459285 ) ) ;
#32191 = VERTEX_POINT ( 'NONE', #59447 ) ;
#32190 = CARTESIAN_POINT ( 'NONE',  ( 51.55836038379622011, -7.949999999999996625, -2.130196079827426203 ) ) ;
#32192 = COLOUR_RGB ( '', 0.40784314, 0.44705882, 0.49803922) ;
#32193 = VECTOR ( 'NONE', #29688, 1000.000000000000000 ) ;
#32194 = DIRECTION ( 'NONE',  ( 0.7071067811865486830, -0.7071067811865464625, -0.000000000000000000 ) ) ;
#32195 = ORIENTED_EDGE ( 'NONE', *, *, #134026, .T. ) ;
#32196 = EDGE_CURVE ( 'NONE', #73650, #23831, #4982, .T. ) ;
#32197 = EDGE_CURVE ( 'NONE', #143191, #47477, #70340, .T. ) ;
#32198 = ORIENTED_EDGE ( 'NONE', *, *, #118453, .F. ) ;
#32199 = CARTESIAN_POINT ( 'NONE',  ( 87.12043019189812298, 3.055000000000001936, -5.291415217122916737 ) ) ;
#32200 = VERTEX_POINT ( 'NONE', #127519 ) ;
#32201 = ADVANCED_FACE ( 'NONE', ( #49979 ), #84053, .F. ) ;
#32202 = DIRECTION ( 'NONE',  ( -1.000000000000000000, -1.224606353822377258E-16, -0.000000000000000000 ) ) ;
#32203 = ADVANCED_FACE ( 'NONE', ( #28924 ), #4241, .T. ) ;
#32204 = ORIENTED_EDGE ( 'NONE', *, *, #92887, .T. ) ;
#32205 = CARTESIAN_POINT ( 'NONE',  ( 25.00000000000000000, 0.000000000000000000, 0.000000000000000000 ) ) ;
#32206 = VECTOR ( 'NONE', #97795, 1000.000000000000000 ) ;
#32207 = ADVANCED_FACE ( 'NONE', ( #115176 ), #94162, .F. ) ;
#32208 = LINE ( 'NONE', #119196, #37896 ) ;
#32209 = CARTESIAN_POINT ( 'NONE',  ( -25.39999999999996305, 0.000000000000000000, 0.000000000000000000 ) ) ;
#32210 = EDGE_CURVE ( 'NONE', #111562, #37040, #116640, .T. ) ;
#32211 = CARTESIAN_POINT ( 'NONE',  ( 2.999999999999999112, -7.600000000000061817, 28.92499999999998650 ) ) ;
#32212 = CARTESIAN_POINT ( 'NONE',  ( -19.49999999999986500, -14.70932175296479549, -11.46312253303832840 ) ) ;
#32213 = DIRECTION ( 'NONE',  ( 0.000000000000000000, 0.000000000000000000, 1.000000000000000000 ) ) ;
#32214 = DIRECTION ( 'NONE',  ( 0.7071067811865487940, 0.7071067811865463515, 0.000000000000000000 ) ) ;
#32215 = PLANE ( 'NONE',  #67130 ) ;
#32216 = ORIENTED_EDGE ( 'NONE', *, *, #121014, .T. ) ;
#32217 = FILL_AREA_STYLE ('',( #131527 ) ) ;
#32218 = VERTEX_POINT ( 'NONE', #115895 ) ;
#32219 = CARTESIAN_POINT ( 'NONE',  ( 124.0375270504628986, -9.735942053221456900E-16, 7.949999999999998401 ) ) ;
#32220 = CARTESIAN_POINT ( 'NONE',  ( 7.001930566820925961, -22.22500000000000142, 4.500000000000000888 ) ) ;
#32221 = EDGE_CURVE ( 'NONE', #101064, #71067, #17325, .T. ) ;
#32222 = VERTEX_POINT ( 'NONE', #27473 ) ;
#32223 = ORIENTED_EDGE ( 'NONE', *, *, #115909, .T. ) ;
#32224 = CARTESIAN_POINT ( 'NONE',  ( 34.56293019189809712, 1.637169565754157174, 6.110000000000002984 ) ) ;
#32225 = ORIENTED_EDGE ( 'NONE', *, *, #33764, .F. ) ;
#32226 = LINE ( 'NONE', #65608, #81068 ) ;
#32227 = ADVANCED_FACE ( 'NONE', ( #15852 ), #37682, .T. ) ;
#32228 = CARTESIAN_POINT ( 'NONE',  ( 90.35002705046288440, -5.819803920172573086, -5.819803920172573086 ) ) ;
#32229 = CARTESIAN_POINT ( 'NONE',  ( 20.60830628287043709, 1.633150327867687324, -6.094999999999991758 ) ) ;
#32230 = CARTESIAN_POINT ( 'NONE',  ( -5.385325943209082311, 13.08800193907929277, -24.86884355624839316 ) ) ;
#32231 = ORIENTED_EDGE ( 'NONE', *, *, #35765, .F. ) ;
#32232 = CARTESIAN_POINT ( 'NONE',  ( 0.000000000000000000, 0.000000000000000000, 0.000000000000000000 ) ) ;
#32233 = ORIENTED_EDGE ( 'NONE', *, *, #86515, .T. ) ;
#32234 = DIRECTION ( 'NONE',  ( 0.000000000000000000, 0.3543493200069153248, 0.9351131265310291818 ) ) ;
#32235 = DIRECTION ( 'NONE',  ( 0.7071067811865487940, 0.7071067811865463515, 0.000000000000000000 ) ) ;
#32237 = ORIENTED_EDGE ( 'NONE', *, *, #36274, .T. ) ;
#32236 = CARTESIAN_POINT ( 'NONE',  ( 0.000000000000000000, 7.776507174585692163E-16, -6.349999999999999645 ) ) ;
#32238 = EDGE_LOOP ( 'NONE', ( #59879, #52037, #114555, #26943 ) ) ;
#32239 = CARTESIAN_POINT ( 'NONE',  ( 5.671830600776432973, 8.259292476615636147, 4.000000000000000000 ) ) ;
#32240 = CARTESIAN_POINT ( 'NONE',  ( 2.999999999999978240, -3.485240976185077777, -4.108735105802389320 ) ) ;
#32241 = CARTESIAN_POINT ( 'NONE',  ( -2.999999999999975131, -3.412538124160726660, 4.000000000000000000 ) ) ;
#32242 = ORIENTED_EDGE ( 'NONE', *, *, #63225, .T. ) ;
#32243 = LINE ( 'NONE', #85901, #96679 ) ;
#32244 = ORIENTED_EDGE ( 'NONE', *, *, #13956, .T. ) ;
#32245 = ORIENTED_EDGE ( 'NONE', *, *, #131407, .F. ) ;
#32246 = ORIENTED_EDGE ( 'NONE', *, *, #125707, .T. ) ;
#32247 = ADVANCED_FACE ( 'NONE', ( #105735 ), #104314, .T. ) ;
#32248 = DIRECTION ( 'NONE',  ( 0.000000000000000000, -1.000000000000000000, 0.000000000000000000 ) ) ;
#32249 = CARTESIAN_POINT ( 'NONE',  ( -9.183988606268997046, 28.73617430169793607, 5.000000000000000000 ) ) ;
#32250 = STYLED_ITEM ( 'NONE', ( #38454 ), #70028 ) ;
#32251 = VECTOR ( 'NONE', #35870, 1000.000000000000000 ) ;
#32252 = VECTOR ( 'NONE', #25000, 1000.000000000000000 ) ;
#32253 = FACE_OUTER_BOUND ( 'NONE', #50929, .T. ) ;
#32254 = DIRECTION ( 'NONE',  ( 0.7071067811865487940, -0.7071067811865463515, 0.000000000000000000 ) ) ;
#32256 = ADVANCED_FACE ( 'NONE', ( #102926 ), #93469, .F. ) ;
#32255 =( BOUNDED_CURVE ( )  B_SPLINE_CURVE ( 3, ( #2364, #58984, #80695, #23428 ),
 .UNSPECIFIED., .F., .T. ) 
 B_SPLINE_CURVE_WITH_KNOTS ( ( 4, 4 ),
 ( 2.779374508378133601, 4.199602562396782091 ),
 .UNSPECIFIED. ) 
 CURVE ( )  GEOMETRIC_REPRESENTATION_ITEM ( )  RATIONAL_B_SPLINE_CURVE ( ( 1.000000000000000000, 0.8388583629366748173, 0.8388583629366748173, 1.000000000000000000 ) ) 
 REPRESENTATION_ITEM ( '' )  );
#32257 = FACE_OUTER_BOUND ( 'NONE', #5173, .T. ) ;
#32258 = VECTOR ( 'NONE', #9898, 1000.000000000000000 ) ;
#32259 = CARTESIAN_POINT ( 'NONE',  ( -6.299744871391586898, -27.71228299555210484, 4.000000000000000000 ) ) ;
#32260 = DIRECTION ( 'NONE',  ( -0.7071067811865486830, -0.7071067811865464625, 0.000000000000000000 ) ) ;
#32261 = ORIENTED_EDGE ( 'NONE', *, *, #92935, .T. ) ;
#32262 = LINE ( 'NONE', #110497, #125343 ) ;
#32263 = ORIENTED_EDGE ( 'NONE', *, *, #118281, .F. ) ;
#32264 = VECTOR ( 'NONE', #96588, 1000.000000000000000 ) ;
#32265 = CARTESIAN_POINT ( 'NONE',  ( 6.792893218813411238, 6.759292476615645029, 5.000000000000000000 ) ) ;
#32266 = ADVANCED_FACE ( 'NONE', ( #92028 ), #136250, .T. ) ;
#32267 = CARTESIAN_POINT ( 'NONE',  ( 0.000000000000000000, 5.495644160703818878E-16, 4.487534009422227577 ) ) ;
#32268 = CARTESIAN_POINT ( 'NONE',  ( -45.48921356237309510, -27.52281430457087197, 5.000000000000000000 ) ) ;
#32269 = EDGE_LOOP ( 'NONE', ( #128859, #56317, #17433, #45860 ) ) ;
#32270 = CARTESIAN_POINT ( 'NONE',  ( -23.99999999999982592, 20.96639925780204550, 5.000000000000000000 ) ) ;
#32271 = CARTESIAN_POINT ( 'NONE',  ( 20.99999999999986500, 14.87792677143811026, -11.06722581663435356 ) ) ;
#32272 = CARTESIAN_POINT ( 'NONE',  ( 9.707106781186480404, 17.25929247661554911, 5.000000000000000000 ) ) ;
#32273 = EDGE_LOOP ( 'NONE', ( #48181, #112492, #117656, #44344 ) ) ;
#32274 = ORIENTED_EDGE ( 'NONE', *, *, #3520, .T. ) ;
#32275 = EDGE_CURVE ( 'NONE', #46867, #120251, #15166, .T. ) ;
#32276 = DIRECTION ( 'NONE',  ( 0.000000000000000000, -1.000000000000000000, 0.000000000000000000 ) ) ;
#32277 = DIRECTION ( 'NONE',  ( -1.000000000000000000, 0.000000000000000000, 0.000000000000000000 ) ) ;
#32278 = DIRECTION ( 'NONE',  ( 0.7071067811865487940, -0.7071067811865463515, 0.000000000000000000 ) ) ;
#32279 = AXIS2_PLACEMENT_3D ( 'NONE', #43722, #67655, #142341 ) ;
#32280 = CARTESIAN_POINT ( 'NONE',  ( 28.00000000000002487, -52.14999999999999147, -34.92499999999976978 ) ) ;
#32281 = LINE ( 'NONE', #89502, #13440 ) ;
#32282 = CARTESIAN_POINT ( 'NONE',  ( 68.59959685856476597, -6.109999999999998543, -1.637169565754160727 ) ) ;
#32283 = CARTESIAN_POINT ( 'NONE',  ( 7.171830600776424092, -20.24070752338407431, 4.000000000000000000 ) ) ;
#32285 = DIRECTION ( 'NONE',  ( -0.000000000000000000, -0.3543493200069152693, 0.9351131265310292928 ) ) ;
#32284 = AXIS2_PLACEMENT_3D ( 'NONE', #68368, #78495, #21956 ) ;
#32286 = DIRECTION ( 'NONE',  ( 0.7071067811865487940, 0.7071067811865463515, 0.000000000000000000 ) ) ;
#32287 = CARTESIAN_POINT ( 'NONE',  ( -34.42499999999997584, -22.26999999999999247, -37.00000000000000000 ) ) ;
#32288 = VERTEX_POINT ( 'NONE', #38378 ) ;
#32289 = LINE ( 'NONE', #76521, #83512 ) ;
#32290 = VERTEX_POINT ( 'NONE', #71736 ) ;
#32291 = CARTESIAN_POINT ( 'NONE',  ( 12.32816939922343913, -6.740707523384219968, 4.000000000000000000 ) ) ;
#32292 = ORIENTED_EDGE ( 'NONE', *, *, #100702, .F. ) ;
#32293 = VECTOR ( 'NONE', #118257, 999.9999999999998863 ) ;
#32294 = VECTOR ( 'NONE', #61393, 1000.000000000000000 ) ;
#32295 = VECTOR ( 'NONE', #66009, 1000.000000000000000 ) ;
#32296 = CARTESIAN_POINT ( 'NONE',  ( -3.469446951953614189E-15, -13.06887692260767864, 4.000000000000000000 ) ) ;
#32297 = CARTESIAN_POINT ( 'NONE',  ( -30.81323691877862458, -22.22500000000000142, 6.558100737250206258 ) ) ;
#32298 = EDGE_CURVE ( 'NONE', #113508, #36808, #53953, .T. ) ;
#32299 = DIRECTION ( 'NONE',  ( -0.7071067811865486830, -0.7071067811865464625, 0.000000000000000000 ) ) ;
#32300 = CARTESIAN_POINT ( 'NONE',  ( 152.4000000000000057, 25.96999999999993847, 33.92499999999998295 ) ) ;
#32301 = EDGE_CURVE ( 'NONE', #121901, #38643, #7122, .T. ) ;
#32302 = ORIENTED_EDGE ( 'NONE', *, *, #141353, .F. ) ;
#32303 = VECTOR ( 'NONE', #29255, 1000.000000000000000 ) ;
#32304 = EDGE_LOOP ( 'NONE', ( #3719, #75236, #61506, #92929 ) ) ;
#32305 = CARTESIAN_POINT ( 'NONE',  ( 24.48921356237309510, -27.52281430457072631, 5.000000000000000000 ) ) ;
#32306 = CARTESIAN_POINT ( 'NONE',  ( -36.48921356237310221, -27.52281430457080802, 5.000000000000000000 ) ) ;
#32307 = VECTOR ( 'NONE', #115694, 1000.000000000000000 ) ;
#32308 = AXIS2_PLACEMENT_3D ( 'NONE', #66134, #66833, #89292 ) ;
#32309 = LINE ( 'NONE', #54779, #93618 ) ;
#32310 = CARTESIAN_POINT ( 'NONE',  ( 26.12840764549667583, 9.139736423841732040E-16, 0.000000000000000000 ) ) ;
#32311 = CARTESIAN_POINT ( 'NONE',  ( 83.05836038379621300, -7.949999999999997513, -2.130196079827425759 ) ) ;
#32312 = DIRECTION ( 'NONE',  ( -0.7071067811865487940, 0.7071067811865463515, 0.000000000000000000 ) ) ;
#32313 = DIRECTION ( 'NONE',  ( -0.7071067811865487940, 0.7071067811865463515, 0.000000000000000000 ) ) ;
#32314 = ORIENTED_EDGE ( 'NONE', *, *, #48558, .T. ) ;
#32315 = CARTESIAN_POINT ( 'NONE',  ( 83.54166666666667140, -3.975000000000002753, 6.884901960086286188 ) ) ;
#32316 = CARTESIAN_POINT ( 'NONE',  ( -65.99451991528749772, 28.92564299267984396, 4.000000000000000000 ) ) ;
#32317 = CARTESIAN_POINT ( 'NONE',  ( 42.48921356237308800, -27.52281430457085065, 5.000000000000000000 ) ) ;
#32318 = CARTESIAN_POINT ( 'NONE',  ( 78.53752705046289861, -9.735942053221456900E-16, 7.949999999999998401 ) ) ;
#32319 =( GEOMETRIC_REPRESENTATION_CONTEXT ( 3 ) GLOBAL_UNCERTAINTY_ASSIGNED_CONTEXT ( ( #115862 ) ) GLOBAL_UNIT_ASSIGNED_CONTEXT ( ( #13359, #112004, #142491 ) ) REPRESENTATION_CONTEXT ( 'NONE', 'WORKASPACE' ) );
#32320 = ORIENTED_EDGE ( 'NONE', *, *, #135915, .F. ) ;
#32321 = DIRECTION ( 'NONE',  ( 1.000000000000000000, 0.000000000000000000, 0.000000000000000000 ) ) ;
#32322 = ORIENTED_EDGE ( 'NONE', *, *, #142994, .F. ) ;
#32323 = ADVANCED_FACE ( 'NONE', ( #98457 ), #118773, .T. ) ;
#32324 = CARTESIAN_POINT ( 'NONE',  ( 74.81293019189809002, -1.637169565754159617, -6.110000000000001208 ) ) ;
#32325 = FACE_OUTER_BOUND ( 'NONE', #7197, .T. ) ;
#32326 = ORIENTED_EDGE ( 'NONE', *, *, #136662, .F. ) ;
#32327 = DIRECTION ( 'NONE',  ( 0.000000000000000000, -1.000000000000000000, 0.000000000000000000 ) ) ;
#32328 = CARTESIAN_POINT ( 'NONE',  ( 0.000000000000000000, 0.000000000000000000, 5.000000000000000000 ) ) ;
#32329 = DIRECTION ( 'NONE',  ( 1.000000000000000000, 0.000000000000000000, 0.000000000000000000 ) ) ;
#32330 = CARTESIAN_POINT ( 'NONE',  ( -8.999999999999934275, 1.552185695429156187, 5.000000000000000000 ) ) ;
#32331 = EDGE_CURVE ( 'NONE', #108896, #33283, #129647, .T. ) ;
#32332 = CARTESIAN_POINT ( 'NONE',  ( 55.56056557994608625, -52.00875322212550600, 39.86617647058822200 ) ) ;
#32334 = EDGE_LOOP ( 'NONE', ( #44962, #90749, #134060, #36809 ) ) ;
#32333 = CARTESIAN_POINT ( 'NONE',  ( 34.42499999999998295, -3.022814304570575761, 5.000000000000000000 ) ) ;
#32335 = DIRECTION ( 'NONE',  ( -0.6830127018922180770, -0.6830127018922204085, -0.2588190451025213501 ) ) ;
#32336 = DIRECTION ( 'NONE',  ( -1.000000000000000000, -1.224606353822377258E-16, -0.000000000000000000 ) ) ;
#32337 = DIRECTION ( 'NONE',  ( 0.3543493200069162685, -0.000000000000000000, -0.9351131265310288487 ) ) ;
#32338 = DIRECTION ( 'NONE',  ( -0.7071067811865487940, 0.7071067811865463515, -0.000000000000000000 ) ) ;
#32339 = EDGE_LOOP ( 'NONE', ( #43489, #95086, #84490, #39937 ) ) ;
#32340 = EDGE_LOOP ( 'NONE', ( #109656, #24891, #136018, #110837 ) ) ;
#32341 = CARTESIAN_POINT ( 'NONE',  ( 65.77126352523144703, 4.472830434245839371, 4.472830434245842035 ) ) ;
#32342 = EDGE_LOOP ( 'NONE', ( #14189, #5938, #66972, #109698 ) ) ;
#32343 = LINE ( 'NONE', #109893, #3539 ) ;
#32344 = CARTESIAN_POINT ( 'NONE',  ( 11.99999999999992006, -6.108550654416948333, -3.114665004254939973 ) ) ;
#32345 = LINE ( 'NONE', #96142, #24911 ) ;
#32346 = FILL_AREA_STYLE ('',( #21467 ) ) ;
#32347 = EDGE_LOOP ( 'NONE', ( #92425, #87650, #101324 ) ) ;
#32348 = VERTEX_POINT ( 'NONE', #86880 ) ;
#32349 = CARTESIAN_POINT ( 'NONE',  ( -11.99999999999991296, -9.033600742197648970, 5.000000000000000000 ) ) ;
#32350 = CARTESIAN_POINT ( 'NONE',  ( 1.500000000000000000, 0.000000000000000000, 0.000000000000000000 ) ) ;
#32351 = ORIENTED_EDGE ( 'NONE', *, *, #63274, .F. ) ;
#32352 = CARTESIAN_POINT ( 'NONE',  ( 1.828169399223512848, -17.24070752338410983, 4.000000000000000000 ) ) ;
#32353 = DIRECTION ( 'NONE',  ( 0.7071067811865486830, -0.7071067811865464625, -0.000000000000000000 ) ) ;
#32354 = DIRECTION ( 'NONE',  ( 1.000000000000000000, 1.224606353822377258E-16, 0.000000000000000000 ) ) ;
#32355 = VECTOR ( 'NONE', #20261, 999.9999999999998863 ) ;
#32356 = VECTOR ( 'NONE', #77742, 1000.000000000000000 ) ;
#32357 = VECTOR ( 'NONE', #69092, 1000.000000000000227 ) ;
#32358 = ORIENTED_EDGE ( 'NONE', *, *, #132781, .F. ) ;
#32359 = AXIS2_PLACEMENT_3D ( 'NONE', #94591, #60597, #82324 ) ;
#32360 = FACE_BOUND ( 'NONE', #100645, .T. ) ;
#32361 = LINE ( 'NONE', #63593, #8394 ) ;
#32362 = CARTESIAN_POINT ( 'NONE',  ( -27.32816939922334143, 20.25929247661551003, 4.000000000000000000 ) ) ;
#32363 = CARTESIAN_POINT ( 'NONE',  ( 61.08333333333332149, 6.884901960086290629, -3.974999999999994316 ) ) ;
#32364 = AXIS2_PLACEMENT_3D ( 'NONE', #136941, #37653, #71702 ) ;
#32365 = LINE ( 'NONE', #86755, #59699 ) ;
#32366 = CARTESIAN_POINT ( 'NONE',  ( 0.000000000000000000, -0.6000000000000000888, 3.054668707061620747 ) ) ;
#32367 =( NAMED_UNIT ( * ) SI_UNIT ( $, .STERADIAN. ) SOLID_ANGLE_UNIT ( ) );
#32368 = ORIENTED_EDGE ( 'NONE', *, *, #8124, .F. ) ;
#32369 = EDGE_CURVE ( 'NONE', #86631, #84615, #74588, .T. ) ;
#32370 = VECTOR ( 'NONE', #57595, 1000.000000000000000 ) ;
#32371 = ORIENTED_EDGE ( 'NONE', *, *, #34294, .T. ) ;
#32372 = CARTESIAN_POINT ( 'NONE',  ( 108.2662635252314374, 4.472830434245838482, -4.472830434245837594 ) ) ;
#32373 =( BOUNDED_CURVE ( )  B_SPLINE_CURVE ( 3, ( #75391, #119564, #139238, #18101 ),
 .UNSPECIFIED., .F., .T. ) 
 B_SPLINE_CURVE_WITH_KNOTS ( ( 4, 4 ),
 ( 3.334020839929785929, 3.401188224464155585 ),
 .UNSPECIFIED. ) 
 CURVE ( )  GEOMETRIC_REPRESENTATION_ITEM ( )  RATIONAL_B_SPLINE_CURVE ( ( 1.000000000000000000, 0.9996240805387412998, 0.9996240805387412998, 1.000000000000000000 ) ) 
 REPRESENTATION_ITEM ( '' )  );
#32374 = ORIENTED_EDGE ( 'NONE', *, *, #99072, .T. ) ;
#32375 = ADVANCED_FACE ( 'NONE', ( #97746 ), #119466, .F. ) ;
#32376 = EDGE_CURVE ( 'NONE', #66690, #96412, #84728, .T. ) ;
#32377 = ORIENTED_EDGE ( 'NONE', *, *, #71274, .F. ) ;
#32378 = ADVANCED_FACE ( 'NONE', ( #141237 ), #53535, .T. ) ;
#32379 = AXIS2_PLACEMENT_3D ( 'NONE', #48009, #125562, #92179 ) ;
#32380 = EDGE_CURVE ( 'NONE', #74861, #63837, #42708, .T. ) ;
#32381 = DIRECTION ( 'NONE',  ( -0.7071067811865486830, -0.7071067811865464625, -0.000000000000000000 ) ) ;
#32382 = VECTOR ( 'NONE', #24462, 1000.000000000000000 ) ;
#32383 = PLANE ( 'NONE',  #63657 ) ;
#32384 = ORIENTED_EDGE ( 'NONE', *, *, #54317, .T. ) ;
#32385 = DIRECTION ( 'NONE',  ( 0.7071067811865487940, -0.7071067811865463515, 0.000000000000000000 ) ) ;
#32386 = LINE ( 'NONE', #107070, #114377 ) ;
#32387 = EDGE_CURVE ( 'NONE', #5277, #79775, #86531, .T. ) ;
#32388 = CARTESIAN_POINT ( 'NONE',  ( 0.000000000000000000, 1.931123077392161935, 4.000000000000000000 ) ) ;
#32389 = DIRECTION ( 'NONE',  ( -0.000000000000000000, -1.000000000000000000, -0.000000000000000000 ) ) ;
#32390 = VECTOR ( 'NONE', #55517, 1000.000000000000227 ) ;
#32391 = FACE_OUTER_BOUND ( 'NONE', #82290, .T. ) ;
#32392 = ORIENTED_EDGE ( 'NONE', *, *, #29357, .T. ) ;
#32393 = VECTOR ( 'NONE', #60318, 1000.000000000000000 ) ;
#32394 = FACE_OUTER_BOUND ( 'NONE', #22695, .T. ) ;
#32395 = DIRECTION ( 'NONE',  ( -0.7071067811865486830, 0.7071067811865464625, 0.000000000000000000 ) ) ;
#32396 = VECTOR ( 'NONE', #18703, 999.9999999999998863 ) ;
#32397 = EDGE_CURVE ( 'NONE', #82859, #102617, #106439, .T. ) ;
#32398 = ORIENTED_EDGE ( 'NONE', *, *, #63248, .F. ) ;
#32399 = ORIENTED_EDGE ( 'NONE', *, *, #132187, .F. ) ;
#32400 = EDGE_CURVE ( 'NONE', #95357, #7059, #66558, .T. ) ;
#32401 = CIRCLE ( 'NONE', #46298, 2.055000000000000604 ) ;
#32402 = ORIENTED_EDGE ( 'NONE', *, *, #85897, .T. ) ;
#32404 = VECTOR ( 'NONE', #35187, 1000.000000000000000 ) ;
#32403 = CARTESIAN_POINT ( 'NONE',  ( 63.43793019189811133, -6.110000000000001208, 1.637169565754158951 ) ) ;
#32405 = ORIENTED_EDGE ( 'NONE', *, *, #140232, .T. ) ;
#32406 = EDGE_CURVE ( 'NONE', #119351, #34476, #58738, .T. ) ;
#32407 = CYLINDRICAL_SURFACE ( 'NONE', #53488, 0.5000000000000004441 ) ;
#32408 = FILL_AREA_STYLE ('',( #75214 ) ) ;
#32409 = CARTESIAN_POINT ( 'NONE',  ( 95.37543019189810423, -5.291415217122920289, -3.055000000000001492 ) ) ;
#32411 = CARTESIAN_POINT ( 'NONE',  ( 1.499999999999997780, 1.087461875839228931, 4.000000000000000000 ) ) ;
#32410 = CARTESIAN_POINT ( 'NONE',  ( 0.000000000000000000, 0.4000000000000001332, -2.015694669338588429 ) ) ;
#32412 = VERTEX_POINT ( 'NONE', #21620 ) ;
#32413 = DIRECTION ( 'NONE',  ( 0.7071067811865487940, 0.7071067811865463515, -0.000000000000000000 ) ) ;
#32414 = AXIS2_PLACEMENT_3D ( 'NONE', #13902, #59604, #136410 ) ;
#32415 = DIRECTION ( 'NONE',  ( 0.6830127018922180770, -0.6830127018922204085, -0.2588190451025213501 ) ) ;
#32416 = CARTESIAN_POINT ( 'NONE',  ( 91.70833333333334281, -3.974999999999999201, -6.884901960086287964 ) ) ;
#32417 = CARTESIAN_POINT ( 'NONE',  ( -2.999999999999981792, -22.22500000000000142, 4.412002311790018894 ) ) ;
#32418 = ORIENTED_EDGE ( 'NONE', *, *, #45655, .F. ) ;
#32419 = LINE ( 'NONE', #86802, #62284 ) ;
#32420 = ORIENTED_EDGE ( 'NONE', *, *, #84429, .F. ) ;
#32421 = ORIENTED_EDGE ( 'NONE', *, *, #63784, .F. ) ;
#32422 = ORIENTED_EDGE ( 'NONE', *, *, #51510, .F. ) ;
#32423 = EDGE_CURVE ( 'NONE', #72772, #107486, #22288, .T. ) ;
#32424 = CARTESIAN_POINT ( 'NONE',  ( 121.6829301918981088, -1.637169565754158951, -6.109999999999998543 ) ) ;
#32425 = VERTEX_POINT ( 'NONE', #556 ) ;
#32426 = AXIS2_PLACEMENT_3D ( 'NONE', #98029, #106008, #130675 ) ;
#32427 = DIRECTION ( 'NONE',  ( -0.7071067811865486830, -0.7071067811865464625, 0.000000000000000000 ) ) ;
#32428 = DIRECTION ( 'NONE',  ( -0.6830127018922181881, 0.6830127018922202975, -0.2588190451025214056 ) ) ;
#32429 = ORIENTED_EDGE ( 'NONE', *, *, #117095, .F. ) ;
#32430 = FACE_OUTER_BOUND ( 'NONE', #34067, .T. ) ;
#32431 = ORIENTED_EDGE ( 'NONE', *, *, #140831, .F. ) ;
#32432 = CIRCLE ( 'NONE', #67197, 1.142820323027524232 ) ;
#32433 = VECTOR ( 'NONE', #38496, 1000.000000000000000 ) ;
#32434 = ADVANCED_FACE ( 'NONE', ( #79625 ), #68030, .T. ) ;
#32435 = CARTESIAN_POINT ( 'NONE',  ( 17.33290314143522082, -3.967499999999994476, 6.871911579029513106 ) ) ;
#32436 = CARTESIAN_POINT ( 'NONE',  ( -28.49999999999980105, -2.947814304570797184, 5.000000000000000000 ) ) ;
#32437 = CARTESIAN_POINT ( 'NONE',  ( -25.82816939922334853, 6.759292476615651246, 4.000000000000000000 ) ) ;
#32438 = ORIENTED_EDGE ( 'NONE', *, *, #50749, .F. ) ;
#32439 = ORIENTED_EDGE ( 'NONE', *, *, #4105, .T. ) ;
#32440 = EDGE_CURVE ( 'NONE', #25852, #110079, #17076, .T. ) ;
#32441 = ORIENTED_EDGE ( 'NONE', *, *, #78693, .F. ) ;
#32442 = CARTESIAN_POINT ( 'NONE',  ( 20.70833333333333570, 3.047499999999997655, 5.278424836066143655 ) ) ;
#32443 = CARTESIAN_POINT ( 'NONE',  ( 58.75000000000000000, -9.735942053221458872E-16, 7.950000000000000178 ) ) ;
#32444 = DIRECTION ( 'NONE',  ( 0.6830127018922180770, -0.6830127018922204085, -0.2588190451025213501 ) ) ;
#32445 = FACE_OUTER_BOUND ( 'NONE', #20905, .T. ) ;
#32446 = AXIS2_PLACEMENT_3D ( 'NONE', #8475, #32428, #31706 ) ;
#32447 = DIRECTION ( 'NONE',  ( 1.000000000000000000, 0.000000000000000000, 0.000000000000000000 ) ) ;
#32448 = CARTESIAN_POINT ( 'NONE',  ( 28.43793019189810423, -6.110000000000001208, 1.637169565754158951 ) ) ;
#32449 = ADVANCED_FACE ( 'NONE', ( #24464 ), #111471, .F. ) ;
#32450 = FACE_OUTER_BOUND ( 'NONE', #82176, .T. ) ;
#32451 = CARTESIAN_POINT ( 'NONE',  ( -18.48921356237309510, -27.52281430457068367, 5.000000000000000000 ) ) ;
#32452 = VERTEX_POINT ( 'NONE', #54974 ) ;
#32453 = LINE ( 'NONE', #20116, #27811 ) ;
#32454 = VECTOR ( 'NONE', #92228, 1000.000000000000000 ) ;
#32455 = VERTEX_POINT ( 'NONE', #56440 ) ;
#32456 = VECTOR ( 'NONE', #39755, 1000.000000000000000 ) ;
#32457 = AXIS2_PLACEMENT_3D ( 'NONE', #63143, #18134, #72612 ) ;
#32458 = AXIS2_PLACEMENT_3D ( 'NONE', #126725, #94802, #69546 ) ;
#32459 = LINE ( 'NONE', #68669, #70802 ) ;
#32460 = ORIENTED_EDGE ( 'NONE', *, *, #116729, .T. ) ;
#32461 = AXIS2_PLACEMENT_3D ( 'NONE', #127801, #28487, #132812 ) ;
#32462 = FACE_OUTER_BOUND ( 'NONE', #58691, .T. ) ;
#32464 = ORIENTED_EDGE ( 'NONE', *, *, #123548, .F. ) ;
#32463 = CARTESIAN_POINT ( 'NONE',  ( 42.70833333333333570, -3.974999999999999201, -6.884901960086287964 ) ) ;
#32465 = EDGE_CURVE ( 'NONE', #65533, #27038, #91187, .T. ) ;
#32466 = LINE ( 'NONE', #30311, #32981 ) ;
#32467 = ORIENTED_EDGE ( 'NONE', *, *, #143247, .F. ) ;
#32468 = PLANE ( 'NONE',  #94740 ) ;
#32469 = ORIENTED_EDGE ( 'NONE', *, *, #140099, .T. ) ;
#32470 = CARTESIAN_POINT ( 'NONE',  ( -10.67372558692450113, -22.22500000000000142, 14.18971443535745358 ) ) ;
#32471 = VECTOR ( 'NONE', #38545, 1000.000000000000227 ) ;
#32472 = ORIENTED_EDGE ( 'NONE', *, *, #112897, .F. ) ;
#32473 = DIRECTION ( 'NONE',  ( -0.3543493200069162685, -0.000000000000000000, -0.9351131265310288487 ) ) ;
#32474 = CARTESIAN_POINT ( 'NONE',  ( 108.2875270504628986, 0.000000000000000000, -7.949999999999998401 ) ) ;
#32475 = CARTESIAN_POINT ( 'NONE',  ( 0.000000000000000000, 0.000000000000000000, 5.000000000000000000 ) ) ;
#32476 = SURFACE_SIDE_STYLE ('',( #53511 ) ) ;
#32477 = CARTESIAN_POINT ( 'NONE',  ( 20.97999999999999687, -2.055000000000000160, 0.000000000000000000 ) ) ;
#32478 = CARTESIAN_POINT ( 'NONE',  ( 23.70025512860841133, -27.71228299555189523, 4.000000000000000000 ) ) ;
#32479 = CARTESIAN_POINT ( 'NONE',  ( -0.1839886062690032631, 28.73617430169787568, 5.000000000000000000 ) ) ;
#32480 = CARTESIAN_POINT ( 'NONE',  ( 1.312499999999999778, -4.461849672132299993, -4.461849672132299105 ) ) ;
#32482 = VECTOR ( 'NONE', #15840, 1000.000000000000000 ) ;
#32481 = CARTESIAN_POINT ( 'NONE',  ( 21.27040314143522082, -7.934999999999988951, 2.126176841940957907 ) ) ;
#32483 = DIRECTION ( 'NONE',  ( 0.000000000000000000, -1.000000000000000000, 0.000000000000000000 ) ) ;
#32484 = CARTESIAN_POINT ( 'NONE',  ( -32.99999999999976552, 7.931123077392111753, 4.000000000000000000 ) ) ;
#32485 = ORIENTED_EDGE ( 'NONE', *, *, #80089, .F. ) ;
#32486 = ORIENTED_EDGE ( 'NONE', *, *, #30038, .F. ) ;
#32487 = VECTOR ( 'NONE', #53170, 999.9999999999998863 ) ;
#32488 = FACE_OUTER_BOUND ( 'NONE', #36456, .T. ) ;
#32489 = ORIENTED_EDGE ( 'NONE', *, *, #75395, .T. ) ;
#32490 = EDGE_CURVE ( 'NONE', #83478, #64860, #12155, .T. ) ;
#32491 = EDGE_CURVE ( 'NONE', #54885, #48586, #1950, .T. ) ;
#32492 = VECTOR ( 'NONE', #41744, 1000.000000000000114 ) ;
#32493 = FACE_OUTER_BOUND ( 'NONE', #19269, .T. ) ;
#32494 = CARTESIAN_POINT ( 'NONE',  ( 78.29974487139158157, -27.71228299555260577, 4.000000000000000000 ) ) ;
#32495 = CYLINDRICAL_SURFACE ( 'NONE', #51608, 2.552699999999994418 ) ;
#32496 = FILL_AREA_STYLE ('',( #55682 ) ) ;
#32497 = ORIENTED_EDGE ( 'NONE', *, *, #137923, .F. ) ;
#32498 = AXIS2_PLACEMENT_3D ( 'NONE', #126565, #70118, #36710 ) ;
#32499 = DIRECTION ( 'NONE',  ( 0.000000000000000000, -1.000000000000000000, 0.000000000000000000 ) ) ;
#32500 = LINE ( 'NONE', #20155, #97356 ) ;
#32501 = DIRECTION ( 'NONE',  ( -0.6830127018922180770, -0.6830127018922204085, -0.2588190451025213501 ) ) ;
#32502 = EDGE_CURVE ( 'NONE', #37517, #84503, #33934, .T. ) ;
#32503 = CYLINDRICAL_SURFACE ( 'NONE', #71719, 3.999999999999996447 ) ;
#32504 = VECTOR ( 'NONE', #18497, 1000.000000000000000 ) ;
#32505 = EDGE_CURVE ( 'NONE', #84071, #85957, #44096, .T. ) ;
#32507 = ORIENTED_EDGE ( 'NONE', *, *, #131636, .T. ) ;
#32506 = CARTESIAN_POINT ( 'NONE',  ( -8.999999999999934275, -3.412538124160724884, 4.000000000000000000 ) ) ;
#32508 = SURFACE_STYLE_USAGE ( .BOTH. , #98461 ) ;
#32509 = FILL_AREA_STYLE ('',( #44101 ) ) ;
#32510 = PLANE ( 'NONE',  #38696 ) ;
#32511 = DIRECTION ( 'NONE',  ( 0.000000000000000000, -1.000000000000000000, 0.000000000000000000 ) ) ;
#32512 = ORIENTED_EDGE ( 'NONE', *, *, #132380, .T. ) ;
#32513 = EDGE_LOOP ( 'NONE', ( #38754, #62765, #42751, #56442 ) ) ;
#32514 = ORIENTED_EDGE ( 'NONE', *, *, #127816, .T. ) ;
#32515 = CARTESIAN_POINT ( 'NONE',  ( 97.12543019189810423, 5.291415217122919401, 3.055000000000002824 ) ) ;
#32516 = VECTOR ( 'NONE', #93869, 999.9999999999998863 ) ;
#32517 = VERTEX_POINT ( 'NONE', #89721 ) ;
#32518 = DIRECTION ( 'NONE',  ( -0.000000000000000000, -0.000000000000000000, 1.000000000000000000 ) ) ;
#32519 = VECTOR ( 'NONE', #82083, 1000.000000000000227 ) ;
#32520 = LINE ( 'NONE', #10034, #54733 ) ;
#32521 = ORIENTED_EDGE ( 'NONE', *, *, #6738, .F. ) ;
#32522 = EDGE_CURVE ( 'NONE', #20496, #38971, #102034, .T. ) ;
#32523 = CARTESIAN_POINT ( 'NONE',  ( 51.48921356237309510, -27.52281430457091460, 5.000000000000000000 ) ) ;
#32524 = CARTESIAN_POINT ( 'NONE',  ( 49.56249999999999289, -5.819803920172573086, -5.819803920172573974 ) ) ;
#32525 = CARTESIAN_POINT ( 'NONE',  ( 90.47459685856479439, 1.637169565754164058, -6.109999999999996767 ) ) ;
#32526 = ORIENTED_EDGE ( 'NONE', *, *, #136975, .F. ) ;
#32527 = CARTESIAN_POINT ( 'NONE',  ( 45.48921356237309510, -27.52281430457087197, 5.000000000000000000 ) ) ;
#32528 = LINE ( 'NONE', #44880, #37919 ) ;
#32529 = AXIS2_PLACEMENT_3D ( 'NONE', #30456, #85517, #29711 ) ;
#32530 = ORIENTED_EDGE ( 'NONE', *, *, #62047, .T. ) ;
#32531 = ORIENTED_EDGE ( 'NONE', *, *, #138091, .T. ) ;
#32532 = VERTEX_POINT ( 'NONE', #33252 ) ;
#32533 = PLANE ( 'NONE',  #16690 ) ;
#32534 = DIRECTION ( 'NONE',  ( 0.7071067811865487940, 0.7071067811865463515, 0.000000000000000000 ) ) ;
#32535 = LINE ( 'NONE', #106672, #120573 ) ;
#32536 = AXIS2_PLACEMENT_3D ( 'NONE', #43704, #44452, #77773 ) ;
#32537 = VECTOR ( 'NONE', #139255, 1000.000000000000000 ) ;
#32538 = CARTESIAN_POINT ( 'NONE',  ( 3.730677800976855973, -49.14999999999999147, -40.92499999999998295 ) ) ;
#32539 = CARTESIAN_POINT ( 'NONE',  ( -54.48921356237310221, -27.52281430457093236, 5.000000000000000000 ) ) ;
#32540 = ADVANCED_FACE ( 'NONE', ( #77458 ), #101314, .F. ) ;
#32541 = VERTEX_POINT ( 'NONE', #93295 ) ;
#32542 = EDGE_LOOP ( 'NONE', ( #81905, #132905, #26230, #116536 ) ) ;
#32543 = EDGE_CURVE ( 'NONE', #130580, #4806, #103433, .T. ) ;
#32544 = DIRECTION ( 'NONE',  ( -0.7071067811865486830, 0.7071067811865464625, 0.000000000000000000 ) ) ;
#32545 = ORIENTED_EDGE ( 'NONE', *, *, #105621, .F. ) ;
#32546 = ORIENTED_EDGE ( 'NONE', *, *, #21591, .F. ) ;
#32547 = CIRCLE ( 'NONE', #41857, 2.500000000000000444 ) ;
#32548 = EDGE_CURVE ( 'NONE', #89800, #36309, #4078, .T. ) ;
#32549 = ADVANCED_FACE ( 'NONE', ( #38917 ), #83140, .F. ) ;
#32550 = CONICAL_SURFACE ( 'NONE', #37196, 2.500000000000000888, 0.9599310885968822538 ) ;
#32551 = CIRCLE ( 'NONE', #141287, 2.337593264352433753 ) ;
#32552 = CARTESIAN_POINT ( 'NONE',  ( 20.53839644629416128, -9.740707523384177335, 17.74957260769615530 ) ) ;
#32553 = EDGE_LOOP ( 'NONE', ( #77886, #45065, #128194, #120762 ) ) ;
#32554 = LINE ( 'NONE', #97794, #52910 ) ;
#32555 = CARTESIAN_POINT ( 'NONE',  ( -8.999999999999934275, -4.447814304570786526, 5.000000000000000000 ) ) ;
#32556 = DIRECTION ( 'NONE',  ( 0.7071067811865487940, 0.7071067811865463515, 0.000000000000000000 ) ) ;
#32557 = DIRECTION ( 'NONE',  ( 0.000000000000000000, -1.000000000000000000, 0.000000000000000000 ) ) ;
#32558 = AXIS2_PLACEMENT_3D ( 'NONE', #31875, #101405, #1357 ) ;
#32559 = AXIS2_PLACEMENT_3D ( 'NONE', #33209, #65105, #86843 ) ;
#32560 = AXIS2_PLACEMENT_3D ( 'NONE', #104254, #125331, #136911 ) ;
#32561 = COLOUR_RGB ( '', 0.08235294, 0.09019608, 0.10196078) ;
#32562 = DIRECTION ( 'NONE',  ( 0.000000000000000000, -1.000000000000000000, -1.091707662666338270E-16 ) ) ;
#32563 = EDGE_LOOP ( 'NONE', ( #96368, #78645, #37820, #26013 ) ) ;
#32564 = VECTOR ( 'NONE', #61338, 1000.000000000000000 ) ;
#32565 = CARTESIAN_POINT ( 'NONE',  ( 5.671830600776432973, -15.74070752338412049, 4.000000000000000000 ) ) ;
#32566 = EDGE_CURVE ( 'NONE', #61026, #28815, #31516, .T. ) ;
#32567 = VERTEX_POINT ( 'NONE', #71556 ) ;
#32568 = CARTESIAN_POINT ( 'NONE',  ( -2.999999999999975131, -3.033600742197712030, 5.000000000000000000 ) ) ;
#32569 = ORIENTED_EDGE ( 'NONE', *, *, #100950, .F. ) ;
#32570 = PRESENTATION_STYLE_ASSIGNMENT (( #131876 ) ) ;
#32571 = EDGE_CURVE ( 'NONE', #94004, #24699, #25899, .T. ) ;
#32572 = ORIENTED_EDGE ( 'NONE', *, *, #88186, .T. ) ;
#32573 = DIRECTION ( 'NONE',  ( -0.000000000000000000, 0.3543493200069153248, 0.9351131265310292928 ) ) ;
#32574 = ORIENTED_EDGE ( 'NONE', *, *, #72661, .F. ) ;
#32575 = ORIENTED_EDGE ( 'NONE', *, *, #127846, .F. ) ;
#32576 = VECTOR ( 'NONE', #139315, 1000.000000000000000 ) ;
#32577 = VERTEX_POINT ( 'NONE', #48363 ) ;
#32578 = ADVANCED_FACE ( 'NONE', ( #102757 ), #91856, .F. ) ;
#32579 = DIRECTION ( 'NONE',  ( 0.7071067811865486830, -0.7071067811865464625, -0.000000000000000000 ) ) ;
#32580 = CARTESIAN_POINT ( 'NONE',  ( 20.01088028653934003, -22.02621442084248571, 4.990779571109219326 ) ) ;
#32581 = PLANE ( 'NONE',  #896 ) ;
#32582 = CARTESIAN_POINT ( 'NONE',  ( 123.5212635252314470, -4.472830434245838482, -4.472830434245840259 ) ) ;
#32583 = PLANE ( 'NONE',  #31197 ) ;
#32584 = PLANE ( 'NONE',  #50527 ) ;
#32586 = DIRECTION ( 'NONE',  ( 0.6830127018922181881, 0.6830127018922202975, -0.2588190451025214056 ) ) ;
#32585 = CARTESIAN_POINT ( 'NONE',  ( -16.49999999999988276, 16.77039438581777375, 0.4657186855308104723 ) ) ;
#32587 = VECTOR ( 'NONE', #81694, 1000.000000000000000 ) ;
#32588 = ADVANCED_FACE ( 'NONE', ( #37508 ), #15003, .F. ) ;
#32589 = CARTESIAN_POINT ( 'NONE',  ( -27.18398860626900060, 28.73617430169806042, 5.000000000000000000 ) ) ;
#32590 = AXIS2_PLACEMENT_3D ( 'NONE', #90842, #35763, #90085 ) ;
#32591 = PRESENTATION_STYLE_ASSIGNMENT (( #76826 ) ) ;
#32592 = AXIS2_PLACEMENT_3D ( 'NONE', #44354, #32021, #58 ) ;
#32593 = CARTESIAN_POINT ( 'NONE',  ( 30.81246187583926144, -22.22500000000000142, 4.000000000000000000 ) ) ;
#32594 = CARTESIAN_POINT ( 'NONE',  ( -66.18398860626901126, 28.73617430169833753, 5.000000000000000000 ) ) ;
#32595 = ORIENTED_EDGE ( 'NONE', *, *, #51554, .F. ) ;
#32596 = AXIS2_PLACEMENT_3D ( 'NONE', #71921, #95047, #82774 ) ;
#32597 = ORIENTED_EDGE ( 'NONE', *, *, #89982, .T. ) ;
#32599 = ORIENTED_EDGE ( 'NONE', *, *, #105243, .T. ) ;
#32598 = EDGE_CURVE ( 'NONE', #78254, #30546, #54061, .T. ) ;
#32600 = CARTESIAN_POINT ( 'NONE',  ( 3.489213562373097322, -27.52281430457057709, 5.000000000000000000 ) ) ;
#32601 = EDGE_LOOP ( 'NONE', ( #92221, #75420, #82628 ) ) ;
#32602 = VECTOR ( 'NONE', #97508, 1000.000000000000000 ) ;
#32603 = ORIENTED_EDGE ( 'NONE', *, *, #76930, .F. ) ;
#32604 = DIRECTION ( 'NONE',  ( 0.7071067811865487940, 0.7071067811865463515, -0.000000000000000000 ) ) ;
#32605 = CARTESIAN_POINT ( 'NONE',  ( 10.82816939922345156, -14.24070752338413293, 4.000000000000000000 ) ) ;
#32606 = STYLED_ITEM ( 'NONE', ( #45323 ), #82293 ) ;
#32607 = LINE ( 'NONE', #55069, #95845 ) ;
#32608 = LINE ( 'NONE', #76842, #14000 ) ;
#32609 = EDGE_CURVE ( 'NONE', #24642, #24958, #26611, .T. ) ;
#32610 = VERTEX_POINT ( 'NONE', #15682 ) ;
#32611 = EDGE_CURVE ( 'NONE', #19510, #128631, #16417, .T. ) ;
#32612 = CARTESIAN_POINT ( 'NONE',  ( 32.67183060077623935, -12.74070752338415602, 4.000000000000000000 ) ) ;
#32613 = ORIENTED_EDGE ( 'NONE', *, *, #92748, .F. ) ;
#32614 = ADVANCED_FACE ( 'NONE', ( #38214 ), #102672, .T. ) ;
#32615 = AXIS2_PLACEMENT_3D ( 'NONE', #5331, #71341, #49614 ) ;
#32616 = CARTESIAN_POINT ( 'NONE',  ( 15.81706980810188767, -2.126176841940956130, 7.934999999999991616 ) ) ;
#32617 = ORIENTED_EDGE ( 'NONE', *, *, #142645, .T. ) ;
#32618 = CARTESIAN_POINT ( 'NONE',  ( 89.59959685856475176, -6.109999999999998543, -1.637169565754160727 ) ) ;
#32619 = CARTESIAN_POINT ( 'NONE',  ( 6.849737334536333044, -9.119535513348605349, -2.672630034853287206 ) ) ;
#32620 = FACE_OUTER_BOUND ( 'NONE', #58915, .T. ) ;
#32621 = CARTESIAN_POINT ( 'NONE',  ( 35.99451991528749772, 28.92564299267963079, 4.000000000000000000 ) ) ;
#32622 = ORIENTED_EDGE ( 'NONE', *, *, #7414, .F. ) ;
#32623 = VERTEX_POINT ( 'NONE', #69424 ) ;
#32624 = VECTOR ( 'NONE', #50846, 999.9999999999998863 ) ;
#32625 = VERTEX_POINT ( 'NONE', #57593 ) ;
#32626 = DIRECTION ( 'NONE',  ( 1.000000000000000000, 1.224606353822377258E-16, 0.000000000000000000 ) ) ;
#32627 = PLANE ( 'NONE',  #78715 ) ;
#32628 = DIRECTION ( 'NONE',  ( -0.000000000000000000, -0.3543493200069152693, 0.9351131265310292928 ) ) ;
#32629 = CARTESIAN_POINT ( 'NONE',  ( -15.78162688292483118, 21.74787736706805674, 4.999607392498049308 ) ) ;
#32630 = PLANE ( 'NONE',  #3265 ) ;
#32631 = ORIENTED_EDGE ( 'NONE', *, *, #122212, .F. ) ;
#32632 = CARTESIAN_POINT ( 'NONE',  ( 15.48921356237309510, -27.52281430457066236, 5.000000000000000000 ) ) ;
#32633 = PRESENTATION_STYLE_ASSIGNMENT (( #143510 ) ) ;
#32634 = DIRECTION ( 'NONE',  ( -0.6830127018922180770, -0.6830127018922204085, -0.2588190451025213501 ) ) ;
#32635 = ORIENTED_EDGE ( 'NONE', *, *, #52665, .T. ) ;
#32636 = DIRECTION ( 'NONE',  ( 0.000000000000000000, 0.000000000000000000, -1.000000000000000000 ) ) ;
#32637 = AXIS2_PLACEMENT_3D ( 'NONE', #114257, #57062, #68642 ) ;
#32638 = PLANE ( 'NONE',  #84098 ) ;
#32639 = ORIENTED_EDGE ( 'NONE', *, *, #35749, .F. ) ;
#32641 = ORIENTED_EDGE ( 'NONE', *, *, #36614, .F. ) ;
#32640 = DIRECTION ( 'NONE',  ( -0.6830127018922180770, -0.6830127018922204085, -0.2588190451025213501 ) ) ;
#32642 = ORIENTED_EDGE ( 'NONE', *, *, #47023, .F. ) ;
#32643 = CARTESIAN_POINT ( 'NONE',  ( 0.000000000000000000, 0.000000000000000000, 5.000000000000000000 ) ) ;
#32644 = DIRECTION ( 'NONE',  ( -1.000000000000000000, -0.000000000000000000, -0.000000000000000000 ) ) ;
#32646 = ORIENTED_EDGE ( 'NONE', *, *, #127332, .F. ) ;
#32645 = VECTOR ( 'NONE', #136411, 1000.000000000000227 ) ;
#32647 = CARTESIAN_POINT ( 'NONE',  ( 0.000000000000000000, 0.000000000000000000, 5.000000000000000000 ) ) ;
#32648 = DIRECTION ( 'NONE',  ( -0.7071067811865486830, -0.7071067811865464625, 0.000000000000000000 ) ) ;
#32649 = CARTESIAN_POINT ( 'NONE',  ( 6.299744871391586898, -27.71228299555210484, 4.000000000000000000 ) ) ;
#32650 = CARTESIAN_POINT ( 'NONE',  ( 4.603431928946396745, -14.24070752338413648, 19.24067776001727026 ) ) ;
#32651 = CARTESIAN_POINT ( 'NONE',  ( 32.20833333333332149, -3.974999999999999201, -6.884901960086287964 ) ) ;
#32652 = PLANE ( 'NONE',  #58432 ) ;
#32653 = LINE ( 'NONE', #78296, #12364 ) ;
#32654 = LINE ( 'NONE', #130543, #2023 ) ;
#32655 = DIRECTION ( 'NONE',  ( 0.7071067811865487940, 0.7071067811865463515, 0.000000000000000000 ) ) ;
#32656 = CARTESIAN_POINT ( 'NONE',  ( 10.49999999999992895, 16.77039438581780217, 0.4657186855307497431 ) ) ;
#32657 = CARTESIAN_POINT ( 'NONE',  ( -20.67183060077632817, 14.25929247661556865, 4.000000000000000000 ) ) ;
#32658 = AXIS2_PLACEMENT_3D ( 'NONE', #2244, #15262, #832 ) ;
#32659 = CARTESIAN_POINT ( 'NONE',  ( -2.010880286539463935, -22.02621442084248216, 4.990779571109222879 ) ) ;
#32660 = CARTESIAN_POINT ( 'NONE',  ( -18.32816939922339472, 11.25929247661559884, 4.000000000000000000 ) ) ;
#32661 = EDGE_LOOP ( 'NONE', ( #66423, #75087, #43937 ) ) ;
#32662 =( BOUNDED_CURVE ( )  B_SPLINE_CURVE ( 3, ( #73978, #118895, #52899, #139257 ),
 .UNSPECIFIED., .F., .F. ) 
 B_SPLINE_CURVE_WITH_KNOTS ( ( 4, 4 ),
 ( 1.208578181583235267, 1.359146454359416278 ),
 .UNSPECIFIED. ) 
 CURVE ( )  GEOMETRIC_REPRESENTATION_ITEM ( )  RATIONAL_B_SPLINE_CURVE ( ( 1.000000000000000000, 0.9981116584018958626, 0.9981116584018958626, 1.000000000000000000 ) ) 
 REPRESENTATION_ITEM ( '' )  );
#32663 = ORIENTED_EDGE ( 'NONE', *, *, #58045, .T. ) ;
#32664 = VECTOR ( 'NONE', #125097, 1000.000000000000000 ) ;
#32665 = CARTESIAN_POINT ( 'NONE',  ( 99.87499999999998579, 7.950000000000000178, 1.460391307983218535E-15 ) ) ;
#32666 = VECTOR ( 'NONE', #44890, 1000.000000000000000 ) ;
#32667 = VERTEX_POINT ( 'NONE', #66319 ) ;
#32668 = ORIENTED_EDGE ( 'NONE', *, *, #13493, .T. ) ;
#32669 = ORIENTED_EDGE ( 'NONE', *, *, #51359, .T. ) ;
#32670 = FACE_OUTER_BOUND ( 'NONE', #89409, .T. ) ;
#32671 = CARTESIAN_POINT ( 'NONE',  ( 12.18398860626900060, 28.73617430169795739, 5.000000000000000000 ) ) ;
#32672 = AXIS2_PLACEMENT_3D ( 'NONE', #50269, #114769, #82207 ) ;
#32673 = AXIS2_PLACEMENT_3D ( 'NONE', #22787, #69958, #48162 ) ;
#32674 = VECTOR ( 'NONE', #45324, 1000.000000000000000 ) ;
#32675 = VECTOR ( 'NONE', #129667, 1000.000000000000000 ) ;
#32676 = EDGE_LOOP ( 'NONE', ( #47320, #58207, #96380, #41486 ) ) ;
#32677 =( BOUNDED_CURVE ( )  B_SPLINE_CURVE ( 3, ( #65530, #109704, #143046, #79274 ),
 .UNSPECIFIED., .F., .F. ) 
 B_SPLINE_CURVE_WITH_KNOTS ( ( 4, 4 ),
 ( 5.584306267627116682, 5.657315652343092971 ),
 .UNSPECIFIED. ) 
 CURVE ( )  GEOMETRIC_REPRESENTATION_ITEM ( )  RATIONAL_B_SPLINE_CURVE ( ( 1.000000000000000000, 0.9995558518042845231, 0.9995558518042845231, 1.000000000000000000 ) ) 
 REPRESENTATION_ITEM ( '' )  );
#32678 = DIRECTION ( 'NONE',  ( -1.000000000000000000, -1.224606353822377258E-16, -0.000000000000000000 ) ) ;
#32679 = VECTOR ( 'NONE', #77720, 1000.000000000000000 ) ;
#32680 = DIRECTION ( 'NONE',  ( -0.000000000000000000, 0.3543493200069153248, 0.9351131265310292928 ) ) ;
#32681 = CARTESIAN_POINT ( 'NONE',  ( 19.10840764549667270, 9.139736423841732040E-16, 0.000000000000000000 ) ) ;
#32682 = DIRECTION ( 'NONE',  ( 0.3543493200069162685, -0.000000000000000000, -0.9351131265310288487 ) ) ;
#32683 = EDGE_CURVE ( 'NONE', #98472, #52633, #133017, .T. ) ;
#32684 = VERTEX_POINT ( 'NONE', #68477 ) ;
#32685 = CARTESIAN_POINT ( 'NONE',  ( 15.15628408943919858, 3.809557873852078114, -32.44464145375744835 ) ) ;
#32686 = ADVANCED_FACE ( 'NONE', ( #67776 ), #24922, .T. ) ;
#32687 = DIRECTION ( 'NONE',  ( -0.000000000000000000, 0.000000000000000000, 1.000000000000000000 ) ) ;
#32688 = AXIS2_PLACEMENT_3D ( 'NONE', #79622, #78874, #12852 ) ;
#32689 = LINE ( 'NONE', #31955, #137742 ) ;
#32690 = CARTESIAN_POINT ( 'NONE',  ( 24.50000000000000000, 0.000000000000000000, 6.094999999999989981 ) ) ;
#32691 = CARTESIAN_POINT ( 'NONE',  ( -12.20000000000000284, -35.14999999999999147, -40.00000000000000000 ) ) ;
#32692 = CARTESIAN_POINT ( 'NONE',  ( 10.46799328145038821, 4.202752102959690472E-16, 0.000000000000000000 ) ) ;
#32693 = CARTESIAN_POINT ( 'NONE',  ( 66.18398860626901126, 28.73617430169833753, 5.000000000000000000 ) ) ;
#32694 = ORIENTED_EDGE ( 'NONE', *, *, #125858, .T. ) ;
#32695 = ORIENTED_EDGE ( 'NONE', *, *, #96277, .F. ) ;
#32696 = CARTESIAN_POINT ( 'NONE',  ( 118.8545968585647898, -1.637169565754161615, 6.110000000000000320 ) ) ;
#32697 = VERTEX_POINT ( 'NONE', #45300 ) ;
#32698 = EDGE_CURVE ( 'NONE', #27002, #68801, #111208, .T. ) ;
#32699 = VECTOR ( 'NONE', #115219, 1000.000000000000000 ) ;
#32700 = DIRECTION ( 'NONE',  ( 1.000000000000000000, 0.000000000000000000, 0.000000000000000000 ) ) ;
#32701 = VECTOR ( 'NONE', #107336, 1000.000000000000000 ) ;
#32702 = DIRECTION ( 'NONE',  ( 1.000000000000000000, 0.000000000000000000, 0.000000000000000000 ) ) ;
#32703 = DIRECTION ( 'NONE',  ( 0.3543493200069162685, -0.000000000000000000, -0.9351131265310288487 ) ) ;
#32704 = EDGE_CURVE ( 'NONE', #122378, #42180, #36527, .T. ) ;
#32705 = CARTESIAN_POINT ( 'NONE',  ( -54.18398860626899705, 28.73617430169825226, 5.000000000000000000 ) ) ;
#32706 = AXIS2_PLACEMENT_3D ( 'NONE', #121141, #9504, #34158 ) ;
#32707 = VECTOR ( 'NONE', #32899, 1000.000000000000000 ) ;
#32708 = CARTESIAN_POINT ( 'NONE',  ( 115.5579301918981088, 6.110000000000000320, -1.637169565754156064 ) ) ;
#32709 = ORIENTED_EDGE ( 'NONE', *, *, #26910, .T. ) ;
#32710 = AXIS2_PLACEMENT_3D ( 'NONE', #6297, #138305, #16494 ) ;
#32711 = ORIENTED_EDGE ( 'NONE', *, *, #87003, .T. ) ;
#32712 = PLANE ( 'NONE',  #134226 ) ;
#32713 = ADVANCED_FACE ( 'NONE', ( #11897 ), #35856, .F. ) ;
#32714 = AXIS2_PLACEMENT_3D ( 'NONE', #18901, #73309, #108027 ) ;
#32715 = DIRECTION ( 'NONE',  ( -0.5735764363510499342, -0.8191520442889891340, 0.000000000000000000 ) ) ;
#32716 = VERTEX_POINT ( 'NONE', #124248 ) ;
#32717 = ORIENTED_EDGE ( 'NONE', *, *, #125645, .T. ) ;
#32718 = CARTESIAN_POINT ( 'NONE',  ( 40.10459685856476142, 1.637169565754164946, -6.109999999999999432 ) ) ;
#32719 = EDGE_LOOP ( 'NONE', ( #65005, #118252, #25426 ) ) ;
#32720 = AXIS2_PLACEMENT_3D ( 'NONE', #15297, #29070, #71169 ) ;
#32721 = LINE ( 'NONE', #9483, #7465 ) ;
#32722 = CARTESIAN_POINT ( 'NONE',  ( -26.99999999999980815, -3.033600742197708477, 5.000000000000000000 ) ) ;
#32723 = VECTOR ( 'NONE', #90037, 1000.000000000000000 ) ;
#32724 = CARTESIAN_POINT ( 'NONE',  ( 39.87043019189810877, -3.055000000000001492, 5.291415217122917625 ) ) ;
#32725 = EDGE_LOOP ( 'NONE', ( #37956, #47541, #109246, #92809 ) ) ;
#32726 = ADVANCED_FACE ( 'NONE', ( #56891 ), #56186, .F. ) ;
#32727 = CARTESIAN_POINT ( 'NONE',  ( 10.49999999999991829, -9.462702396501002866, -9.474982329943541615 ) ) ;
#32728 = VERTEX_POINT ( 'NONE', #100369 ) ;
#32729 = EDGE_LOOP ( 'NONE', ( #123651, #40812, #102327, #20385 ) ) ;
#32730 = ORIENTED_EDGE ( 'NONE', *, *, #132924, .T. ) ;
#32731 = ADVANCED_FACE ( 'NONE', ( #58338 ), #79370, .F. ) ;
#32732 = ADVANCED_FACE ( 'NONE', ( #101053 ), #33696, .F. ) ;
#32733 = SURFACE_STYLE_USAGE ( .BOTH. , #89930 ) ;
#32734 = DIRECTION ( 'NONE',  ( -0.000000000000000000, 0.3543493200069153248, 0.9351131265310292928 ) ) ;
#32735 = ORIENTED_EDGE ( 'NONE', *, *, #87877, .F. ) ;
#32736 = CARTESIAN_POINT ( 'NONE',  ( 15.98840764549667703, 9.139736423841732040E-16, 0.000000000000000000 ) ) ;
#32737 = CARTESIAN_POINT ( 'NONE',  ( -36.48921356237310221, -27.52281430457080802, 5.000000000000000000 ) ) ;
#32738 = VECTOR ( 'NONE', #104453, 1000.000000000000000 ) ;
#32739 = ADVANCED_FACE ( 'NONE', ( #24233 ), #134430, .F. ) ;
#32740 = LINE ( 'NONE', #76975, #25741 ) ;
#32741 = FACE_BOUND ( 'NONE', #112179, .T. ) ;
#32742 = EDGE_CURVE ( 'NONE', #29861, #80396, #13319, .T. ) ;
#32743 = VERTEX_POINT ( 'NONE', #101776 ) ;
#32744 = CARTESIAN_POINT ( 'NONE',  ( 0.000000000000000000, 0.000000000000000000, 0.000000000000000000 ) ) ;
#32745 = CARTESIAN_POINT ( 'NONE',  ( 31.49999999999977973, 6.431123077392124188, 4.000000000000000000 ) ) ;
#32746 = DIRECTION ( 'NONE',  ( -0.7071067811865487940, 0.7071067811865463515, -0.000000000000000000 ) ) ;
#32747 = EDGE_CURVE ( 'NONE', #134254, #46293, #34389, .T. ) ;
#32748 = ORIENTED_EDGE ( 'NONE', *, *, #58996, .T. ) ;
#32749 = LINE ( 'NONE', #110259, #98994 ) ;
#32750 = EDGE_LOOP ( 'NONE', ( #47466, #84667, #78307, #31828 ) ) ;
#32751 = VERTEX_POINT ( 'NONE', #77899 ) ;
#32752 = AXIS2_PLACEMENT_3D ( 'NONE', #118947, #18173, #95044 ) ;
#32753 = DIRECTION ( 'NONE',  ( 0.7071067811865486830, -0.7071067811865464625, -0.000000000000000000 ) ) ;
#32754 = ORIENTED_EDGE ( 'NONE', *, *, #134173, .T. ) ;
#32755 = CARTESIAN_POINT ( 'NONE',  ( 48.18293019189812298, -1.637169565754158951, -6.109999999999998543 ) ) ;
#32756 = ORIENTED_EDGE ( 'NONE', *, *, #116842, .T. ) ;
#32757 = EDGE_CURVE ( 'NONE', #89225, #142320, #46751, .T. ) ;
#32758 = DIRECTION ( 'NONE',  ( 0.6830127018922181881, 0.6830127018922202975, -0.2588190451025214056 ) ) ;
#32759 = CARTESIAN_POINT ( 'NONE',  ( 0.000000000000000000, 0.000000000000000000, 5.000000000000000000 ) ) ;
#32760 = CARTESIAN_POINT ( 'NONE',  ( 0.1839886062690032631, 28.73617430169787568, 5.000000000000000000 ) ) ;
#32761 = ORIENTED_EDGE ( 'NONE', *, *, #66011, .T. ) ;
#32762 = LINE ( 'NONE', #120418, #141790 ) ;
#32763 = DIRECTION ( 'NONE',  ( 0.7071067811865487940, -0.7071067811865463515, 0.000000000000000000 ) ) ;
#32765 = EDGE_CURVE ( 'NONE', #99565, #118931, #122090, .T. ) ;
#32764 = STYLED_ITEM ( 'NONE', ( #62767 ), #74598 ) ;
#32766 = AXIS2_PLACEMENT_3D ( 'NONE', #25605, #91591, #115434 ) ;
#32767 = VECTOR ( 'NONE', #36470, 999.9999999999998863 ) ;
#32768 = PLANE ( 'NONE',  #71062 ) ;
#32769 = DIRECTION ( 'NONE',  ( 2.110369192185896011E-16, -1.000000000000000000, 0.000000000000000000 ) ) ;
#32770 = DIRECTION ( 'NONE',  ( 0.7071067811865487940, 0.7071067811865463515, 0.000000000000000000 ) ) ;
#32771 = CARTESIAN_POINT ( 'NONE',  ( -6.707106781186491062, -3.740707523384241728, 5.000000000000000000 ) ) ;
#32772 = LINE ( 'NONE', #121171, #67228 ) ;
#32773 = ORIENTED_EDGE ( 'NONE', *, *, #91067, .T. ) ;
#32774 =( GEOMETRIC_REPRESENTATION_CONTEXT ( 3 ) GLOBAL_UNCERTAINTY_ASSIGNED_CONTEXT ( ( #47664 ) ) GLOBAL_UNIT_ASSIGNED_CONTEXT ( ( #127656, #41331, #74722 ) ) REPRESENTATION_CONTEXT ( 'NONE', 'WORKASPACE' ) );
#32775 = CIRCLE ( 'NONE', #88344, 1.320799999999990870 ) ;
#32776 = ORIENTED_EDGE ( 'NONE', *, *, #81870, .F. ) ;
#32777 = AXIS2_PLACEMENT_3D ( 'NONE', #137670, #127484, #125355 ) ;
#32778 = VERTEX_POINT ( 'NONE', #111965 ) ;
#32779 = VECTOR ( 'NONE', #12345, 1000.000000000000000 ) ;
#32780 = DIRECTION ( 'NONE',  ( 0.7071067811865486830, -0.7071067811865464625, -0.000000000000000000 ) ) ;
#32781 = LINE ( 'NONE', #21161, #12029 ) ;
#32782 = VERTEX_POINT ( 'NONE', #90181 ) ;
#32783 = AXIS2_PLACEMENT_3D ( 'NONE', #142101, #76852, #42788 ) ;
#32784 = VERTEX_POINT ( 'NONE', #80072 ) ;
#32785 = CARTESIAN_POINT ( 'NONE',  ( 166.8575281714868481, 26.96999999999994557, -32.10255624693994747 ) ) ;
#32786 = LINE ( 'NONE', #63971, #73398 ) ;
#32787 = DIRECTION ( 'NONE',  ( 0.000000000000000000, 1.000000000000000000, 0.000000000000000000 ) ) ;
#32788 = VERTEX_POINT ( 'NONE', #113350 ) ;
#32789 = VECTOR ( 'NONE', #21972, 999.9999999999998863 ) ;
#32790 = CARTESIAN_POINT ( 'NONE',  ( -34.92500000000001137, 5.087954687542278975, -1.493867085284239948 ) ) ;
#32791 = ADVANCED_FACE ( 'NONE', ( #102521 ), #101996, .F. ) ;
#32792 = CARTESIAN_POINT ( 'NONE',  ( 10.49999999999992539, -1.592773361805362109, -6.492772025301252192 ) ) ;
#32793 = ADVANCED_FACE ( 'NONE', ( #58551 ), #23718, .F. ) ;
#32794 = CARTESIAN_POINT ( 'NONE',  ( 19.02540314143521982, 2.126176841940962348, 7.934999999999989839 ) ) ;
#32795 = DIRECTION ( 'NONE',  ( 1.000000000000000000, 1.224606353822377258E-16, 0.000000000000000000 ) ) ;
#32796 = VERTEX_POINT ( 'NONE', #80268 ) ;
#32797 = CARTESIAN_POINT ( 'NONE',  ( 117.4537635252314516, -6.109999999999999432, -3.741295971395163529E-16 ) ) ;
#32798 = VECTOR ( 'NONE', #31490, 1000.000000000000000 ) ;
#32799 = DIRECTION ( 'NONE',  ( -0.7071067811865486830, -0.7071067811865464625, 0.000000000000000000 ) ) ;
#32800 = DIRECTION ( 'NONE',  ( -0.7071067811865487940, 0.7071067811865463515, -0.000000000000000000 ) ) ;
#32802 = VERTEX_POINT ( 'NONE', #46956 ) ;
#32801 = DIRECTION ( 'NONE',  ( -0.000000000000000000, 0.3543493200069153248, 0.9351131265310292928 ) ) ;
#32803 = DIRECTION ( 'NONE',  ( -0.000000000000000000, 0.000000000000000000, 1.000000000000000000 ) ) ;
#32804 = ORIENTED_EDGE ( 'NONE', *, *, #71617, .T. ) ;
#32805 = CARTESIAN_POINT ( 'NONE',  ( 24.18398860626899705, 28.73617430169804265, 5.000000000000000000 ) ) ;
#32806 = EDGE_CURVE ( 'NONE', #35917, #101850, #111983, .T. ) ;
#32807 = LINE ( 'NONE', #24051, #67872 ) ;
#32808 = CARTESIAN_POINT ( 'NONE',  ( 48.29974487139158867, -27.71228299555239971, 4.000000000000000000 ) ) ;
#32809 = VERTEX_POINT ( 'NONE', #124458 ) ;
#32810 = VECTOR ( 'NONE', #85278, 1000.000000000000000 ) ;
#32811 = VECTOR ( 'NONE', #130669, 999.9999999999998863 ) ;
#32812 = LINE ( 'NONE', #23309, #9432 ) ;
#32813 = DIRECTION ( 'NONE',  ( 0.000000000000000000, 1.000000000000000000, 0.000000000000000000 ) ) ;
#32814 = ORIENTED_EDGE ( 'NONE', *, *, #73298, .F. ) ;
#32815 = CARTESIAN_POINT ( 'NONE',  ( 151.4000000000000057, -16.48000000000005016, -33.92499999999998295 ) ) ;
#32816 = AXIS2_PLACEMENT_3D ( 'NONE', #58006, #15147, #137686 ) ;
#32817 = CARTESIAN_POINT ( 'NONE',  ( 31.49999999999977973, 12.05218569542904206, 5.000000000000000000 ) ) ;
#32818 = ORIENTED_EDGE ( 'NONE', *, *, #49999, .F. ) ;
#32819 = DIRECTION ( 'NONE',  ( -0.3543493200069162685, -0.000000000000000000, -0.9351131265310288487 ) ) ;
#32821 = VERTEX_POINT ( 'NONE', #79586 ) ;
#32820 = DIRECTION ( 'NONE',  ( 0.000000000000000000, -1.000000000000000000, 0.000000000000000000 ) ) ;
#32822 = ORIENTED_EDGE ( 'NONE', *, *, #8071, .F. ) ;
#32823 = DIRECTION ( 'NONE',  ( -0.7071067811865486830, -0.7071067811865464625, 0.000000000000000000 ) ) ;
#32824 = DIRECTION ( 'NONE',  ( 0.7071067811865486830, -0.7071067811865464625, -0.000000000000000000 ) ) ;
#32825 = VECTOR ( 'NONE', #30040, 1000.000000000000114 ) ;
#32826 = VERTEX_POINT ( 'NONE', #33897 ) ;
#32827 = CARTESIAN_POINT ( 'NONE',  ( 2.999999999999978240, -11.35517001088072142, -1.126524801160101230 ) ) ;
#32828 = CARTESIAN_POINT ( 'NONE',  ( -29.99999999999979039, -5.527737879153217015, -7.983877177622302312 ) ) ;
#32829 = CARTESIAN_POINT ( 'NONE',  ( 9.328169399223463998, -6.740707523384218192, 4.000000000000000000 ) ) ;
#32830 = VERTEX_POINT ( 'NONE', #89685 ) ;
#32831 = PRODUCT ( '1.5 Handle Ball', '1.5 Handle Ball', '', ( #126485 ) ) ;
#32832 = CARTESIAN_POINT ( 'NONE',  ( 20.99999999999985789, 13.55218569542903140, 5.000000000000000000 ) ) ;
#32833 = EDGE_CURVE ( 'NONE', #96928, #84615, #78114, .T. ) ;
#32835 = ADVANCED_FACE ( 'NONE', ( #2659 ), #3365, .T. ) ;
#32834 = CARTESIAN_POINT ( 'NONE',  ( 36.29974487139159578, -27.71228299555231445, 4.000000000000000000 ) ) ;
#32836 = CARTESIAN_POINT ( 'NONE',  ( -17.61782366839360847, 8.969638207445433054, 4.000000000000000000 ) ) ;
#32837 = AXIS2_PLACEMENT_3D ( 'NONE', #132866, #47313, #133560 ) ;
#32838 = CARTESIAN_POINT ( 'NONE',  ( -34.49999999999976552, 21.43112307739196254, 4.000000000000000000 ) ) ;
#32839 = CARTESIAN_POINT ( 'NONE',  ( 41.32876352523144448, 0.000000000000000000, -6.109999999999999432 ) ) ;
#32840 = FACE_OUTER_BOUND ( 'NONE', #103371, .T. ) ;
#32841 = ORIENTED_EDGE ( 'NONE', *, *, #53790, .F. ) ;
#32842 = ORIENTED_EDGE ( 'NONE', *, *, #91289, .T. ) ;
#32843 = DIRECTION ( 'NONE',  ( 0.3543493200069162685, -0.000000000000000000, -0.9351131265310288487 ) ) ;
#32844 = EDGE_LOOP ( 'NONE', ( #135965, #31890, #123661, #31192 ) ) ;
#32845 = VECTOR ( 'NONE', #127418, 1000.000000000000000 ) ;
#32846 = ORIENTED_EDGE ( 'NONE', *, *, #130962, .F. ) ;
#32847 = AXIS2_PLACEMENT_3D ( 'NONE', #70629, #126379, #94460 ) ;
#32848 = LINE ( 'NONE', #42297, #108035 ) ;
#32849 = DIRECTION ( 'NONE',  ( 0.7071067811865487940, 0.7071067811865463515, 0.000000000000000000 ) ) ;
#32850 = ORIENTED_EDGE ( 'NONE', *, *, #33067, .T. ) ;
#32851 = CARTESIAN_POINT ( 'NONE',  ( -28.49999999999979750, 16.46639925780209168, 5.000000000000000000 ) ) ;
#32852 = CARTESIAN_POINT ( 'NONE',  ( 33.70710678118631165, 2.259292476615694323, 5.000000000000000000 ) ) ;
#32853 = EDGE_CURVE ( 'NONE', #31006, #2581, #34601, .T. ) ;
#32854 = DIRECTION ( 'NONE',  ( 0.3543493200069162685, -0.000000000000000000, -0.9351131265310288487 ) ) ;
#32855 = PLANE ( 'NONE',  #122868 ) ;
#32856 = CARTESIAN_POINT ( 'NONE',  ( 124.8337635252314470, 6.110000000000001208, 1.122388791418549305E-15 ) ) ;
#32857 = EDGE_CURVE ( 'NONE', #93902, #3598, #111432, .T. ) ;
#32858 = EDGE_LOOP ( 'NONE', ( #73386, #18242, #123655, #29469, #123225 ) ) ;
#32859 = DIRECTION ( 'NONE',  ( -0.7071067811865486830, -0.7071067811865464625, 0.000000000000000000 ) ) ;
#32860 = DIRECTION ( 'NONE',  ( -0.000000000000000000, -0.3543493200069152693, 0.9351131265310292928 ) ) ;
#32861 = DIRECTION ( 'NONE',  ( -0.000000000000000000, 0.000000000000000000, 1.000000000000000000 ) ) ;
#32862 = DIRECTION ( 'NONE',  ( 0.7071067811865487940, 0.7071067811865463515, -0.000000000000000000 ) ) ;
#32863 = FACE_OUTER_BOUND ( 'NONE', #78272, .T. ) ;
#32864 = CARTESIAN_POINT ( 'NONE',  ( 0.5685132242927012358, -0.3999999999999997446, -2.467792535850613866 ) ) ;
#32865 = DIRECTION ( 'NONE',  ( 0.000000000000000000, 0.000000000000000000, 1.000000000000000000 ) ) ;
#32866 = ADVANCED_FACE ( 'NONE', ( #67232 ), #45507, .F. ) ;
#32868 = EDGE_CURVE ( 'NONE', #115465, #49398, #36728, .T. ) ;
#32867 = CARTESIAN_POINT ( 'NONE',  ( 54.32919371712956291, -3.975000000000001865, 6.884901960086284411 ) ) ;
#32869 = PLANE ( 'NONE',  #93016 ) ;
#32870 = CYLINDRICAL_SURFACE ( 'NONE', #124892, 2.500000000000000444 ) ;
#32871 = ORIENTED_EDGE ( 'NONE', *, *, #118916, .F. ) ;
#32872 = EDGE_LOOP ( 'NONE', ( #58309, #94468, #4134, #49446 ) ) ;
#32873 = CARTESIAN_POINT ( 'NONE',  ( 47.52083333333332860, 7.949999999999999289, 2.130196079827431532 ) ) ;
#32874 = ADVANCED_FACE ( 'NONE', ( #12113 ), #78833, .F. ) ;
#32875 = DIRECTION ( 'NONE',  ( 0.7071067811865487940, -0.7071067811865463515, 0.000000000000000000 ) ) ;
#32876 = CARTESIAN_POINT ( 'NONE',  ( -34.49999999999975131, 16.08746187583907528, 4.000000000000000000 ) ) ;
#32877 = VERTEX_POINT ( 'NONE', #123043 ) ;
#32878 = CIRCLE ( 'NONE', #30688, 5.968999999999998529 ) ;
#32879 = VECTOR ( 'NONE', #82021, 1000.000000000000227 ) ;
#32880 = CARTESIAN_POINT ( 'NONE',  ( 127.0000000000000000, -4.071459123471990793, -4.960746789751230068 ) ) ;
#32881 = LINE ( 'NONE', #119826, #46989 ) ;
#32882 = COLOUR_RGB ( '', 0.40784314, 0.44705882, 0.49803922) ;
#32883 = EDGE_CURVE ( 'NONE', #119795, #22356, #47659, .T. ) ;
#32884 = VECTOR ( 'NONE', #23249, 1000.000000000000000 ) ;
#32885 = CARTESIAN_POINT ( 'NONE',  ( 44.18793019189810423, 6.110000000000002984, -1.637169565754156730 ) ) ;
#32886 = VERTEX_POINT ( 'NONE', #69384 ) ;
#32887 = SURFACE_STYLE_FILL_AREA ( #65524 ) ;
#32888 = ORIENTED_EDGE ( 'NONE', *, *, #119476, .F. ) ;
#32889 = ORIENTED_EDGE ( 'NONE', *, *, #99630, .T. ) ;
#32890 = VECTOR ( 'NONE', #140353, 999.9999999999998863 ) ;
#32891 = VECTOR ( 'NONE', #120711, 1000.000000000000000 ) ;
#32892 = VECTOR ( 'NONE', #81764, 1000.000000000000000 ) ;
#32893 = DIRECTION ( 'NONE',  ( -0.6830127018922181881, 0.6830127018922202975, -0.2588190451025214056 ) ) ;
#32894 = EDGE_CURVE ( 'NONE', #106547, #77537, #514, .T. ) ;
#32895 = LINE ( 'NONE', #21971, #31455 ) ;
#32896 = DIRECTION ( 'NONE',  ( 0.7071067811865486830, -0.7071067811865464625, -0.000000000000000000 ) ) ;
#32897 = CARTESIAN_POINT ( 'NONE',  ( -20.99451991528748707, 28.92564299267952777, 4.000000000000000000 ) ) ;
#32898 = ORIENTED_EDGE ( 'NONE', *, *, #93750, .F. ) ;
#32899 = DIRECTION ( 'NONE',  ( -0.7071067811865486830, -0.7071067811865464625, -0.000000000000000000 ) ) ;
#32901 = ORIENTED_EDGE ( 'NONE', *, *, #7903, .T. ) ;
#32900 = CARTESIAN_POINT ( 'NONE',  ( 5.994519915287488843, 28.92564299267942118, 4.000000000000000000 ) ) ;
#32902 = CARTESIAN_POINT ( 'NONE',  ( 81.22959685856476142, -6.110000000000000320, -1.637169565754161393 ) ) ;
#32903 = DIRECTION ( 'NONE',  ( -0.7071067811865487940, 0.7071067811865463515, -0.000000000000000000 ) ) ;
#32904 = LINE ( 'NONE', #55352, #98688 ) ;
#32905 = LINE ( 'NONE', #142362, #49420 ) ;
#32906 = EDGE_CURVE ( 'NONE', #70409, #39875, #90400, .T. ) ;
#32907 = CARTESIAN_POINT ( 'NONE',  ( 16.49999999999989342, 10.08746187583914278, 4.000000000000000000 ) ) ;
#32908 = EDGE_LOOP ( 'NONE', ( #136686, #75537, #74017, #24261 ) ) ;
#32909 = CARTESIAN_POINT ( 'NONE',  ( 30.70710678118632941, 2.259292476615694323, 5.000000000000000000 ) ) ;
#32910 = CARTESIAN_POINT ( 'NONE',  ( 65.39126352523145158, -4.472830434245839371, -4.472830434245839371 ) ) ;
#32911 = DIRECTION ( 'NONE',  ( 0.7071067811865487940, 0.7071067811865463515, 0.000000000000000000 ) ) ;
#32912 = EDGE_CURVE ( 'NONE', #42695, #92475, #91145, .T. ) ;
#32913 = LINE ( 'NONE', #45226, #96385 ) ;
#32914 = ORIENTED_EDGE ( 'NONE', *, *, #7175, .F. ) ;
#32915 = VERTEX_POINT ( 'NONE', #13527 ) ;
#32916 = PLANE ( 'NONE',  #2892 ) ;
#32917 = VERTEX_POINT ( 'NONE', #113569 ) ;
#32918 = VECTOR ( 'NONE', #116532, 1000.000000000000000 ) ;
#32919 = EDGE_CURVE ( 'NONE', #53913, #98731, #102719, .T. ) ;
#32920 = ORIENTED_EDGE ( 'NONE', *, *, #30820, .T. ) ;
#32921 = VECTOR ( 'NONE', #121484, 1000.000000000000000 ) ;
#32922 = CARTESIAN_POINT ( 'NONE',  ( 11.99999999999992184, 13.93112307739204425, 4.000000000000000000 ) ) ;
#32924 = ADVANCED_FACE ( 'NONE', ( #51199 ), #128056, .F. ) ;
#32923 = ORIENTED_EDGE ( 'NONE', *, *, #140769, .F. ) ;
#32925 = AXIS2_PLACEMENT_3D ( 'NONE', #37596, #69523, #93387 ) ;
#32926 = CARTESIAN_POINT ( 'NONE',  ( -27.29974487139158512, -27.71228299555225405, 4.000000000000000000 ) ) ;
#32927 = DIRECTION ( 'NONE',  ( 0.000000000000000000, -1.000000000000000000, 0.000000000000000000 ) ) ;
#32928 = AXIS2_PLACEMENT_3D ( 'NONE', #33585, #121266, #22638 ) ;
#32929 = EDGE_CURVE ( 'NONE', #114916, #3959, #28009, .T. ) ;
#32930 = LINE ( 'NONE', #111892, #102127 ) ;
#32931 = FACE_BOUND ( 'NONE', #58786, .T. ) ;
#32932 = CARTESIAN_POINT ( 'NONE',  ( -16.00193056682086379, -22.22500000000000142, 4.500000000000000888 ) ) ;
#32933 = CARTESIAN_POINT ( 'NONE',  ( 40.76669371712956291, -7.949999999999998401, 2.130196079827423983 ) ) ;
#32934 = DIRECTION ( 'NONE',  ( 0.7071067811865486830, -0.7071067811865464625, -0.000000000000000000 ) ) ;
#32936 = ORIENTED_EDGE ( 'NONE', *, *, #89146, .F. ) ;
#32935 = CARTESIAN_POINT ( 'NONE',  ( 51.12086038379622011, -6.884901960086286188, 3.974999999999997424 ) ) ;
#32937 = PRESENTATION_LAYER_ASSIGNMENT (  '', '', ( #74625 ) ) ;
#32938 = CARTESIAN_POINT ( 'NONE',  ( 15.29974487139158867, -27.71228299555216879, 4.000000000000000000 ) ) ;
#32939 = CONTEXT_DEPENDENT_SHAPE_REPRESENTATION ( #124459, #126776 ) ;
#32940 = ORIENTED_EDGE ( 'NONE', *, *, #89196, .T. ) ;
#32941 = ORIENTED_EDGE ( 'NONE', *, *, #75131, .F. ) ;
#32942 = CARTESIAN_POINT ( 'NONE',  ( 75.74543019189810877, -5.291415217122918513, -3.055000000000000160 ) ) ;
#32943 = ORIENTED_EDGE ( 'NONE', *, *, #141001, .T. ) ;
#32944 = DIRECTION ( 'NONE',  ( -0.7071067811865486830, 0.7071067811865463515, 0.000000000000000000 ) ) ;
#32945 = EDGE_CURVE ( 'NONE', #55371, #130377, #27699, .T. ) ;
#32946 = DIRECTION ( 'NONE',  ( -0.7071067811865486830, -0.7071067811865464625, -0.000000000000000000 ) ) ;
#32947 = VECTOR ( 'NONE', #5569, 1000.000000000000227 ) ;
#32948 = ORIENTED_EDGE ( 'NONE', *, *, #124506, .T. ) ;
#32949 = DIRECTION ( 'NONE',  ( -0.7071067811865486830, -0.7071067811865464625, 0.000000000000000000 ) ) ;
#32950 = AXIS2_PLACEMENT_3D ( 'NONE', #42658, #28902, #106409 ) ;
#32951 = EDGE_CURVE ( 'NONE', #59015, #76484, #27271, .T. ) ;
#32952 = CARTESIAN_POINT ( 'NONE',  ( -26.33153258840125588, -18.74070752338408496, 20.73178291233834969 ) ) ;
#32953 = LINE ( 'NONE', #47930, #50663 ) ;
#32954 = DIRECTION ( 'NONE',  ( 0.3543493200069162685, -0.000000000000000000, -0.9351131265310288487 ) ) ;
#32955 = CARTESIAN_POINT ( 'NONE',  ( -21.29974487139158512, -27.71228299555221142, 4.000000000000000000 ) ) ;
#32956 = DIRECTION ( 'NONE',  ( 0.6830127018922181881, 0.6830127018922202975, -0.2588190451025214056 ) ) ;
#32957 = LINE ( 'NONE', #10435, #70154 ) ;
#32958 = DIRECTION ( 'NONE',  ( 0.000000000000000000, -1.000000000000000000, 0.000000000000000000 ) ) ;
#32959 = ORIENTED_EDGE ( 'NONE', *, *, #58131, .F. ) ;
#32960 = AXIS2_PLACEMENT_3D ( 'NONE', #100025, #143511, #33375 ) ;
#32961 = FACE_OUTER_BOUND ( 'NONE', #3191, .T. ) ;
#32962 = ORIENTED_EDGE ( 'NONE', *, *, #77346, .T. ) ;
#32963 = CARTESIAN_POINT ( 'NONE',  ( -18.18398860626898994, 28.73617430169800002, 5.000000000000000000 ) ) ;
#32964 = PRESENTATION_STYLE_ASSIGNMENT (( #112629 ) ) ;
#32965 = ORIENTED_EDGE ( 'NONE', *, *, #109148, .T. ) ;
#32966 = VERTEX_POINT ( 'NONE', #137491 ) ;
#32967 = ADVANCED_FACE ( 'NONE', ( #136751 ), #128740, .F. ) ;
#32968 = CARTESIAN_POINT ( 'NONE',  ( 26.54209685856477563, 5.291415217122923842, -3.054999999999996163 ) ) ;
#32969 = VECTOR ( 'NONE', #77600, 1000.000000000000000 ) ;
#32970 = ORIENTED_EDGE ( 'NONE', *, *, #75996, .F. ) ;
#32971 = CARTESIAN_POINT ( 'NONE',  ( 34.42499999999998295, 22.22500000000000142, 5.000000000000000000 ) ) ;
#32972 = EDGE_CURVE ( 'NONE', #69819, #15156, #28738, .T. ) ;
#32973 = LINE ( 'NONE', #142430, #100226 ) ;
#32974 = CARTESIAN_POINT ( 'NONE',  ( 27.89997294953710494, 4.461849672132297329, -4.461849672132302658 ) ) ;
#32975 = CARTESIAN_POINT ( 'NONE',  ( 8.585466709768445170, 2.500000000000003109, 3.061616997868386592E-16 ) ) ;
#32976 = VERTEX_POINT ( 'NONE', #92522 ) ;
#32977 = CARTESIAN_POINT ( 'NONE',  ( 32.99999999999977973, -7.447814304570745669, 5.000000000000000000 ) ) ;
#32978 = ORIENTED_EDGE ( 'NONE', *, *, #97452, .T. ) ;
#32979 = CARTESIAN_POINT ( 'NONE',  ( -51.48921356237309510, -27.52281430457091460, 5.000000000000000000 ) ) ;
#32980 = CARTESIAN_POINT ( 'NONE',  ( -32.99999999999976552, 2.966399257802230682, 5.000000000000000000 ) ) ;
#32981 = VECTOR ( 'NONE', #74551, 1000.000000000000000 ) ;
#32982 = VECTOR ( 'NONE', #51878, 1000.000000000000000 ) ;
#32984 = ORIENTED_EDGE ( 'NONE', *, *, #49765, .F. ) ;
#32983 = CARTESIAN_POINT ( 'NONE',  ( -2.700255128608413990, -27.71228299555204089, 4.000000000000000000 ) ) ;
#32985 = AXIS2_PLACEMENT_3D ( 'NONE', #108615, #41989, #10737 ) ;
#32986 = ORIENTED_EDGE ( 'NONE', *, *, #50570, .F. ) ;
#32987 = CARTESIAN_POINT ( 'NONE',  ( 115.2875270504628986, 0.000000000000000000, -7.949999999999998401 ) ) ;
#32988 = LINE ( 'NONE', #14763, #44587 ) ;
#32989 = DIRECTION ( 'NONE',  ( 0.7071067811865487940, 0.7071067811865463515, 0.000000000000000000 ) ) ;
#32991 = VERTEX_POINT ( 'NONE', #114966 ) ;
#32990 = AXIS2_PLACEMENT_3D ( 'NONE', #50039, #94231, #127591 ) ;
#32992 = EDGE_CURVE ( 'NONE', #22931, #27577, #83851, .T. ) ;
#32993 = FACE_OUTER_BOUND ( 'NONE', #103642, .T. ) ;
#32994 = ORIENTED_EDGE ( 'NONE', *, *, #17095, .F. ) ;
#32995 = ORIENTED_EDGE ( 'NONE', *, *, #78088, .F. ) ;
#32996 = DIRECTION ( 'NONE',  ( 0.7071067811865486830, -0.7071067811865464625, -0.000000000000000000 ) ) ;
#32997 = LINE ( 'NONE', #28858, #81103 ) ;
#32998 = VECTOR ( 'NONE', #87236, 1000.000000000000000 ) ;
#32999 = VECTOR ( 'NONE', #14085, 1000.000000000000000 ) ;
#33000 = PRESENTATION_LAYER_ASSIGNMENT (  '', '', ( #137067 ) ) ;
#33001 = CARTESIAN_POINT ( 'NONE',  ( -1.499999999999990896, -12.66682484999666514, -0.6294897503863975396 ) ) ;
#33002 = CARTESIAN_POINT ( 'NONE',  ( -32.99999999999976552, -19.44781430457063465, 5.000000000000000000 ) ) ;
#33003 = PLANE ( 'NONE',  #102419 ) ;
#33004 = CARTESIAN_POINT ( 'NONE',  ( 45.29974487139158867, -27.71228299555237840, 4.000000000000000000 ) ) ;
#33005 = CARTESIAN_POINT ( 'NONE',  ( -23.99451991528749062, 28.92564299267954908, 4.000000000000000000 ) ) ;
#33006 = EDGE_CURVE ( 'NONE', #75731, #134905, #139839, .T. ) ;
#33007 = ORIENTED_EDGE ( 'NONE', *, *, #28259, .F. ) ;
#33008 = CARTESIAN_POINT ( 'NONE',  ( 97.35002705046287019, -5.819803920172573086, -5.819803920172573086 ) ) ;
#33009 = ORIENTED_EDGE ( 'NONE', *, *, #12518, .F. ) ;
#33010 = CARTESIAN_POINT ( 'NONE',  ( -12.20000000000000107, -34.64999999999999147, 17.49210858042622263 ) ) ;
#33011 = CARTESIAN_POINT ( 'NONE',  ( -0.4587635252314472556, 0.000000000000000000, 7.934999999999990727 ) ) ;
#33012 = CARTESIAN_POINT ( 'NONE',  ( -2.483345613589531542, 22.22500000000000142, 4.500000000000000888 ) ) ;
#33013 = ORIENTED_EDGE ( 'NONE', *, *, #74692, .T. ) ;
#33014 = FACE_OUTER_BOUND ( 'NONE', #107807, .T. ) ;
#33015 = CARTESIAN_POINT ( 'NONE',  ( -17.20710678118642178, -5.240707523384227073, 5.000000000000000000 ) ) ;
#33016 = DIRECTION ( 'NONE',  ( -0.7071067811865487940, 0.7071067811865463515, 0.000000000000000000 ) ) ;
#33017 = VERTEX_POINT ( 'NONE', #38183 ) ;
#33018 = FACE_OUTER_BOUND ( 'NONE', #20180, .T. ) ;
#33019 = LINE ( 'NONE', #43868, #139161 ) ;
#33020 = UNCERTAINTY_MEASURE_WITH_UNIT (LENGTH_MEASURE( 1.000000000000000082E-05 ), #52138, 'distance_accuracy_value', 'NONE');
#33021 = DIRECTION ( 'NONE',  ( 0.7071067811865486830, -0.7071067811865464625, -0.000000000000000000 ) ) ;
#33022 = CARTESIAN_POINT ( 'NONE',  ( 52.04166666666666430, -3.975000000000002753, 6.884901960086286188 ) ) ;
#33023 = CARTESIAN_POINT ( 'NONE',  ( 26.99451991528749417, 28.92564299267956685, 4.000000000000000000 ) ) ;
#33024 = CARTESIAN_POINT ( 'NONE',  ( 67.57876352523145158, -7.482591942790327058E-16, 6.109999999999999432 ) ) ;
#33025 = VECTOR ( 'NONE', #72196, 1000.000000000000227 ) ;
#33026 = LINE ( 'NONE', #101086, #115849 ) ;
#33027 = CARTESIAN_POINT ( 'NONE',  ( 50.99451991528749062, 28.92564299267973738, 4.000000000000000000 ) ) ;
#33028 = CARTESIAN_POINT ( 'NONE',  ( 33.03752705046289151, -9.735942053221456900E-16, 7.949999999999998401 ) ) ;
#33029 = LINE ( 'NONE', #122123, #58042 ) ;
#33030 = STYLED_ITEM ( 'NONE', ( #57767 ), #86018 ) ;
#33031 = EDGE_LOOP ( 'NONE', ( #74336, #62964, #76995, #107618, #86423 ) ) ;
#33032 = CARTESIAN_POINT ( 'NONE',  ( -23.20710678118638270, 9.759292476615620160, 5.000000000000000000 ) ) ;
#33033 = EDGE_CURVE ( 'NONE', #56766, #2192, #5510, .T. ) ;
#33034 = ORIENTED_EDGE ( 'NONE', *, *, #126966, .F. ) ;
#33035 = PRESENTATION_LAYER_ASSIGNMENT (  '', '', ( #19123 ) ) ;
#33036 = DIRECTION ( 'NONE',  ( -0.7071067811865487940, 0.7071067811865463515, -0.000000000000000000 ) ) ;
#33038 = VECTOR ( 'NONE', #31788, 1000.000000000000000 ) ;
#33037 = DIRECTION ( 'NONE',  ( -0.000000000000000000, -0.3543493200069152693, 0.9351131265310292928 ) ) ;
#33039 = CARTESIAN_POINT ( 'NONE',  ( 5.281315875828549444, 2.500000000000000444, 0.000000000000000000 ) ) ;
#33040 = DIRECTION ( 'NONE',  ( -0.7071067811865487940, 0.7071067811865463515, -0.000000000000000000 ) ) ;
#33041 = CARTESIAN_POINT ( 'NONE',  ( -8.816011393731004731, 28.73617430169781173, 5.000000000000000000 ) ) ;
#33042 = CARTESIAN_POINT ( 'NONE',  ( -50.99451991528749062, 28.92564299267973738, 4.000000000000000000 ) ) ;
#33043 = CARTESIAN_POINT ( 'NONE',  ( 0.005480084712502889671, 28.92564299267938210, 4.000000000000000000 ) ) ;
#33044 = EDGE_CURVE ( 'NONE', #2192, #36781, #49789, .T. ) ;
#33045 = EDGE_CURVE ( 'NONE', #38188, #121396, #82399, .T. ) ;
#33046 = ORIENTED_EDGE ( 'NONE', *, *, #13865, .T. ) ;
#33047 = ORIENTED_EDGE ( 'NONE', *, *, #142211, .F. ) ;
#33048 = CARTESIAN_POINT ( 'NONE',  ( 1.499999999999990896, -7.533600742197664069, 5.000000000000000000 ) ) ;
#33049 =( NAMED_UNIT ( * ) SI_UNIT ( $, .STERADIAN. ) SOLID_ANGLE_UNIT ( ) );
#33050 = UNCERTAINTY_MEASURE_WITH_UNIT (LENGTH_MEASURE( 1.000000000000000082E-05 ), #33490, 'distance_accuracy_value', 'NONE');
#33051 = CARTESIAN_POINT ( 'NONE',  ( -19.05000000000000071, 3.174999999999997158, 4.000000000000000000 ) ) ;
#33052 = CARTESIAN_POINT ( 'NONE',  ( 16.52497294953710849, -4.461849672132299993, -4.461849672132299105 ) ) ;
#33053 = EDGE_CURVE ( 'NONE', #122674, #122361, #50480, .T. ) ;
#33055 = ADVANCED_FACE ( 'NONE', ( #71523 ), #38883, .F. ) ;
#33054 = CARTESIAN_POINT ( 'NONE',  ( 82.62086038379624142, -6.884901960086286188, 3.974999999999997424 ) ) ;
#33056 = CARTESIAN_POINT ( 'NONE',  ( -32.91685193227049666, 21.75929247661549581, 7.311836541447975790 ) ) ;
#33057 = DIRECTION ( 'NONE',  ( -0.3543493200069163240, -0.000000000000000000, 0.9351131265310288487 ) ) ;
#33059 = ADVANCED_FACE ( 'NONE', ( #127307 ), #72979, .F. ) ;
#33058 = ORIENTED_EDGE ( 'NONE', *, *, #100819, .T. ) ;
#33060 = CARTESIAN_POINT ( 'NONE',  ( 76.83333333333334281, -6.884901960086287964, 3.974999999999998312 ) ) ;
#33061 = DIRECTION ( 'NONE',  ( -0.6830127018922181881, 0.6830127018922202975, -0.2588190451025214056 ) ) ;
#33062 = EDGE_CURVE ( 'NONE', #121198, #96033, #26401, .T. ) ;
#33063 = LINE ( 'NONE', #32317, #110906 ) ;
#33065 = VECTOR ( 'NONE', #101156, 1000.000000000000000 ) ;
#33064 = DIRECTION ( 'NONE',  ( 0.6830127018922180770, -0.6830127018922204085, -0.2588190451025213501 ) ) ;
#33066 = AXIS2_PLACEMENT_3D ( 'NONE', #27283, #104857, #59951 ) ;
#33067 = EDGE_CURVE ( 'NONE', #5308, #139710, #117135, .T. ) ;
#33068 = ORIENTED_EDGE ( 'NONE', *, *, #32077, .T. ) ;
#33069 = CARTESIAN_POINT ( 'NONE',  ( 19.93618820137057668, -6.269999999999995133, -40.00000000000000000 ) ) ;
#33071 = ORIENTED_EDGE ( 'NONE', *, *, #2782, .T. ) ;
#33070 = ADVANCED_FACE ( 'NONE', ( #9051 ), #76531, .F. ) ;
#33072 = DIRECTION ( 'NONE',  ( -0.7071067811865486830, -0.7071067811865464625, 0.000000000000000000 ) ) ;
#33073 = CARTESIAN_POINT ( 'NONE',  ( 79.18793019189810423, 6.110000000000002984, -1.637169565754156730 ) ) ;
#33074 = PLANE ( 'NONE',  #82506 ) ;
#33075 = ORIENTED_EDGE ( 'NONE', *, *, #30382, .F. ) ;
#33076 = FACE_OUTER_BOUND ( 'NONE', #34027, .T. ) ;
#33077 = PLANE ( 'NONE',  #91573 ) ;
#33078 = EDGE_CURVE ( 'NONE', #121198, #11327, #70423, .T. ) ;
#33079 = DIRECTION ( 'NONE',  ( 0.3543493200069162685, -0.000000000000000000, -0.9351131265310288487 ) ) ;
#33080 = CARTESIAN_POINT ( 'NONE',  ( -2.395137668124769359, 21.75929247661549937, 21.32995629748187483 ) ) ;
#33081 = CARTESIAN_POINT ( 'NONE',  ( 8.510786437626906675, -27.52281430457049183, 5.000000000000000000 ) ) ;
#33083 = ORIENTED_EDGE ( 'NONE', *, *, #45574, .F. ) ;
#33082 = CARTESIAN_POINT ( 'NONE',  ( -15.97910837819034668, 22.22500000000000142, -2.179306570123547893 ) ) ;
#33084 = DIRECTION ( 'NONE',  ( 0.3543493200069162685, -0.000000000000000000, -0.9351131265310288487 ) ) ;
#33085 = VECTOR ( 'NONE', #135567, 1000.000000000000000 ) ;
#33086 = EDGE_CURVE ( 'NONE', #92724, #103666, #21419, .T. ) ;
#33087 = CARTESIAN_POINT ( 'NONE',  ( 34.92499999999998295, -21.72500000000000142, 5.000000000000000000 ) ) ;
#33088 = ORIENTED_EDGE ( 'NONE', *, *, #123194, .F. ) ;
#33089 = ORIENTED_EDGE ( 'NONE', *, *, #5648, .F. ) ;
#33090 = CARTESIAN_POINT ( 'NONE',  ( 64.45876352523144703, 0.000000000000000000, -6.110000000000001208 ) ) ;
#33091 = ORIENTED_EDGE ( 'NONE', *, *, #77083, .T. ) ;
#33092 = LINE ( 'NONE', #392, #33718 ) ;
#33093 = DIRECTION ( 'NONE',  ( -0.000000000000000000, -0.3543493200069152693, 0.9351131265310292928 ) ) ;
#33094 = DIRECTION ( 'NONE',  ( -0.000000000000000000, -1.016133275908817741E-16, 1.000000000000000000 ) ) ;
#33095 = DIRECTION ( 'NONE',  ( -0.000000000000000000, 0.3543493200069153248, 0.9351131265310292928 ) ) ;
#33096 = ORIENTED_EDGE ( 'NONE', *, *, #63013, .F. ) ;
#33097 = EDGE_LOOP ( 'NONE', ( #119140, #76329, #86983, #78993 ) ) ;
#33098 = VECTOR ( 'NONE', #65453, 1000.000000000000000 ) ;
#33099 = VECTOR ( 'NONE', #108998, 999.9999999999998863 ) ;
#33100 = CARTESIAN_POINT ( 'NONE',  ( 9.328169399223469327, 14.25929247661557575, 4.000000000000000000 ) ) ;
#33101 = LINE ( 'NONE', #41795, #51396 ) ;
#33102 = AXIS2_PLACEMENT_3D ( 'NONE', #8662, #129774, #74714 ) ;
#33103 = AXIS2_PLACEMENT_3D ( 'NONE', #64847, #8274, #66279 ) ;
#33104 = EDGE_CURVE ( 'NONE', #125114, #76630, #119973, .T. ) ;
#33105 = ORIENTED_EDGE ( 'NONE', *, *, #3227, .F. ) ;
#33106 = CARTESIAN_POINT ( 'NONE',  ( 29.48831394071549994, 6.759292476615649470, 16.35960578974462720 ) ) ;
#33107 = EDGE_CURVE ( 'NONE', #69740, #13073, #118573, .T. ) ;
#33109 = CARTESIAN_POINT ( 'NONE',  ( -34.92500000000001137, -6.281509562795707602, 4.759050581649337808 ) ) ;
#33108 = VECTOR ( 'NONE', #90162, 1000.000000000000000 ) ;
#33110 = CARTESIAN_POINT ( 'NONE',  ( -7.499999999999944045, -6.839392718269134974, -8.480912228396066510 ) ) ;
#33111 = AXIS2_PLACEMENT_3D ( 'NONE', #12847, #57126, #124487 ) ;
#33112 = COLOUR_RGB ( '', 0.09019608, 0.27058824, 0.51372549) ;
#33113 = EDGE_CURVE ( 'NONE', #79922, #107272, #64215, .T. ) ;
#33114 = VERTEX_POINT ( 'NONE', #74388 ) ;
#33115 = LINE ( 'NONE', #87460, #75502 ) ;
#33116 = CARTESIAN_POINT ( 'NONE',  ( 180.8471172286433841, -48.98543874033772738, 39.51758185027075143 ) ) ;
#33117 = CARTESIAN_POINT ( 'NONE',  ( 127.5761022459138161, -4.648522628062369932, 4.648522628062369932 ) ) ;
#33118 = CARTESIAN_POINT ( 'NONE',  ( -5.999999999999956479, -22.06887692260758982, 4.000000000000000000 ) ) ;
#33119 = LINE ( 'NONE', #65011, #29540 ) ;
#33120 = DIRECTION ( 'NONE',  ( 0.6830127018922181881, 0.6830127018922202975, -0.2588190451025214056 ) ) ;
#33121 = ORIENTED_EDGE ( 'NONE', *, *, #73479, .T. ) ;
#33122 = VECTOR ( 'NONE', #21400, 999.9999999999998863 ) ;
#33123 = ORIENTED_EDGE ( 'NONE', *, *, #131921, .F. ) ;
#33124 = CARTESIAN_POINT ( 'NONE',  ( 107.8287635252314516, 0.000000000000000000, -6.109999999999998543 ) ) ;
#33125 = ORIENTED_EDGE ( 'NONE', *, *, #121610, .T. ) ;
#33126 = EDGE_CURVE ( 'NONE', #56496, #130555, #43891, .T. ) ;
#33127 = ORIENTED_EDGE ( 'NONE', *, *, #88249, .T. ) ;
#33128 = CARTESIAN_POINT ( 'NONE',  ( 20.99999999999985789, -3.412538124160721331, 4.000000000000000000 ) ) ;
#33129 = AXIS2_PLACEMENT_3D ( 'NONE', #71639, #138314, #118691 ) ;
#33130 = LINE ( 'NONE', #131690, #22278 ) ;
#33131 = CYLINDRICAL_SURFACE ( 'NONE', #125841, 0.5000000000000004441 ) ;
#33132 = ORIENTED_EDGE ( 'NONE', *, *, #39622, .T. ) ;
#33133 = LINE ( 'NONE', #77348, #119964 ) ;
#33134 = CARTESIAN_POINT ( 'NONE',  ( 15.18398860626900237, 28.73617430169797871, 5.000000000000000000 ) ) ;
#33135 = EDGE_CURVE ( 'NONE', #48771, #117579, #106980, .T. ) ;
#33136 = PLANE ( 'NONE',  #87088 ) ;
#33137 = VECTOR ( 'NONE', #35131, 1000.000000000000000 ) ;
#33139 = CARTESIAN_POINT ( 'NONE',  ( 59.28752705046289151, 0.000000000000000000, -7.949999999999998401 ) ) ;
#33138 = DIRECTION ( 'NONE',  ( -0.7071067811865487940, 0.7071067811865463515, -0.000000000000000000 ) ) ;
#33140 = LINE ( 'NONE', #136676, #127127 ) ;
#33141 = PRESENTATION_LAYER_ASSIGNMENT (  '', '', ( #102555 ) ) ;
#33142 = CARTESIAN_POINT ( 'NONE',  ( 0.8065107498756644011, 1.049489235317104807, 3.918521177239187026 ) ) ;
#33143 = ORIENTED_EDGE ( 'NONE', *, *, #121401, .T. ) ;
#33144 = DIRECTION ( 'NONE',  ( -1.000000000000000000, 0.000000000000000000, 0.000000000000000000 ) ) ;
#33145 = CARTESIAN_POINT ( 'NONE',  ( 9.370933818357753964, 0.000000000000000000, 2.500000000000000444 ) ) ;
#33146 = ORIENTED_EDGE ( 'NONE', *, *, #40854, .T. ) ;
#33147 = ADVANCED_FACE ( 'NONE', ( #141036 ), #112085, .F. ) ;
#33148 = ORIENTED_EDGE ( 'NONE', *, *, #112245, .F. ) ;
#33149 = ORIENTED_EDGE ( 'NONE', *, *, #77719, .F. ) ;
#33150 = CARTESIAN_POINT ( 'NONE',  ( 64.75043019189810423, 3.055000000000002824, -5.291415217122919401 ) ) ;
#33151 = EDGE_LOOP ( 'NONE', ( #45892, #39255, #71292, #131107 ) ) ;
#33152 = VECTOR ( 'NONE', #25301, 1000.000000000000227 ) ;
#33153 = CARTESIAN_POINT ( 'NONE',  ( 60.29974487139158867, -27.71228299555248142, 4.000000000000000000 ) ) ;
#33154 = EDGE_CURVE ( 'NONE', #111848, #31083, #75808, .T. ) ;
#33155 = CARTESIAN_POINT ( 'NONE',  ( 0.4833062828704390301, 6.094999999999991758, 1.633150327867687102 ) ) ;
#33156 = CARTESIAN_POINT ( 'NONE',  ( 98.14626352523143282, -4.472830434245840259, 4.472830434245838482 ) ) ;
#33157 = LINE ( 'NONE', #52706, #37927 ) ;
#33158 = VECTOR ( 'NONE', #92237, 1000.000000000000000 ) ;
#33159 = EDGE_LOOP ( 'NONE', ( #110584, #49942, #5798, #124110 ) ) ;
#33160 = CARTESIAN_POINT ( 'NONE',  ( 2.000000000000008882, 0.000000000000000000, 0.000000000000000000 ) ) ;
#33161 = VECTOR ( 'NONE', #82951, 1000.000000000000000 ) ;
#33162 = CARTESIAN_POINT ( 'NONE',  ( 27.18398860626900060, 28.73617430169806042, 5.000000000000000000 ) ) ;
#33163 = EDGE_CURVE ( 'NONE', #34776, #137982, #130191, .T. ) ;
#33164 = LINE ( 'NONE', #77374, #88441 ) ;
#33165 = DIRECTION ( 'NONE',  ( -1.000000000000000000, -0.000000000000000000, -0.000000000000000000 ) ) ;
#33166 = VERTEX_POINT ( 'NONE', #98269 ) ;
#33167 = EDGE_CURVE ( 'NONE', #139146, #42711, #85224, .T. ) ;
#33168 = SURFACE_STYLE_USAGE ( .BOTH. , #54893 ) ;
#33169 = ORIENTED_EDGE ( 'NONE', *, *, #103146, .F. ) ;
#33170 = EDGE_LOOP ( 'NONE', ( #136809, #137754, #84358, #141153 ) ) ;
#33171 = ORIENTED_EDGE ( 'NONE', *, *, #72625, .T. ) ;
#33172 = CARTESIAN_POINT ( 'NONE',  ( 123.8704301918981230, -3.055000000000001492, 5.291415217122917625 ) ) ;
#33173 = VECTOR ( 'NONE', #26923, 1000.000000000000000 ) ;
#33174 = DIRECTION ( 'NONE',  ( 0.6830127018922180770, -0.6830127018922204085, -0.2588190451025213501 ) ) ;
#33175 = CARTESIAN_POINT ( 'NONE',  ( 20.48334561358940675, 22.22500000000000142, 4.500000000000000888 ) ) ;
#33176 = ADVANCED_FACE ( 'NONE', ( #43181 ), #53314, .F. ) ;
#33177 = ORIENTED_EDGE ( 'NONE', *, *, #12723, .T. ) ;
#33178 = DIRECTION ( 'NONE',  ( -0.000000000000000000, 0.000000000000000000, 1.000000000000000000 ) ) ;
#33179 = VECTOR ( 'NONE', #41219, 1000.000000000000227 ) ;
#33180 = ORIENTED_EDGE ( 'NONE', *, *, #137058, .F. ) ;
#33181 = CARTESIAN_POINT ( 'NONE',  ( 12.95790314143521904, 6.871911579029515771, 3.967499999999989146 ) ) ;
#33182 = FACE_OUTER_BOUND ( 'NONE', #10565, .T. ) ;
#33183 = LINE ( 'NONE', #22233, #140882 ) ;
#33184 = DIRECTION ( 'NONE',  ( 0.6830127018922180770, -0.6830127018922204085, -0.2588190451025213501 ) ) ;
#33185 = VERTEX_POINT ( 'NONE', #141785 ) ;
#33186 = ORIENTED_EDGE ( 'NONE', *, *, #36788, .T. ) ;
#33187 = VERTEX_POINT ( 'NONE', #108374 ) ;
#33188 = CARTESIAN_POINT ( 'NONE',  ( 15.00548008471250228, 28.92564299267927552, 4.000000000000000000 ) ) ;
#33189 = CARTESIAN_POINT ( 'NONE',  ( 34.49999999999975842, -13.53574439159937093, 4.994342998332162331 ) ) ;
#33190 = UNCERTAINTY_MEASURE_WITH_UNIT (LENGTH_MEASURE( 1.000000000000000082E-05 ), #75858, 'distance_accuracy_value', 'NONE');
#33191 = VECTOR ( 'NONE', #28351, 999.9999999999998863 ) ;
#33192 = DIRECTION ( 'NONE',  ( -0.7071067811865486830, 0.7071067811865464625, 0.000000000000000000 ) ) ;
#33193 = LINE ( 'NONE', #87533, #43630 ) ;
#33194 = AXIS2_PLACEMENT_3D ( 'NONE', #18828, #76086, #64490 ) ;
#33195 = LINE ( 'NONE', #9203, #41479 ) ;
#33196 = CARTESIAN_POINT ( 'NONE',  ( -15.00548008471250228, 28.92564299267927552, 4.000000000000000000 ) ) ;
#33197 = LINE ( 'NONE', #66511, #104217 ) ;
#33198 = DIRECTION ( 'NONE',  ( -0.7071067811865486830, -0.7071067811865464625, 0.000000000000000000 ) ) ;
#33199 = ORIENTED_EDGE ( 'NONE', *, *, #84145, .F. ) ;
#33200 = FACE_OUTER_BOUND ( 'NONE', #62329, .T. ) ;
#33201 = EDGE_CURVE ( 'NONE', #66673, #76695, #65684, .T. ) ;
#33202 = VECTOR ( 'NONE', #128457, 1000.000000000000000 ) ;
#33204 = EDGE_LOOP ( 'NONE', ( #109688, #112558, #123431, #117064 ) ) ;
#33203 =( GEOMETRIC_REPRESENTATION_CONTEXT ( 3 ) GLOBAL_UNCERTAINTY_ASSIGNED_CONTEXT ( ( #5227 ) ) GLOBAL_UNIT_ASSIGNED_CONTEXT ( ( #53393, #130979, #133128 ) ) REPRESENTATION_CONTEXT ( 'NONE', 'WORKASPACE' ) );
#33205 = LINE ( 'NONE', #8501, #96203 ) ;
#33206 = VERTEX_POINT ( 'NONE', #32300 ) ;
#33207 =( GEOMETRIC_REPRESENTATION_CONTEXT ( 3 ) GLOBAL_UNCERTAINTY_ASSIGNED_CONTEXT ( ( #1393 ) ) GLOBAL_UNIT_ASSIGNED_CONTEXT ( ( #82010, #126190, #82692 ) ) REPRESENTATION_CONTEXT ( 'NONE', 'WORKASPACE' ) );
#33208 = CARTESIAN_POINT ( 'NONE',  ( 17.54580628287044064, 5.278424836066143655, -3.047499999999997655 ) ) ;
#33210 = ORIENTED_EDGE ( 'NONE', *, *, #56265, .F. ) ;
#33209 = CARTESIAN_POINT ( 'NONE',  ( 0.000000000000000000, 0.000000000000000000, 5.000000000000000000 ) ) ;
#33211 = CARTESIAN_POINT ( 'NONE',  ( 24.48921356237309510, -27.52281430457072631, 5.000000000000000000 ) ) ;
#33212 = ADVANCED_FACE ( 'NONE', ( #18520 ), #30883, .F. ) ;
#33213 = VERTEX_POINT ( 'NONE', #41741 ) ;
#33214 = DIRECTION ( 'NONE',  ( 0.7071067811865487940, -0.7071067811865463515, 0.000000000000000000 ) ) ;
#33215 = ORIENTED_EDGE ( 'NONE', *, *, #21704, .T. ) ;
#33216 = LINE ( 'NONE', #91149, #106831 ) ;
#33217 = VERTEX_POINT ( 'NONE', #119280 ) ;
#33218 = CARTESIAN_POINT ( 'NONE',  ( 29.99999999999999645, 2.375000000000000000, -4.320000000000002061 ) ) ;
#33220 = EDGE_CURVE ( 'NONE', #49530, #128364, #107693, .T. ) ;
#33219 = CARTESIAN_POINT ( 'NONE',  ( 111.6416937171295558, -2.130196079827424871, -7.949999999999999289 ) ) ;
#33221 = DIRECTION ( 'NONE',  ( 0.000000000000000000, 0.000000000000000000, -1.000000000000000000 ) ) ;
#33222 = VECTOR ( 'NONE', #58905, 999.9999999999998863 ) ;
#33223 = CARTESIAN_POINT ( 'NONE',  ( 6.792893218813409462, 9.759292476615618384, 5.000000000000000000 ) ) ;
#33224 = EDGE_CURVE ( 'NONE', #91232, #111908, #63929, .T. ) ;
#33225 = CARTESIAN_POINT ( 'NONE',  ( 9.183988606268997046, 28.73617430169793607, 5.000000000000000000 ) ) ;
#33226 = LINE ( 'NONE', #99116, #82057 ) ;
#33227 = EDGE_CURVE ( 'NONE', #86031, #41563, #68515, .T. ) ;
#33228 = DIRECTION ( 'NONE',  ( -0.7071067811865486830, 0.7071067811865464625, 0.000000000000000000 ) ) ;
#33229 = CARTESIAN_POINT ( 'NONE',  ( 11.81250000000000355, -4.461849672132299993, -4.461849672132299105 ) ) ;
#33230 = CARTESIAN_POINT ( 'NONE',  ( 18.49956980810188867, -3.967499999999998028, -6.871911579029511330 ) ) ;
#33231 = DIRECTION ( 'NONE',  ( 0.000000000000000000, 0.000000000000000000, 1.000000000000000000 ) ) ;
#33233 = ADVANCED_FACE ( 'NONE', ( #46792 ), #23550, .T. ) ;
#33232 = DIRECTION ( 'NONE',  ( 0.000000000000000000, 1.000000000000000000, 0.000000000000000000 ) ) ;
#33234 = ORIENTED_EDGE ( 'NONE', *, *, #71873, .F. ) ;
#33235 = VECTOR ( 'NONE', #6864, 1000.000000000000227 ) ;
#33236 = ORIENTED_EDGE ( 'NONE', *, *, #26211, .F. ) ;
#33237 = CARTESIAN_POINT ( 'NONE',  ( -0.6567100016621301162, 3.759292476615681888, 13.27625715073265589 ) ) ;
#33238 = ORIENTED_EDGE ( 'NONE', *, *, #78563, .T. ) ;
#33239 = VECTOR ( 'NONE', #49574, 1000.000000000000227 ) ;
#33240 = ADVANCED_FACE ( 'NONE', ( #58381 ), #113397, .F. ) ;
#33241 = DIRECTION ( 'NONE',  ( -1.000000000000000000, -0.000000000000000000, -0.000000000000000000 ) ) ;
#33242 = DIRECTION ( 'NONE',  ( -0.7071067811865486830, -0.7071067811865464625, 0.000000000000000000 ) ) ;
#33243 = DIRECTION ( 'NONE',  ( -0.000000000000000000, 0.000000000000000000, 1.000000000000000000 ) ) ;
#33244 = CARTESIAN_POINT ( 'NONE',  ( 128.6577301979894798, -49.12413125935659508, -39.93743342457428724 ) ) ;
#33245 = ORIENTED_EDGE ( 'NONE', *, *, #39293, .T. ) ;
#33246 = LINE ( 'NONE', #99884, #92820 ) ;
#33247 = VECTOR ( 'NONE', #12625, 999.9999999999998863 ) ;
#33248 = EDGE_CURVE ( 'NONE', #23925, #43233, #110532, .T. ) ;
#33249 = CARTESIAN_POINT ( 'NONE',  ( -10.49999999999992184, 7.466399257802187606, 5.000000000000000000 ) ) ;
#33250 = EDGE_CURVE ( 'NONE', #120007, #115599, #46046, .T. ) ;
#33251 = CARTESIAN_POINT ( 'NONE',  ( 156.1500000000000057, -49.14999999999999147, -49.92499999999968452 ) ) ;
#33252 = CARTESIAN_POINT ( 'NONE',  ( 5.999999999999966249, 19.55218569542897100, 5.000000000000000000 ) ) ;
#33254 = ORIENTED_EDGE ( 'NONE', *, *, #89794, .T. ) ;
#33253 = DIRECTION ( 'NONE',  ( -0.000000000000000000, -0.3543493200069152693, 0.9351131265310292928 ) ) ;
#33255 = CYLINDRICAL_SURFACE ( 'NONE', #35417, 7.950000000000000178 ) ;
#33256 = LINE ( 'NONE', #66562, #84736 ) ;
#33257 = LINE ( 'NONE', #52792, #42372 ) ;
#33258 = CARTESIAN_POINT ( 'NONE',  ( -7.140000000000001457, -35.14999999999999147, -40.00000000000000000 ) ) ;
#33259 = EDGE_CURVE ( 'NONE', #111034, #22009, #67817, .T. ) ;
#33260 = LINE ( 'NONE', #12162, #33038 ) ;
#33261 = AXIS2_PLACEMENT_3D ( 'NONE', #22880, #35261, #2571 ) ;
#33262 = EDGE_LOOP ( 'NONE', ( #125849, #35592, #130870, #125908 ) ) ;
#33263 = ORIENTED_EDGE ( 'NONE', *, *, #69953, .F. ) ;
#33264 = EDGE_LOOP ( 'NONE', ( #21969, #119526, #126602, #45137 ) ) ;
#33265 = CARTESIAN_POINT ( 'NONE',  ( 88.81293019189809002, -1.637169565754159617, -6.110000000000001208 ) ) ;
#33266 = AXIS2_PLACEMENT_3D ( 'NONE', #93931, #105508, #137458 ) ;
#33267 =( BOUNDED_CURVE ( )  B_SPLINE_CURVE ( 3, ( #7461, #106052, #72076, #72803 ),
 .UNSPECIFIED., .F., .T. ) 
 B_SPLINE_CURVE_WITH_KNOTS ( ( 4, 4 ),
 ( 5.920967161967927161, 7.341195215986605405 ),
 .UNSPECIFIED. ) 
 CURVE ( )  GEOMETRIC_REPRESENTATION_ITEM ( )  RATIONAL_B_SPLINE_CURVE ( ( 1.000000000000000000, 0.8388583629366683780, 0.8388583629366683780, 1.000000000000000000 ) ) 
 REPRESENTATION_ITEM ( '' )  );
#33268 = ORIENTED_EDGE ( 'NONE', *, *, #73052, .F. ) ;
#33269 = CARTESIAN_POINT ( 'NONE',  ( 14.95136400821897205, -1.164498636767094197, 4.123993368336929422 ) ) ;
#33270 = VECTOR ( 'NONE', #87585, 1000.000000000000000 ) ;
#33271 = CARTESIAN_POINT ( 'NONE',  ( 83.78752705046288440, 0.000000000000000000, -7.949999999999998401 ) ) ;
#33272 = ORIENTED_EDGE ( 'NONE', *, *, #66553, .T. ) ;
#33273 = DIRECTION ( 'NONE',  ( -0.7071067811865486830, 0.7071067811865464625, 0.000000000000000000 ) ) ;
#33274 = CARTESIAN_POINT ( 'NONE',  ( -16.82334089840016844, 5.259292476615659240, 15.86257073897101577 ) ) ;
#33275 = CARTESIAN_POINT ( 'NONE',  ( 86.53709685856478018, -3.054999999999998828, -5.291415217122919401 ) ) ;
#33276 = ORIENTED_EDGE ( 'NONE', *, *, #19685, .F. ) ;
#33277 = CARTESIAN_POINT ( 'NONE',  ( 1.199999999999999956, 0.5999999999999987566, -4.543283425070392845 ) ) ;
#33278 = EDGE_CURVE ( 'NONE', #18830, #26483, #100412, .T. ) ;
#33279 = COLOUR_RGB ( '', 0.31764706, 0.68627451, 0.89019608) ;
#33280 = CARTESIAN_POINT ( 'NONE',  ( -34.75611968250420603, 11.81293425470724578, 4.955485411084898040 ) ) ;
#33281 = VERTEX_POINT ( 'NONE', #44642 ) ;
#33282 = ORIENTED_EDGE ( 'NONE', *, *, #15419, .F. ) ;
#33283 = VERTEX_POINT ( 'NONE', #3208 ) ;
#33284 = DIRECTION ( 'NONE',  ( -0.000000000000000000, 0.000000000000000000, 1.000000000000000000 ) ) ;
#33285 = LINE ( 'NONE', #65905, #100948 ) ;
#33286 = CARTESIAN_POINT ( 'NONE',  ( 15.67123647476855552, 0.000000000000000000, 7.934999999999990727 ) ) ;
#33287 = VECTOR ( 'NONE', #137363, 1000.000000000000000 ) ;
#33288 = FACE_OUTER_BOUND ( 'NONE', #44666, .T. ) ;
#33289 = DIRECTION ( 'NONE',  ( 0.7071067811865487940, 0.7071067811865463515, 0.000000000000000000 ) ) ;
#33290 = ADVANCED_FACE ( 'NONE', ( #45343 ), #35172, .T. ) ;
#33291 = CARTESIAN_POINT ( 'NONE',  ( -48.48921356237309510, -27.52281430457089328, 5.000000000000000000 ) ) ;
#33292 = DIRECTION ( 'NONE',  ( 0.000000000000000000, 0.000000000000000000, 1.000000000000000000 ) ) ;
#33293 = SURFACE_SIDE_STYLE ('',( #20922 ) ) ;
#33294 = AXIS2_PLACEMENT_3D ( 'NONE', #36840, #125290, #133328 ) ;
#33295 = ORIENTED_EDGE ( 'NONE', *, *, #27117, .T. ) ;
#33296 = ORIENTED_EDGE ( 'NONE', *, *, #59393, .F. ) ;
#33297 = DIRECTION ( 'NONE',  ( -0.7071067811865487940, 0.7071067811865463515, 0.000000000000000000 ) ) ;
#33299 = ORIENTED_EDGE ( 'NONE', *, *, #46954, .F. ) ;
#33298 = EDGE_CURVE ( 'NONE', #90674, #24049, #88830, .T. ) ;
#33300 = EDGE_LOOP ( 'NONE', ( #119781, #71877, #16374, #79122 ) ) ;
#33301 = AXIS2_PLACEMENT_3D ( 'NONE', #35474, #46352, #68114 ) ;
#33302 = CARTESIAN_POINT ( 'NONE',  ( -54.48921356237310221, -27.52281430457093236, 5.000000000000000000 ) ) ;
#33303 = VERTEX_POINT ( 'NONE', #135203 ) ;
#33304 = CARTESIAN_POINT ( 'NONE',  ( 56.41666666666665719, -6.884901960086287076, -3.975000000000000977 ) ) ;
#33305 = LINE ( 'NONE', #141293, #87777 ) ;
#33306 = EDGE_CURVE ( 'NONE', #42501, #134318, #55485, .T. ) ;
#33307 = CARTESIAN_POINT ( 'NONE',  ( 34.49999999999975842, -19.53574439159931231, 4.994342998332164107 ) ) ;
#33308 = CARTESIAN_POINT ( 'NONE',  ( 34.92499999999998295, 22.22500000000000142, 4.000000000000000000 ) ) ;
#33309 = CARTESIAN_POINT ( 'NONE',  ( 5.292893218813423672, 2.259292476615697876, 5.000000000000000000 ) ) ;
#33310 = VERTEX_POINT ( 'NONE', #22105 ) ;
#33311 = DIRECTION ( 'NONE',  ( 0.3543493200069162685, -0.000000000000000000, -0.9351131265310288487 ) ) ;
#33312 = ORIENTED_EDGE ( 'NONE', *, *, #136141, .T. ) ;
#33314 = ADVANCED_FACE ( 'NONE', ( #99668 ), #133059, .T. ) ;
#33313 = CARTESIAN_POINT ( 'NONE',  ( 19.72391290958995569, -1.589875490879015141, -32.21414776232133192 ) ) ;
#33315 = VERTEX_POINT ( 'NONE', #122863 ) ;
#33316 = CARTESIAN_POINT ( 'NONE',  ( -39.48921356237310221, -27.52281430457082934, 5.000000000000000000 ) ) ;
#33317 = ORIENTED_EDGE ( 'NONE', *, *, #44347, .T. ) ;
#33318 = FACE_OUTER_BOUND ( 'NONE', #72298, .T. ) ;
#33319 = ORIENTED_EDGE ( 'NONE', *, *, #61364, .F. ) ;
#33320 = ORIENTED_EDGE ( 'NONE', *, *, #101685, .F. ) ;
#33321 = CIRCLE ( 'NONE', #81956, 6.499999999999999112 ) ;
#33322 = ORIENTED_EDGE ( 'NONE', *, *, #121125, .T. ) ;
#33323 =( BOUNDED_CURVE ( )  B_SPLINE_CURVE ( 2, ( #95018, #94320, #137855, #27630, #127687, #115319, #84880, #72630, #73308 ),
 .UNSPECIFIED., .F., .T. ) 
 B_SPLINE_CURVE_WITH_KNOTS ( ( 3, 2, 2, 2, 3 ),
 ( 0.008333333333333340157, 0.01111111111111109939, 0.01388888888888885689, 0.01666666666666661439, 0.01881059163983938437 ),
 .UNSPECIFIED. ) 
 CURVE ( )  GEOMETRIC_REPRESENTATION_ITEM ( )  RATIONAL_B_SPLINE_CURVE ( ( 0.9999999999999995559, 0.9659258262890687563, 1.000000000000000000, 0.9659258262890683122, 1.000000000000000000, 0.9659258262890683122, 1.000000000000000000, 0.9737011100947261522, 0.9879978699103917350 ) ) 
 REPRESENTATION_ITEM ( '' )  );
#33324 = DIRECTION ( 'NONE',  ( -0.3543493200069162685, -0.000000000000000000, -0.9351131265310288487 ) ) ;
#33325 = VECTOR ( 'NONE', #66013, 1000.000000000000000 ) ;
#33326 = CARTESIAN_POINT ( 'NONE',  ( 0.000000000000000000, 0.000000000000000000, -10.00000000000000000 ) ) ;
#33327 = DIRECTION ( 'NONE',  ( 0.3240768213499733985, -0.9146165434626267743, -0.2417659866237898969 ) ) ;
#33328 = CARTESIAN_POINT ( 'NONE',  ( -24.48921356237309510, -27.52281430457072631, 5.000000000000000000 ) ) ;
#33329 = CARTESIAN_POINT ( 'NONE',  ( 7.139999999999991687, -35.76999999999998892, -7.899272885403729738 ) ) ;
#33330 = LINE ( 'NONE', #121696, #143130 ) ;
#33331 = CARTESIAN_POINT ( 'NONE',  ( 13.49999999999990052, -14.70932175296476352, -11.46312253303840478 ) ) ;
#33333 = LINE ( 'NONE', #98536, #118758 ) ;
#33332 = AXIS2_PLACEMENT_3D ( 'NONE', #116924, #17591, #61860 ) ;
#33334 = CARTESIAN_POINT ( 'NONE',  ( 20.99451991528748707, 28.92564299267952777, 4.000000000000000000 ) ) ;
#33335 = EDGE_CURVE ( 'NONE', #103671, #21557, #67068, .T. ) ;
#33336 = DIRECTION ( 'NONE',  ( -0.7071067811865487940, 0.7071067811865463515, -0.000000000000000000 ) ) ;
#33337 = LINE ( 'NONE', #12240, #100430 ) ;
#33338 = EDGE_LOOP ( 'NONE', ( #115845, #15677, #118942, #46294 ) ) ;
#33339 = ORIENTED_EDGE ( 'NONE', *, *, #73087, .F. ) ;
#33340 = ORIENTED_EDGE ( 'NONE', *, *, #78606, .F. ) ;
#33341 = DIRECTION ( 'NONE',  ( 0.000000000000000000, 1.000000000000000000, 0.000000000000000000 ) ) ;
#33342 = ORIENTED_EDGE ( 'NONE', *, *, #120272, .F. ) ;
#33343 = AXIS2_PLACEMENT_3D ( 'NONE', #127852, #137293, #27798 ) ;
#33344 = ORIENTED_EDGE ( 'NONE', *, *, #89753, .F. ) ;
#33345 = DIRECTION ( 'NONE',  ( -0.7071067811865486830, -0.7071067811865464625, 0.000000000000000000 ) ) ;
#33346 = CARTESIAN_POINT ( 'NONE',  ( 107.7041937171295558, -6.884901960086285300, -3.975000000000000089 ) ) ;
#33347 = CARTESIAN_POINT ( 'NONE',  ( 8.031592354503320763, 9.902892378096218942E-16, 0.000000000000000000 ) ) ;
#33348 = ADVANCED_FACE ( 'NONE', ( #56231 ), #34429, .F. ) ;
#33349 = CARTESIAN_POINT ( 'NONE',  ( -28.49999999999980815, 12.43112307739205846, 4.000000000000000000 ) ) ;
#33350 = ORIENTED_EDGE ( 'NONE', *, *, #18601, .T. ) ;
#33351 = CARTESIAN_POINT ( 'NONE',  ( 20.20519093902540320, 0.000000000000000000, 2.500000000000000444 ) ) ;
#33352 = ORIENTED_EDGE ( 'NONE', *, *, #105358, .T. ) ;
#33355 = VECTOR ( 'NONE', #48088, 1000.000000000000227 ) ;
#33354 = DIRECTION ( 'NONE',  ( 0.000000000000000000, -1.000000000000000000, 0.000000000000000000 ) ) ;
#33353 = PRODUCT_RELATED_PRODUCT_CATEGORY ( 'part', '', ( #7609 ) ) ;
#33356 = VECTOR ( 'NONE', #78245, 1000.000000000000000 ) ;
#33357 = CARTESIAN_POINT ( 'NONE',  ( 14.50456980810188767, 6.871911579029510442, -3.967499999999998916 ) ) ;
#33358 = VERTEX_POINT ( 'NONE', #1749 ) ;
#33359 = CARTESIAN_POINT ( 'NONE',  ( 81.72459685856476597, -1.637169565754161171, 6.109999999999998543 ) ) ;
#33360 = DIRECTION ( 'NONE',  ( 0.7071067811865486830, -0.7071067811865464625, -0.000000000000000000 ) ) ;
#33361 = CARTESIAN_POINT ( 'NONE',  ( 33.48921356237309510, -27.52281430457078670, 5.000000000000000000 ) ) ;
#33362 = ORIENTED_EDGE ( 'NONE', *, *, #141464, .T. ) ;
#33363 = ORIENTED_EDGE ( 'NONE', *, *, #104781, .F. ) ;
#33364 = ORIENTED_EDGE ( 'NONE', *, *, #100797, .F. ) ;
#33365 = CARTESIAN_POINT ( 'NONE',  ( -4.499999999999968914, -13.91253812416061209, 4.000000000000000000 ) ) ;
#33367 = VECTOR ( 'NONE', #22964, 1000.000000000000000 ) ;
#33366 = CARTESIAN_POINT ( 'NONE',  ( 57.48921356237308800, -27.52281430457095368, 5.000000000000000000 ) ) ;
#33368 = CARTESIAN_POINT ( 'NONE',  ( 16.55917894070448426, 0.6741881004290185553, -33.57943960405233241 ) ) ;
#33369 = DIRECTION ( 'NONE',  ( 0.7071067811865487940, 0.7071067811865463515, 0.000000000000000000 ) ) ;
#33370 = DIRECTION ( 'NONE',  ( -0.000000000000000000, 0.3543493200069153248, 0.9351131265310292928 ) ) ;
#33371 = EDGE_CURVE ( 'NONE', #1453, #2022, #56550, .T. ) ;
#33372 = EDGE_LOOP ( 'NONE', ( #67497, #2469, #5300, #44123 ) ) ;
#33373 = DIRECTION ( 'NONE',  ( -1.000000000000000000, 0.000000000000000000, 0.000000000000000000 ) ) ;
#33374 = DIRECTION ( 'NONE',  ( -0.7071067811865487940, 0.7071067811865463515, 0.000000000000000000 ) ) ;
#33375 = DIRECTION ( 'NONE',  ( 0.000000000000000000, -1.000000000000000000, 0.000000000000000000 ) ) ;
#33376 = ORIENTED_EDGE ( 'NONE', *, *, #28466, .F. ) ;
#33377 = DIRECTION ( 'NONE',  ( 0.6830127018922180770, -0.6830127018922204085, -0.2588190451025213501 ) ) ;
#33378 = AXIS2_PLACEMENT_3D ( 'NONE', #60083, #47112, #57965 ) ;
#33379 = DIRECTION ( 'NONE',  ( -0.7071067811865487940, 0.7071067811865463515, -0.000000000000000000 ) ) ;
#33380 = VERTEX_POINT ( 'NONE', #112696 ) ;
#33382 = ORIENTED_EDGE ( 'NONE', *, *, #72932, .T. ) ;
#33381 = LINE ( 'NONE', #133380, #76448 ) ;
#33383 = EDGE_LOOP ( 'NONE', ( #62836, #142691, #102658, #128839 ) ) ;
#33384 = LINE ( 'NONE', #67422, #141999 ) ;
#33385 = DIRECTION ( 'NONE',  ( -0.000000000000000000, 1.000000000000000000, -0.000000000000000000 ) ) ;
#33386 = VERTEX_POINT ( 'NONE', #57636 ) ;
#33387 = CARTESIAN_POINT ( 'NONE',  ( -5.999999999999954703, 7.552185695429089130, 5.000000000000000000 ) ) ;
#33388 = PLANE ( 'NONE',  #119264 ) ;
#33389 = ADVANCED_FACE ( 'NONE', ( #124290 ), #61234, .F. ) ;
#33391 = VECTOR ( 'NONE', #73432, 1000.000000000000000 ) ;
#33390 =( LENGTH_UNIT ( ) NAMED_UNIT ( * ) SI_UNIT ( .MILLI., .METRE. ) );
#33392 = PLANE ( 'NONE',  #41585 ) ;
#33393 = ADVANCED_FACE ( 'NONE', ( #50310 ), #116973, .F. ) ;
#33394 = CARTESIAN_POINT ( 'NONE',  ( 30.70710678118632941, -12.74070752338415247, 5.000000000000000000 ) ) ;
#33395 = DIRECTION ( 'NONE',  ( -0.7071067811865487940, 0.7071067811865463515, 0.000000000000000000 ) ) ;
#33396 = DIRECTION ( 'NONE',  ( 0.3543493200069162685, -0.000000000000000000, -0.9351131265310288487 ) ) ;
#33397 = DIRECTION ( 'NONE',  ( 0.7071067811865486830, -0.7071067811865464625, -0.000000000000000000 ) ) ;
#33398 = CARTESIAN_POINT ( 'NONE',  ( 16.74956980810188867, 3.967499999999998916, 6.871911579029510442 ) ) ;
#33399 = FACE_OUTER_BOUND ( 'NONE', #100729, .T. ) ;
#33400 = DIRECTION ( 'NONE',  ( -0.7071067811865487940, 0.7071067811865463515, 0.000000000000000000 ) ) ;
#33401 = PLANE ( 'NONE',  #4794 ) ;
#33403 = EDGE_CURVE ( 'NONE', #96788, #102292, #17643, .T. ) ;
#33402 = DIRECTION ( 'NONE',  ( 0.7071067811865487940, 0.7071067811865463515, 0.000000000000000000 ) ) ;
#33405 = ADVANCED_FACE ( 'NONE', ( #60494 ), #127132, .F. ) ;
#33404 = VERTEX_POINT ( 'NONE', #103240 ) ;
#33406 = AXIS2_PLACEMENT_3D ( 'NONE', #30970, #120798, #130281 ) ;
#33407 = ORIENTED_EDGE ( 'NONE', *, *, #118076, .T. ) ;
#33408 = CARTESIAN_POINT ( 'NONE',  ( 99.43749999999998579, 5.819803920172573974, -5.819803920172572198 ) ) ;
#33409 = ORIENTED_EDGE ( 'NONE', *, *, #64663, .F. ) ;
#33410 = ORIENTED_EDGE ( 'NONE', *, *, #101611, .F. ) ;
#33411 = VERTEX_POINT ( 'NONE', #104671 ) ;
#33412 = DIRECTION ( 'NONE',  ( 0.7071067811865486830, -0.7071067811865464625, -0.000000000000000000 ) ) ;
#33413 = DIRECTION ( 'NONE',  ( -0.7071067811865486830, 0.7071067811865464625, 0.000000000000000000 ) ) ;
#33414 = ORIENTED_EDGE ( 'NONE', *, *, #131857, .F. ) ;
#33415 = LINE ( 'NONE', #42844, #106431 ) ;
#33416 = EDGE_CURVE ( 'NONE', #140659, #99485, #6034, .T. ) ;
#33417 = CARTESIAN_POINT ( 'NONE',  ( -5.999999999999953815, -18.41253812416056945, 4.000000000000000000 ) ) ;
#33418 = LINE ( 'NONE', #21786, #2592 ) ;
#33419 = ORIENTED_EDGE ( 'NONE', *, *, #38885, .T. ) ;
#33420 = EDGE_CURVE ( 'NONE', #96438, #105463, #3537, .T. ) ;
#33421 = DIRECTION ( 'NONE',  ( 1.000000000000000000, 0.000000000000000000, 0.000000000000000000 ) ) ;
#33422 = CARTESIAN_POINT ( 'NONE',  ( 18.32266436734346726, 2.055000000000001048, 2.516649172247811554E-16 ) ) ;
#33423 = VECTOR ( 'NONE', #80200, 1000.000000000000000 ) ;
#33424 = CARTESIAN_POINT ( 'NONE',  ( -34.92500000000001137, 16.80009451602703052, 4.759050581649338696 ) ) ;
#33425 = CARTESIAN_POINT ( 'NONE',  ( 32.99999999999977973, -12.41253812416062985, 4.000000000000000000 ) ) ;
#33426 = LINE ( 'NONE', #100078, #117111 ) ;
#33427 = CARTESIAN_POINT ( 'NONE',  ( 8.483345613589499123, 22.22500000000000142, 4.500000000000000888 ) ) ;
#33428 = ADVANCED_FACE ( 'NONE', ( #115508 ), #130618, .T. ) ;
#33429 = DIRECTION ( 'NONE',  ( -0.3543493200069162685, -0.000000000000000000, -0.9351131265310288487 ) ) ;
#33430 = VECTOR ( 'NONE', #100239, 1000.000000000000000 ) ;
#33431 = ORIENTED_EDGE ( 'NONE', *, *, #107335, .F. ) ;
#33432 = ORIENTED_EDGE ( 'NONE', *, *, #127993, .F. ) ;
#33433 = CARTESIAN_POINT ( 'NONE',  ( 120.0212635252314328, -4.472830434245839371, -4.472830434245840259 ) ) ;
#33434 = EDGE_LOOP ( 'NONE', ( #67853, #54013, #95098, #94020, #116764 ) ) ;
#33435 = CARTESIAN_POINT ( 'NONE',  ( 5.207106781186508826, 12.75929247661558996, 5.000000000000000000 ) ) ;
#33436 = ADVANCED_FACE ( 'NONE', ( #117655 ), #131437, .T. ) ;
#33437 = CARTESIAN_POINT ( 'NONE',  ( 21.70710678118638981, -6.740707523384214639, 5.000000000000000000 ) ) ;
#33438 = CARTESIAN_POINT ( 'NONE',  ( 33.48921356237309510, -27.52281430457078670, 5.000000000000000000 ) ) ;
#33439 = DIRECTION ( 'NONE',  ( -1.000000000000000000, -1.224606353822377258E-16, -0.000000000000000000 ) ) ;
#33440 = CARTESIAN_POINT ( 'NONE',  ( 116.8704301918981230, -3.055000000000001492, 5.291415217122917625 ) ) ;
#33441 = CIRCLE ( 'NONE', #116692, 2.500000000000000888 ) ;
#33442 = ORIENTED_EDGE ( 'NONE', *, *, #117938, .T. ) ;
#33443 = ORIENTED_EDGE ( 'NONE', *, *, #42088, .T. ) ;
#33444 = EDGE_CURVE ( 'NONE', #25651, #82699, #76342, .T. ) ;
#33445 = CARTESIAN_POINT ( 'NONE',  ( 70.07919371712955581, 3.975000000000002753, -6.884901960086283523 ) ) ;
#33446 = CARTESIAN_POINT ( 'NONE',  ( 98.85416666666665719, -2.130196079827387567, -7.950000000000023270 ) ) ;
#33447 = ORIENTED_EDGE ( 'NONE', *, *, #46344, .T. ) ;
#33448 = ORIENTED_EDGE ( 'NONE', *, *, #15385, .F. ) ;
#33449 = CARTESIAN_POINT ( 'NONE',  ( 39.95876352523143282, 0.000000000000000000, -6.110000000000001208 ) ) ;
#33450 = VECTOR ( 'NONE', #112479, 1000.000000000000000 ) ;
#33451 = ORIENTED_EDGE ( 'NONE', *, *, #94014, .T. ) ;
#33452 = FACE_OUTER_BOUND ( 'NONE', #87969, .T. ) ;
#33453 = CARTESIAN_POINT ( 'NONE',  ( -9.793339364578404371, 21.75929247661549581, 4.998822639870701856 ) ) ;
#33454 = FACE_OUTER_BOUND ( 'NONE', #24027, .T. ) ;
#33455 = CIRCLE ( 'NONE', #116818, 2.055000000000000604 ) ;
#33456 = ADVANCED_FACE ( 'NONE', ( #108204 ), #19093, .F. ) ;
#33457 = VECTOR ( 'NONE', #11888, 1000.000000000000000 ) ;
#33458 = CARTESIAN_POINT ( 'NONE',  ( 32.28709685856477307, 3.054999999999997495, 5.291415217122919401 ) ) ;
#33459 = VERTEX_POINT ( 'NONE', #62617 ) ;
#33460 = FACE_OUTER_BOUND ( 'NONE', #38964, .T. ) ;
#33461 = VERTEX_POINT ( 'NONE', #84385 ) ;
#33462 = ORIENTED_EDGE ( 'NONE', *, *, #89622, .F. ) ;
#33463 = ORIENTED_EDGE ( 'NONE', *, *, #59876, .F. ) ;
#33464 = DIRECTION ( 'NONE',  ( -0.6830127018922181881, 0.6830127018922202975, -0.2588190451025214056 ) ) ;
#33465 = CARTESIAN_POINT ( 'NONE',  ( 0.000000000000000000, 0.000000000000000000, 0.000000000000000000 ) ) ;
#33466 = ORIENTED_EDGE ( 'NONE', *, *, #93592, .F. ) ;
#33467 = PLANE ( 'NONE',  #129298 ) ;
#33468 = EDGE_CURVE ( 'NONE', #130345, #18115, #120507, .T. ) ;
#33469 = CARTESIAN_POINT ( 'NONE',  ( 8.999999999999941380, 8.966399257802168066, 5.000000000000000000 ) ) ;
#33470 = FACE_BOUND ( 'NONE', #87450, .T. ) ;
#33471 = ORIENTED_EDGE ( 'NONE', *, *, #40194, .F. ) ;
#33472 = LINE ( 'NONE', #134928, #62058 ) ;
#33473 = EDGE_CURVE ( 'NONE', #108519, #10814, #19798, .T. ) ;
#33474 = DIRECTION ( 'NONE',  ( -0.7071067811865486830, 0.7071067811865464625, 0.000000000000000000 ) ) ;
#33475 = DIRECTION ( 'NONE',  ( 0.6830127018922181881, 0.6830127018922202975, -0.2588190451025214056 ) ) ;
#33476 = EDGE_LOOP ( 'NONE', ( #104052, #28166, #30986, #303 ) ) ;
#33477 = CARTESIAN_POINT ( 'NONE',  ( 23.96247294953710849, -7.464222240803106570E-16, -6.094999999999989981 ) ) ;
#33478 = VERTEX_POINT ( 'NONE', #42303 ) ;
#33479 = EDGE_LOOP ( 'NONE', ( #81194, #75533, #22565 ) ) ;
#33480 = LINE ( 'NONE', #113671, #7788 ) ;
#33481 = ORIENTED_EDGE ( 'NONE', *, *, #98234, .T. ) ;
#33482 = CARTESIAN_POINT ( 'NONE',  ( 47.89126352523143737, -4.472830434245838482, -4.472830434245838482 ) ) ;
#33483 = ORIENTED_EDGE ( 'NONE', *, *, #70240, .T. ) ;
#33484 = DIRECTION ( 'NONE',  ( 0.6830127018922181881, 0.6830127018922202975, -0.2588190451025214056 ) ) ;
#33485 = PLANE ( 'NONE',  #61251 ) ;
#33486 = CARTESIAN_POINT ( 'NONE',  ( 20.99999999999984368, -2.904428200921294057, -6.989807076074993297 ) ) ;
#33487 = ORIENTED_EDGE ( 'NONE', *, *, #5976, .F. ) ;
#33488 = CARTESIAN_POINT ( 'NONE',  ( -13.10362284818588741, 2.655808543615126638, 5.000000000000000000 ) ) ;
#33489 = CARTESIAN_POINT ( 'NONE',  ( 9.423278458063483853, 11.25929247661560240, 17.85071094206582387 ) ) ;
#33490 =( LENGTH_UNIT ( ) NAMED_UNIT ( * ) SI_UNIT ( .MILLI., .METRE. ) );
#33491 = CARTESIAN_POINT ( 'NONE',  ( -3.299744871391591339, -27.71228299555208352, 4.000000000000000000 ) ) ;
#33492 = EDGE_CURVE ( 'NONE', #46825, #136452, #7488, .T. ) ;
#33493 = DIRECTION ( 'NONE',  ( 1.000000000000000000, 1.224606353822377258E-16, 0.000000000000000000 ) ) ;
#33494 = CARTESIAN_POINT ( 'NONE',  ( 152.4000000000000057, -14.29000000000013593, -12.70000000000045404 ) ) ;
#33495 = DIRECTION ( 'NONE',  ( -0.7071067811865486830, -0.7071067811865464625, 0.000000000000000000 ) ) ;
#33496 = EDGE_CURVE ( 'NONE', #103780, #41370, #107526, .T. ) ;
#33497 = VERTEX_POINT ( 'NONE', #109670 ) ;
#33498 = ORIENTED_EDGE ( 'NONE', *, *, #112427, .F. ) ;
#33499 = EDGE_LOOP ( 'NONE', ( #130964, #20560, #20710, #123928 ) ) ;
#33500 = DIRECTION ( 'NONE',  ( 0.7071067811865486830, -0.7071067811865464625, -0.000000000000000000 ) ) ;
#33501 = PLANE ( 'NONE',  #81519 ) ;
#33502 = ORIENTED_EDGE ( 'NONE', *, *, #35035, .F. ) ;
#33503 = ORIENTED_EDGE ( 'NONE', *, *, #43858, .T. ) ;
#33504 = FACE_OUTER_BOUND ( 'NONE', #130581, .T. ) ;
#33505 = EDGE_CURVE ( 'NONE', #967, #4434, #140173, .T. ) ;
#33506 = EDGE_CURVE ( 'NONE', #12339, #78479, #21235, .T. ) ;
#33507 = DIRECTION ( 'NONE',  ( -0.7071067811865486830, 0.7071067811865464625, 0.000000000000000000 ) ) ;
#33508 = ORIENTED_EDGE ( 'NONE', *, *, #44607, .T. ) ;
#33509 = CARTESIAN_POINT ( 'NONE',  ( 7.828169399223479985, 6.759292476615645917, 4.000000000000000000 ) ) ;
#33510 = AXIS2_PLACEMENT_3D ( 'NONE', #3811, #37209, #137244 ) ;
#33511 = DIRECTION ( 'NONE',  ( -0.6830127018922181881, 0.6830127018922202975, -0.2588190451025214056 ) ) ;
#33512 = AXIS2_PLACEMENT_3D ( 'NONE', #54449, #122513, #142855 ) ;
#33513 = CARTESIAN_POINT ( 'NONE',  ( 30.98373647476855552, -5.808823158059035485, -5.808823158059033709 ) ) ;
#33514 = PLANE ( 'NONE',  #124907 ) ;
#33515 = ORIENTED_EDGE ( 'NONE', *, *, #47471, .T. ) ;
#33516 = CARTESIAN_POINT ( 'NONE',  ( 107.3912635252314516, -4.472830434245839371, -4.472830434245839371 ) ) ;
#33517 = EDGE_CURVE ( 'NONE', #119845, #2171, #53132, .T. ) ;
#33518 = VECTOR ( 'NONE', #54088, 1000.000000000000000 ) ;
#33519 = CARTESIAN_POINT ( 'NONE',  ( -27.79289321881325492, -11.24070752338416490, 5.000000000000000000 ) ) ;
#33520 = LINE ( 'NONE', #121895, #79719 ) ;
#33522 = ORIENTED_EDGE ( 'NONE', *, *, #121896, .T. ) ;
#33521 = LINE ( 'NONE', #111771, #107380 ) ;
#33523 = CARTESIAN_POINT ( 'NONE',  ( -21.48921356237309155, -27.52281430457070499, 5.000000000000000000 ) ) ;
#33524 = ORIENTED_EDGE ( 'NONE', *, *, #143025, .T. ) ;
#33525 = DIRECTION ( 'NONE',  ( 0.000000000000000000, 0.000000000000000000, 1.000000000000000000 ) ) ;
#33526 = CARTESIAN_POINT ( 'NONE',  ( -31.49999999999977973, 9.052185695429077583, 5.000000000000000000 ) ) ;
#33527 = PLANE ( 'NONE',  #88640 ) ;
#33528 = CARTESIAN_POINT ( 'NONE',  ( 6.328169399223481761, -21.74070752338406365, 4.000000000000000000 ) ) ;
#33529 = EDGE_CURVE ( 'NONE', #28313, #113494, #65494, .T. ) ;
#33531 = ORIENTED_EDGE ( 'NONE', *, *, #29628, .F. ) ;
#33530 =( BOUNDED_CURVE ( )  B_SPLINE_CURVE ( 3, ( #134399, #131530, #88760, #32220 ),
 .UNSPECIFIED., .F., .F. ) 
 B_SPLINE_CURVE_WITH_KNOTS ( ( 4, 4 ),
 ( 1.964434688349496305, 3.503810798801452187 ),
 .UNSPECIFIED. ) 
 CURVE ( )  GEOMETRIC_REPRESENTATION_ITEM ( )  RATIONAL_B_SPLINE_CURVE ( ( 1.000000000000000000, 0.8120851936182298392, 0.8120851936182298392, 1.000000000000000000 ) ) 
 REPRESENTATION_ITEM ( '' )  );
#33532 = CIRCLE ( 'NONE', #40454, 9.500000000000000000 ) ;
#33533 = DIRECTION ( 'NONE',  ( -0.000000000000000000, 0.3543493200069153248, 0.9351131265310292928 ) ) ;
#33534 = DIRECTION ( 'NONE',  ( 0.3543493200069162685, -0.000000000000000000, -0.9351131265310288487 ) ) ;
#33535 = ORIENTED_EDGE ( 'NONE', *, *, #35203, .F. ) ;
#33536 = DIRECTION ( 'NONE',  ( 0.7071067811865487940, 0.7071067811865463515, -0.000000000000000000 ) ) ;
#33537 =( BOUNDED_CURVE ( )  B_SPLINE_CURVE ( 2, ( #4214, #2098, #26050, #92003, #89856, #123946, #48507, #134102, #122478, #70313, #13001, #23913, #114462 ),
 .UNSPECIFIED., .F., .T. ) 
 B_SPLINE_CURVE_WITH_KNOTS ( ( 3, 2, 2, 2, 2, 2, 3 ),
 ( 0.7666666666666667185, 0.7694444444444444864, 0.7722222222222222543, 0.7750000000000000222, 0.7777777777777777901, 0.7805555555555555580, 0.7833333333333333259 ),
 .UNSPECIFIED. ) 
 CURVE ( )  GEOMETRIC_REPRESENTATION_ITEM ( )  RATIONAL_B_SPLINE_CURVE ( ( 1.000000000000000000, 0.9659258262890683122, 1.000000000000000000, 0.9659258262890683122, 1.000000000000000000, 0.9659258262890683122, 1.000000000000000000, 0.9659258262890683122, 1.000000000000000000, 0.9659258262890683122, 1.000000000000000000, 0.9659258262890683122, 1.000000000000000000 ) ) 
 REPRESENTATION_ITEM ( '' )  );
#33538 = CARTESIAN_POINT ( 'NONE',  ( 18.48921356237309510, -27.52281430457068367, 5.000000000000000000 ) ) ;
#33539 = ORIENTED_EDGE ( 'NONE', *, *, #102459, .F. ) ;
#33540 = FACE_OUTER_BOUND ( 'NONE', #54458, .T. ) ;
#33542 = VERTEX_POINT ( 'NONE', #52425 ) ;
#33541 = LINE ( 'NONE', #99449, #13784 ) ;
#33543 = ORIENTED_EDGE ( 'NONE', *, *, #59822, .T. ) ;
#33544 = LINE ( 'NONE', #66160, #61195 ) ;
#33545 = VERTEX_POINT ( 'NONE', #85770 ) ;
#33546 = AXIS2_PLACEMENT_3D ( 'NONE', #60510, #47516, #71368 ) ;
#33547 = DIRECTION ( 'NONE',  ( 0.000000000000000000, -1.000000000000000000, 0.000000000000000000 ) ) ;
#33548 = VECTOR ( 'NONE', #78919, 1000.000000000000227 ) ;
#33549 = EDGE_CURVE ( 'NONE', #55674, #106215, #85061, .T. ) ;
#33550 = CARTESIAN_POINT ( 'NONE',  ( -29.99999999999979039, -1.068876922607804314, 4.000000000000000000 ) ) ;
#33551 = DIRECTION ( 'NONE',  ( -0.7071067811865486830, -0.7071067811865464625, 0.000000000000000000 ) ) ;
#33552 = ORIENTED_EDGE ( 'NONE', *, *, #102782, .F. ) ;
#33553 = VECTOR ( 'NONE', #120964, 1000.000000000000000 ) ;
#33554 = EDGE_CURVE ( 'NONE', #69087, #116374, #75631, .T. ) ;
#33555 = LINE ( 'NONE', #19070, #65107 ) ;
#33556 = DIRECTION ( 'NONE',  ( 1.000000000000000000, 0.000000000000000000, 0.000000000000000000 ) ) ;
#33557 = DIRECTION ( 'NONE',  ( -0.6830127018922181881, 0.6830127018922202975, -0.2588190451025214056 ) ) ;
#33558 = DIRECTION ( 'NONE',  ( -0.7071067811865487940, 0.7071067811865463515, -0.000000000000000000 ) ) ;
#33559 = CARTESIAN_POINT ( 'NONE',  ( 30.24543019189811233, -5.291415217122919401, -3.055000000000000604 ) ) ;
#33560 = CARTESIAN_POINT ( 'NONE',  ( 0.000000000000000000, 0.000000000000000000, 5.000000000000000000 ) ) ;
#33561 = ADVANCED_FACE ( 'NONE', ( #30712 ), #124145, .T. ) ;
#33562 = ADVANCED_FACE ( 'NONE', ( #31410 ), #82340, .T. ) ;
#33563 = ORIENTED_EDGE ( 'NONE', *, *, #70497, .T. ) ;
#33564 = VERTEX_POINT ( 'NONE', #110940 ) ;
#33565 = CARTESIAN_POINT ( 'NONE',  ( 125.2500000000000000, -9.735942053221458872E-16, 7.950000000000000178 ) ) ;
#33566 = ORIENTED_EDGE ( 'NONE', *, *, #114654, .T. ) ;
#33567 = ORIENTED_EDGE ( 'NONE', *, *, #40754, .F. ) ;
#33568 = CARTESIAN_POINT ( 'NONE',  ( -2.700255128608413990, -27.71228299555204089, 4.000000000000000000 ) ) ;
#33569 = CARTESIAN_POINT ( 'NONE',  ( -8.206660635421469507, 21.75929247661548516, 4.998822639870715179 ) ) ;
#33570 = VERTEX_POINT ( 'NONE', #100814 ) ;
#33571 = CARTESIAN_POINT ( 'NONE',  ( -60.18398860626900415, 28.73617430169829490, 5.000000000000000000 ) ) ;
#33572 = DIRECTION ( 'NONE',  ( -0.6830127018922180770, -0.6830127018922204085, -0.2588190451025213501 ) ) ;
#33573 = DIRECTION ( 'NONE',  ( -0.000000000000000000, 0.3543493200069153248, 0.9351131265310292928 ) ) ;
#33574 = EDGE_CURVE ( 'NONE', #31939, #66309, #1466, .T. ) ;
#33575 = CARTESIAN_POINT ( 'NONE',  ( -17.99999999999987566, 18.08204922493371214, 0.9627537363045279850 ) ) ;
#33576 = CARTESIAN_POINT ( 'NONE',  ( 122.0629301918981042, 1.637169565754157174, 6.110000000000002984 ) ) ;
#33577 = ORIENTED_EDGE ( 'NONE', *, *, #67771, .T. ) ;
#33578 = EDGE_CURVE ( 'NONE', #8853, #43828, #57340, .T. ) ;
#33579 = CARTESIAN_POINT ( 'NONE',  ( 63.48921356237309510, -27.52281430457099631, 5.000000000000000000 ) ) ;
#33580 = CARTESIAN_POINT ( 'NONE',  ( 78.87500000000000000, 7.950000000000000178, 1.460391307983218535E-15 ) ) ;
#33581 = CARTESIAN_POINT ( 'NONE',  ( 32.99999999999977973, 16.55218569542899942, 5.000000000000000000 ) ) ;
#33582 = FACE_OUTER_BOUND ( 'NONE', #100900, .T. ) ;
#33583 = CARTESIAN_POINT ( 'NONE',  ( -6.640000000000001457, 0.000000000000000000, -39.50000000000000000 ) ) ;
#33584 = CARTESIAN_POINT ( 'NONE',  ( 47.18336038379622721, -2.130196079827426203, 7.949999999999997513 ) ) ;
#33585 = CARTESIAN_POINT ( 'NONE',  ( 21.18398860626899349, 28.73617430169802134, 5.000000000000000000 ) ) ;
#33586 = PLANE ( 'NONE',  #9033 ) ;
#33587 = ORIENTED_EDGE ( 'NONE', *, *, #26202, .T. ) ;
#33588 = ORIENTED_EDGE ( 'NONE', *, *, #40410, .F. ) ;
#33589 = CARTESIAN_POINT ( 'NONE',  ( 45.62500000000000000, -7.950000000000000178, -4.867971026610729436E-16 ) ) ;
#33590 = EDGE_CURVE ( 'NONE', #129048, #78673, #125431, .T. ) ;
#33591 = CARTESIAN_POINT ( 'NONE',  ( -12.20000000000000284, -22.33999999999998565, 0.000000000000000000 ) ) ;
#33592 = LINE ( 'NONE', #122702, #131829 ) ;
#33593 = ORIENTED_EDGE ( 'NONE', *, *, #118180, .F. ) ;
#33594 = EDGE_CURVE ( 'NONE', #70001, #23807, #60929, .T. ) ;
#33595 = CARTESIAN_POINT ( 'NONE',  ( -1.055214894802011694, -0.8126175113835719666, 3.860312914990109423 ) ) ;
#33596 = CARTESIAN_POINT ( 'NONE',  ( 0.000000000000000000, 0.000000000000000000, 5.000000000000000000 ) ) ;
#33597 = CARTESIAN_POINT ( 'NONE',  ( 41.70876352523143993, -7.482591942790329030E-16, 6.110000000000001208 ) ) ;
#33598 = VERTEX_POINT ( 'NONE', #94204 ) ;
#33599 = LINE ( 'NONE', #64779, #61897 ) ;
#33600 = EDGE_LOOP ( 'NONE', ( #1312, #19872, #115860, #79418 ) ) ;
#33601 = EDGE_LOOP ( 'NONE', ( #71716, #30536, #95297, #71122 ) ) ;
#33602 = EDGE_CURVE ( 'NONE', #27758, #105889, #61663, .T. ) ;
#33603 = CARTESIAN_POINT ( 'NONE',  ( 0.000000000000000000, 0.000000000000000000, 5.000000000000000000 ) ) ;
#33604 = LINE ( 'NONE', #75661, #63947 ) ;
#33605 = LINE ( 'NONE', #45902, #65183 ) ;
#33606 = DIRECTION ( 'NONE',  ( 0.7071067811865487940, 0.7071067811865463515, 0.000000000000000000 ) ) ;
#33607 = EDGE_LOOP ( 'NONE', ( #104582, #57827, #107517 ) ) ;
#33608 = DIRECTION ( 'NONE',  ( -0.000000000000000000, 0.000000000000000000, 1.000000000000000000 ) ) ;
#33609 = VERTEX_POINT ( 'NONE', #3603 ) ;
#33610 = CARTESIAN_POINT ( 'NONE',  ( 85.02126352523144703, -4.472830434245838482, -4.472830434245840259 ) ) ;
#33611 = PLANE ( 'NONE',  #4470 ) ;
#33612 =( NAMED_UNIT ( * ) SI_UNIT ( $, .STERADIAN. ) SOLID_ANGLE_UNIT ( ) );
#33613 = CARTESIAN_POINT ( 'NONE',  ( -34.49999999999974420, -20.94567065516883275, 4.994342998332162331 ) ) ;
#33614 = LINE ( 'NONE', #65543, #104124 ) ;
#33615 = DIRECTION ( 'NONE',  ( -0.000000000000000000, 0.000000000000000000, 1.000000000000000000 ) ) ;
#33616 = EDGE_CURVE ( 'NONE', #25257, #95492, #81958, .T. ) ;
#33617 = VECTOR ( 'NONE', #138960, 1000.000000000000000 ) ;
#33618 = ORIENTED_EDGE ( 'NONE', *, *, #76203, .F. ) ;
#33619 = LINE ( 'NONE', #67687, #61561 ) ;
#33620 = CARTESIAN_POINT ( 'NONE',  ( 58.24543019189810877, -5.291415217122918513, -3.055000000000000160 ) ) ;
#33621 = AXIS2_PLACEMENT_3D ( 'NONE', #78872, #111467, #67269 ) ;
#33622 = CARTESIAN_POINT ( 'NONE',  ( -8.816011393731004731, 28.73617430169781173, 5.000000000000000000 ) ) ;
#33623 = CARTESIAN_POINT ( 'NONE',  ( 34.92499999999998295, -9.415263340095632927, 16.98967855471611799 ) ) ;
#33624 = PLANE ( 'NONE',  #3945 ) ;
#33625 = ORIENTED_EDGE ( 'NONE', *, *, #86257, .F. ) ;
#33626 = CARTESIAN_POINT ( 'NONE',  ( -12.20000000000000817, -1.670812611072399357E-15, -39.50000000000000000 ) ) ;
#33628 = EDGE_CURVE ( 'NONE', #54899, #5733, #80194, .T. ) ;
#33627 = FILL_AREA_STYLE_COLOUR ( '', #60746 ) ;
#33629 = EDGE_LOOP ( 'NONE', ( #52471, #122740, #47197, #32204 ) ) ;
#33630 = VECTOR ( 'NONE', #108727, 1000.000000000000000 ) ;
#33631 = CARTESIAN_POINT ( 'NONE',  ( 0.000000000000000000, 0.000000000000000000, 7.950000000000000178 ) ) ;
#33632 = VERTEX_POINT ( 'NONE', #126145 ) ;
#33633 = LINE ( 'NONE', #54662, #139569 ) ;
#33634 = CARTESIAN_POINT ( 'NONE',  ( -2.999999999999979128, -12.03360074219761700, 5.000000000000000000 ) ) ;
#33635 = DIRECTION ( 'NONE',  ( 0.6830127018922180770, -0.6830127018922204085, -0.2588190451025213501 ) ) ;
#33636 = FACE_OUTER_BOUND ( 'NONE', #81293, .T. ) ;
#33637 = FACE_BOUND ( 'NONE', #89066, .T. ) ;
#33638 = CARTESIAN_POINT ( 'NONE',  ( -24.18398860626899705, 28.73617430169804265, 5.000000000000000000 ) ) ;
#33639 = DIRECTION ( 'NONE',  ( -0.6830127018922180770, -0.6830127018922204085, -0.2588190451025213501 ) ) ;
#33640 = LINE ( 'NONE', #66965, #136052 ) ;
#33642 = ORIENTED_EDGE ( 'NONE', *, *, #27567, .T. ) ;
#33641 = PLANE ( 'NONE',  #99068 ) ;
#33643 = CARTESIAN_POINT ( 'NONE',  ( -42.29974487139158157, -27.71228299555235708, 4.000000000000000000 ) ) ;
#33644 =( GEOMETRIC_REPRESENTATION_CONTEXT ( 3 ) GLOBAL_UNCERTAINTY_ASSIGNED_CONTEXT ( ( #21563 ) ) GLOBAL_UNIT_ASSIGNED_CONTEXT ( ( #129652, #29617, #86170 ) ) REPRESENTATION_CONTEXT ( 'NONE', 'WORKASPACE' ) );
#33645 = VERTEX_POINT ( 'NONE', #39134 ) ;
#33646 = VECTOR ( 'NONE', #109057, 1000.000000000000000 ) ;
#33648 = ORIENTED_EDGE ( 'NONE', *, *, #80992, .F. ) ;
#33647 = VECTOR ( 'NONE', #106736, 1000.000000000000227 ) ;
#33649 = CARTESIAN_POINT ( 'NONE',  ( 77.49543019189810877, 5.291415217122916737, 3.055000000000001936 ) ) ;
#33650 = ORIENTED_EDGE ( 'NONE', *, *, #88380, .F. ) ;
#33651 = CIRCLE ( 'NONE', #114630, 2.500000000000000444 ) ;
#33652 = CARTESIAN_POINT ( 'NONE',  ( -6.183988606268994381, 28.73617430169791476, 5.000000000000000000 ) ) ;
#33653 = EDGE_CURVE ( 'NONE', #91708, #3709, #38418, .T. ) ;
#33654 = EDGE_LOOP ( 'NONE', ( #34654, #149, #92124, #119468 ) ) ;
#33655 = CARTESIAN_POINT ( 'NONE',  ( 27.48921356237309155, -27.52281430457074762, 5.000000000000000000 ) ) ;
#33656 = DIRECTION ( 'NONE',  ( -0.7071067811865486830, -0.7071067811865464625, -0.000000000000000000 ) ) ;
#33657 = CARTESIAN_POINT ( 'NONE',  ( -34.92500000000001137, 0.6624618758389808626, 4.000000000000000000 ) ) ;
#33658 = LINE ( 'NONE', #79329, #96460 ) ;
#33660 = DIRECTION ( 'NONE',  ( -0.7071067811865486830, -0.7071067811865464625, 0.000000000000000000 ) ) ;
#33659 = FACE_OUTER_BOUND ( 'NONE', #121179, .T. ) ;
#33661 = CARTESIAN_POINT ( 'NONE',  ( -26.99451991528749417, 28.92564299267956685, 4.000000000000000000 ) ) ;
#33662 = FACE_OUTER_BOUND ( 'NONE', #107099, .T. ) ;
#33663 = VERTEX_POINT ( 'NONE', #93508 ) ;
#33664 = FACE_OUTER_BOUND ( 'NONE', #97464, .T. ) ;
#33665 = ORIENTED_EDGE ( 'NONE', *, *, #108560, .T. ) ;
#33666 = FACE_OUTER_BOUND ( 'NONE', #83947, .T. ) ;
#33667 = CARTESIAN_POINT ( 'NONE',  ( 12.18398860626900060, 28.73617430169795739, 5.000000000000000000 ) ) ;
#33668 = ORIENTED_EDGE ( 'NONE', *, *, #62620, .F. ) ;
#33669 = ORIENTED_EDGE ( 'NONE', *, *, #133650, .T. ) ;
#33670 = ORIENTED_EDGE ( 'NONE', *, *, #11409, .F. ) ;
#33671 = EDGE_CURVE ( 'NONE', #122655, #40407, #117184, .T. ) ;
#33672 = EDGE_CURVE ( 'NONE', #89696, #50223, #36971, .T. ) ;
#33673 = CARTESIAN_POINT ( 'NONE',  ( 30.33376352523143993, 6.110000000000001208, 1.122388791418549305E-15 ) ) ;
#33674 = ORIENTED_EDGE ( 'NONE', *, *, #22815, .T. ) ;
#33675 = CARTESIAN_POINT ( 'NONE',  ( 20.70025512860841133, -27.71228299555191654, 4.000000000000000000 ) ) ;
#33676 = EDGE_CURVE ( 'NONE', #106936, #60182, #81226, .T. ) ;
#33677 = CARTESIAN_POINT ( 'NONE',  ( 18.17159235450331778, 2.500000000000001332, 0.000000000000000000 ) ) ;
#33678 = CARTESIAN_POINT ( 'NONE',  ( 4.296236474768552860, 7.934999999999990727, -1.457635852685135314E-15 ) ) ;
#33679 = CARTESIAN_POINT ( 'NONE',  ( 14.19664412335589887, 5.303595669547504166, -31.75409969297703938 ) ) ;
#33680 = VERTEX_POINT ( 'NONE', #71774 ) ;
#33681 = ADVANCED_FACE ( 'NONE', ( #126827 ), #47895, .F. ) ;
#33682 = CARTESIAN_POINT ( 'NONE',  ( -34.92500000000001137, -4.168643983631880268, 15.00153835162127969 ) ) ;
#33683 = LINE ( 'NONE', #45286, #93742 ) ;
#33685 = ORIENTED_EDGE ( 'NONE', *, *, #132604, .F. ) ;
#33684 = CARTESIAN_POINT ( 'NONE',  ( 0.000000000000000000, 0.000000000000000000, 5.000000000000000000 ) ) ;
#33686 = ORIENTED_EDGE ( 'NONE', *, *, #92256, .T. ) ;
#33687 = FILL_AREA_STYLE_COLOUR ( '', #105124 ) ;
#33688 = FACE_OUTER_BOUND ( 'NONE', #24588, .T. ) ;
#33689 = DIRECTION ( 'NONE',  ( 0.7071067811865487940, 0.7071067811865463515, 0.000000000000000000 ) ) ;
#33690 = ADVANCED_FACE ( 'NONE', ( #72355 ), #93344, .F. ) ;
#33691 = ORIENTED_EDGE ( 'NONE', *, *, #136946, .T. ) ;
#33692 = DIRECTION ( 'NONE',  ( 0.000000000000000000, -1.000000000000000000, 0.000000000000000000 ) ) ;
#33693 = CARTESIAN_POINT ( 'NONE',  ( 34.45011844616453800, -14.99769585840590302, 5.000000000000001776 ) ) ;
#33694 = ORIENTED_EDGE ( 'NONE', *, *, #106933, .F. ) ;
#33695 = CARTESIAN_POINT ( 'NONE',  ( 29.99999999999999645, -2.375000000000000000, -0.000000000000000000 ) ) ;
#33696 = PLANE ( 'NONE',  #135092 ) ;
#33697 = EDGE_CURVE ( 'NONE', #38602, #141315, #18604, .T. ) ;
#33698 = FACE_OUTER_BOUND ( 'NONE', #141410, .T. ) ;
#33699 = LINE ( 'NONE', #100371, #42436 ) ;
#33700 = LINE ( 'NONE', #1713, #28298 ) ;
#33701 = DIRECTION ( 'NONE',  ( -1.000000000000000000, -1.224606353822377258E-16, -0.000000000000000000 ) ) ;
#33702 = CARTESIAN_POINT ( 'NONE',  ( -2.381615093980022024, -2.240707523384260824, 13.37739548510239906 ) ) ;
#33703 = ORIENTED_EDGE ( 'NONE', *, *, #104552, .F. ) ;
#33704 = CARTESIAN_POINT ( 'NONE',  ( 1.369639479247480862, 4.811953009385816285E-13, 6.725360520752516891 ) ) ;
#33705 = ORIENTED_EDGE ( 'NONE', *, *, #67696, .F. ) ;
#33706 = EDGE_CURVE ( 'NONE', #137770, #23390, #104184, .T. ) ;
#33707 = ADVANCED_FACE ( 'NONE', ( #128133 ), #52415, .T. ) ;
#33708 = DIRECTION ( 'NONE',  ( 0.000000000000000000, 0.000000000000000000, 1.000000000000000000 ) ) ;
#33709 = DIRECTION ( 'NONE',  ( 0.000000000000000000, 0.000000000000000000, 1.000000000000000000 ) ) ;
#33710 =( BOUNDED_CURVE ( )  B_SPLINE_CURVE ( 3, ( #66206, #101664, #90819, #45891 ),
 .UNSPECIFIED., .F., .T. ) 
 B_SPLINE_CURVE_WITH_KNOTS ( ( 4, 4 ),
 ( 1.208578181583249256, 1.359146454359418055 ),
 .UNSPECIFIED. ) 
 CURVE ( )  GEOMETRIC_REPRESENTATION_ITEM ( )  RATIONAL_B_SPLINE_CURVE ( ( 1.000000000000000000, 0.9981116584018960847, 0.9981116584018960847, 1.000000000000000000 ) ) 
 REPRESENTATION_ITEM ( '' )  );
#33711 =( LENGTH_UNIT ( ) NAMED_UNIT ( * ) SI_UNIT ( .MILLI., .METRE. ) );
#33712 = VECTOR ( 'NONE', #97375, 1000.000000000000000 ) ;
#33713 = FACE_OUTER_BOUND ( 'NONE', #50367, .T. ) ;
#33714 = ORIENTED_EDGE ( 'NONE', *, *, #95553, .F. ) ;
#33715 = DIRECTION ( 'NONE',  ( 0.3543493200069162685, -0.000000000000000000, -0.9351131265310288487 ) ) ;
#33716 = LINE ( 'NONE', #32271, #129825 ) ;
#33717 = CARTESIAN_POINT ( 'NONE',  ( -34.92499999999999005, -7.730000000000016414, 3.180000000000000160 ) ) ;
#33718 = VECTOR ( 'NONE', #112049, 1000.000000000000000 ) ;
#33719 = ORIENTED_EDGE ( 'NONE', *, *, #52016, .T. ) ;
#33720 = EDGE_CURVE ( 'NONE', #45460, #35930, #125988, .T. ) ;
#33721 = PLANE ( 'NONE',  #106545 ) ;
#33722 = CARTESIAN_POINT ( 'NONE',  ( 112.8541666666666714, -2.130196079827406219, -7.950000000000012612 ) ) ;
#33723 = FACE_OUTER_BOUND ( 'NONE', #103861, .T. ) ;
#33724 = CARTESIAN_POINT ( 'NONE',  ( 52.77083333333332149, -7.949999999999998401, -2.130196079827426203 ) ) ;
#33725 = CARTESIAN_POINT ( 'NONE',  ( 66.48921356237309510, -27.52281430457101763, 5.000000000000000000 ) ) ;
#33726 = CARTESIAN_POINT ( 'NONE',  ( 53.57876352523144448, -7.482591942790327058E-16, 6.109999999999999432 ) ) ;
#33727 = FACE_OUTER_BOUND ( 'NONE', #110644, .T. ) ;
#33728 = ADVANCED_FACE ( 'NONE', ( #27348 ), #17210, .F. ) ;
#33729 = EDGE_CURVE ( 'NONE', #21534, #24725, #73726, .T. ) ;
#33730 = CARTESIAN_POINT ( 'NONE',  ( -30.48921356237309510, -27.52281430457076894, 5.000000000000000000 ) ) ;
#33731 = VECTOR ( 'NONE', #54946, 999.9999999999998863 ) ;
#33732 = LINE ( 'NONE', #87380, #64955 ) ;
#33733 = ORIENTED_EDGE ( 'NONE', *, *, #47607, .F. ) ;
#33734 =( NAMED_UNIT ( * ) PLANE_ANGLE_UNIT ( ) SI_UNIT ( $, .RADIAN. ) );
#33735 = ORIENTED_EDGE ( 'NONE', *, *, #143397, .F. ) ;
#33736 = CARTESIAN_POINT ( 'NONE',  ( -4.828169399223495084, -14.24070752338413648, 4.000000000000000000 ) ) ;
#33737 = FACE_OUTER_BOUND ( 'NONE', #44441, .T. ) ;
#33738 = EDGE_CURVE ( 'NONE', #55203, #77465, #127388, .T. ) ;
#33739 = DIRECTION ( 'NONE',  ( 0.7071067811865486830, -0.7071067811865464625, -0.000000000000000000 ) ) ;
#33740 = PLANE ( 'NONE',  #76660 ) ;
#33741 = CARTESIAN_POINT ( 'NONE',  ( 8.510786437626906675, -27.52281430457049183, 5.000000000000000000 ) ) ;
#33742 = EDGE_CURVE ( 'NONE', #78506, #1174, #83187, .T. ) ;
#33743 = CARTESIAN_POINT ( 'NONE',  ( 51.29974487139158867, -27.71228299555242103, 4.000000000000000000 ) ) ;
#33744 = CARTESIAN_POINT ( 'NONE',  ( -21.18398860626899349, 28.73617430169802134, 5.000000000000000000 ) ) ;
#33745 = ORIENTED_EDGE ( 'NONE', *, *, #62331, .F. ) ;
#33746 = EDGE_LOOP ( 'NONE', ( #138608, #141589, #121346, #111903 ) ) ;
#33747 = DIRECTION ( 'NONE',  ( 0.7071067811865486830, -0.7071067811865464625, -0.000000000000000000 ) ) ;
#33748 = LINE ( 'NONE', #78661, #130684 ) ;
#33749 = VECTOR ( 'NONE', #120749, 1000.000000000000000 ) ;
#33750 = CARTESIAN_POINT ( 'NONE',  ( -28.82816939922333077, -17.24070752338409918, 4.000000000000000000 ) ) ;
#33751 = CARTESIAN_POINT ( 'NONE',  ( 88.01669371712955581, 7.950000000000001066, -2.130196079827421318 ) ) ;
#33752 = CARTESIAN_POINT ( 'NONE',  ( -12.18398860626900060, 28.73617430169795739, 5.000000000000000000 ) ) ;
#33753 = AXIS2_PLACEMENT_3D ( 'NONE', #36585, #34460, #3236 ) ;
#33754 = CARTESIAN_POINT ( 'NONE',  ( 66.18398860626901126, 28.73617430169833753, 5.000000000000000000 ) ) ;
#33755 = ORIENTED_EDGE ( 'NONE', *, *, #94951, .F. ) ;
#33756 = CARTESIAN_POINT ( 'NONE',  ( 76.10416666666667140, 2.130196079827422206, 7.950000000000001954 ) ) ;
#33757 = AXIS2_PLACEMENT_3D ( 'NONE', #4157, #123175, #138153 ) ;
#33758 = EDGE_CURVE ( 'NONE', #76267, #102238, #60763, .T. ) ;
#33759 = FACE_OUTER_BOUND ( 'NONE', #133690, .T. ) ;
#33760 = FACE_OUTER_BOUND ( 'NONE', #22317, .T. ) ;
#33761 = FACE_OUTER_BOUND ( 'NONE', #131403, .T. ) ;
#33762 = VECTOR ( 'NONE', #98422, 1000.000000000000000 ) ;
#33763 = VERTEX_POINT ( 'NONE', #117907 ) ;
#33764 = EDGE_CURVE ( 'NONE', #16747, #84400, #28087, .T. ) ;
#33765 = LINE ( 'NONE', #67091, #49129 ) ;
#33766 = ORIENTED_EDGE ( 'NONE', *, *, #104713, .F. ) ;
#33767 = FACE_OUTER_BOUND ( 'NONE', #89762, .T. ) ;
#33768 = CARTESIAN_POINT ( 'NONE',  ( 70.72959685856477563, -6.110000000000000320, -1.637169565754161393 ) ) ;
#33769 = CARTESIAN_POINT ( 'NONE',  ( 4.600000000000001421, 2.055000000000001492, 2.516649172247811554E-16 ) ) ;
#33770 = EDGE_LOOP ( 'NONE', ( #135593, #107271, #48198, #70843 ) ) ;
#33771 = DIRECTION ( 'NONE',  ( -0.7071067811865486830, -0.7071067811865464625, -0.000000000000000000 ) ) ;
#33772 = DIRECTION ( 'NONE',  ( 1.000000000000000000, 0.000000000000000000, 0.000000000000000000 ) ) ;
#33773 = DIRECTION ( 'NONE',  ( 0.000000000000000000, -1.000000000000000000, 0.000000000000000000 ) ) ;
#33774 = CARTESIAN_POINT ( 'NONE',  ( -36.48921356237310221, -27.52281430457080802, 5.000000000000000000 ) ) ;
#33775 = CARTESIAN_POINT ( 'NONE',  ( -12.19999999999999574, -60.26999999999998892, 25.00000000000000000 ) ) ;
#33777 = VERTEX_POINT ( 'NONE', #107066 ) ;
#33776 = CARTESIAN_POINT ( 'NONE',  ( 127.0000000000000000, 1.864289179696898779, 6.174700466780991270 ) ) ;
#33778 = DIRECTION ( 'NONE',  ( -1.000000000000000000, -0.000000000000000000, -0.000000000000000000 ) ) ;
#33779 = CARTESIAN_POINT ( 'NONE',  ( 57.18398860626899705, 28.73617430169827358, 5.000000000000000000 ) ) ;
#33780 = LINE ( 'NONE', #69253, #72615 ) ;
#33781 = DIRECTION ( 'NONE',  ( 0.000000000000000000, 0.000000000000000000, 1.000000000000000000 ) ) ;
#33782 = VERTEX_POINT ( 'NONE', #70904 ) ;
#33783 = ORIENTED_EDGE ( 'NONE', *, *, #117897, .T. ) ;
#33784 = CARTESIAN_POINT ( 'NONE',  ( 64.89626352523144703, 4.472830434245840259, -4.472830434245839371 ) ) ;
#33785 = ORIENTED_EDGE ( 'NONE', *, *, #40253, .T. ) ;
#33786 = DIRECTION ( 'NONE',  ( 0.7071067811865487940, 0.7071067811865463515, -0.000000000000000000 ) ) ;
#33787 = CARTESIAN_POINT ( 'NONE',  ( -7.140000000000001457, -35.56014942880461405, -8.278119684037248405 ) ) ;
#33788 = DIRECTION ( 'NONE',  ( 0.000000000000000000, 0.000000000000000000, 1.000000000000000000 ) ) ;
#33789 = CARTESIAN_POINT ( 'NONE',  ( -26.67183060077627488, 2.259292476615697876, 4.000000000000000000 ) ) ;
#33790 = DIRECTION ( 'NONE',  ( 0.7071067811865487940, -0.7071067811865463515, 0.000000000000000000 ) ) ;
#33791 = VERTEX_POINT ( 'NONE', #15724 ) ;
#33792 = EDGE_LOOP ( 'NONE', ( #64143, #102380, #29702, #115496, #91795, #28090 ) ) ;
#33793 = DIRECTION ( 'NONE',  ( 0.7071067811865487940, 0.7071067811865463515, -0.000000000000000000 ) ) ;
#33794 = CARTESIAN_POINT ( 'NONE',  ( -16.95726112187796986, -0.7092031756307797252, -35.09041480028862736 ) ) ;
#33795 = ORIENTED_EDGE ( 'NONE', *, *, #16352, .F. ) ;
#33796 = LINE ( 'NONE', #108432, #67589 ) ;
#33797 = CARTESIAN_POINT ( 'NONE',  ( 24.39999999999999858, -1.600000000000094458, 34.92499999999998295 ) ) ;
#33798 = DIRECTION ( 'NONE',  ( 0.7071067811865487940, -0.7071067811865463515, 0.000000000000000000 ) ) ;
#33799 = VERTEX_POINT ( 'NONE', #43970 ) ;
#33800 = FACE_BOUND ( 'NONE', #30266, .T. ) ;
#33801 = LINE ( 'NONE', #57703, #17719 ) ;
#33802 = LINE ( 'NONE', #46859, #69836 ) ;
#33803 = CARTESIAN_POINT ( 'NONE',  ( -27.29974487139158512, -27.71228299555225405, 4.000000000000000000 ) ) ;
#33804 =( LENGTH_UNIT ( ) NAMED_UNIT ( * ) SI_UNIT ( .MILLI., .METRE. ) );
#33805 = DIRECTION ( 'NONE',  ( -0.7071067811865486830, 0.7071067811865464625, 0.000000000000000000 ) ) ;
#33807 = EDGE_LOOP ( 'NONE', ( #100248, #81552, #101357 ) ) ;
#33806 = CIRCLE ( 'NONE', #142565, 0.5000000000000004441 ) ;
#33808 = ORIENTED_EDGE ( 'NONE', *, *, #47299, .T. ) ;
#33809 = CARTESIAN_POINT ( 'NONE',  ( 101.1204301918981230, 3.055000000000001936, -5.291415217122916737 ) ) ;
#33810 = ORIENTED_EDGE ( 'NONE', *, *, #1664, .T. ) ;
#33811 = AXIS2_PLACEMENT_3D ( 'NONE', #112580, #57509, #46663 ) ;
#33812 = LINE ( 'NONE', #67144, #92888 ) ;
#33813 = ORIENTED_EDGE ( 'NONE', *, *, #99554, .T. ) ;
#33814 = EDGE_CURVE ( 'NONE', #110456, #89877, #86037, .T. ) ;
#33815 = CARTESIAN_POINT ( 'NONE',  ( 6.066782984417857350, 2.500000000000000888, 0.000000000000000000 ) ) ;
#33816 = CARTESIAN_POINT ( 'NONE',  ( 3.399972949537105826, 4.461849672132297329, -4.461849672132302658 ) ) ;
#33817 = LINE ( 'NONE', #46129, #7728 ) ;
#33818 = ORIENTED_EDGE ( 'NONE', *, *, #123570, .F. ) ;
#33819 = LINE ( 'NONE', #134565, #131698 ) ;
#33820 = DIRECTION ( 'NONE',  ( 1.000000000000000000, -2.496005001405478586E-15, 6.809571051365719919E-16 ) ) ;
#33821 = DIRECTION ( 'NONE',  ( 0.000000000000000000, -1.000000000000000000, 0.000000000000000000 ) ) ;
#33822 = VECTOR ( 'NONE', #98092, 1000.000000000000000 ) ;
#33823 = CARTESIAN_POINT ( 'NONE',  ( 17.99999999999987921, 11.96639925780213254, 5.000000000000000000 ) ) ;
#33824 = CARTESIAN_POINT ( 'NONE',  ( 32.52487387214934245, 14.25929247661556865, 9.797011795316713290 ) ) ;
#33825 = CARTESIAN_POINT ( 'NONE',  ( 9.722814304570524868, -21.72500000000000497, 5.000000000000000000 ) ) ;
#33826 = CARTESIAN_POINT ( 'NONE',  ( 30.18398860626900060, 28.73617430169808173, 5.000000000000000000 ) ) ;
#33827 = ORIENTED_EDGE ( 'NONE', *, *, #13152, .F. ) ;
#33828 = DIRECTION ( 'NONE',  ( -0.6830127018922181881, 0.6830127018922202975, -0.2588190451025214056 ) ) ;
#33829 = CARTESIAN_POINT ( 'NONE',  ( 6.183988606268994381, 28.73617430169791476, 5.000000000000000000 ) ) ;
#33830 = EDGE_CURVE ( 'NONE', #7428, #35701, #54857, .T. ) ;
#33831 = VERTEX_POINT ( 'NONE', #119349 ) ;
#33832 = ORIENTED_EDGE ( 'NONE', *, *, #36171, .F. ) ;
#33833 = ADVANCED_FACE ( 'NONE', ( #43266 ), #8427, .T. ) ;
#33834 = EDGE_CURVE ( 'NONE', #93386, #59760, #30220, .T. ) ;
#33835 = ORIENTED_EDGE ( 'NONE', *, *, #90482, .T. ) ;
#33836 = CARTESIAN_POINT ( 'NONE',  ( 53.08376352523143282, -6.110000000000001208, -3.741295971395164515E-16 ) ) ;
#33837 = EDGE_LOOP ( 'NONE', ( #120753, #32066, #57331, #89782 ) ) ;
#33838 = AXIS2_PLACEMENT_3D ( 'NONE', #77125, #120552, #21284 ) ;
#33839 = EDGE_CURVE ( 'NONE', #81231, #71971, #107765, .T. ) ;
#33840 = EDGE_CURVE ( 'NONE', #116493, #86617, #9133, .T. ) ;
#33841 = DIRECTION ( 'NONE',  ( 0.6830127018922180770, -0.6830127018922204085, -0.2588190451025213501 ) ) ;
#33842 = VECTOR ( 'NONE', #99517, 1000.000000000000000 ) ;
#33843 = CARTESIAN_POINT ( 'NONE',  ( -2.287527050462894618, 0.000000000000000000, 6.094999999999989981 ) ) ;
#33844 = CARTESIAN_POINT ( 'NONE',  ( 93.33376352523144703, 6.110000000000001208, 1.122388791418549305E-15 ) ) ;
#33845 = DIRECTION ( 'NONE',  ( 0.7071067811865486830, -0.7071067811865464625, -0.000000000000000000 ) ) ;
#33846 = COLOUR_RGB ( '', 0.66274510, 0.83137255, 0.94901961) ;
#33847 = ADVANCED_FACE ( 'NONE', ( #55566 ), #88191, .F. ) ;
#33848 = VERTEX_POINT ( 'NONE', #141112 ) ;
#33849 = DIRECTION ( 'NONE',  ( 0.7071067811865486830, -0.7071067811865464625, -0.000000000000000000 ) ) ;
#33850 = AXIS2_PLACEMENT_3D ( 'NONE', #103589, #47156, #68871 ) ;
#33851 = CARTESIAN_POINT ( 'NONE',  ( 2.510786437626908008, -27.52281430457053446, 5.000000000000000000 ) ) ;
#33852 = ORIENTED_EDGE ( 'NONE', *, *, #20937, .F. ) ;
#33853 = CYLINDRICAL_SURFACE ( 'NONE', #30694, 0.5000000000000000000 ) ;
#33854 = DIRECTION ( 'NONE',  ( 1.000000000000000000, -0.000000000000000000, -0.000000000000000000 ) ) ;
#33855 = EDGE_CURVE ( 'NONE', #108597, #1998, #118660, .T. ) ;
#33856 = VERTEX_POINT ( 'NONE', #65021 ) ;
#33857 = LINE ( 'NONE', #22919, #89770 ) ;
#33858 = VERTEX_POINT ( 'NONE', #130275 ) ;
#33859 = ORIENTED_EDGE ( 'NONE', *, *, #53076, .F. ) ;
#33860 = EDGE_LOOP ( 'NONE', ( #25036, #138873, #29543, #27878 ) ) ;
#33861 = CARTESIAN_POINT ( 'NONE',  ( 122.8495968585647660, 6.109999999999996767, 1.637169565754163836 ) ) ;
#33862 = CARTESIAN_POINT ( 'NONE',  ( -33.18398860626899705, 28.73617430169810305, 5.000000000000000000 ) ) ;
#33863 = FACE_OUTER_BOUND ( 'NONE', #30961, .T. ) ;
#33864 = PLANE ( 'NONE',  #99769 ) ;
#33865 = ORIENTED_EDGE ( 'NONE', *, *, #30070, .F. ) ;
#33866 = ADVANCED_FACE ( 'NONE', ( #141870 ), #21502, .F. ) ;
#33867 = CARTESIAN_POINT ( 'NONE',  ( 16.89540314143521726, 2.126176841940962348, 7.934999999999989839 ) ) ;
#33868 = DIRECTION ( 'NONE',  ( -0.5735764363510501562, 0.8191520442889890230, 1.003171929053521419E-16 ) ) ;
#33869 = PLANE ( 'NONE',  #85413 ) ;
#33870 = CARTESIAN_POINT ( 'NONE',  ( 125.2500000000000000, -9.735942053221458872E-16, 7.950000000000000178 ) ) ;
#33871 = ORIENTED_EDGE ( 'NONE', *, *, #68244, .F. ) ;
#33872 = ORIENTED_EDGE ( 'NONE', *, *, #75182, .T. ) ;
#33874 = VERTEX_POINT ( 'NONE', #65760 ) ;
#33873 = EDGE_CURVE ( 'NONE', #85530, #103515, #110612, .T. ) ;
#33875 = SURFACE_SIDE_STYLE ('',( #77402 ) ) ;
#33876 = CARTESIAN_POINT ( 'NONE',  ( 58.45833333333333570, 3.974999999999997424, 6.884901960086288852 ) ) ;
#33877 = VECTOR ( 'NONE', #59961, 1000.000000000000000 ) ;
#33878 = CARTESIAN_POINT ( 'NONE',  ( -36.29974487139159578, -27.71228299555231445, 4.000000000000000000 ) ) ;
#33879 = LINE ( 'NONE', #78098, #55236 ) ;
#33880 = EDGE_CURVE ( 'NONE', #104041, #122724, #86977, .T. ) ;
#33881 = DIRECTION ( 'NONE',  ( 0.3543493200069164351, 2.781805975412904658E-17, -0.9351131265310288487 ) ) ;
#33882 = LINE ( 'NONE', #57079, #88907 ) ;
#33883 = DIRECTION ( 'NONE',  ( -0.3543493200069163240, 0.000000000000000000, -0.9351131265310288487 ) ) ;
#33884 = CARTESIAN_POINT ( 'NONE',  ( -28.49999999999980460, 10.46639925780215563, 5.000000000000000000 ) ) ;
#33885 = EDGE_CURVE ( 'NONE', #3157, #100719, #130988, .T. ) ;
#33886 = ORIENTED_EDGE ( 'NONE', *, *, #13522, .T. ) ;
#33887 = CARTESIAN_POINT ( 'NONE',  ( 17.99451991528748351, 28.92564299267950645, 4.000000000000000000 ) ) ;
#33888 = AXIS2_PLACEMENT_3D ( 'NONE', #22781, #88096, #130906 ) ;
#33889 = ORIENTED_EDGE ( 'NONE', *, *, #85839, .T. ) ;
#33890 = CARTESIAN_POINT ( 'NONE',  ( 17.33001774602888645, -2.066807786662312463, -32.74895997315899621 ) ) ;
#33891 = ORIENTED_EDGE ( 'NONE', *, *, #74699, .F. ) ;
#33892 = EDGE_CURVE ( 'NONE', #19670, #21326, #120792, .T. ) ;
#33893 = EDGE_CURVE ( 'NONE', #79777, #140721, #33130, .T. ) ;
#33894 = DIRECTION ( 'NONE',  ( -0.7071067811865486830, -0.7071067811865464625, 0.000000000000000000 ) ) ;
#33896 = ORIENTED_EDGE ( 'NONE', *, *, #75901, .F. ) ;
#33895 = CARTESIAN_POINT ( 'NONE',  ( -23.99999999999983302, 7.007997736742422212, -8.085015511992168058 ) ) ;
#33897 = CARTESIAN_POINT ( 'NONE',  ( 22.17183060077631396, 12.75929247661558996, 4.000000000000000000 ) ) ;
#33898 = ORIENTED_EDGE ( 'NONE', *, *, #43480, .F. ) ;
#33899 = DIRECTION ( 'NONE',  ( -1.000000000000000000, 2.496005001405478586E-15, -0.000000000000000000 ) ) ;
#33900 = VERTEX_POINT ( 'NONE', #54165 ) ;
#33901 = CARTESIAN_POINT ( 'NONE',  ( 34.42499999999998295, 16.54139925780187781, 5.000000000000000000 ) ) ;
#33902 = ORIENTED_EDGE ( 'NONE', *, *, #115834, .T. ) ;
#33903 = EDGE_CURVE ( 'NONE', #89049, #50410, #70970, .T. ) ;
#33904 = LINE ( 'NONE', #121595, #66110 ) ;
#33905 = AXIS2_PLACEMENT_3D ( 'NONE', #19881, #97437, #7573 ) ;
#33906 = CARTESIAN_POINT ( 'NONE',  ( 116.6000270504628844, 5.819803920172570422, 5.819803920172574863 ) ) ;
#33907 = FACE_OUTER_BOUND ( 'NONE', #13178, .T. ) ;
#33908 = LINE ( 'NONE', #68001, #57877 ) ;
#33909 = STYLED_ITEM ( 'NONE', ( #112239 ), #91558 ) ;
#33910 = EDGE_CURVE ( 'NONE', #133767, #87366, #143265, .T. ) ;
#33911 = LINE ( 'NONE', #9232, #109747 ) ;
#33912 = LINE ( 'NONE', #1929, #129454 ) ;
#33913 = CARTESIAN_POINT ( 'NONE',  ( 16.62500000000000000, 6.094999999999989981, -1.119633336120465690E-15 ) ) ;
#33914 = DIRECTION ( 'NONE',  ( 0.6830127018922181881, 0.6830127018922202975, -0.2588190451025214056 ) ) ;
#33915 = LINE ( 'NONE', #67250, #79093 ) ;
#33916 = PLANE ( 'NONE',  #105717 ) ;
#33917 = ORIENTED_EDGE ( 'NONE', *, *, #54022, .F. ) ;
#33918 =( BOUNDED_CURVE ( )  B_SPLINE_CURVE ( 2, ( #9257, #64400, #108575, #41949, #118771, #8538, #97744, #87583, #86164, #30343, #19466, #96985, #141235 ),
 .UNSPECIFIED., .F., .F. ) 
 B_SPLINE_CURVE_WITH_KNOTS ( ( 3, 2, 2, 2, 2, 2, 3 ),
 ( 0.3166666666666666519, 0.3194444444444444198, 0.3222222222222222432, 0.3250000000000000111, 0.3277777777777777790, 0.3305555555555555469, 0.3333333333333333148 ),
 .UNSPECIFIED. ) 
 CURVE ( )  GEOMETRIC_REPRESENTATION_ITEM ( )  RATIONAL_B_SPLINE_CURVE ( ( 1.000000000000000000, 0.9659258262890683122, 1.000000000000000000, 0.9659258262890683122, 1.000000000000000000, 0.9659258262890683122, 1.000000000000000000, 0.9659258262890683122, 1.000000000000000000, 0.9659258262890683122, 1.000000000000000000, 0.9659258262890683122, 1.000000000000000000 ) ) 
 REPRESENTATION_ITEM ( '' )  );
#33919 = ORIENTED_EDGE ( 'NONE', *, *, #39825, .T. ) ;
#33920 = CARTESIAN_POINT ( 'NONE',  ( 0.000000000000000000, 0.000000000000000000, 5.000000000000000000 ) ) ;
#33921 = VERTEX_POINT ( 'NONE', #85297 ) ;
#33922 = AXIS2_PLACEMENT_3D ( 'NONE', #57716, #134562, #91737 ) ;
#33923 = CARTESIAN_POINT ( 'NONE',  ( 94.50043019189810423, -3.055000000000002380, 5.291415217122920289 ) ) ;
#33924 = DIRECTION ( 'NONE',  ( -0.6830127018922180770, -0.6830127018922204085, -0.2588190451025213501 ) ) ;
#33925 = CYLINDRICAL_SURFACE ( 'NONE', #62296, 0.5000000000000004441 ) ;
#33926 = CARTESIAN_POINT ( 'NONE',  ( 28.49999999999980815, -17.91344420646039737, 1.358650452708529022 ) ) ;
#33927 = CARTESIAN_POINT ( 'NONE',  ( 125.6094186379952902, -46.07581969935851163, -35.63601533998082260 ) ) ;
#33928 = ORIENTED_EDGE ( 'NONE', *, *, #6137, .T. ) ;
#33929 = CARTESIAN_POINT ( 'NONE',  ( 21.44840764549667611, 2.500000000000003553, 3.061616997868386099E-16 ) ) ;
#33930 = CARTESIAN_POINT ( 'NONE',  ( 29.99999999999978328, -6.033600742197672950, 5.000000000000000000 ) ) ;
#33931 = PLANE ( 'NONE',  #32688 ) ;
#33932 = EDGE_CURVE ( 'NONE', #60350, #133314, #114204, .T. ) ;
#33933 = VECTOR ( 'NONE', #130241, 1000.000000000000227 ) ;
#33935 = ADVANCED_FACE ( 'NONE', ( #88920 ), #14175, .T. ) ;
#33934 = LINE ( 'NONE', #13564, #91090 ) ;
#33937 = ORIENTED_EDGE ( 'NONE', *, *, #64393, .F. ) ;
#33936 = LINE ( 'NONE', #89040, #56814 ) ;
#33938 = DIRECTION ( 'NONE',  ( 0.000000000000000000, -1.000000000000000000, 0.000000000000000000 ) ) ;
#33939 = CARTESIAN_POINT ( 'NONE',  ( 21.29974487139158512, -27.71228299555221142, 4.000000000000000000 ) ) ;
#33940 = DIRECTION ( 'NONE',  ( 0.7071067811865486830, -0.7071067811865464625, -0.000000000000000000 ) ) ;
#33941 = FACE_OUTER_BOUND ( 'NONE', #66713, .T. ) ;
#33942 = VECTOR ( 'NONE', #14331, 1000.000000000000000 ) ;
#33943 = DIRECTION ( 'NONE',  ( -0.7071067811865486830, -0.7071067811865464625, 0.000000000000000000 ) ) ;
#33944 = VECTOR ( 'NONE', #76401, 1000.000000000000000 ) ;
#33945 = VERTEX_POINT ( 'NONE', #14889 ) ;
#33946 = EDGE_CURVE ( 'NONE', #46830, #48007, #57010, .T. ) ;
#33947 = ORIENTED_EDGE ( 'NONE', *, *, #130170, .T. ) ;
#33948 = EDGE_LOOP ( 'NONE', ( #71376, #118201, #61395, #137816, #10196, #100838 ) ) ;
#33949 = AXIS2_PLACEMENT_3D ( 'NONE', #101506, #2159, #34132 ) ;
#33950 = CARTESIAN_POINT ( 'NONE',  ( 89.54209685856477563, 5.291415217122923842, -3.054999999999996163 ) ) ;
#33951 = EDGE_LOOP ( 'NONE', ( #660, #72896, #102332, #61489 ) ) ;
#33952 = FACE_OUTER_BOUND ( 'NONE', #19365, .T. ) ;
#33953 = CARTESIAN_POINT ( 'NONE',  ( 18.32816939922340183, 11.25929247661560595, 4.000000000000000000 ) ) ;
#33954 = DIRECTION ( 'NONE',  ( -0.000000000000000000, -1.000000000000000000, -0.000000000000000000 ) ) ;
#33955 = FACE_OUTER_BOUND ( 'NONE', #73010, .T. ) ;
#33956 = ORIENTED_EDGE ( 'NONE', *, *, #95935, .F. ) ;
#33957 = LINE ( 'NONE', #77474, #395 ) ;
#33959 = EDGE_CURVE ( 'NONE', #71690, #63474, #135282, .T. ) ;
#33958 = CARTESIAN_POINT ( 'NONE',  ( 24.61838490601981988, -2.240707523384257716, 13.37739548510233689 ) ) ;
#33960 = CARTESIAN_POINT ( 'NONE',  ( 29.67183060077627133, -3.740707523384236399, 4.000000000000000000 ) ) ;
#33961 = CARTESIAN_POINT ( 'NONE',  ( 89.01626352523143737, -4.472830434245839371, 4.472830434245839371 ) ) ;
#33962 = EDGE_CURVE ( 'NONE', #81346, #10533, #18355, .T. ) ;
#33963 = ORIENTED_EDGE ( 'NONE', *, *, #2838, .T. ) ;
#33964 = CARTESIAN_POINT ( 'NONE',  ( 5.999999999999974243, 17.58746187583906817, 4.000000000000000000 ) ) ;
#33965 = CARTESIAN_POINT ( 'NONE',  ( 9.994118527364397764, 4.584330080086930965E-16, 0.000000000000000000 ) ) ;
#33966 = VERTEX_POINT ( 'NONE', #36639 ) ;
#33967 = ORIENTED_EDGE ( 'NONE', *, *, #55450, .T. ) ;
#33968 = CARTESIAN_POINT ( 'NONE',  ( -0.005480084712502889671, 28.92564299267938210, 4.000000000000000000 ) ) ;
#33969 = EDGE_CURVE ( 'NONE', #96308, #79314, #113479, .T. ) ;
#33970 = CARTESIAN_POINT ( 'NONE',  ( 0.000000000000000000, -2.375000000000000000, -4.320000000000002061 ) ) ;
#33971 = DIRECTION ( 'NONE',  ( 0.7071067811865486830, -0.7071067811865464625, -0.000000000000000000 ) ) ;
#33972 = CARTESIAN_POINT ( 'NONE',  ( 1.190181675744472756, -18.74070752338409562, 7.910009926591503593 ) ) ;
#33973 = DIRECTION ( 'NONE',  ( 0.7071067811865487940, 0.7071067811865463515, 0.000000000000000000 ) ) ;
#33974 = CARTESIAN_POINT ( 'NONE',  ( 12.19999999999999574, -59.76999999999998892, -39.50000000000000000 ) ) ;
#33975 = ORIENTED_EDGE ( 'NONE', *, *, #66068, .T. ) ;
#33976 = VERTEX_POINT ( 'NONE', #70042 ) ;
#33977 = CARTESIAN_POINT ( 'NONE',  ( 12.19999999999999574, -21.76999999999999247, 0.000000000000000000 ) ) ;
#33978 = EDGE_LOOP ( 'NONE', ( #143441, #95928, #12136, #22198 ) ) ;
#33979 = EDGE_LOOP ( 'NONE', ( #91382, #58329, #92180, #1827 ) ) ;
#33980 = VECTOR ( 'NONE', #39288, 999.9999999999998863 ) ;
#33981 = DIRECTION ( 'NONE',  ( -0.6830127018922181881, 0.6830127018922202975, -0.2588190451025214056 ) ) ;
#33982 = ORIENTED_EDGE ( 'NONE', *, *, #55937, .T. ) ;
#33983 = FACE_OUTER_BOUND ( 'NONE', #126204, .T. ) ;
#33984 = LINE ( 'NONE', #102813, #21668 ) ;
#33985 = CARTESIAN_POINT ( 'NONE',  ( -9.489213562373095101, -27.52281430457062328, 5.000000000000000000 ) ) ;
#33986 = VECTOR ( 'NONE', #19085, 999.9999999999998863 ) ;
#33987 = DIRECTION ( 'NONE',  ( 1.000000000000000000, -0.000000000000000000, -0.000000000000000000 ) ) ;
#33988 = CARTESIAN_POINT ( 'NONE',  ( 12.61838490601988383, -2.240707523384260824, 13.37739548510236531 ) ) ;
#33989 = EDGE_LOOP ( 'NONE', ( #50505, #39261, #70062, #74442 ) ) ;
#33991 = VERTEX_POINT ( 'NONE', #112780 ) ;
#33990 = VECTOR ( 'NONE', #142735, 1000.000000000000000 ) ;
#33992 = DIRECTION ( 'NONE',  ( 0.000000000000000000, -1.000000000000000000, 0.000000000000000000 ) ) ;
#33993 = ORIENTED_EDGE ( 'NONE', *, *, #12597, .T. ) ;
#33994 = DIRECTION ( 'NONE',  ( -0.6830127018922181881, 0.6830127018922202975, -0.2588190451025214056 ) ) ;
#33996 = ORIENTED_EDGE ( 'NONE', *, *, #30079, .T. ) ;
#33995 = EDGE_CURVE ( 'NONE', #37390, #34938, #102642, .T. ) ;
#33997 = LINE ( 'NONE', #23070, #69021 ) ;
#33998 = ORIENTED_EDGE ( 'NONE', *, *, #43951, .T. ) ;
#33999 = ORIENTED_EDGE ( 'NONE', *, *, #107848, .F. ) ;
#34000 = ORIENTED_EDGE ( 'NONE', *, *, #52449, .F. ) ;
#34001 = EDGE_CURVE ( 'NONE', #1472, #19682, #46878, .T. ) ;
#34002 = VECTOR ( 'NONE', #62537, 999.9999999999998863 ) ;
#34003 = EDGE_CURVE ( 'NONE', #16702, #81122, #58464, .T. ) ;
#34004 = EDGE_CURVE ( 'NONE', #95435, #82553, #38571, .T. ) ;
#34005 = LINE ( 'NONE', #78226, #104376 ) ;
#34006 = DIRECTION ( 'NONE',  ( 1.000000000000000000, 0.000000000000000000, 0.000000000000000000 ) ) ;
#34008 = EDGE_CURVE ( 'NONE', #8278, #121029, #2568, .T. ) ;
#34007 = LINE ( 'NONE', #122411, #51849 ) ;
#34009 = AXIS2_PLACEMENT_3D ( 'NONE', #7552, #109738, #108270 ) ;
#34010 = CARTESIAN_POINT ( 'NONE',  ( 117.5420968585647756, 5.291415217122923842, -3.054999999999996163 ) ) ;
#34011 = PLANE ( 'NONE',  #123829 ) ;
#34012 = PRODUCT_DEFINITION_SHAPE ( 'NONE', 'NONE',  #22636 ) ;
#34013 = EDGE_CURVE ( 'NONE', #133133, #80135, #68698, .T. ) ;
#34015 = VECTOR ( 'NONE', #98783, 999.9999999999998863 ) ;
#34014 = CARTESIAN_POINT ( 'NONE',  ( -28.28119340046980668, 22.22500000000000142, 2.482413320905432208 ) ) ;
#34016 = FACE_OUTER_BOUND ( 'NONE', #46656, .T. ) ;
#34017 = EDGE_CURVE ( 'NONE', #79053, #137006, #52678, .T. ) ;
#34018 = LINE ( 'NONE', #131893, #47021 ) ;
#34019 = DIRECTION ( 'NONE',  ( -0.7071067811865486830, 0.7071067811865464625, 0.000000000000000000 ) ) ;
#34020 = EDGE_CURVE ( 'NONE', #112772, #67004, #24684, .T. ) ;
#34021 = ORIENTED_EDGE ( 'NONE', *, *, #70429, .F. ) ;
#34022 = DIRECTION ( 'NONE',  ( 0.7071067811865487940, 0.7071067811865463515, -0.000000000000000000 ) ) ;
#34023 = CARTESIAN_POINT ( 'NONE',  ( 34.47516574401890921, 1.490517612115608737, 4.998110765256834398 ) ) ;
#34024 = LINE ( 'NONE', #10790, #37935 ) ;
#34025 = ORIENTED_EDGE ( 'NONE', *, *, #114167, .T. ) ;
#34026 = EDGE_LOOP ( 'NONE', ( #40884, #54307, #99274, #34893 ) ) ;
#34027 = EDGE_LOOP ( 'NONE', ( #140288, #65847, #132623, #79089 ) ) ;
#34028 = LINE ( 'NONE', #88411, #72699 ) ;
#34029 = ORIENTED_EDGE ( 'NONE', *, *, #53996, .F. ) ;
#34030 = ORIENTED_EDGE ( 'NONE', *, *, #95843, .F. ) ;
#34031 = DIRECTION ( 'NONE',  ( 4.681814790819592407E-17, 0.3543493200069153248, 0.9351131265310292928 ) ) ;
#34032 = DIRECTION ( 'NONE',  ( 0.7071067811865487940, -0.7071067811865463515, 0.000000000000000000 ) ) ;
#34033 = ADVANCED_FACE ( 'NONE', ( #67903 ), #112088, .F. ) ;
#34034 = VECTOR ( 'NONE', #23417, 1000.000000000000000 ) ;
#34035 = CARTESIAN_POINT ( 'NONE',  ( -0.4892135623730947680, -27.52281430457055578, 5.000000000000000000 ) ) ;
#34036 = CARTESIAN_POINT ( 'NONE',  ( -39.48921356237310221, -27.52281430457082934, 5.000000000000000000 ) ) ;
#34037 = VERTEX_POINT ( 'NONE', #128658 ) ;
#34038 = CARTESIAN_POINT ( 'NONE',  ( 19.04500000000000881, 3.130000000000007887, -22.35000000000000142 ) ) ;
#34039 = ORIENTED_EDGE ( 'NONE', *, *, #120554, .T. ) ;
#34040 = EDGE_CURVE ( 'NONE', #23445, #88587, #15563, .T. ) ;
#34042 = LINE ( 'NONE', #2807, #139472 ) ;
#34041 = VECTOR ( 'NONE', #116684, 1000.000000000000000 ) ;
#34043 = AXIS2_PLACEMENT_3D ( 'NONE', #93288, #103426, #28038 ) ;
#34044 = CARTESIAN_POINT ( 'NONE',  ( 19.02540314143521982, 2.126176841940962348, 7.934999999999989839 ) ) ;
#34045 = ORIENTED_EDGE ( 'NONE', *, *, #57904, .F. ) ;
#34046 = CARTESIAN_POINT ( 'NONE',  ( 82.59959685856478018, -6.109999999999998543, -1.637169565754160727 ) ) ;
#34047 = CARTESIAN_POINT ( 'NONE',  ( 6.181419415492839242, -9.395137122893222781, 1.432941346517488723 ) ) ;
#34048 = DIRECTION ( 'NONE',  ( 0.6830127018922181881, 0.6830127018922202975, -0.2588190451025214056 ) ) ;
#34049 = ORIENTED_EDGE ( 'NONE', *, *, #137897, .T. ) ;
#34050 = VECTOR ( 'NONE', #100621, 999.9999999999998863 ) ;
#34051 = ORIENTED_EDGE ( 'NONE', *, *, #107751, .F. ) ;
#34052 = ORIENTED_EDGE ( 'NONE', *, *, #6967, .F. ) ;
#34053 = DIRECTION ( 'NONE',  ( -0.000000000000000000, 0.3543493200069153248, 0.9351131265310292928 ) ) ;
#34054 = DIRECTION ( 'NONE',  ( -0.6830127018922180770, -0.6830127018922204085, -0.2588190451025213501 ) ) ;
#34055 = DIRECTION ( 'NONE',  ( 0.000000000000000000, -1.000000000000000000, 0.000000000000000000 ) ) ;
#34056 = AXIS2_PLACEMENT_3D ( 'NONE', #118977, #8736, #40035 ) ;
#34057 = LINE ( 'NONE', #133366, #19541 ) ;
#34058 = DIRECTION ( 'NONE',  ( 0.7071067811865486830, -0.7071067811865464625, -0.000000000000000000 ) ) ;
#34059 = ORIENTED_EDGE ( 'NONE', *, *, #55998, .F. ) ;
#34060 = LINE ( 'NONE', #58709, #27210 ) ;
#34061 = DIRECTION ( 'NONE',  ( -0.3543493200069162685, -0.000000000000000000, -0.9351131265310288487 ) ) ;
#34062 = LINE ( 'NONE', #110154, #55814 ) ;
#34063 = EDGE_CURVE ( 'NONE', #52412, #98565, #126496, .T. ) ;
#34064 = EDGE_LOOP ( 'NONE', ( #13898, #55584, #130258, #11617 ) ) ;
#34065 = LINE ( 'NONE', #78278, #62861 ) ;
#34066 = FACE_OUTER_BOUND ( 'NONE', #48694, .T. ) ;
#34067 = EDGE_LOOP ( 'NONE', ( #74543, #33963, #6957, #32531 ) ) ;
#34068 = EDGE_CURVE ( 'NONE', #33303, #40492, #38799, .T. ) ;
#34070 = ORIENTED_EDGE ( 'NONE', *, *, #49723, .F. ) ;
#34069 = CARTESIAN_POINT ( 'NONE',  ( -19.49999999999985434, 13.46639925780212366, 5.000000000000000000 ) ) ;
#34071 = ORIENTED_EDGE ( 'NONE', *, *, #114794, .F. ) ;
#34072 = DIRECTION ( 'NONE',  ( 0.6830127018922181881, 0.6830127018922202975, -0.2588190451025214056 ) ) ;
#34074 = AXIS2_PLACEMENT_3D ( 'NONE', #122433, #99992, #26000 ) ;
#34073 = DIRECTION ( 'NONE',  ( -0.7071067811865486830, -0.7071067811865464625, 0.000000000000000000 ) ) ;
#34075 = ORIENTED_EDGE ( 'NONE', *, *, #63758, .F. ) ;
#34076 = CARTESIAN_POINT ( 'NONE',  ( 34.92499999999998295, -17.14387692260740792, 4.000000000000000000 ) ) ;
#34077 = ADVANCED_FACE ( 'NONE', ( #81611 ), #127967, .T. ) ;
#34078 = PLANE ( 'NONE',  #3453 ) ;
#34079 = AXIS2_PLACEMENT_3D ( 'NONE', #72723, #126325, #127026 ) ;
#34080 = CARTESIAN_POINT ( 'NONE',  ( -10.17183060077640278, 15.75929247661555976, 4.000000000000000000 ) ) ;
#34081 =( BOUNDED_CURVE ( )  B_SPLINE_CURVE ( 3, ( #120906, #99131, #68018, #143374 ),
 .UNSPECIFIED., .F., .T. ) 
 B_SPLINE_CURVE_WITH_KNOTS ( ( 4, 4 ),
 ( 5.106027341939277875, 6.645403452391244414 ),
 .UNSPECIFIED. ) 
 CURVE ( )  GEOMETRIC_REPRESENTATION_ITEM ( )  RATIONAL_B_SPLINE_CURVE ( ( 1.000000000000000000, 0.8120851936182275077, 0.8120851936182275077, 1.000000000000000000 ) ) 
 REPRESENTATION_ITEM ( '' )  );
#34082 = DIRECTION ( 'NONE',  ( -0.000000000000000000, 0.000000000000000000, 1.000000000000000000 ) ) ;
#34083 = DIRECTION ( 'NONE',  ( -0.3543493200069162685, -0.000000000000000000, -0.9351131265310288487 ) ) ;
#34084 = EDGE_CURVE ( 'NONE', #66493, #47010, #6115, .T. ) ;
#34085 = CARTESIAN_POINT ( 'NONE',  ( -22.49999999999984368, -20.56887692260760048, 4.000000000000000000 ) ) ;
#34086 = CARTESIAN_POINT ( 'NONE',  ( 3.328169399223507074, -6.740707523384214639, 4.000000000000000000 ) ) ;
#34087 = DIRECTION ( 'NONE',  ( -0.7071067811865486830, -0.7071067811865464625, 0.000000000000000000 ) ) ;
#34088 = CARTESIAN_POINT ( 'NONE',  ( 17.33290314143522082, -3.967499999999994476, 6.871911579029513106 ) ) ;
#34090 = VECTOR ( 'NONE', #24480, 1000.000000000000000 ) ;
#34089 = CARTESIAN_POINT ( 'NONE',  ( 1.437069808101886004, 2.126176841940952134, -7.934999999999992504 ) ) ;
#34091 = FACE_OUTER_BOUND ( 'NONE', #81129, .T. ) ;
#34092 = DIRECTION ( 'NONE',  ( -0.000000000000000000, 0.000000000000000000, 1.000000000000000000 ) ) ;
#34093 = FACE_OUTER_BOUND ( 'NONE', #7563, .T. ) ;
#34094 = VERTEX_POINT ( 'NONE', #61314 ) ;
#34095 = ORIENTED_EDGE ( 'NONE', *, *, #142052, .T. ) ;
#34096 = CARTESIAN_POINT ( 'NONE',  ( 103.6666666666666714, 6.884901960086285300, 3.975000000000003642 ) ) ;
#34097 = ORIENTED_EDGE ( 'NONE', *, *, #9186, .T. ) ;
#34098 = VERTEX_POINT ( 'NONE', #105452 ) ;
#34099 = EDGE_CURVE ( 'NONE', #87121, #98769, #37374, .T. ) ;
#34100 = VERTEX_POINT ( 'NONE', #60585 ) ;
#34101 = AXIS2_PLACEMENT_3D ( 'NONE', #99308, #121782, #135554 ) ;
#34102 = LINE ( 'NONE', #47164, #24544 ) ;
#34103 = CARTESIAN_POINT ( 'NONE',  ( 39.48921356237310221, -27.52281430457082934, 5.000000000000000000 ) ) ;
#34104 = EDGE_LOOP ( 'NONE', ( #31795, #62496, #107892, #61223 ) ) ;
#34105 = LINE ( 'NONE', #135558, #62514 ) ;
#34106 = CARTESIAN_POINT ( 'NONE',  ( 9.707106781186476852, -9.740707523384187994, 5.000000000000000000 ) ) ;
#34107 = CARTESIAN_POINT ( 'NONE',  ( -22.37177410554622980, -1.784312229707115893, 4.000000000000000000 ) ) ;
#34108 = EDGE_CURVE ( 'NONE', #108030, #113572, #28651, .T. ) ;
#34109 = ORIENTED_EDGE ( 'NONE', *, *, #51739, .T. ) ;
#34110 = CARTESIAN_POINT ( 'NONE',  ( 127.9537635252314658, -6.109999999999998543, -3.741295971395162543E-16 ) ) ;
#34111 = DIRECTION ( 'NONE',  ( 0.000000000000000000, -1.000000000000000000, 0.000000000000000000 ) ) ;
#34112 = CARTESIAN_POINT ( 'NONE',  ( 34.49999999999975131, 22.21934299833216642, 4.348028800457638177 ) ) ;
#34113 = DIRECTION ( 'NONE',  ( 0.000000000000000000, -1.000000000000000000, -1.301042606982605074E-16 ) ) ;
#34114 = DIRECTION ( 'NONE',  ( 0.7071067811865487940, 0.7071067811865463515, 0.000000000000000000 ) ) ;
#34115 = CARTESIAN_POINT ( 'NONE',  ( 72.48921356237309510, -27.52281430457106026, 5.000000000000000000 ) ) ;
#34116 = CARTESIAN_POINT ( 'NONE',  ( 27.99999999999996803, -49.14999999999999147, 53.92499999999996874 ) ) ;
#34117 = ORIENTED_EDGE ( 'NONE', *, *, #16711, .T. ) ;
#34118 = ORIENTED_EDGE ( 'NONE', *, *, #7277, .T. ) ;
#34119 = CARTESIAN_POINT ( 'NONE',  ( 116.8129301918981184, -1.637169565754159617, -6.110000000000001208 ) ) ;
#34120 = VECTOR ( 'NONE', #132958, 1000.000000000000000 ) ;
#34121 = ORIENTED_EDGE ( 'NONE', *, *, #104680, .F. ) ;
#34122 = ADVANCED_FACE ( 'NONE', ( #36363 ), #45827, .F. ) ;
#34123 = LINE ( 'NONE', #45034, #140442 ) ;
#34124 = DIRECTION ( 'NONE',  ( -0.7071067811865486830, -0.7071067811865464625, 0.000000000000000000 ) ) ;
#34125 = CARTESIAN_POINT ( 'NONE',  ( 8.000000000000007105, 0.000000000000000000, 1.142820323027522456 ) ) ;
#34126 = LINE ( 'NONE', #121109, #78938 ) ;
#34127 = CARTESIAN_POINT ( 'NONE',  ( 111.6204301918981088, 3.055000000000001936, -5.291415217122916737 ) ) ;
#34128 = ADVANCED_FACE ( 'NONE', ( #67587 ), #90758, .T. ) ;
#34129 = ORIENTED_EDGE ( 'NONE', *, *, #97066, .F. ) ;
#34130 = EDGE_LOOP ( 'NONE', ( #100489, #52336, #115255 ) ) ;
#34131 = CARTESIAN_POINT ( 'NONE',  ( 36.65494483745359844, 5.259292476615669010, 12.77922209995902314 ) ) ;
#34132 = DIRECTION ( 'NONE',  ( 1.000000000000000000, 0.000000000000000000, 0.000000000000000000 ) ) ;
#34133 = VERTEX_POINT ( 'NONE', #133535 ) ;
#34134 = ORIENTED_EDGE ( 'NONE', *, *, #3701, .F. ) ;
#34135 = AXIS2_PLACEMENT_3D ( 'NONE', #28964, #62324, #60927 ) ;
#34136 = CARTESIAN_POINT ( 'NONE',  ( 40.54209685856477563, 5.291415217122923842, -3.054999999999996163 ) ) ;
#34137 = EDGE_LOOP ( 'NONE', ( #97362, #12326, #124370, #70797 ) ) ;
#34138 = CYLINDRICAL_SURFACE ( 'NONE', #95444, 0.5000000000000004441 ) ;
#34139 = ADVANCED_FACE ( 'NONE', ( #13855 ), #124785, .T. ) ;
#34140 = LINE ( 'NONE', #49130, #117299 ) ;
#34141 = DIRECTION ( 'NONE',  ( -0.3543493200069162685, -0.000000000000000000, -0.9351131265310288487 ) ) ;
#34142 = AXIS2_PLACEMENT_3D ( 'NONE', #91717, #100472, #35232 ) ;
#34143 = VECTOR ( 'NONE', #132243, 1000.000000000000000 ) ;
#34144 = AXIS2_PLACEMENT_3D ( 'NONE', #21806, #66053, #110216 ) ;
#34145 = CARTESIAN_POINT ( 'NONE',  ( 28.93293019189811943, 1.637169565754156508, 6.110000000000000320 ) ) ;
#34146 = VERTEX_POINT ( 'NONE', #66848 ) ;
#34147 = DIRECTION ( 'NONE',  ( 0.7071067811865487940, 0.7071067811865463515, 0.000000000000000000 ) ) ;
#34148 = ORIENTED_EDGE ( 'NONE', *, *, #108715, .T. ) ;
#34149 = ORIENTED_EDGE ( 'NONE', *, *, #124012, .F. ) ;
#34150 = CIRCLE ( 'NONE', #73474, 2.500000000000000888 ) ;
#34151 = ORIENTED_EDGE ( 'NONE', *, *, #29446, .F. ) ;
#34152 = DIRECTION ( 'NONE',  ( -0.000000000000000000, -0.000000000000000000, 1.000000000000000000 ) ) ;
#34153 = DIRECTION ( 'NONE',  ( -0.6830127018922181881, 0.6830127018922202975, -0.2588190451025214056 ) ) ;
#34154 = ORIENTED_EDGE ( 'NONE', *, *, #32298, .F. ) ;
#34155 = FACE_OUTER_BOUND ( 'NONE', #12538, .T. ) ;
#34156 = CARTESIAN_POINT ( 'NONE',  ( -34.92500000000001137, 3.662461875838966208, 4.000000000000000000 ) ) ;
#34157 = DIRECTION ( 'NONE',  ( -0.000000000000000000, 0.000000000000000000, 1.000000000000000000 ) ) ;
#34158 = DIRECTION ( 'NONE',  ( 0.7071067811865487940, -0.7071067811865463515, 0.000000000000000000 ) ) ;
#34159 = FACE_BOUND ( 'NONE', #139706, .T. ) ;
#34160 = ORIENTED_EDGE ( 'NONE', *, *, #38752, .F. ) ;
#34161 = DIRECTION ( 'NONE',  ( -0.7071067811865486830, 0.7071067811865464625, 0.000000000000000000 ) ) ;
#34162 = CARTESIAN_POINT ( 'NONE',  ( -16.63753812416086930, 22.22500000000000142, 4.000000000000000000 ) ) ;
#34163 = DIRECTION ( 'NONE',  ( 0.6830127018922181881, 0.6830127018922202975, -0.2588190451025214056 ) ) ;
#34164 = DIRECTION ( 'NONE',  ( -0.7071067811865487940, 0.7071067811865463515, 0.000000000000000000 ) ) ;
#34165 = EDGE_LOOP ( 'NONE', ( #32941, #60812, #100450, #31151 ) ) ;
#34166 = FACE_OUTER_BOUND ( 'NONE', #63677, .T. ) ;
#34167 = EDGE_LOOP ( 'NONE', ( #125558, #66121, #63177, #40360 ) ) ;
#34168 = AXIS2_PLACEMENT_3D ( 'NONE', #32232, #21353, #121367 ) ;
#34169 = ORIENTED_EDGE ( 'NONE', *, *, #1508, .T. ) ;
#34170 = ORIENTED_EDGE ( 'NONE', *, *, #20399, .F. ) ;
#34171 = EDGE_CURVE ( 'NONE', #771, #123496, #12446, .T. ) ;
#34172 = CARTESIAN_POINT ( 'NONE',  ( 43.07876352523144448, -7.482591942790325086E-16, 6.109999999999998543 ) ) ;
#34173 = AXIS2_PLACEMENT_3D ( 'NONE', #17416, #37034, #105146 ) ;
#34174 = VERTEX_POINT ( 'NONE', #37059 ) ;
#34175 = LINE ( 'NONE', #14553, #129735 ) ;
#34176 = EDGE_CURVE ( 'NONE', #110282, #140231, #111779, .T. ) ;
#34177 =( NAMED_UNIT ( * ) PLANE_ANGLE_UNIT ( ) SI_UNIT ( $, .RADIAN. ) );
#34178 = VERTEX_POINT ( 'NONE', #34946 ) ;
#34179 = ADVANCED_FACE ( 'NONE', ( #56728 ), #46570, .F. ) ;
#34180 = DIRECTION ( 'NONE',  ( 0.7071067811865487940, 0.7071067811865463515, 0.000000000000000000 ) ) ;
#34181 = EDGE_CURVE ( 'NONE', #123762, #2143, #89310, .T. ) ;
#34182 = CARTESIAN_POINT ( 'NONE',  ( -18.48921356237309510, -27.52281430457068367, 5.000000000000000000 ) ) ;
#34183 = DIRECTION ( 'NONE',  ( -0.7071067811865486830, -0.7071067811865464625, 0.000000000000000000 ) ) ;
#34184 = DIRECTION ( 'NONE',  ( 0.000000000000000000, 0.000000000000000000, 1.000000000000000000 ) ) ;
#34185 = PLANE ( 'NONE',  #10060 ) ;
#34186 = ORIENTED_EDGE ( 'NONE', *, *, #63618, .T. ) ;
#34187 = VERTEX_POINT ( 'NONE', #90002 ) ;
#34188 = EDGE_LOOP ( 'NONE', ( #101326, #74284, #46371, #97469 ) ) ;
#34189 = ORIENTED_EDGE ( 'NONE', *, *, #131576, .T. ) ;
#34190 = DIRECTION ( 'NONE',  ( 0.6830127018922181881, 0.6830127018922202975, -0.2588190451025214056 ) ) ;
#34191 = CARTESIAN_POINT ( 'NONE',  ( -54.48921356237310221, -27.52281430457093236, 5.000000000000000000 ) ) ;
#34192 = EDGE_LOOP ( 'NONE', ( #43865, #84618, #17716, #45897 ) ) ;
#34193 = ORIENTED_EDGE ( 'NONE', *, *, #25541, .F. ) ;
#34194 = CARTESIAN_POINT ( 'NONE',  ( 166.8266634454907660, 26.96999999999994557, -32.27463857217006904 ) ) ;
#34196 = EDGE_CURVE ( 'NONE', #120984, #27268, #55996, .T. ) ;
#34195 = DIRECTION ( 'NONE',  ( 0.7071067811865487940, 0.7071067811865463515, 0.000000000000000000 ) ) ;
#34197 = EDGE_CURVE ( 'NONE', #62041, #105140, #133229, .T. ) ;
#34198 = LINE ( 'NONE', #34920, #138951 ) ;
#34199 = ORIENTED_EDGE ( 'NONE', *, *, #74245, .F. ) ;
#34200 = CARTESIAN_POINT ( 'NONE',  ( -63.29974487139158867, -27.71228299555250274, 4.000000000000000000 ) ) ;
#34201 = EDGE_CURVE ( 'NONE', #114640, #15762, #24758, .T. ) ;
#34202 = CARTESIAN_POINT ( 'NONE',  ( -34.92500000000001137, -2.038703271653886429, -4.194424194487899271 ) ) ;
#34203 = CARTESIAN_POINT ( 'NONE',  ( 26.46290314143521982, -3.967499999999994476, 6.871911579029513106 ) ) ;
#34204 = DIRECTION ( 'NONE',  ( -0.6830127018922180770, -0.6830127018922204085, -0.2588190451025213501 ) ) ;
#34205 = ORIENTED_EDGE ( 'NONE', *, *, #10281, .F. ) ;
#34206 = CARTESIAN_POINT ( 'NONE',  ( 113.3704301918981230, -3.055000000000001936, 5.291415217122918513 ) ) ;
#34207 = PRESENTATION_LAYER_ASSIGNMENT (  '', '', ( #85107 ) ) ;
#34208 = DIRECTION ( 'NONE',  ( 0.7071067811865487940, 0.7071067811865463515, -0.000000000000000000 ) ) ;
#34209 = DIRECTION ( 'NONE',  ( -1.000000000000000000, -0.000000000000000000, -0.000000000000000000 ) ) ;
#34210 = CARTESIAN_POINT ( 'NONE',  ( 1.171830600776465392, -5.240707523384232402, 4.000000000000000000 ) ) ;
#34211 = EDGE_CURVE ( 'NONE', #74950, #4967, #78439, .T. ) ;
#34213 = VERTEX_POINT ( 'NONE', #113180 ) ;
#34212 = CARTESIAN_POINT ( 'NONE',  ( 0.000000000000000000, -21.72500000000000142, 4.500000000000000888 ) ) ;
#34214 = CARTESIAN_POINT ( 'NONE',  ( -42.48921356237308800, -27.52281430457085065, 5.000000000000000000 ) ) ;
#34215 = ORIENTED_EDGE ( 'NONE', *, *, #93924, .T. ) ;
#34216 = DIRECTION ( 'NONE',  ( -1.000000000000000000, -0.000000000000000000, -0.000000000000000000 ) ) ;
#34217 = FACE_OUTER_BOUND ( 'NONE', #132297, .T. ) ;
#34218 = LINE ( 'NONE', #79906, #75025 ) ;
#34219 = VERTEX_POINT ( 'NONE', #102348 ) ;
#34220 = DIRECTION ( 'NONE',  ( 0.000000000000000000, 0.000000000000000000, 1.000000000000000000 ) ) ;
#34221 = FACE_OUTER_BOUND ( 'NONE', #88914, .T. ) ;
#34222 = ADVANCED_FACE ( 'NONE', ( #47290 ), #50802, .T. ) ;
#34223 = VERTEX_POINT ( 'NONE', #94987 ) ;
#34224 = AXIS2_PLACEMENT_3D ( 'NONE', #45999, #77205, #90928 ) ;
#34225 = CARTESIAN_POINT ( 'NONE',  ( -3.707106781186516375, 8.259292476615639700, 5.000000000000000000 ) ) ;
#34226 = VERTEX_POINT ( 'NONE', #73284 ) ;
#34227 = VECTOR ( 'NONE', #31651, 1000.000000000000000 ) ;
#34228 = DIRECTION ( 'NONE',  ( -0.7071067811865487940, 0.7071067811865463515, 0.000000000000000000 ) ) ;
#34230 = VERTEX_POINT ( 'NONE', #139974 ) ;
#34229 = DIRECTION ( 'NONE',  ( 1.000000000000000000, 1.224606353822377258E-16, 0.000000000000000000 ) ) ;
#34231 = VERTEX_POINT ( 'NONE', #5827 ) ;
#34232 = CARTESIAN_POINT ( 'NONE',  ( 19.28515664589288647, 1.196650378695337302, -30.59010235425025215 ) ) ;
#34233 = CARTESIAN_POINT ( 'NONE',  ( -2.999999999999971578, -19.44781430457064175, 5.000000000000000000 ) ) ;
#34234 = VECTOR ( 'NONE', #135457, 1000.000000000000000 ) ;
#34235 = ORIENTED_EDGE ( 'NONE', *, *, #87199, .T. ) ;
#34236 = VECTOR ( 'NONE', #58091, 1000.000000000000227 ) ;
#34237 = EDGE_CURVE ( 'NONE', #100336, #69474, #49409, .T. ) ;
#34238 = LINE ( 'NONE', #78460, #25121 ) ;
#34239 = DIRECTION ( 'NONE',  ( -0.7071067811865486830, -0.7071067811865464625, 0.000000000000000000 ) ) ;
#34240 = CARTESIAN_POINT ( 'NONE',  ( 19.05000000000000071, 3.174999999999997158, 4.000000000000000000 ) ) ;
#34241 = VERTEX_POINT ( 'NONE', #15273 ) ;
#34242 = LINE ( 'NONE', #1565, #90550 ) ;
#34243 = EDGE_CURVE ( 'NONE', #65901, #99074, #72604, .T. ) ;
#34244 = CARTESIAN_POINT ( 'NONE',  ( -2.994519915287485734, 28.92564299267940342, 4.000000000000000000 ) ) ;
#34245 = PLANE ( 'NONE',  #67894 ) ;
#34246 = DIRECTION ( 'NONE',  ( -0.000000000000000000, -0.3543493200069152693, 0.9351131265310292928 ) ) ;
#34247 = CARTESIAN_POINT ( 'NONE',  ( 29.37043019189811233, -3.055000000000001936, 5.291415217122918513 ) ) ;
#34248 = CARTESIAN_POINT ( 'NONE',  ( -30.00000000000000355, 2.375000000000000000, -4.320000000000002061 ) ) ;
#34249 = EDGE_LOOP ( 'NONE', ( #1863, #28587, #67206, #138658 ) ) ;
#34250 = ORIENTED_EDGE ( 'NONE', *, *, #93760, .F. ) ;
#34251 = ORIENTED_EDGE ( 'NONE', *, *, #30080, .F. ) ;
#34252 = ORIENTED_EDGE ( 'NONE', *, *, #137632, .T. ) ;
#34253 = EDGE_CURVE ( 'NONE', #14203, #45336, #26900, .T. ) ;
#34254 = VERTEX_POINT ( 'NONE', #37804 ) ;
#34255 = CARTESIAN_POINT ( 'NONE',  ( 21.66240673564756491, 2.862726108897619232E-16, -2.337593264352432421 ) ) ;
#34256 = CARTESIAN_POINT ( 'NONE',  ( -24.48921356237309510, -27.52281430457072631, 5.000000000000000000 ) ) ;
#34257 = ORIENTED_EDGE ( 'NONE', *, *, #119030, .T. ) ;
#34258 = DIRECTION ( 'NONE',  ( 0.7071067811865486830, -0.7071067811865464625, -0.000000000000000000 ) ) ;
#34259 = DIRECTION ( 'NONE',  ( 1.000000000000000000, 0.000000000000000000, 0.000000000000000000 ) ) ;
#34260 = LINE ( 'NONE', #45172, #41717 ) ;
#34261 = DIRECTION ( 'NONE',  ( 0.7071067811865487940, -0.7071067811865463515, 0.000000000000000000 ) ) ;
#34262 = CARTESIAN_POINT ( 'NONE',  ( 119.5837635252314470, -6.110000000000001208, -3.741295971395164515E-16 ) ) ;
#34263 = EDGE_CURVE ( 'NONE', #50240, #142853, #82039, .T. ) ;
#34264 = ORIENTED_EDGE ( 'NONE', *, *, #90339, .F. ) ;
#34265 = CARTESIAN_POINT ( 'NONE',  ( 1.042387978378689573, 4.202752102959690472E-16, 0.000000000000000000 ) ) ;
#34266 = CARTESIAN_POINT ( 'NONE',  ( -8.671830600776408104, -18.74070752338409562, 4.000000000000000000 ) ) ;
#34267 = CARTESIAN_POINT ( 'NONE',  ( 31.92500000000001492, -3.269999999999992468, -36.39086428169088094 ) ) ;
#34268 = LINE ( 'NONE', #67643, #20231 ) ;
#34269 = CARTESIAN_POINT ( 'NONE',  ( -57.48921356237308800, -27.52281430457095368, 5.000000000000000000 ) ) ;
#34270 = DIRECTION ( 'NONE',  ( -0.7071067811865486830, 0.7071067811865464625, 0.000000000000000000 ) ) ;
#34271 = DIRECTION ( 'NONE',  ( -1.000000000000000000, -1.224606353822377258E-16, -0.000000000000000000 ) ) ;
#34272 = CARTESIAN_POINT ( 'NONE',  ( 44.70419371712955581, -6.884901960086285300, -3.975000000000000089 ) ) ;
#34273 = LINE ( 'NONE', #122691, #7407 ) ;
#34274 = CARTESIAN_POINT ( 'NONE',  ( 14.20710678118644665, -5.240707523384228850, 5.000000000000000000 ) ) ;
#34275 = VERTEX_POINT ( 'NONE', #105860 ) ;
#34276 = ORIENTED_EDGE ( 'NONE', *, *, #86207, .T. ) ;
#34277 = CARTESIAN_POINT ( 'NONE',  ( 43.58333333333333570, 6.884901960086290629, -3.974999999999994316 ) ) ;
#34278 = CARTESIAN_POINT ( 'NONE',  ( -18.48921356237309510, -27.52281430457068367, 5.000000000000000000 ) ) ;
#34279 = EDGE_CURVE ( 'NONE', #2943, #82308, #117452, .T. ) ;
#34280 = LINE ( 'NONE', #119822, #120186 ) ;
#34281 = EDGE_LOOP ( 'NONE', ( #135909, #30837, #129870, #97019 ) ) ;
#34282 = DIRECTION ( 'NONE',  ( 0.7071067811865486830, 0.7071067811865463515, 0.000000000000000000 ) ) ;
#34283 = LINE ( 'NONE', #78504, #74682 ) ;
#34284 = CARTESIAN_POINT ( 'NONE',  ( 40.97959685856477563, 6.109999999999999432, 1.637169565754164280 ) ) ;
#34285 = EDGE_CURVE ( 'NONE', #4808, #5121, #59559, .T. ) ;
#34286 = VERTEX_POINT ( 'NONE', #95724 ) ;
#34287 = ORIENTED_EDGE ( 'NONE', *, *, #117351, .F. ) ;
#34288 = ORIENTED_EDGE ( 'NONE', *, *, #1120, .T. ) ;
#34289 = CARTESIAN_POINT ( 'NONE',  ( -54.18398860626899705, 28.73617430169825226, 5.000000000000000000 ) ) ;
#34290 = CARTESIAN_POINT ( 'NONE',  ( 0.5752130600809799432, 22.22500000000000142, -8.452357796116274358 ) ) ;
#34291 = FACE_OUTER_BOUND ( 'NONE', #37635, .T. ) ;
#34292 = LINE ( 'NONE', #100965, #92580 ) ;
#34294 = EDGE_CURVE ( 'NONE', #109431, #28308, #17443, .T. ) ;
#34293 = ORIENTED_EDGE ( 'NONE', *, *, #7309, .T. ) ;
#34295 = CARTESIAN_POINT ( 'NONE',  ( -45.18398860626900415, 28.73617430169818832, 5.000000000000000000 ) ) ;
#34296 = VERTEX_POINT ( 'NONE', #138527 ) ;
#34297 = CARTESIAN_POINT ( 'NONE',  ( 39.45419371712956291, 6.884901960086283523, 3.975000000000002753 ) ) ;
#34298 = EDGE_CURVE ( 'NONE', #94899, #53957, #114606, .T. ) ;
#34299 = CARTESIAN_POINT ( 'NONE',  ( 41.99451991528749062, 28.92564299267967343, 4.000000000000000000 ) ) ;
#34300 = DIRECTION ( 'NONE',  ( -0.7071067811865486830, -0.7071067811865464625, -0.000000000000000000 ) ) ;
#34301 = DIRECTION ( 'NONE',  ( -1.000000000000000000, -1.224606353822377258E-16, -0.000000000000000000 ) ) ;
#34302 = DIRECTION ( 'NONE',  ( -0.7071067811865486830, 0.7071067811865464625, 0.000000000000000000 ) ) ;
#34303 = CARTESIAN_POINT ( 'NONE',  ( -9.299744871391588674, -27.71228299555212971, 4.000000000000000000 ) ) ;
#34304 = ORIENTED_EDGE ( 'NONE', *, *, #81017, .T. ) ;
#34305 = AXIS2_PLACEMENT_3D ( 'NONE', #86606, #41644, #51834 ) ;
#34306 = PLANE ( 'NONE',  #138010 ) ;
#34307 = CARTESIAN_POINT ( 'NONE',  ( 62.32876352523145158, 0.000000000000000000, -6.109999999999998543 ) ) ;
#34308 = CARTESIAN_POINT ( 'NONE',  ( -72.48921356237309510, -27.52281430457106026, 5.000000000000000000 ) ) ;
#34309 = LINE ( 'NONE', #65552, #6044 ) ;
#34310 = DIRECTION ( 'NONE',  ( 0.7071067811865487940, -0.7071067811865463515, 0.000000000000000000 ) ) ;
#34311 = ORIENTED_EDGE ( 'NONE', *, *, #111158, .F. ) ;
#34312 = CYLINDRICAL_SURFACE ( 'NONE', #125756, 7.950000000000000178 ) ;
#34313 = ORIENTED_EDGE ( 'NONE', *, *, #10089, .F. ) ;
#34314 = EDGE_CURVE ( 'NONE', #37230, #49472, #116760, .T. ) ;
#34315 = ADVANCED_BREP_SHAPE_REPRESENTATION ( '', ( #45918, #127880 ), #137188 ) ;
#34316 = CARTESIAN_POINT ( 'NONE',  ( -26.99999999999981171, -16.06887692260764666, 4.000000000000000000 ) ) ;
#34317 = ORIENTED_EDGE ( 'NONE', *, *, #41753, .F. ) ;
#34318 = CARTESIAN_POINT ( 'NONE',  ( -35.99451991528749772, 28.92564299267963079, 4.000000000000000000 ) ) ;
#34319 = LINE ( 'NONE', #111135, #20132 ) ;
#34320 = CARTESIAN_POINT ( 'NONE',  ( 18.48921356237309510, -27.52281430457068367, 5.000000000000000000 ) ) ;
#34321 = AXIS2_PLACEMENT_3D ( 'NONE', #80412, #36865, #26011 ) ;
#34322 = CARTESIAN_POINT ( 'NONE',  ( -23.99999999999983302, -18.03360074219755660, 5.000000000000000000 ) ) ;
#34323 = AXIS2_PLACEMENT_3D ( 'NONE', #66966, #2371, #34329 ) ;
#34324 = FACE_BOUND ( 'NONE', #75392, .T. ) ;
#34325 = DIRECTION ( 'NONE',  ( 0.7071067811865487940, -0.7071067811865463515, 0.000000000000000000 ) ) ;
#34326 = DIRECTION ( 'NONE',  ( -0.000000000000000000, -0.3543493200069152693, 0.9351131265310292928 ) ) ;
#34327 = EDGE_CURVE ( 'NONE', #58810, #94676, #137824, .T. ) ;
#34328 = CARTESIAN_POINT ( 'NONE',  ( 14.99999999999989164, -21.41253812416053748, 4.000000000000000000 ) ) ;
#34330 = EDGE_LOOP ( 'NONE', ( #3169, #66886, #126298, #84762 ) ) ;
#34329 = DIRECTION ( 'NONE',  ( 0.000000000000000000, -1.000000000000000000, 0.000000000000000000 ) ) ;
#34331 = AXIS2_PLACEMENT_3D ( 'NONE', #46713, #90895, #124210 ) ;
#34332 = VECTOR ( 'NONE', #25238, 1000.000000000000000 ) ;
#34333 = DIRECTION ( 'NONE',  ( -0.7071067811865486830, 0.7071067811865464625, 0.000000000000000000 ) ) ;
#34334 = ORIENTED_EDGE ( 'NONE', *, *, #106642, .F. ) ;
#34336 = ORIENTED_EDGE ( 'NONE', *, *, #139627, .F. ) ;
#34335 = EDGE_CURVE ( 'NONE', #89571, #41615, #26199, .T. ) ;
#34337 = CARTESIAN_POINT ( 'NONE',  ( 74.28709685856478018, 3.054999999999997495, 5.291415217122919401 ) ) ;
#34338 = ORIENTED_EDGE ( 'NONE', *, *, #89021, .F. ) ;
#34339 = FACE_OUTER_BOUND ( 'NONE', #26228, .T. ) ;
#34340 = EDGE_CURVE ( 'NONE', #112149, #89022, #15982, .T. ) ;
#34341 = ORIENTED_EDGE ( 'NONE', *, *, #135193, .F. ) ;
#34342 = PLANE ( 'NONE',  #19247 ) ;
#34343 = VECTOR ( 'NONE', #46589, 1000.000000000000000 ) ;
#34344 = EDGE_CURVE ( 'NONE', #96477, #127633, #128373, .T. ) ;
#34345 = EDGE_CURVE ( 'NONE', #100536, #96477, #29045, .T. ) ;
#34346 = PLANE ( 'NONE',  #5555 ) ;
#34347 = CARTESIAN_POINT ( 'NONE',  ( -12.69999999999998153, 0.000000000000000000, 0.000000000000000000 ) ) ;
#34348 = DIRECTION ( 'NONE',  ( 0.7071067811865487940, 0.7071067811865463515, 0.000000000000000000 ) ) ;
#34349 = FACE_OUTER_BOUND ( 'NONE', #92097, .T. ) ;
#34351 = CARTESIAN_POINT ( 'NONE',  ( -50.99451991528749062, 28.92564299267973738, 4.000000000000000000 ) ) ;
#34350 = CARTESIAN_POINT ( 'NONE',  ( -65.99451991528749772, 28.92564299267984396, 4.000000000000000000 ) ) ;
#34352 = CYLINDRICAL_SURFACE ( 'NONE', #77064, 2.500000000000000444 ) ;
#34353 = PLANE ( 'NONE',  #55547 ) ;
#34354 = ORIENTED_EDGE ( 'NONE', *, *, #32833, .T. ) ;
#34355 = VECTOR ( 'NONE', #56934, 999.9999999999998863 ) ;
#34356 = ORIENTED_EDGE ( 'NONE', *, *, #127480, .T. ) ;
#34357 = CARTESIAN_POINT ( 'NONE',  ( -28.49999999999980105, -10.04351517176480613, -1.623559851933888964 ) ) ;
#34358 =( BOUNDED_CURVE ( )  B_SPLINE_CURVE ( 3, ( #136275, #16629, #125420, #72502 ),
 .UNSPECIFIED., .F., .T. ) 
 B_SPLINE_CURVE_WITH_KNOTS ( ( 4, 4 ),
 ( 5.005968288816732503, 5.074607125596331869 ),
 .UNSPECIFIED. ) 
 CURVE ( )  GEOMETRIC_REPRESENTATION_ITEM ( )  RATIONAL_B_SPLINE_CURVE ( ( 1.000000000000000000, 0.9996074310407765395, 0.9996074310407765395, 1.000000000000000000 ) ) 
 REPRESENTATION_ITEM ( '' )  );
#34359 = CARTESIAN_POINT ( 'NONE',  ( 69.29974487139159578, -27.71228299555254537, 4.000000000000000000 ) ) ;
#34360 = EDGE_LOOP ( 'NONE', ( #41169, #74798, #78924, #42805 ) ) ;
#34361 = EDGE_LOOP ( 'NONE', ( #18014, #65218, #117805, #121158, #46525, #93190 ) ) ;
#34362 = VECTOR ( 'NONE', #100697, 999.9999999999998863 ) ;
#34363 = ORIENTED_EDGE ( 'NONE', *, *, #109809, .T. ) ;
#34364 = ADVANCED_FACE ( 'NONE', ( #4362 ), #48665, .F. ) ;
#34365 = ADVANCED_FACE ( 'NONE', ( #116034 ), #16736, .F. ) ;
#34366 = LINE ( 'NONE', #79344, #99367 ) ;
#34367 = EDGE_LOOP ( 'NONE', ( #52874, #139272, #74067, #54223 ) ) ;
#34368 = LINE ( 'NONE', #78588, #127298 ) ;
#34369 = EDGE_CURVE ( 'NONE', #142313, #134912, #108703, .T. ) ;
#34370 = CARTESIAN_POINT ( 'NONE',  ( -42.48921356237308800, -27.52281430457085065, 5.000000000000000000 ) ) ;
#34371 = CARTESIAN_POINT ( 'NONE',  ( -0.3704301918981141029, -3.967499999999998028, -6.871911579029511330 ) ) ;
#34372 = CARTESIAN_POINT ( 'NONE',  ( 15.15510207594467218, 3.811689137368155844, -32.44374734479579558 ) ) ;
#34373 = EDGE_LOOP ( 'NONE', ( #21006, #78120, #88383, #14407, #63686 ) ) ;
#34374 = DIRECTION ( 'NONE',  ( 0.000000000000000000, -1.000000000000000000, 0.000000000000000000 ) ) ;
#34375 = DIRECTION ( 'NONE',  ( -0.7071067811865487940, 0.7071067811865463515, -0.000000000000000000 ) ) ;
#34376 = EDGE_CURVE ( 'NONE', #1859, #99111, #32137, .T. ) ;
#34377 = AXIS2_PLACEMENT_3D ( 'NONE', #129016, #73934, #118111 ) ;
#34379 = VERTEX_POINT ( 'NONE', #31199 ) ;
#34378 = CARTESIAN_POINT ( 'NONE',  ( 17.84878961325748037, 4.584330080086930965E-16, 0.000000000000000000 ) ) ;
#34380 = VERTEX_POINT ( 'NONE', #141370 ) ;
#34381 = CARTESIAN_POINT ( 'NONE',  ( 1.499999999999990896, 6.277155672890271099, -3.510561720658945450 ) ) ;
#34382 = CONICAL_SURFACE ( 'NONE', #31995, 2.500000000000000888, 0.9599310885968822538 ) ;
#34383 = CARTESIAN_POINT ( 'NONE',  ( 3.654944837453800943, 5.259292476615669010, 12.77922209995894498 ) ) ;
#34384 = ORIENTED_EDGE ( 'NONE', *, *, #94714, .F. ) ;
#34385 = CARTESIAN_POINT ( 'NONE',  ( -5.999999999999960032, 5.587461875839188075, 4.000000000000000000 ) ) ;
#34386 = ORIENTED_EDGE ( 'NONE', *, *, #76083, .F. ) ;
#34387 = CARTESIAN_POINT ( 'NONE',  ( 18.95159235450331892, 9.902892378096218942E-16, 0.000000000000000000 ) ) ;
#34388 = CARTESIAN_POINT ( 'NONE',  ( 27.54166666666665719, -3.975000000000002753, 6.884901960086286188 ) ) ;
#34389 = LINE ( 'NONE', #88789, #84276 ) ;
#34390 = ADVANCED_FACE ( 'NONE', ( #19588 ), #7981, .F. ) ;
#34391 = DIRECTION ( 'NONE',  ( -1.000000000000000000, -0.000000000000000000, -0.000000000000000000 ) ) ;
#34392 = LINE ( 'NONE', #14774, #70194 ) ;
#34393 = PLANE ( 'NONE',  #88535 ) ;
#34394 = DIRECTION ( 'NONE',  ( 0.3543493200069162685, -0.000000000000000000, -0.9351131265310288487 ) ) ;
#34395 = LINE ( 'NONE', #2446, #92299 ) ;
#34396 = ORIENTED_EDGE ( 'NONE', *, *, #61374, .F. ) ;
#34397 = EDGE_CURVE ( 'NONE', #123427, #36268, #87706, .T. ) ;
#34398 = ORIENTED_EDGE ( 'NONE', *, *, #33067, .F. ) ;
#34399 = ADVANCED_FACE ( 'NONE', ( #63132 ), #130520, .F. ) ;
#34400 = CARTESIAN_POINT ( 'NONE',  ( 57.18398860626899705, 28.73617430169827358, 5.000000000000000000 ) ) ;
#34401 = DIRECTION ( 'NONE',  ( 0.7071067811865486830, -0.7071067811865464625, -0.000000000000000000 ) ) ;
#34402 = EDGE_CURVE ( 'NONE', #46120, #51714, #10828, .T. ) ;
#34403 = SURFACE_STYLE_FILL_AREA ( #100382 ) ;
#34404 = CARTESIAN_POINT ( 'NONE',  ( 65.41252705046289861, -7.949999999999998401, -4.867971026610728450E-16 ) ) ;
#34405 = ORIENTED_EDGE ( 'NONE', *, *, #58246, .T. ) ;
#34406 = DIRECTION ( 'NONE',  ( -0.6830127018922181881, 0.6830127018922202975, -0.2588190451025214056 ) ) ;
#34407 = FACE_OUTER_BOUND ( 'NONE', #143328, .T. ) ;
#34408 = ORIENTED_EDGE ( 'NONE', *, *, #130157, .T. ) ;
#34409 = LINE ( 'NONE', #69192, #113607 ) ;
#34410 = CARTESIAN_POINT ( 'NONE',  ( 7.213219033033542615, 12.75929247661559351, 10.29404684609036913 ) ) ;
#34411 = CARTESIAN_POINT ( 'NONE',  ( 11.99999999999991651, 7.588810512006220144, -3.013526669885254972 ) ) ;
#34412 = CARTESIAN_POINT ( 'NONE',  ( -15.18398860626900237, 28.73617430169797871, 5.000000000000000000 ) ) ;
#34413 = CARTESIAN_POINT ( 'NONE',  ( 52.84959685856479439, 6.109999999999997655, 1.637169565754163836 ) ) ;
#34414 = LINE ( 'NONE', #44625, #113601 ) ;
#34415 = LINE ( 'NONE', #43877, #60368 ) ;
#34416 = VECTOR ( 'NONE', #51528, 999.9999999999998863 ) ;
#34417 = DIRECTION ( 'NONE',  ( 0.3543493200069162685, -0.000000000000000000, -0.9351131265310288487 ) ) ;
#34418 = ORIENTED_EDGE ( 'NONE', *, *, #59614, .F. ) ;
#34419 = CARTESIAN_POINT ( 'NONE',  ( 20.99451991528748707, 28.92564299267952777, 4.000000000000000000 ) ) ;
#34420 = ORIENTED_EDGE ( 'NONE', *, *, #104569, .T. ) ;
#34421 = CARTESIAN_POINT ( 'NONE',  ( -48.48921356237309510, -27.52281430457089328, 5.000000000000000000 ) ) ;
#34422 = STYLED_ITEM ( 'NONE', ( #127390 ), #69272 ) ;
#34423 = VECTOR ( 'NONE', #85922, 1000.000000000000227 ) ;
#34424 = CONICAL_SURFACE ( 'NONE', #8899, 2.500000000000000444, 0.9599310885968830309 ) ;
#34425 = FACE_OUTER_BOUND ( 'NONE', #1623, .T. ) ;
#34426 = CARTESIAN_POINT ( 'NONE',  ( 1.499999999999996225, -10.91253812416064406, 4.000000000000000000 ) ) ;
#34427 = VECTOR ( 'NONE', #31303, 1000.000000000000000 ) ;
#34428 = DIRECTION ( 'NONE',  ( 1.000000000000000000, 0.000000000000000000, 0.000000000000000000 ) ) ;
#34429 = PLANE ( 'NONE',  #12977 ) ;
#34430 = ORIENTED_EDGE ( 'NONE', *, *, #43746, .F. ) ;
#34431 = EDGE_LOOP ( 'NONE', ( #44970, #81356, #51541, #61162 ) ) ;
#34432 = CARTESIAN_POINT ( 'NONE',  ( -27.31657961132772883, -6.740707523384216415, 11.88629033278130542 ) ) ;
#34433 = SURFACE_SIDE_STYLE ('',( #13365 ) ) ;
#34434 = UNCERTAINTY_MEASURE_WITH_UNIT (LENGTH_MEASURE( 1.000000000000000082E-05 ), #86886, 'distance_accuracy_value', 'NONE');
#34435 = VECTOR ( 'NONE', #10955, 1000.000000000000000 ) ;
#34436 = VECTOR ( 'NONE', #27852, 999.9999999999998863 ) ;
#34437 = LINE ( 'NONE', #66367, #1074 ) ;
#34438 = CARTESIAN_POINT ( 'NONE',  ( 15.94163961620377279, -6.094999999999989093, 1.633150327867691542 ) ) ;
#34439 = CARTESIAN_POINT ( 'NONE',  ( 73.43336038379621300, 2.130196079827431532, -7.949999999999997513 ) ) ;
#34440 = CARTESIAN_POINT ( 'NONE',  ( -34.75611968250420603, -10.29434930147582783, 4.955485411084898040 ) ) ;
#34441 = DIRECTION ( 'NONE',  ( 0.7071067811865487940, 0.7071067811865463515, -0.000000000000000000 ) ) ;
#34442 = ORIENTED_EDGE ( 'NONE', *, *, #23993, .F. ) ;
#34443 = CARTESIAN_POINT ( 'NONE',  ( 72.45833333333332860, 3.974999999999997424, 6.884901960086288852 ) ) ;
#34444 = DIRECTION ( 'NONE',  ( 0.6830127018922180770, -0.6830127018922204085, -0.2588190451025214056 ) ) ;
#34445 = DIRECTION ( 'NONE',  ( -0.7071067811865486830, -0.7071067811865464625, 0.000000000000000000 ) ) ;
#34446 = CARTESIAN_POINT ( 'NONE',  ( 24.18398860626899705, 28.73617430169804265, 5.000000000000000000 ) ) ;
#34447 = VECTOR ( 'NONE', #124628, 1000.000000000000000 ) ;
#34448 = VECTOR ( 'NONE', #108222, 1000.000000000000000 ) ;
#34449 = ORIENTED_EDGE ( 'NONE', *, *, #142516, .F. ) ;
#34450 = DIRECTION ( 'NONE',  ( 0.3543493200069162685, -0.000000000000000000, -0.9351131265310288487 ) ) ;
#34451 = VECTOR ( 'NONE', #81714, 1000.000000000000000 ) ;
#34452 = CARTESIAN_POINT ( 'NONE',  ( 0.000000000000000000, 0.000000000000000000, 5.000000000000000000 ) ) ;
#34453 = CARTESIAN_POINT ( 'NONE',  ( 68.39626352523141861, 4.472830434245840259, -4.472830434245839371 ) ) ;
#34455 = ORIENTED_EDGE ( 'NONE', *, *, #97849, .F. ) ;
#34454 = AXIS2_PLACEMENT_3D ( 'NONE', #140001, #5859, #60301 ) ;
#34456 = ORIENTED_EDGE ( 'NONE', *, *, #106436, .T. ) ;
#34457 = AXIS2_PLACEMENT_3D ( 'NONE', #66908, #111088, #11780 ) ;
#34458 = CARTESIAN_POINT ( 'NONE',  ( 32.99999999999977973, 2.587461875839218273, 4.000000000000000000 ) ) ;
#34459 = VECTOR ( 'NONE', #100210, 1000.000000000000227 ) ;
#34460 = DIRECTION ( 'NONE',  ( 0.6830127018922181881, 0.6830127018922202975, -0.2588190451025214056 ) ) ;
#34461 = CARTESIAN_POINT ( 'NONE',  ( 14.99999999999990585, -16.44781430457066662, 5.000000000000000000 ) ) ;
#34462 = VECTOR ( 'NONE', #39606, 1000.000000000000227 ) ;
#34463 = DIRECTION ( 'NONE',  ( 0.3543493200069162685, -0.000000000000000000, -0.9351131265310288487 ) ) ;
#34464 = ADVANCED_FACE ( 'NONE', ( #9389 ), #27552, .T. ) ;
#34465 = CARTESIAN_POINT ( 'NONE',  ( -14.54016161050250844, 18.75929247661552779, 8.305906642995452671 ) ) ;
#34467 = ORIENTED_EDGE ( 'NONE', *, *, #135902, .F. ) ;
#34466 = DIRECTION ( 'NONE',  ( -0.000000000000000000, -0.3543493200069152693, 0.9351131265310292928 ) ) ;
#34468 = EDGE_CURVE ( 'NONE', #87036, #52226, #55090, .T. ) ;
#34469 = FACE_OUTER_BOUND ( 'NONE', #107121, .T. ) ;
#34470 = LINE ( 'NONE', #24303, #82368 ) ;
#34471 = DIRECTION ( 'NONE',  ( 0.000000000000000000, 0.7453559924999330066, 0.6666666666666630769 ) ) ;
#34472 = VECTOR ( 'NONE', #106411, 999.9999999999998863 ) ;
#34473 = DIRECTION ( 'NONE',  ( 0.6830127018922181881, 0.6830127018922202975, -0.2588190451025214056 ) ) ;
#34474 = AXIS2_PLACEMENT_3D ( 'NONE', #91773, #112124, #34554 ) ;
#34475 = ORIENTED_EDGE ( 'NONE', *, *, #64775, .T. ) ;
#34476 = VERTEX_POINT ( 'NONE', #10138 ) ;
#34477 = CARTESIAN_POINT ( 'NONE',  ( 53.95876352523143282, 0.000000000000000000, -6.110000000000001208 ) ) ;
#34478 = ORIENTED_EDGE ( 'NONE', *, *, #99126, .T. ) ;
#34479 = EDGE_CURVE ( 'NONE', #106022, #124937, #97874, .T. ) ;
#34480 = DIRECTION ( 'NONE',  ( -0.6830127018922181881, 0.6830127018922202975, -0.2588190451025214056 ) ) ;
#34481 = CARTESIAN_POINT ( 'NONE',  ( 27.78162688292474769, 21.74787736706806740, 4.999607392498048419 ) ) ;
#34482 = CARTESIAN_POINT ( 'NONE',  ( 1.828169399223519953, -11.24070752338416845, 4.000000000000000000 ) ) ;
#34483 = CARTESIAN_POINT ( 'NONE',  ( 125.4958603837962272, -3.974999999999998312, -6.884901960086286188 ) ) ;
#34484 = ORIENTED_EDGE ( 'NONE', *, *, #60923, .T. ) ;
#34485 = ORIENTED_EDGE ( 'NONE', *, *, #22718, .F. ) ;
#34486 = VECTOR ( 'NONE', #12627, 999.9999999999998863 ) ;
#34487 = CARTESIAN_POINT ( 'NONE',  ( 21.15294044719737698, 3.821174125832445049E-16, 0.000000000000000000 ) ) ;
#34488 = CARTESIAN_POINT ( 'NONE',  ( -17.01299344913721612, -0.9444867979315253459, -36.05398659021086871 ) ) ;
#34489 = EDGE_CURVE ( 'NONE', #6107, #38956, #52219, .T. ) ;
#34490 = ORIENTED_EDGE ( 'NONE', *, *, #105076, .T. ) ;
#34491 = CARTESIAN_POINT ( 'NONE',  ( 30.79289321881325137, -20.24070752338407431, 5.000000000000000000 ) ) ;
#34492 = FACE_OUTER_BOUND ( 'NONE', #132695, .T. ) ;
#34493 = PLANE ( 'NONE',  #65566 ) ;
#34494 = ADVANCED_FACE ( 'NONE', ( #54400 ), #52902, .T. ) ;
#34495 = EDGE_LOOP ( 'NONE', ( #22923, #114917, #25166, #8951 ) ) ;
#34496 = FACE_BOUND ( 'NONE', #46536, .T. ) ;
#34497 = DIRECTION ( 'NONE',  ( 0.7071067811865487940, 0.7071067811865463515, 0.000000000000000000 ) ) ;
#34498 = PLANE ( 'NONE',  #86040 ) ;
#34499 = CARTESIAN_POINT ( 'NONE',  ( 14.51078643762690490, -27.52281430457045275, 5.000000000000000000 ) ) ;
#34500 = FACE_OUTER_BOUND ( 'NONE', #58897, .T. ) ;
#34501 = FACE_OUTER_BOUND ( 'NONE', #105829, .T. ) ;
#34502 = CARTESIAN_POINT ( 'NONE',  ( -78.45649007701574362, -18.96625297709787716, 26.24785786468246229 ) ) ;
#34503 = ORIENTED_EDGE ( 'NONE', *, *, #123118, .T. ) ;
#34504 = ORIENTED_EDGE ( 'NONE', *, *, #141234, .F. ) ;
#34505 = CARTESIAN_POINT ( 'NONE',  ( 104.7662635252314516, 4.472830434245838482, -4.472830434245837594 ) ) ;
#34506 = ORIENTED_EDGE ( 'NONE', *, *, #33758, .T. ) ;
#34507 = ORIENTED_EDGE ( 'NONE', *, *, #42046, .F. ) ;
#34508 = EDGE_CURVE ( 'NONE', #9125, #40590, #119591, .T. ) ;
#34509 = CARTESIAN_POINT ( 'NONE',  ( -14.99451991528749595, 28.92564299267948513, 4.000000000000000000 ) ) ;
#34510 = CARTESIAN_POINT ( 'NONE',  ( 14.86920357848291196, 3.821174125832445049E-16, 0.000000000000000000 ) ) ;
#34511 = EDGE_CURVE ( 'NONE', #4615, #48007, #65992, .T. ) ;
#34512 = EDGE_CURVE ( 'NONE', #139953, #87542, #43834, .T. ) ;
#34513 = LINE ( 'NONE', #122955, #84156 ) ;
#34514 = VERTEX_POINT ( 'NONE', #118159 ) ;
#34515 = CARTESIAN_POINT ( 'NONE',  ( -6.328169399223487090, 14.25929247661557575, 4.000000000000000000 ) ) ;
#34516 = DIRECTION ( 'NONE',  ( 0.6830127018922181881, 0.6830127018922202975, -0.2588190451025214056 ) ) ;
#34517 = DIRECTION ( 'NONE',  ( -0.7071067811865486830, 0.7071067811865464625, 0.000000000000000000 ) ) ;
#34518 = DIRECTION ( 'NONE',  ( 0.000000000000000000, 0.000000000000000000, 1.000000000000000000 ) ) ;
#34519 = CARTESIAN_POINT ( 'NONE',  ( -39.18398860626899705, 28.73617430169814568, 5.000000000000000000 ) ) ;
#34520 = DIRECTION ( 'NONE',  ( 0.000000000000000000, 1.000000000000000000, -0.000000000000000000 ) ) ;
#34521 = VECTOR ( 'NONE', #138624, 1000.000000000000227 ) ;
#34522 = VECTOR ( 'NONE', #18429, 1000.000000000000227 ) ;
#34523 = CIRCLE ( 'NONE', #76232, 2.500000000000000888 ) ;
#34524 = CARTESIAN_POINT ( 'NONE',  ( 0.000000000000000000, 0.000000000000000000, 5.000000000000000000 ) ) ;
#34525 = ORIENTED_EDGE ( 'NONE', *, *, #132716, .T. ) ;
#34526 = EDGE_CURVE ( 'NONE', #45818, #34226, #109456, .T. ) ;
#34527 = CARTESIAN_POINT ( 'NONE',  ( 88.50000000000000000, 0.000000000000000000, -7.950000000000000178 ) ) ;
#34528 = DIRECTION ( 'NONE',  ( 1.000000000000000000, 0.000000000000000000, 0.000000000000000000 ) ) ;
#34529 = AXIS2_PLACEMENT_3D ( 'NONE', #129701, #30409, #130452 ) ;
#34530 = ORIENTED_EDGE ( 'NONE', *, *, #122834, .T. ) ;
#34531 = EDGE_LOOP ( 'NONE', ( #22615, #6234, #63044, #3037 ) ) ;
#34532 = EDGE_CURVE ( 'NONE', #128563, #28263, #99261, .T. ) ;
#34534 = EDGE_LOOP ( 'NONE', ( #33058, #142917, #7618, #134042 ) ) ;
#34533 = ADVANCED_FACE ( 'NONE', ( #29734 ), #73981, .F. ) ;
#34535 = CARTESIAN_POINT ( 'NONE',  ( 58.77126352523141861, 4.472830434245838482, 4.472830434245842035 ) ) ;
#34536 = VERTEX_POINT ( 'NONE', #68838 ) ;
#34537 = VECTOR ( 'NONE', #87729, 1000.000000000000227 ) ;
#34538 =( BOUNDED_CURVE ( )  B_SPLINE_CURVE ( 3, ( #28751, #137505, #29431, #95409 ),
 .UNSPECIFIED., .F., .T. ) 
 B_SPLINE_CURVE_WITH_KNOTS ( ( 4, 4 ),
 ( 4.712388980384696779, 6.283185307179586232 ),
 .UNSPECIFIED. ) 
 CURVE ( )  GEOMETRIC_REPRESENTATION_ITEM ( )  RATIONAL_B_SPLINE_CURVE ( ( 1.000000000000000000, 0.8047378541243667138, 0.8047378541243667138, 1.000000000000000000 ) ) 
 REPRESENTATION_ITEM ( '' )  );
#34539 = CARTESIAN_POINT ( 'NONE',  ( 11.20710678118647508, 0.7592924766157104211, 5.000000000000000000 ) ) ;
#34540 =( BOUNDED_CURVE ( )  B_SPLINE_CURVE ( 3, ( #26892, #60266, #17437, #129772 ),
 .UNSPECIFIED., .F., .F. ) 
 B_SPLINE_CURVE_WITH_KNOTS ( ( 4, 4 ),
 ( 1.901594255663625388, 1.933014472006574280 ),
 .UNSPECIFIED. ) 
 CURVE ( )  GEOMETRIC_REPRESENTATION_ITEM ( )  RATIONAL_B_SPLINE_CURVE ( ( 1.000000000000000000, 0.9999177325257868620, 0.9999177325257868620, 1.000000000000000000 ) ) 
 REPRESENTATION_ITEM ( '' )  );
#34541 = CARTESIAN_POINT ( 'NONE',  ( 4.858306282870439752, -1.633150327867689988, 6.094999999999989981 ) ) ;
#34542 = CARTESIAN_POINT ( 'NONE',  ( 93.77126352523141861, 4.472830434245838482, 4.472830434245842035 ) ) ;
#34543 = LINE ( 'NONE', #135987, #116548 ) ;
#34544 = EDGE_CURVE ( 'NONE', #1349, #105081, #121740, .T. ) ;
#34545 = ORIENTED_EDGE ( 'NONE', *, *, #28598, .T. ) ;
#34546 = ORIENTED_EDGE ( 'NONE', *, *, #79102, .T. ) ;
#34547 = PLANE ( 'NONE',  #46472 ) ;
#34548 = VECTOR ( 'NONE', #60851, 1000.000000000000227 ) ;
#34549 = AXIS2_PLACEMENT_3D ( 'NONE', #11782, #131457, #43028 ) ;
#34550 = EDGE_CURVE ( 'NONE', #113756, #80227, #123909, .T. ) ;
#34551 = CARTESIAN_POINT ( 'NONE',  ( -60.18398860626900415, 28.73617430169829490, 5.000000000000000000 ) ) ;
#34552 = ORIENTED_EDGE ( 'NONE', *, *, #4445, .F. ) ;
#34553 = LINE ( 'NONE', #67939, #141840 ) ;
#34554 = DIRECTION ( 'NONE',  ( -0.7071067811865486830, 0.7071067811865464625, 0.000000000000000000 ) ) ;
#34555 = LINE ( 'NONE', #43293, #42863 ) ;
#34556 = VERTEX_POINT ( 'NONE', #79743 ) ;
#34557 = VECTOR ( 'NONE', #129279, 1000.000000000000000 ) ;
#34558 = CARTESIAN_POINT ( 'NONE',  ( 18.98911971346037930, -22.02621442084248216, 4.990779571109221102 ) ) ;
#34559 = ORIENTED_EDGE ( 'NONE', *, *, #94726, .F. ) ;
#34560 = ORIENTED_EDGE ( 'NONE', *, *, #118806, .T. ) ;
#34561 = ORIENTED_EDGE ( 'NONE', *, *, #75173, .T. ) ;
#34562 = CARTESIAN_POINT ( 'NONE',  ( 39.48921356237310221, -27.52281430457082934, 5.000000000000000000 ) ) ;
#34563 = VECTOR ( 'NONE', #23583, 999.9999999999998863 ) ;
#34564 = VECTOR ( 'NONE', #98948, 1000.000000000000000 ) ;
#34565 = DIRECTION ( 'NONE',  ( 0.7071067811865487940, 0.7071067811865463515, 0.000000000000000000 ) ) ;
#34566 = VECTOR ( 'NONE', #25310, 1000.000000000000000 ) ;
#34567 = CARTESIAN_POINT ( 'NONE',  ( 12.69999999999999574, -22.26999999999999247, -39.50000000000000000 ) ) ;
#34568 = CARTESIAN_POINT ( 'NONE',  ( 6.299744871391586898, -27.71228299555210484, 4.000000000000000000 ) ) ;
#34569 = CARTESIAN_POINT ( 'NONE',  ( 13.00193056682088688, -22.22500000000000142, 4.500000000000000888 ) ) ;
#34570 = ORIENTED_EDGE ( 'NONE', *, *, #73842, .T. ) ;
#34571 = VECTOR ( 'NONE', #105554, 1000.000000000000000 ) ;
#34572 = LINE ( 'NONE', #123009, #74845 ) ;
#34573 = EDGE_CURVE ( 'NONE', #104604, #23136, #34766, .T. ) ;
#34574 = EDGE_CURVE ( 'NONE', #99644, #119678, #36195, .T. ) ;
#34575 = CARTESIAN_POINT ( 'NONE',  ( 9.603736474768549414, 5.808823158059036373, 5.808823158059032821 ) ) ;
#34576 = LINE ( 'NONE', #35314, #74059 ) ;
#34577 = CARTESIAN_POINT ( 'NONE',  ( 29.99999999999978328, 17.58746187583907172, 4.000000000000000000 ) ) ;
#34578 = CARTESIAN_POINT ( 'NONE',  ( -0.1839886062690032631, 28.73617430169787568, 5.000000000000000000 ) ) ;
#34579 = ORIENTED_EDGE ( 'NONE', *, *, #100328, .F. ) ;
#34580 = ORIENTED_EDGE ( 'NONE', *, *, #14780, .T. ) ;
#34581 = VERTEX_POINT ( 'NONE', #46389 ) ;
#34582 = DIRECTION ( 'NONE',  ( -0.6830127018922181881, 0.6830127018922202975, -0.2588190451025214056 ) ) ;
#34583 = UNCERTAINTY_MEASURE_WITH_UNIT (LENGTH_MEASURE( 1.000000000000000082E-05 ), #71296, 'distance_accuracy_value', 'NONE');
#34584 = VECTOR ( 'NONE', #48855, 999.9999999999998863 ) ;
#34585 = DIRECTION ( 'NONE',  ( 0.6830127018922181881, 0.6830127018922202975, -0.2588190451025214056 ) ) ;
#34586 = CARTESIAN_POINT ( 'NONE',  ( 27.29974487139158512, -27.71228299555225405, 4.000000000000000000 ) ) ;
#34587 = CARTESIAN_POINT ( 'NONE',  ( 8.901524630118204939, 8.548075541684278633, -4.146687777219522530 ) ) ;
#34588 = DIRECTION ( 'NONE',  ( 0.000000000000000000, 0.000000000000000000, 1.000000000000000000 ) ) ;
#34589 = DIRECTION ( 'NONE',  ( 0.000000000000000000, -1.000000000000000000, 0.000000000000000000 ) ) ;
#34590 = FACE_OUTER_BOUND ( 'NONE', #6797, .T. ) ;
#34591 = FACE_OUTER_BOUND ( 'NONE', #29160, .T. ) ;
#34592 = EDGE_LOOP ( 'NONE', ( #30785, #109275, #45922, #78497 ) ) ;
#34593 = PLANE ( 'NONE',  #129850 ) ;
#34594 = ORIENTED_EDGE ( 'NONE', *, *, #141859, .F. ) ;
#34595 = CARTESIAN_POINT ( 'NONE',  ( 19.92001344501310456, -3.130733134304450438, -35.06310854429385415 ) ) ;
#34596 = ORIENTED_EDGE ( 'NONE', *, *, #40328, .F. ) ;
#34597 = DIRECTION ( 'NONE',  ( 0.000000000000000000, 1.000000000000000000, 0.000000000000000000 ) ) ;
#34599 = VERTEX_POINT ( 'NONE', #2824 ) ;
#34598 = CARTESIAN_POINT ( 'NONE',  ( 2.475998614145494603, 22.03583458319438648, 4.979811245910084061 ) ) ;
#34600 = CARTESIAN_POINT ( 'NONE',  ( -26.99451991528749417, 28.92564299267956685, 4.000000000000000000 ) ) ;
#34601 = LINE ( 'NONE', #91820, #58839 ) ;
#34602 = ORIENTED_EDGE ( 'NONE', *, *, #103559, .T. ) ;
#34603 = CARTESIAN_POINT ( 'NONE',  ( 15.48921356237309510, -27.52281430457066236, 5.000000000000000000 ) ) ;
#34604 = VERTEX_POINT ( 'NONE', #90576 ) ;
#34605 = PLANE ( 'NONE',  #69954 ) ;
#34606 = VERTEX_POINT ( 'NONE', #134812 ) ;
#34607 = CARTESIAN_POINT ( 'NONE',  ( 9.748407645496676821, 9.139736423841732040E-16, 0.000000000000000000 ) ) ;
#34608 = CARTESIAN_POINT ( 'NONE',  ( 105.3708603837962272, 6.884901960086289741, -3.974999999999993427 ) ) ;
#34609 =( LENGTH_UNIT ( ) NAMED_UNIT ( * ) SI_UNIT ( .MILLI., .METRE. ) );
#34610 = CARTESIAN_POINT ( 'NONE',  ( 19.21071296386495675, 9.141836041257182188, 4.000000000000000000 ) ) ;
#34611 = ORIENTED_EDGE ( 'NONE', *, *, #80918, .T. ) ;
#34612 = CARTESIAN_POINT ( 'NONE',  ( 32.99451991528749062, 28.92564299267960948, 4.000000000000000000 ) ) ;
#34613 = EDGE_CURVE ( 'NONE', #25257, #21326, #133370, .T. ) ;
#34614 = LINE ( 'NONE', #13541, #106248 ) ;
#34615 = CARTESIAN_POINT ( 'NONE',  ( 11.95833333333333393, -3.047499999999997211, -5.278424836066143655 ) ) ;
#34616 = CARTESIAN_POINT ( 'NONE',  ( 21.85373647476855297, -5.808823158059035485, -5.808823158059033709 ) ) ;
#34617 = DIRECTION ( 'NONE',  ( -0.7071067811865486830, -0.7071067811865464625, 0.000000000000000000 ) ) ;
#34618 = DIRECTION ( 'NONE',  ( -1.000000000000000000, -1.224606353822377258E-16, -0.000000000000000000 ) ) ;
#34619 = ORIENTED_EDGE ( 'NONE', *, *, #52294, .F. ) ;
#34620 = ORIENTED_EDGE ( 'NONE', *, *, #104940, .T. ) ;
#34621 = CARTESIAN_POINT ( 'NONE',  ( 11.99999999999991296, -10.06887692260771239, 4.000000000000000000 ) ) ;
#34622 = ORIENTED_EDGE ( 'NONE', *, *, #102664, .F. ) ;
#34623 = VECTOR ( 'NONE', #21742, 1000.000000000000000 ) ;
#34624 = CARTESIAN_POINT ( 'NONE',  ( 89.54209685856477563, 5.291415217122923842, -3.054999999999996163 ) ) ;
#34625 = PLANE ( 'NONE',  #112616 ) ;
#34626 = CARTESIAN_POINT ( 'NONE',  ( -34.42500000000001137, 0.000000000000000000, 4.500000000000000888 ) ) ;
#34627 = VECTOR ( 'NONE', #60753, 1000.000000000000000 ) ;
#34628 = CARTESIAN_POINT ( 'NONE',  ( 33.48921356237309510, -27.52281430457078670, 5.000000000000000000 ) ) ;
#34629 = CARTESIAN_POINT ( 'NONE',  ( -18.29974487139159223, -27.71228299555219010, 4.000000000000000000 ) ) ;
#34630 = ORIENTED_EDGE ( 'NONE', *, *, #139243, .T. ) ;
#34631 = AXIS2_PLACEMENT_3D ( 'NONE', #7205, #118109, #139927 ) ;
#34632 = VECTOR ( 'NONE', #81673, 1000.000000000000000 ) ;
#34633 = DIRECTION ( 'NONE',  ( -0.000000000000000000, 0.3543493200069153248, 0.9351131265310292928 ) ) ;
#34634 = FILL_AREA_STYLE_COLOUR ( '', #99756 ) ;
#34636 = EDGE_CURVE ( 'NONE', #121050, #96774, #102169, .T. ) ;
#34635 = AXIS2_PLACEMENT_3D ( 'NONE', #71608, #13622, #104190 ) ;
#34637 = FACE_OUTER_BOUND ( 'NONE', #23926, .T. ) ;
#34638 = CARTESIAN_POINT ( 'NONE',  ( 153.4000000000000057, 26.96999999999993847, -34.92499999999998295 ) ) ;
#34639 = ADVANCED_FACE ( 'NONE', ( #66681 ), #100022, .T. ) ;
#34640 = EDGE_CURVE ( 'NONE', #12475, #25213, #52676, .T. ) ;
#34641 =( LENGTH_UNIT ( ) NAMED_UNIT ( * ) SI_UNIT ( .MILLI., .METRE. ) );
#34643 = ORIENTED_EDGE ( 'NONE', *, *, #132387, .T. ) ;
#34642 = DIRECTION ( 'NONE',  ( 0.7071067811865486830, -0.7071067811865464625, -0.000000000000000000 ) ) ;
#34644 = DIRECTION ( 'NONE',  ( -1.000000000000000000, -1.224606353822377258E-16, -0.000000000000000000 ) ) ;
#34645 = CARTESIAN_POINT ( 'NONE',  ( 101.8708603837962272, 6.884901960086289741, -3.974999999999993427 ) ) ;
#34646 = CARTESIAN_POINT ( 'NONE',  ( 0.000000000000000000, 0.000000000000000000, 5.000000000000000000 ) ) ;
#34647 = DIRECTION ( 'NONE',  ( 0.7071067811865487940, 0.7071067811865463515, -0.000000000000000000 ) ) ;
#34648 = AXIS2_PLACEMENT_3D ( 'NONE', #62980, #18701, #141209 ) ;
#34649 = CARTESIAN_POINT ( 'NONE',  ( -9.280019679893985796, 0.7592924766157034266, 14.27032725228007060 ) ) ;
#34650 = EDGE_CURVE ( 'NONE', #111873, #65837, #34060, .T. ) ;
#34652 = VERTEX_POINT ( 'NONE', #14432 ) ;
#34651 = EDGE_CURVE ( 'NONE', #76579, #51133, #69552, .T. ) ;
#34653 = ORIENTED_EDGE ( 'NONE', *, *, #112277, .T. ) ;
#34654 = ORIENTED_EDGE ( 'NONE', *, *, #38288, .T. ) ;
#34655 = CARTESIAN_POINT ( 'NONE',  ( 96.25043019189810423, 3.055000000000002824, -5.291415217122919401 ) ) ;
#34656 = ORIENTED_EDGE ( 'NONE', *, *, #132523, .T. ) ;
#34657 = EDGE_CURVE ( 'NONE', #65821, #36066, #31883, .T. ) ;
#34658 = CARTESIAN_POINT ( 'NONE',  ( 1.353980332882009252, 4.584330080086930965E-16, 0.000000000000000000 ) ) ;
#34659 = FACE_OUTER_BOUND ( 'NONE', #50424, .T. ) ;
#34660 = VECTOR ( 'NONE', #35344, 1000.000000000000000 ) ;
#34661 = CARTESIAN_POINT ( 'NONE',  ( 34.92499999999998295, -22.22500000000000142, 4.500000000000000888 ) ) ;
#34662 = FACE_OUTER_BOUND ( 'NONE', #120867, .T. ) ;
#34663 = VERTEX_POINT ( 'NONE', #88442 ) ;
#34664 = DIRECTION ( 'NONE',  ( -1.000000000000000000, -1.224606353822377258E-16, -0.000000000000000000 ) ) ;
#34665 = CARTESIAN_POINT ( 'NONE',  ( -34.92500000000001137, 8.947904407527545345, 10.03118784388416351 ) ) ;
#34666 = EDGE_CURVE ( 'NONE', #142228, #73248, #83254, .T. ) ;
#34667 = CARTESIAN_POINT ( 'NONE',  ( 0.3281693992235254487, -12.74070752338415602, 4.000000000000000000 ) ) ;
#34668 = CARTESIAN_POINT ( 'NONE',  ( 89.59959685856475176, -6.109999999999997655, -1.637169565754160283 ) ) ;
#34669 = EDGE_LOOP ( 'NONE', ( #122909, #30005, #58726, #87315 ) ) ;
#34670 = DIRECTION ( 'NONE',  ( 0.7071067811865487940, 0.7071067811865463515, 0.000000000000000000 ) ) ;
#34671 = LINE ( 'NONE', #112929, #37708 ) ;
#34672 = AXIS2_PLACEMENT_3D ( 'NONE', #77124, #32156, #21283 ) ;
#34673 = EDGE_CURVE ( 'NONE', #123961, #74602, #26726, .T. ) ;
#34674 = VECTOR ( 'NONE', #127125, 1000.000000000000000 ) ;
#34675 = VECTOR ( 'NONE', #36905, 1000.000000000000227 ) ;
#34676 = ORIENTED_EDGE ( 'NONE', *, *, #78841, .T. ) ;
#34677 = VERTEX_POINT ( 'NONE', #4190 ) ;
#34678 = CARTESIAN_POINT ( 'NONE',  ( 48.48921356237309510, -27.52281430457089328, 5.000000000000000000 ) ) ;
#34679 = CIRCLE ( 'NONE', #87961, 0.5000000000000004441 ) ;
#34680 = DIRECTION ( 'NONE',  ( -1.000000000000000000, -0.000000000000000000, -0.000000000000000000 ) ) ;
#34681 = DIRECTION ( 'NONE',  ( -1.000000000000000000, 0.000000000000000000, -0.000000000000000000 ) ) ;
#34682 = CIRCLE ( 'NONE', #53183, 5.968999999999998529 ) ;
#34683 = ADVANCED_FACE ( 'NONE', ( #138351 ), #92678, .T. ) ;
#34684 = LINE ( 'NONE', #2743, #94226 ) ;
#34685 = PLANE ( 'NONE',  #11743 ) ;
#34686 = CARTESIAN_POINT ( 'NONE',  ( -6.851816449618514326, 17.25929247661554555, 8.802941693769186671 ) ) ;
#34687 =( NAMED_UNIT ( * ) PLANE_ANGLE_UNIT ( ) SI_UNIT ( $, .RADIAN. ) );
#34688 = ORIENTED_EDGE ( 'NONE', *, *, #26492, .F. ) ;
#34689 = ORIENTED_EDGE ( 'NONE', *, *, #55950, .T. ) ;
#34690 = CARTESIAN_POINT ( 'NONE',  ( -11.51078643762690490, -27.52281430457047406, 5.000000000000000000 ) ) ;
#34691 = ORIENTED_EDGE ( 'NONE', *, *, #122830, .F. ) ;
#34692 = VERTEX_POINT ( 'NONE', #61537 ) ;
#34693 = EDGE_CURVE ( 'NONE', #124198, #107914, #60089, .T. ) ;
#34694 = VECTOR ( 'NONE', #10510, 1000.000000000000000 ) ;
#34695 = EDGE_CURVE ( 'NONE', #96522, #83686, #70968, .T. ) ;
#34696 = LINE ( 'NONE', #135446, #47443 ) ;
#34697 = ORIENTED_EDGE ( 'NONE', *, *, #129435, .F. ) ;
#34698 = DIRECTION ( 'NONE',  ( 0.7071067811865487940, -0.7071067811865463515, 0.000000000000000000 ) ) ;
#34699 = DIRECTION ( 'NONE',  ( -0.7071067811865486830, -0.7071067811865464625, 0.000000000000000000 ) ) ;
#34700 = EDGE_CURVE ( 'NONE', #95585, #72440, #93415, .T. ) ;
#34701 = LINE ( 'NONE', #33308, #25202 ) ;
#34702 = DIRECTION ( 'NONE',  ( -0.000000000000000000, 0.000000000000000000, 1.000000000000000000 ) ) ;
#34703 = ORIENTED_EDGE ( 'NONE', *, *, #111097, .T. ) ;
#34704 = EDGE_CURVE ( 'NONE', #17089, #57042, #82542, .T. ) ;
#34705 = CARTESIAN_POINT ( 'NONE',  ( 34.92500000000001847, -6.269999999999991580, -36.39086428169088094 ) ) ;
#34706 = ORIENTED_EDGE ( 'NONE', *, *, #53365, .F. ) ;
#34707 = CARTESIAN_POINT ( 'NONE',  ( 4.911592354503321545, 9.902892378096218942E-16, 0.000000000000000000 ) ) ;
#34708 = EDGE_LOOP ( 'NONE', ( #108473, #121347, #91424, #38421 ) ) ;
#34709 = PLANE ( 'NONE',  #60834 ) ;
#34710 = ORIENTED_EDGE ( 'NONE', *, *, #31790, .F. ) ;
#34711 = CARTESIAN_POINT ( 'NONE',  ( 12.18398860626900060, 28.73617430169795739, 5.000000000000000000 ) ) ;
#34712 = ORIENTED_EDGE ( 'NONE', *, *, #101230, .F. ) ;
#34713 = ORIENTED_EDGE ( 'NONE', *, *, #103078, .T. ) ;
#34714 = VERTEX_POINT ( 'NONE', #26025 ) ;
#34715 = CARTESIAN_POINT ( 'NONE',  ( -60.48921356237309510, -27.52281430457097500, 5.000000000000000000 ) ) ;
#34716 = DIRECTION ( 'NONE',  ( 0.000000000000000000, 0.000000000000000000, 1.000000000000000000 ) ) ;
#34717 = DIRECTION ( 'NONE',  ( -0.3543493200069162685, -0.000000000000000000, -0.9351131265310288487 ) ) ;
#34718 = CARTESIAN_POINT ( 'NONE',  ( 114.7712635252314328, 4.472830434245838482, 4.472830434245842035 ) ) ;
#34719 = CARTESIAN_POINT ( 'NONE',  ( 0.2569208697893814453, 4.202752102959690472E-16, 0.000000000000000000 ) ) ;
#34720 = EDGE_CURVE ( 'NONE', #122031, #100841, #39032, .T. ) ;
#34721 = DIRECTION ( 'NONE',  ( 0.7071067811865487940, 0.7071067811865463515, -0.000000000000000000 ) ) ;
#34723 = CARTESIAN_POINT ( 'NONE',  ( 18.79653912142945060, 3.061616997868387579E-16, -2.500000000000000444 ) ) ;
#34722 = DIRECTION ( 'NONE',  ( 0.6830127018922181881, 0.6830127018922202975, -0.2588190451025214056 ) ) ;
#34724 = EDGE_CURVE ( 'NONE', #113538, #118058, #71236, .T. ) ;
#34725 = LINE ( 'NONE', #78964, #23884 ) ;
#34727 = ORIENTED_EDGE ( 'NONE', *, *, #119868, .T. ) ;
#34726 = CIRCLE ( 'NONE', #134280, 0.5000000000000004441 ) ;
#34728 = CARTESIAN_POINT ( 'NONE',  ( 20.67906569311139009, 4.202752102959690472E-16, 0.000000000000000000 ) ) ;
#34729 = DIRECTION ( 'NONE',  ( -0.7071067811865486830, -0.7071067811865464625, 0.000000000000000000 ) ) ;
#34730 = LINE ( 'NONE', #78970, #40228 ) ;
#34731 = VERTEX_POINT ( 'NONE', #49929 ) ;
#34732 = ORIENTED_EDGE ( 'NONE', *, *, #57465, .T. ) ;
#34733 = AXIS2_PLACEMENT_3D ( 'NONE', #46659, #90849, #135079 ) ;
#34734 = LINE ( 'NONE', #132652, #142096 ) ;
#34735 = VECTOR ( 'NONE', #31177, 1000.000000000000000 ) ;
#34736 = AXIS2_PLACEMENT_3D ( 'NONE', #136380, #92875, #82047 ) ;
#34737 = ORIENTED_EDGE ( 'NONE', *, *, #82221, .F. ) ;
#34738 = EDGE_LOOP ( 'NONE', ( #3605, #61002, #109732, #93844 ) ) ;
#34739 = CARTESIAN_POINT ( 'NONE',  ( 0.000000000000000000, 21.72500000000000142, 4.500000000000000888 ) ) ;
#34740 = CARTESIAN_POINT ( 'NONE',  ( 107.8500270504628844, -5.819803920172573086, -5.819803920172573086 ) ) ;
#34741 = ADVANCED_FACE ( 'NONE', ( #91981 ), #68961, .T. ) ;
#34742 = CARTESIAN_POINT ( 'NONE',  ( -11.99999999999991473, -19.22509904557637839, 1.855685503482151111 ) ) ;
#34743 = CARTESIAN_POINT ( 'NONE',  ( -32.99451991528749062, 28.92564299267960948, 4.000000000000000000 ) ) ;
#34744 = ADVANCED_FACE ( 'NONE', ( #73114 ), #126059, .F. ) ;
#34745 = VERTEX_POINT ( 'NONE', #115123 ) ;
#34746 = CARTESIAN_POINT ( 'NONE',  ( 27.48921356237309155, -27.52281430457074762, 5.000000000000000000 ) ) ;
#34748 = VERTEX_POINT ( 'NONE', #6347 ) ;
#34747 = VECTOR ( 'NONE', #27648, 1000.000000000000000 ) ;
#34749 = DIRECTION ( 'NONE',  ( 0.6830127018922180770, -0.6830127018922204085, -0.2588190451025213501 ) ) ;
#34750 = ADVANCED_FACE ( 'NONE', ( #104258 ), #17952, .F. ) ;
#34751 = CARTESIAN_POINT ( 'NONE',  ( 23.40040314143521982, -7.934999999999989839, 2.126176841940957907 ) ) ;
#34752 = ORIENTED_EDGE ( 'NONE', *, *, #66926, .F. ) ;
#34753 = CARTESIAN_POINT ( 'NONE',  ( 85.22459685856478018, -1.637169565754161171, 6.109999999999998543 ) ) ;
#34754 = DIRECTION ( 'NONE',  ( 0.000000000000000000, 0.000000000000000000, 1.000000000000000000 ) ) ;
#34755 = PLANE ( 'NONE',  #85931 ) ;
#34756 = ORIENTED_EDGE ( 'NONE', *, *, #135187, .T. ) ;
#34757 = ORIENTED_EDGE ( 'NONE', *, *, #61214, .F. ) ;
#34758 = ORIENTED_EDGE ( 'NONE', *, *, #6532, .T. ) ;
#34760 = VECTOR ( 'NONE', #129261, 1000.000000000000000 ) ;
#34759 = CARTESIAN_POINT ( 'NONE',  ( -27.32816939922334143, -21.74070752338406365, 4.000000000000000000 ) ) ;
#34761 = DIRECTION ( 'NONE',  ( 0.000000000000000000, -1.000000000000000000, 0.000000000000000000 ) ) ;
#34762 = CARTESIAN_POINT ( 'NONE',  ( -3.781626882924915112, 21.74787736706806385, 4.999607392498048419 ) ) ;
#34763 = CARTESIAN_POINT ( 'NONE',  ( 34.92499999999998295, -5.143876922607530489, 4.000000000000000000 ) ) ;
#34765 = ADVANCED_FACE ( 'NONE', ( #3515 ), #47809, .F. ) ;
#34764 = ORIENTED_EDGE ( 'NONE', *, *, #102296, .T. ) ;
#34766 = LINE ( 'NONE', #68149, #89735 ) ;
#34767 = VECTOR ( 'NONE', #104706, 1000.000000000000000 ) ;
#34768 = EDGE_CURVE ( 'NONE', #124632, #100584, #36876, .T. ) ;
#34769 = LINE ( 'NONE', #23125, #65173 ) ;
#34770 = DIRECTION ( 'NONE',  ( -0.7071067811865486830, -0.7071067811865464625, 0.000000000000000000 ) ) ;
#34771 = VECTOR ( 'NONE', #54085, 1000.000000000000227 ) ;
#34772 = ORIENTED_EDGE ( 'NONE', *, *, #42040, .T. ) ;
#34773 = DIRECTION ( 'NONE',  ( 0.7071067811865487940, 0.7071067811865463515, 0.000000000000000000 ) ) ;
#34775 = VECTOR ( 'NONE', #105730, 1000.000000000000000 ) ;
#34774 = DIRECTION ( 'NONE',  ( -1.000000000000000000, -0.000000000000000000, -0.000000000000000000 ) ) ;
#34776 = VERTEX_POINT ( 'NONE', #126730 ) ;
#34778 = EDGE_LOOP ( 'NONE', ( #92042, #12006, #109054, #32530 ) ) ;
#34777 = SURFACE_STYLE_USAGE ( .BOTH. , #136928 ) ;
#34779 = VERTEX_POINT ( 'NONE', #81131 ) ;
#34780 = EDGE_CURVE ( 'NONE', #14374, #116655, #125338, .T. ) ;
#34781 = VECTOR ( 'NONE', #97683, 999.9999999999998863 ) ;
#34782 = DIRECTION ( 'NONE',  ( 1.000000000000000000, 1.224606353822377258E-16, 0.000000000000000000 ) ) ;
#34783 = VECTOR ( 'NONE', #40712, 1000.000000000000000 ) ;
#34784 = CARTESIAN_POINT ( 'NONE',  ( 38.99451991528749062, 28.92564299267965211, 4.000000000000000000 ) ) ;
#34785 = EDGE_LOOP ( 'NONE', ( #140331, #116704, #108839, #95473 ) ) ;
#34786 = CARTESIAN_POINT ( 'NONE',  ( 9.682526172861077640, 2.055000000000001048, 2.516649172247811554E-16 ) ) ;
#34787 = UNCERTAINTY_MEASURE_WITH_UNIT (LENGTH_MEASURE( 1.000000000000000082E-05 ), #94824, 'distance_accuracy_value', 'NONE');
#34788 = DIRECTION ( 'NONE',  ( 0.6830127018922180770, -0.6830127018922204085, -0.2588190451025213501 ) ) ;
#34789 = CARTESIAN_POINT ( 'NONE',  ( 23.81601139373100295, 28.73617430169770870, 5.000000000000000000 ) ) ;
#34790 = DIRECTION ( 'NONE',  ( -0.7071067811865487940, 0.7071067811865463515, -0.000000000000000000 ) ) ;
#34791 = LINE ( 'NONE', #46413, #18160 ) ;
#34792 = CARTESIAN_POINT ( 'NONE',  ( 34.75611968250419181, 5.812934254707337267, 4.955485411084878500 ) ) ;
#34793 = CARTESIAN_POINT ( 'NONE',  ( -17.51078643762690845, -27.52281430457043143, 5.000000000000000000 ) ) ;
#34794 = DIRECTION ( 'NONE',  ( 0.000000000000000000, -1.000000000000000000, 0.000000000000000000 ) ) ;
#34795 = CARTESIAN_POINT ( 'NONE',  ( 9.328169399223462221, 20.25929247661551358, 4.000000000000000000 ) ) ;
#34797 = VECTOR ( 'NONE', #79947, 1000.000000000000000 ) ;
#34796 = CARTESIAN_POINT ( 'NONE',  ( 25.20790314143522082, -6.871911579029513106, -3.967499999999993587 ) ) ;
#34798 = CARTESIAN_POINT ( 'NONE',  ( 2.312069808101886004, 7.934999999999992504, 2.126176841940951689 ) ) ;
#34799 = CARTESIAN_POINT ( 'NONE',  ( -35.99451991528749772, 28.92564299267963079, 4.000000000000000000 ) ) ;
#34800 = CARTESIAN_POINT ( 'NONE',  ( -25.49999999999982592, 9.431123077392085108, 4.000000000000000000 ) ) ;
#34801 = CARTESIAN_POINT ( 'NONE',  ( -34.42500000000001137, -21.02281430457035682, 5.000000000000000000 ) ) ;
#34802 = ORIENTED_EDGE ( 'NONE', *, *, #123242, .T. ) ;
#34803 = ORIENTED_EDGE ( 'NONE', *, *, #65143, .T. ) ;
#34804 = CARTESIAN_POINT ( 'NONE',  ( 101.4791666666666430, -7.950000000000001066, 2.130196079827424427 ) ) ;
#34805 = EDGE_LOOP ( 'NONE', ( #98551, #36831, #20279, #126457 ) ) ;
#34806 = EDGE_LOOP ( 'NONE', ( #47901, #36740, #80686 ) ) ;
#34807 = ORIENTED_EDGE ( 'NONE', *, *, #44900, .T. ) ;
#34808 = ADVANCED_FACE ( 'NONE', ( #16542 ), #104992, .F. ) ;
#34809 = DIRECTION ( 'NONE',  ( 0.7071067811865487940, 0.7071067811865463515, 0.000000000000000000 ) ) ;
#34810 = LINE ( 'NONE', #25332, #67249 ) ;
#34811 = VECTOR ( 'NONE', #10972, 1000.000000000000000 ) ;
#34812 = CARTESIAN_POINT ( 'NONE',  ( 15.52000000000000135, -2.055000000000000160, 2.789133085058098087E-16 ) ) ;
#34813 = ORIENTED_EDGE ( 'NONE', *, *, #90812, .F. ) ;
#34814 = DIRECTION ( 'NONE',  ( -0.3543493200069162685, -0.000000000000000000, -0.9351131265310288487 ) ) ;
#34815 = CARTESIAN_POINT ( 'NONE',  ( -6.411614905948260557, 22.22500000000000142, 4.777194822843818578 ) ) ;
#34816 = DIRECTION ( 'NONE',  ( 0.3543493200069162685, -0.000000000000000000, -0.9351131265310288487 ) ) ;
#34817 = CARTESIAN_POINT ( 'NONE',  ( 57.18398860626899705, 28.73617430169827358, 5.000000000000000000 ) ) ;
#34818 = EDGE_LOOP ( 'NONE', ( #49664, #123870, #28504, #29263 ) ) ;
#34819 = EDGE_CURVE ( 'NONE', #17816, #98498, #31029, .T. ) ;
#34820 = EDGE_CURVE ( 'NONE', #120961, #26817, #53481, .T. ) ;
#34821 = CARTESIAN_POINT ( 'NONE',  ( 128.0995968585647802, -6.109999999999997655, -1.637169565754160283 ) ) ;
#34822 = CARTESIAN_POINT ( 'NONE',  ( -23.99999999999983302, -4.068876922607771895, 4.000000000000000000 ) ) ;
#34823 = CARTESIAN_POINT ( 'NONE',  ( -36.18398860626899705, 28.73617430169812437, 5.000000000000000000 ) ) ;
#34824 = DIRECTION ( 'NONE',  ( -1.000000000000000000, -1.224606353822377258E-16, -0.000000000000000000 ) ) ;
#34825 = VECTOR ( 'NONE', #117832, 1000.000000000000000 ) ;
#34826 = LINE ( 'NONE', #113797, #2910 ) ;
#34827 = CARTESIAN_POINT ( 'NONE',  ( 10.83999999999999986, 2.055000000000001492, 0.000000000000000000 ) ) ;
#34828 = AXIS2_PLACEMENT_3D ( 'NONE', #4356, #36356, #125508 ) ;
#34829 = CARTESIAN_POINT ( 'NONE',  ( -12.69999999999998153, 0.000000000000000000, 0.000000000000000000 ) ) ;
#34830 = DIRECTION ( 'NONE',  ( -0.000000000000000000, 0.000000000000000000, 1.000000000000000000 ) ) ;
#34831 = ADVANCED_FACE ( 'NONE', ( #129589 ), #118720, .T. ) ;
#34832 = EDGE_CURVE ( 'NONE', #45231, #142570, #120119, .T. ) ;
#34833 = ORIENTED_EDGE ( 'NONE', *, *, #67568, .F. ) ;
#34834 = ORIENTED_EDGE ( 'NONE', *, *, #11832, .T. ) ;
#34835 = CARTESIAN_POINT ( 'NONE',  ( 122.3545968585647472, -1.637169565754161615, 6.110000000000000320 ) ) ;
#34836 = EDGE_CURVE ( 'NONE', #81792, #86890, #96232, .T. ) ;
#34837 = ORIENTED_EDGE ( 'NONE', *, *, #31255, .T. ) ;
#34838 = EDGE_CURVE ( 'NONE', #47477, #142342, #107828, .T. ) ;
#34839 = FACE_OUTER_BOUND ( 'NONE', #113308, .T. ) ;
#34840 = EDGE_CURVE ( 'NONE', #13236, #20396, #18677, .T. ) ;
#34841 = FILL_AREA_STYLE ('',( #68905 ) ) ;
#34842 = COLOUR_RGB ( '', 0.09019608, 0.27058824, 0.51372549) ;
#34843 = DIRECTION ( 'NONE',  ( -0.000000000000000000, 0.3543493200069153248, 0.9351131265310292928 ) ) ;
#34844 = PLANE ( 'NONE',  #106717 ) ;
#34845 = VECTOR ( 'NONE', #140580, 1000.000000000000000 ) ;
#34846 = ADVANCED_FACE ( 'NONE', ( #65090 ), #109281, .T. ) ;
#34847 = VECTOR ( 'NONE', #122737, 1000.000000000000000 ) ;
#34848 = CARTESIAN_POINT ( 'NONE',  ( 116.4329301918981088, 1.637169565754156508, 6.110000000000000320 ) ) ;
#34849 = ORIENTED_EDGE ( 'NONE', *, *, #61755, .F. ) ;
#34850 = ORIENTED_EDGE ( 'NONE', *, *, #101254, .T. ) ;
#34851 = AXIS2_PLACEMENT_3D ( 'NONE', #120655, #39015, #73098 ) ;
#34852 = VECTOR ( 'NONE', #59569, 1000.000000000000000 ) ;
#34853 =( GEOMETRIC_REPRESENTATION_CONTEXT ( 3 ) GLOBAL_UNCERTAINTY_ASSIGNED_CONTEXT ( ( #88254 ) ) GLOBAL_UNIT_ASSIGNED_CONTEXT ( ( #118250, #20360, #42882 ) ) REPRESENTATION_CONTEXT ( 'NONE', 'WORKASPACE' ) );
#34854 = CARTESIAN_POINT ( 'NONE',  ( -33.70701326429281153, -21.74070752338405299, 4.999753212805220670 ) ) ;
#34855 = AXIS2_PLACEMENT_3D ( 'NONE', #47770, #49897, #38993 ) ;
#34856 = ADVANCED_FACE ( 'NONE', ( #52057 ), #20110, .T. ) ;
#34857 = ORIENTED_EDGE ( 'NONE', *, *, #48379, .T. ) ;
#34858 = EDGE_LOOP ( 'NONE', ( #84342, #71869, #46149, #106981 ) ) ;
#34859 = ORIENTED_EDGE ( 'NONE', *, *, #82645, .F. ) ;
#34860 = CARTESIAN_POINT ( 'NONE',  ( -25.39999999999996305, 0.000000000000000000, 2.500000000000000000 ) ) ;
#34861 = CARTESIAN_POINT ( 'NONE',  ( 4.150403141435219823, 7.934999999999988951, -2.126176841940961904 ) ) ;
#34862 = AXIS2_PLACEMENT_3D ( 'NONE', #26076, #123267, #47860 ) ;
#34863 = EDGE_CURVE ( 'NONE', #140375, #77966, #74538, .T. ) ;
#34864 = CARTESIAN_POINT ( 'NONE',  ( 31.84959685856478373, 6.109999999999996767, 1.637169565754163836 ) ) ;
#34865 = ORIENTED_EDGE ( 'NONE', *, *, #102259, .F. ) ;
#34866 = CARTESIAN_POINT ( 'NONE',  ( 84.99999999999998579, 0.000000000000000000, -7.950000000000000178 ) ) ;
#34867 = VERTEX_POINT ( 'NONE', #97688 ) ;
#34868 = ORIENTED_EDGE ( 'NONE', *, *, #134261, .F. ) ;
#34869 = AXIS2_PLACEMENT_3D ( 'NONE', #52092, #75294, #118767 ) ;
#34870 = VERTEX_POINT ( 'NONE', #40483 ) ;
#34871 = AXIS2_PLACEMENT_3D ( 'NONE', #97412, #52494, #41621 ) ;
#34872 = EDGE_CURVE ( 'NONE', #122126, #113634, #52743, .T. ) ;
#34874 = FILL_AREA_STYLE_COLOUR ( '', #116920 ) ;
#34873 = VECTOR ( 'NONE', #73405, 1000.000000000000000 ) ;
#34875 = CARTESIAN_POINT ( 'NONE',  ( -16.64175702458850381, 15.75929247661555799, 19.34181609438703475 ) ) ;
#34876 = ORIENTED_EDGE ( 'NONE', *, *, #23214, .T. ) ;
#34877 = CARTESIAN_POINT ( 'NONE',  ( -34.92500000000001137, -22.22500000000000142, 4.500000000000000888 ) ) ;
#34878 = EDGE_CURVE ( 'NONE', #27313, #111053, #128884, .T. ) ;
#34879 = VECTOR ( 'NONE', #8868, 1000.000000000000000 ) ;
#34880 = DIRECTION ( 'NONE',  ( -0.7071067811865486830, 0.7071067811865464625, 0.000000000000000000 ) ) ;
#34881 = VECTOR ( 'NONE', #138910, 1000.000000000000227 ) ;
#34882 = EDGE_CURVE ( 'NONE', #49135, #64365, #59153, .T. ) ;
#34883 = CARTESIAN_POINT ( 'NONE',  ( -71.99451991528749772, 28.92564299267988304, 4.000000000000000000 ) ) ;
#34884 = FACE_BOUND ( 'NONE', #46329, .T. ) ;
#34885 = EDGE_LOOP ( 'NONE', ( #102413, #96004, #100945, #68585 ) ) ;
#34886 = CARTESIAN_POINT ( 'NONE',  ( -19.49999999999986855, -14.56887692260766087, 4.000000000000000000 ) ) ;
#34887 = DIRECTION ( 'NONE',  ( 0.000000000000000000, -1.000000000000000000, 0.000000000000000000 ) ) ;
#34888 = AXIS2_PLACEMENT_3D ( 'NONE', #68653, #123750, #26556 ) ;
#34889 = CARTESIAN_POINT ( 'NONE',  ( 9.489213562373095101, -27.52281430457062328, 5.000000000000000000 ) ) ;
#34890 = PLANE ( 'NONE',  #64770 ) ;
#34891 = ORIENTED_EDGE ( 'NONE', *, *, #64836, .F. ) ;
#34892 = CARTESIAN_POINT ( 'NONE',  ( -15.48921356237309510, -27.52281430457066236, 5.000000000000000000 ) ) ;
#34893 = ORIENTED_EDGE ( 'NONE', *, *, #74431, .T. ) ;
#34894 = ORIENTED_EDGE ( 'NONE', *, *, #1260, .F. ) ;
#34895 = EDGE_LOOP ( 'NONE', ( #130952, #130519, #60760, #38331 ) ) ;
#34896 = CARTESIAN_POINT ( 'NONE',  ( 51.09959685856478728, -6.109999999999997655, -1.637169565754160283 ) ) ;
#34897 = VERTEX_POINT ( 'NONE', #86112 ) ;
#34898 = STYLED_ITEM ( 'NONE', ( #120687 ), #40939 ) ;
#34899 = CARTESIAN_POINT ( 'NONE',  ( 11.93159235450332112, 9.902892378096218942E-16, 0.000000000000000000 ) ) ;
#34900 = CARTESIAN_POINT ( 'NONE',  ( 6.940000000000001279, 9.521314400968980422E-16, 0.000000000000000000 ) ) ;
#34901 = ADVANCED_FACE ( 'NONE', ( #73803 ), #9152, .F. ) ;
#34902 = EDGE_LOOP ( 'NONE', ( #67331, #141193, #33618, #128173 ) ) ;
#34903 = PLANE ( 'NONE',  #44534 ) ;
#34905 = DIRECTION ( 'NONE',  ( 0.000000000000000000, 0.000000000000000000, 1.000000000000000000 ) ) ;
#34904 = COLOUR_RGB ( '', 0.66274510, 0.83137255, 0.94901961) ;
#34906 = CARTESIAN_POINT ( 'NONE',  ( -17.99451991528748351, 28.92564299267950645, 4.000000000000000000 ) ) ;
#34907 = LINE ( 'NONE', #46530, #96756 ) ;
#34908 = DIRECTION ( 'NONE',  ( -0.7071067811865486830, -0.7071067811865464625, 0.000000000000000000 ) ) ;
#34909 = FACE_OUTER_BOUND ( 'NONE', #10388, .T. ) ;
#34910 = ORIENTED_EDGE ( 'NONE', *, *, #65785, .T. ) ;
#34911 = ORIENTED_EDGE ( 'NONE', *, *, #13577, .T. ) ;
#34912 = ORIENTED_EDGE ( 'NONE', *, *, #74157, .F. ) ;
#34913 = AXIS2_PLACEMENT_3D ( 'NONE', #48642, #135650, #105151 ) ;
#34914 = ORIENTED_EDGE ( 'NONE', *, *, #109263, .T. ) ;
#34915 = CARTESIAN_POINT ( 'NONE',  ( 75.48921356237309510, -27.52281430457107803, 5.000000000000000000 ) ) ;
#34916 = ORIENTED_EDGE ( 'NONE', *, *, #9233, .F. ) ;
#34917 = VERTEX_POINT ( 'NONE', #39189 ) ;
#34918 = CARTESIAN_POINT ( 'NONE',  ( -19.05000000000000071, 3.174999999999997158, 4.000000000000000000 ) ) ;
#34919 = EDGE_CURVE ( 'NONE', #127061, #72848, #103688, .T. ) ;
#34920 = CARTESIAN_POINT ( 'NONE',  ( -39.48921356237310221, -27.52281430457082934, 5.000000000000000000 ) ) ;
#34921 = ORIENTED_EDGE ( 'NONE', *, *, #96670, .F. ) ;
#34922 = LINE ( 'NONE', #89979, #122857 ) ;
#34923 = VECTOR ( 'NONE', #96609, 1000.000000000000000 ) ;
#34924 = DIRECTION ( 'NONE',  ( -0.7071067811865487940, 0.7071067811865463515, 0.000000000000000000 ) ) ;
#34925 = EDGE_CURVE ( 'NONE', #133913, #120495, #95693, .T. ) ;
#34926 = CARTESIAN_POINT ( 'NONE',  ( 27.04623647476855197, -7.934999999999990727, 4.858786175617117713E-16 ) ) ;
#34927 = DIRECTION ( 'NONE',  ( -0.7071067811865486830, -0.7071067811865464625, 0.000000000000000000 ) ) ;
#34928 = ORIENTED_EDGE ( 'NONE', *, *, #19614, .T. ) ;
#34930 = CARTESIAN_POINT ( 'NONE',  ( 13.49999999999991473, 22.08746187583902199, 4.000000000000000000 ) ) ;
#34929 = CARTESIAN_POINT ( 'NONE',  ( 106.6620968585647802, -5.291415217122919401, 3.054999999999998384 ) ) ;
#34931 =( BOUNDED_CURVE ( )  B_SPLINE_CURVE ( 2, ( #43435, #65931, #132622, #2017, #10770, #109397, #90516, #55038, #123155, #68089, #78217, #99206, #23068 ),
 .UNSPECIFIED., .F., .T. ) 
 B_SPLINE_CURVE_WITH_KNOTS ( ( 3, 2, 2, 2, 2, 2, 3 ),
 ( 0.1166666666666666685, 0.1194444444444444503, 0.1222222222222222182, 0.1250000000000000000, 0.1277777777777777679, 0.1305555555555555636, 0.1333333333333333315 ),
 .UNSPECIFIED. ) 
 CURVE ( )  GEOMETRIC_REPRESENTATION_ITEM ( )  RATIONAL_B_SPLINE_CURVE ( ( 1.000000000000000000, 0.9659258262890683122, 1.000000000000000000, 0.9659258262890683122, 1.000000000000000000, 0.9659258262890683122, 1.000000000000000000, 0.9659258262890683122, 1.000000000000000000, 0.9659258262890683122, 1.000000000000000000, 0.9659258262890683122, 1.000000000000000000 ) ) 
 REPRESENTATION_ITEM ( '' )  );
#34932 = FACE_OUTER_BOUND ( 'NONE', #11263, .T. ) ;
#34933 = LINE ( 'NONE', #100878, #106702 ) ;
#34934 = CARTESIAN_POINT ( 'NONE',  ( 9.299744871391588674, -27.71228299555212971, 4.000000000000000000 ) ) ;
#34936 = ORIENTED_EDGE ( 'NONE', *, *, #98211, .T. ) ;
#34935 = DIRECTION ( 'NONE',  ( 0.7071067811865487940, 0.7071067811865463515, 0.000000000000000000 ) ) ;
#34937 = FACE_OUTER_BOUND ( 'NONE', #73249, .T. ) ;
#34938 = VERTEX_POINT ( 'NONE', #43464 ) ;
#34939 = FACE_OUTER_BOUND ( 'NONE', #127444, .T. ) ;
#34940 = AXIS2_PLACEMENT_3D ( 'NONE', #72970, #117126, #106232 ) ;
#34941 = CARTESIAN_POINT ( 'NONE',  ( 18.32816939922340183, -21.74070752338405654, 4.000000000000000000 ) ) ;
#34942 = PLANE ( 'NONE',  #37973 ) ;
#34944 = EDGE_CURVE ( 'NONE', #128178, #106502, #52880, .T. ) ;
#34943 = ORIENTED_EDGE ( 'NONE', *, *, #47196, .F. ) ;
#34945 = AXIS2_PLACEMENT_3D ( 'NONE', #105626, #137583, #38268 ) ;
#34946 = CARTESIAN_POINT ( 'NONE',  ( -12.20000000000000284, -25.33999999999998920, 13.17925390838734323 ) ) ;
#34947 = VECTOR ( 'NONE', #88354, 1000.000000000000000 ) ;
#34948 = ADVANCED_FACE ( 'NONE', ( #107964 ), #63807, .T. ) ;
#34949 = DIRECTION ( 'NONE',  ( -0.7071067811865487940, 0.7071067811865463515, -0.000000000000000000 ) ) ;
#34950 = DIRECTION ( 'NONE',  ( 0.6830127018922181881, 0.6830127018922202975, -0.2588190451025214056 ) ) ;
#34951 = ORIENTED_EDGE ( 'NONE', *, *, #37463, .T. ) ;
#34952 = VECTOR ( 'NONE', #82040, 999.9999999999998863 ) ;
#34953 = AXIS2_PLACEMENT_3D ( 'NONE', #137663, #126740, #84692 ) ;
#34954 = VECTOR ( 'NONE', #53290, 1000.000000000000227 ) ;
#34955 = AXIS2_PLACEMENT_3D ( 'NONE', #31272, #64602, #9466 ) ;
#34956 = DIRECTION ( 'NONE',  ( -0.7071067811865486830, -0.7071067811865464625, 0.000000000000000000 ) ) ;
#34958 = VERTEX_POINT ( 'NONE', #131911 ) ;
#34957 = VECTOR ( 'NONE', #110639, 1000.000000000000000 ) ;
#34959 = DIRECTION ( 'NONE',  ( 0.7071067811865486830, -0.7071067811865464625, -0.000000000000000000 ) ) ;
#34961 = ORIENTED_EDGE ( 'NONE', *, *, #77140, .F. ) ;
#34960 = DIRECTION ( 'NONE',  ( 1.000000000000000000, 0.000000000000000000, 0.000000000000000000 ) ) ;
#34962 = ADVANCED_FACE ( 'NONE', ( #52190 ), #8637, .F. ) ;
#34963 = EDGE_LOOP ( 'NONE', ( #77703, #105729, #85119, #103887 ) ) ;
#34964 = DIRECTION ( 'NONE',  ( -0.6830127018922181881, 0.6830127018922202975, -0.2588190451025214056 ) ) ;
#34965 = VECTOR ( 'NONE', #19300, 1000.000000000000000 ) ;
#34966 = DIRECTION ( 'NONE',  ( -0.7071067811865487940, 0.7071067811865463515, 0.000000000000000000 ) ) ;
#34967 = ORIENTED_EDGE ( 'NONE', *, *, #40447, .T. ) ;
#34968 = LINE ( 'NONE', #79205, #140925 ) ;
#34969 = DIRECTION ( 'NONE',  ( -0.3543493200069162685, -0.000000000000000000, -0.9351131265310288487 ) ) ;
#34970 = VERTEX_POINT ( 'NONE', #117420 ) ;
#34971 = VECTOR ( 'NONE', #50910, 999.9999999999998863 ) ;
#34972 = LINE ( 'NONE', #24078, #60567 ) ;
#34973 = DIRECTION ( 'NONE',  ( -0.7071067811865487940, 0.7071067811865463515, -0.000000000000000000 ) ) ;
#34974 = CARTESIAN_POINT ( 'NONE',  ( 27.79996877983145609, 8.259292476615630818, 16.85664084051834877 ) ) ;
#34975 = VECTOR ( 'NONE', #15637, 999.9999999999998863 ) ;
#34976 = FACE_OUTER_BOUND ( 'NONE', #99631, .T. ) ;
#34977 = DIRECTION ( 'NONE',  ( -0.7071067811865486830, 0.7071067811865464625, 0.000000000000000000 ) ) ;
#34978 = DIRECTION ( 'NONE',  ( -0.7071067811865486830, -0.7071067811865464625, 0.000000000000000000 ) ) ;
#34979 = ORIENTED_EDGE ( 'NONE', *, *, #41714, .F. ) ;
#34980 = VECTOR ( 'NONE', #132782, 1000.000000000000000 ) ;
#34981 = ORIENTED_EDGE ( 'NONE', *, *, #59442, .T. ) ;
#34982 = ORIENTED_EDGE ( 'NONE', *, *, #123443, .F. ) ;
#34983 = CARTESIAN_POINT ( 'NONE',  ( -2.816011393730999401, 28.73617430169785436, 5.000000000000000000 ) ) ;
#34984 = VECTOR ( 'NONE', #81567, 1000.000000000000000 ) ;
#34985 = ORIENTED_EDGE ( 'NONE', *, *, #11317, .T. ) ;
#34986 = ORIENTED_EDGE ( 'NONE', *, *, #15494, .F. ) ;
#34987 = AXIS2_PLACEMENT_3D ( 'NONE', #95493, #94067, #140433 ) ;
#34988 = ORIENTED_EDGE ( 'NONE', *, *, #84863, .F. ) ;
#34989 = CARTESIAN_POINT ( 'NONE',  ( -28.49999999999980105, 13.08746187583910725, 4.000000000000000000 ) ) ;
#34990 = DIRECTION ( 'NONE',  ( -0.7071067811865486830, -0.7071067811865464625, -0.000000000000000000 ) ) ;
#34991 = AXIS2_PLACEMENT_3D ( 'NONE', #21035, #109490, #54428 ) ;
#34992 = EDGE_LOOP ( 'NONE', ( #75728, #23561, #142727, #17805 ) ) ;
#34993 = LINE ( 'NONE', #58200, #129532 ) ;
#34994 = CARTESIAN_POINT ( 'NONE',  ( 25.40000000000000213, 6.668511817681099352, 3.138890638869527461 ) ) ;
#34995 = CARTESIAN_POINT ( 'NONE',  ( 51.48921356237309510, -27.52281430457091460, 5.000000000000000000 ) ) ;
#34996 = DIRECTION ( 'NONE',  ( -0.7071067811865486830, 0.7071067811865464625, 0.000000000000000000 ) ) ;
#34997 = CARTESIAN_POINT ( 'NONE',  ( 126.2920968585647614, -5.291415217122921177, 3.054999999999999272 ) ) ;
#34998 = MECHANICAL_DESIGN_GEOMETRIC_PRESENTATION_REPRESENTATION (  '', ( #69668 ), #44199 ) ;
#34999 = VERTEX_POINT ( 'NONE', #32605 ) ;
#35000 = LINE ( 'NONE', #113960, #136784 ) ;
#35001 = SURFACE_STYLE_FILL_AREA ( #98781 ) ;
#35002 = DIRECTION ( 'NONE',  ( -0.3543493200069162685, -0.000000000000000000, -0.9351131265310288487 ) ) ;
#35003 = CARTESIAN_POINT ( 'NONE',  ( 0.4921764442864913769, 7.017265639291151658, -2.933287722884923898 ) ) ;
#35004 = CARTESIAN_POINT ( 'NONE',  ( 19.49999999999986855, -20.94781430457061333, 5.000000000000000000 ) ) ;
#35005 = CARTESIAN_POINT ( 'NONE',  ( 16.44013779566152778, 3.061616997868387579E-16, -2.500000000000000444 ) ) ;
#35006 = DIRECTION ( 'NONE',  ( -1.000000000000000000, -1.224606353822377258E-16, -0.000000000000000000 ) ) ;
#35007 = CARTESIAN_POINT ( 'NONE',  ( 50.53752705046289861, -9.735942053221456900E-16, 7.949999999999998401 ) ) ;
#35008 = CARTESIAN_POINT ( 'NONE',  ( -32.99999999999977263, -21.84840872380827292, 2.849755605029529626 ) ) ;
#35009 = ADVANCED_FACE ( 'NONE', ( #84825 ), #10110, .T. ) ;
#35010 = CARTESIAN_POINT ( 'NONE',  ( 0.000000000000000000, 0.000000000000000000, 5.000000000000000000 ) ) ;
#35011 = AXIS2_PLACEMENT_3D ( 'NONE', #101895, #54844, #111329 ) ;
#35012 = ORIENTED_EDGE ( 'NONE', *, *, #43618, .T. ) ;
#35013 = ORIENTED_EDGE ( 'NONE', *, *, #83532, .T. ) ;
#35014 = CARTESIAN_POINT ( 'NONE',  ( 48.83333333333332860, -6.884901960086287964, 3.974999999999998312 ) ) ;
#35015 = EDGE_CURVE ( 'NONE', #136794, #89060, #86272, .T. ) ;
#35016 = FACE_OUTER_BOUND ( 'NONE', #98969, .T. ) ;
#35017 = EDGE_CURVE ( 'NONE', #142342, #20063, #30453, .T. ) ;
#35018 = VECTOR ( 'NONE', #133944, 1000.000000000000227 ) ;
#35019 = EDGE_LOOP ( 'NONE', ( #7167, #18923, #127586, #101175 ) ) ;
#35020 = AXIS2_PLACEMENT_3D ( 'NONE', #131766, #55635, #88985 ) ;
#35021 = EDGE_CURVE ( 'NONE', #137395, #3235, #29707, .T. ) ;
#35022 = DIRECTION ( 'NONE',  ( -0.3543493200069162685, -0.000000000000000000, -0.9351131265310288487 ) ) ;
#35023 = DIRECTION ( 'NONE',  ( 0.6830127018922180770, -0.6830127018922204085, -0.2588190451025213501 ) ) ;
#35024 = CARTESIAN_POINT ( 'NONE',  ( 35.00043019189810423, -3.055000000000002380, 5.291415217122920289 ) ) ;
#35026 = EDGE_CURVE ( 'NONE', #80827, #103460, #105641, .T. ) ;
#35025 = ORIENTED_EDGE ( 'NONE', *, *, #141179, .F. ) ;
#35027 = FACE_OUTER_BOUND ( 'NONE', #21893, .T. ) ;
#35028 = ORIENTED_EDGE ( 'NONE', *, *, #8932, .F. ) ;
#35029 = CARTESIAN_POINT ( 'NONE',  ( 28.82816939922333432, 12.75929247661558996, 4.000000000000000000 ) ) ;
#35030 = LINE ( 'NONE', #36435, #8323 ) ;
#35031 =( NAMED_UNIT ( * ) PLANE_ANGLE_UNIT ( ) SI_UNIT ( $, .RADIAN. ) );
#35032 = ADVANCED_FACE ( 'NONE', ( #19561 ), #6078, .T. ) ;
#35033 = CARTESIAN_POINT ( 'NONE',  ( -14.72063736826144087, 7.288814752023359489, 4.957798599204234158 ) ) ;
#35034 = ORIENTED_EDGE ( 'NONE', *, *, #135478, .T. ) ;
#35035 = EDGE_CURVE ( 'NONE', #90903, #87458, #65244, .T. ) ;
#35036 = DIRECTION ( 'NONE',  ( 0.5735764363510444941, 0.8191520442889929088, 0.000000000000000000 ) ) ;
#35037 = EDGE_LOOP ( 'NONE', ( #86121, #134701, #85816, #85504, #9042 ) ) ;
#35038 = FACE_OUTER_BOUND ( 'NONE', #43601, .T. ) ;
#35039 = CARTESIAN_POINT ( 'NONE',  ( -31.00193056682077497, -22.22500000000000142, 4.500000000000000888 ) ) ;
#35040 = DIRECTION ( 'NONE',  ( -0.6830127018922181881, 0.6830127018922202975, -0.2588190451025214056 ) ) ;
#35041 = CARTESIAN_POINT ( 'NONE',  ( 25.49999999999982236, -12.08601207473286543, -10.46905243149100251 ) ) ;
#35042 = AXIS2_PLACEMENT_3D ( 'NONE', #58022, #15165, #2874 ) ;
#35043 = EDGE_CURVE ( 'NONE', #23765, #32169, #109429, .T. ) ;
#35044 = VERTEX_POINT ( 'NONE', #67380 ) ;
#35045 = DIRECTION ( 'NONE',  ( -0.3543493200069162685, -0.000000000000000000, -0.9351131265310288487 ) ) ;
#35046 = CARTESIAN_POINT ( 'NONE',  ( 55.91209685856478018, 5.291415217122921177, -3.054999999999994831 ) ) ;
#35047 = PLANE ( 'NONE',  #41863 ) ;
#35048 = LINE ( 'NONE', #66942, #133485 ) ;
#35050 = ORIENTED_EDGE ( 'NONE', *, *, #28016, .T. ) ;
#35049 = CARTESIAN_POINT ( 'NONE',  ( -33.18398860626899705, 28.73617430169810305, 5.000000000000000000 ) ) ;
#35051 = ORIENTED_EDGE ( 'NONE', *, *, #82608, .F. ) ;
#35052 = DIRECTION ( 'NONE',  ( 0.7071067811865487940, 0.7071067811865463515, -0.000000000000000000 ) ) ;
#35053 = AXIS2_PLACEMENT_3D ( 'NONE', #106557, #71132, #94976 ) ;
#35054 = ORIENTED_EDGE ( 'NONE', *, *, #6792, .T. ) ;
#35055 = VECTOR ( 'NONE', #90325, 1000.000000000000000 ) ;
#35056 = AXIS2_PLACEMENT_3D ( 'NONE', #8251, #52498, #22005 ) ;
#35057 = PLANE ( 'NONE',  #46593 ) ;
#35058 = ORIENTED_EDGE ( 'NONE', *, *, #10689, .F. ) ;
#35059 = DIRECTION ( 'NONE',  ( 0.000000000000000000, 0.000000000000000000, 1.000000000000000000 ) ) ;
#35060 = DIRECTION ( 'NONE',  ( -0.7071067811865487940, 0.7071067811865463515, -0.000000000000000000 ) ) ;
#35061 = EDGE_CURVE ( 'NONE', #23219, #19313, #13657, .T. ) ;
#35062 = CIRCLE ( 'NONE', #81314, 9.500000000000000000 ) ;
#35063 = VECTOR ( 'NONE', #98265, 1000.000000000000227 ) ;
#35064 = STYLED_ITEM ( 'NONE', ( #46406 ), #65185 ) ;
#35065 = CONICAL_SURFACE ( 'NONE', #53567, 2.055000000000001048, 0.9599310885968758145 ) ;
#35066 = AXIS2_PLACEMENT_3D ( 'NONE', #77021, #64696, #21889 ) ;
#35067 = CARTESIAN_POINT ( 'NONE',  ( 1.042387978378689573, 0.3999999999999995781, 2.015694669338588429 ) ) ;
#35068 = FACE_BOUND ( 'NONE', #57070, .T. ) ;
#35069 = LINE ( 'NONE', #68419, #13270 ) ;
#35070 = DIRECTION ( 'NONE',  ( 0.7071067811865487940, -0.7071067811865463515, 0.000000000000000000 ) ) ;
#35071 = DIRECTION ( 'NONE',  ( 1.000000000000000000, 0.000000000000000000, 0.000000000000000000 ) ) ;
#35073 = ORIENTED_EDGE ( 'NONE', *, *, #84859, .F. ) ;
#35072 = DIRECTION ( 'NONE',  ( 0.7071067811865487940, 0.7071067811865463515, -0.000000000000000000 ) ) ;
#35074 = LINE ( 'NONE', #33643, #143532 ) ;
#35075 = VERTEX_POINT ( 'NONE', #132656 ) ;
#35076 = ORIENTED_EDGE ( 'NONE', *, *, #120715, .F. ) ;
#35077 = CARTESIAN_POINT ( 'NONE',  ( 76.47459685856476597, 1.637169565754164280, -6.109999999999996767 ) ) ;
#35078 = ORIENTED_EDGE ( 'NONE', *, *, #12027, .T. ) ;
#35079 = VECTOR ( 'NONE', #47573, 1000.000000000000000 ) ;
#35080 = CARTESIAN_POINT ( 'NONE',  ( -18.18398860626898994, 28.73617430169800002, 5.000000000000000000 ) ) ;
#35081 = EDGE_CURVE ( 'NONE', #32751, #98192, #119216, .T. ) ;
#35082 = VERTEX_POINT ( 'NONE', #134055 ) ;
#35083 = PLANE ( 'NONE',  #56013 ) ;
#35084 = CARTESIAN_POINT ( 'NONE',  ( 121.7500000000000000, -9.735942053221458872E-16, 7.950000000000000178 ) ) ;
#35085 = AXIS2_PLACEMENT_3D ( 'NONE', #50702, #95621, #128273 ) ;
#35086 = CARTESIAN_POINT ( 'NONE',  ( -32.99999999999976552, -16.44781430457067373, 5.000000000000000000 ) ) ;
#35087 = EDGE_CURVE ( 'NONE', #74042, #91540, #10799, .T. ) ;
#35088 = SURFACE_SIDE_STYLE ('',( #12579 ) ) ;
#35089 = CARTESIAN_POINT ( 'NONE',  ( 0.000000000000000000, 0.000000000000000000, 5.000000000000000000 ) ) ;
#35090 = AXIS2_PLACEMENT_3D ( 'NONE', #101207, #126355, #27041 ) ;
#35091 = DIRECTION ( 'NONE',  ( 0.7071067811865487940, 0.7071067811865463515, -0.000000000000000000 ) ) ;
#35092 = LINE ( 'NONE', #114738, #9215 ) ;
#35093 = ORIENTED_EDGE ( 'NONE', *, *, #116605, .T. ) ;
#35094 = ORIENTED_EDGE ( 'NONE', *, *, #123556, .F. ) ;
#35095 = AXIS2_PLACEMENT_3D ( 'NONE', #108557, #65128, #33231 ) ;
#35096 = DIRECTION ( 'NONE',  ( 0.6830127018922180770, -0.6830127018922204085, -0.2588190451025213501 ) ) ;
#35097 = CARTESIAN_POINT ( 'NONE',  ( -18.32816939922339472, -3.740707523384251942, 4.000000000000000000 ) ) ;
#35098 = EDGE_LOOP ( 'NONE', ( #96443, #41341, #19082, #125665 ) ) ;
#35099 = EDGE_LOOP ( 'NONE', ( #17282, #135994, #65781, #42920 ) ) ;
#35100 = ORIENTED_EDGE ( 'NONE', *, *, #89012, .T. ) ;
#35101 = ADVANCED_FACE ( 'NONE', ( #68122 ), #79718, .F. ) ;
#35102 = VECTOR ( 'NONE', #100909, 1000.000000000000000 ) ;
#35103 = CARTESIAN_POINT ( 'NONE',  ( 25.81293019189810778, -1.637169565754159617, -6.110000000000001208 ) ) ;
#35104 = VERTEX_POINT ( 'NONE', #134789 ) ;
#35105 = FACE_OUTER_BOUND ( 'NONE', #72174, .T. ) ;
#35106 = LINE ( 'NONE', #135823, #30804 ) ;
#35107 = CARTESIAN_POINT ( 'NONE',  ( 2.983736474768552860, -5.808823158059035485, -5.808823158059033709 ) ) ;
#35108 = DIRECTION ( 'NONE',  ( -0.000000000000000000, 0.3543493200069152138, -0.9351131265310292928 ) ) ;
#35109 = VERTEX_POINT ( 'NONE', #88415 ) ;
#35110 = DIRECTION ( 'NONE',  ( 0.7071067811865486830, -0.7071067811865464625, -0.000000000000000000 ) ) ;
#35111 = CARTESIAN_POINT ( 'NONE',  ( -63.48921356237309510, -27.52281430457099631, 5.000000000000000000 ) ) ;
#35112 = AXIS2_PLACEMENT_3D ( 'NONE', #56261, #25533, #133774 ) ;
#35113 = PLANE ( 'NONE',  #86815 ) ;
#35115 = ORIENTED_EDGE ( 'NONE', *, *, #50913, .F. ) ;
#35114 = FACE_OUTER_BOUND ( 'NONE', #127228, .T. ) ;
#35116 = VECTOR ( 'NONE', #34973, 999.9999999999998863 ) ;
#35117 = VERTEX_POINT ( 'NONE', #45635 ) ;
#35118 = DIRECTION ( 'NONE',  ( 0.000000000000000000, 0.000000000000000000, 1.000000000000000000 ) ) ;
#35119 = CARTESIAN_POINT ( 'NONE',  ( 16.27785539607886633, 4.584330080086930965E-16, 0.000000000000000000 ) ) ;
#35120 = ADVANCED_FACE ( 'NONE', ( #55067 ), #11507, .F. ) ;
#35121 = CARTESIAN_POINT ( 'NONE',  ( 31.49999999999977973, -4.912538124160700015, 4.000000000000000000 ) ) ;
#35122 = VERTEX_POINT ( 'NONE', #47097 ) ;
#35123 = CARTESIAN_POINT ( 'NONE',  ( -72.48921356237309510, -27.52281430457106026, 5.000000000000000000 ) ) ;
#35124 = EDGE_CURVE ( 'NONE', #94490, #49817, #78979, .T. ) ;
#35125 = VECTOR ( 'NONE', #83217, 1000.000000000000227 ) ;
#35126 = CARTESIAN_POINT ( 'NONE',  ( -22.49999999999984013, -19.53360074219753884, 5.000000000000000000 ) ) ;
#35127 = PLANE ( 'NONE',  #118086 ) ;
#35128 = DIRECTION ( 'NONE',  ( -0.000000000000000000, 0.000000000000000000, 1.000000000000000000 ) ) ;
#35129 = AXIS2_PLACEMENT_3D ( 'NONE', #52909, #76127, #131218 ) ;
#35130 = CARTESIAN_POINT ( 'NONE',  ( -12.69999999999998153, 0.000000000000000000, 0.000000000000000000 ) ) ;
#35131 = DIRECTION ( 'NONE',  ( -0.000000000000000000, -0.000000000000000000, -1.000000000000000000 ) ) ;
#35132 = DIRECTION ( 'NONE',  ( 1.000000000000000000, 0.000000000000000000, 0.000000000000000000 ) ) ;
#35134 = EDGE_CURVE ( 'NONE', #122112, #75931, #73926, .T. ) ;
#35133 = CARTESIAN_POINT ( 'NONE',  ( -5.700255128608413102, -27.71228299555201957, 4.000000000000000000 ) ) ;
#35135 = CARTESIAN_POINT ( 'NONE',  ( -32.29289321881323360, 2.259292476615690770, 5.000000000000000000 ) ) ;
#35136 = EDGE_LOOP ( 'NONE', ( #104426, #78643, #97443 ) ) ;
#35137 = ADVANCED_FACE ( 'NONE', ( #2052 ), #90549, .F. ) ;
#35138 = ORIENTED_EDGE ( 'NONE', *, *, #100972, .F. ) ;
#35139 = VECTOR ( 'NONE', #16764, 1000.000000000000000 ) ;
#35140 = SURFACE_STYLE_FILL_AREA ( #58351 ) ;
#35141 = CARTESIAN_POINT ( 'NONE',  ( -4.499999999999972466, 6.277155672890267546, -3.510561720658931684 ) ) ;
#35142 = DIRECTION ( 'NONE',  ( -0.000000000000000000, 0.000000000000000000, 1.000000000000000000 ) ) ;
#35143 = CARTESIAN_POINT ( 'NONE',  ( 65.26669371712957002, -7.949999999999998401, 2.130196079827423983 ) ) ;
#35144 = ORIENTED_EDGE ( 'NONE', *, *, #102065, .F. ) ;
#35145 = CARTESIAN_POINT ( 'NONE',  ( 24.18398860626899705, 28.73617430169804265, 5.000000000000000000 ) ) ;
#35146 = CARTESIAN_POINT ( 'NONE',  ( 32.99999999999977973, 1.931123077392167264, 4.000000000000000000 ) ) ;
#35147 = LINE ( 'NONE', #101076, #25918 ) ;
#35148 = VERTEX_POINT ( 'NONE', #68811 ) ;
#35149 = LINE ( 'NONE', #36547, #134439 ) ;
#35150 = LINE ( 'NONE', #34411, #121022 ) ;
#35151 = VECTOR ( 'NONE', #11345, 1000.000000000000000 ) ;
#35152 = VECTOR ( 'NONE', #82703, 1000.000000000000000 ) ;
#35153 = PLANE ( 'NONE',  #124614 ) ;
#35154 = CARTESIAN_POINT ( 'NONE',  ( 57.51626352523144448, -4.472830434245839371, 4.472830434245839371 ) ) ;
#35155 = ADVANCED_FACE ( 'NONE', ( #94088 ), #43192, .T. ) ;
#35156 = DIRECTION ( 'NONE',  ( 0.6830127018922181881, 0.6830127018922202975, -0.2588190451025214056 ) ) ;
#35157 = AXIS2_PLACEMENT_3D ( 'NONE', #40951, #64135, #75727 ) ;
#35158 = CIRCLE ( 'NONE', #102206, 2.500000000000000888 ) ;
#35159 = DIRECTION ( 'NONE',  ( 0.000000000000000000, -1.000000000000000000, 0.000000000000000000 ) ) ;
#35160 = CARTESIAN_POINT ( 'NONE',  ( -20.81601139373100295, 28.73617430169773002, 5.000000000000000000 ) ) ;
#35161 = ORIENTED_EDGE ( 'NONE', *, *, #48069, .T. ) ;
#35162 = LINE ( 'NONE', #44632, #120603 ) ;
#35163 = EDGE_LOOP ( 'NONE', ( #45454, #26347, #5081, #135934 ) ) ;
#35164 = VECTOR ( 'NONE', #123028, 1000.000000000000227 ) ;
#35165 = VECTOR ( 'NONE', #101277, 1000.000000000000000 ) ;
#35166 = FACE_OUTER_BOUND ( 'NONE', #138560, .T. ) ;
#35167 = VECTOR ( 'NONE', #49841, 1000.000000000000227 ) ;
#35168 = CYLINDRICAL_SURFACE ( 'NONE', #138782, 7.950000000000000178 ) ;
#35169 = DIRECTION ( 'NONE',  ( 0.7071067811865487940, -0.7071067811865463515, 0.000000000000000000 ) ) ;
#35170 = DIRECTION ( 'NONE',  ( -0.6830127018922181881, 0.6830127018922202975, -0.2588190451025214056 ) ) ;
#35171 = DIRECTION ( 'NONE',  ( -0.7071067811865487940, 0.7071067811865463515, -0.000000000000000000 ) ) ;
#35172 = PLANE ( 'NONE',  #52320 ) ;
#35173 = EDGE_LOOP ( 'NONE', ( #56787, #106694, #18224, #27931, #82472 ) ) ;
#35174 = ORIENTED_EDGE ( 'NONE', *, *, #136943, .F. ) ;
#35175 = LINE ( 'NONE', #103935, #39436 ) ;
#35176 = COLOUR_RGB ( '', 0.72549020, 0.75294118, 0.79215686) ;
#35177 = DIRECTION ( 'NONE',  ( -0.000000000000000000, -0.3543493200069152693, 0.9351131265310292928 ) ) ;
#35178 = LINE ( 'NONE', #101832, #131391 ) ;
#35179 = CARTESIAN_POINT ( 'NONE',  ( 77.95419371712955581, 6.884901960086283523, 3.975000000000002753 ) ) ;
#35180 = CARTESIAN_POINT ( 'NONE',  ( 15.48921356237309510, -27.52281430457066236, 5.000000000000000000 ) ) ;
#35181 = ADVANCED_FACE ( 'NONE', ( #105663 ), #17253, .T. ) ;
#35182 = CARTESIAN_POINT ( 'NONE',  ( 1.213219033033586136, 12.75929247661558996, 10.29404684609035492 ) ) ;
#35183 = ORIENTED_EDGE ( 'NONE', *, *, #75867, .F. ) ;
#35184 = CARTESIAN_POINT ( 'NONE',  ( 72.60416666666665719, 2.130196079827422206, 7.950000000000001954 ) ) ;
#35185 = FACE_OUTER_BOUND ( 'NONE', #65926, .T. ) ;
#35186 = EDGE_CURVE ( 'NONE', #120060, #77465, #136176, .T. ) ;
#35187 = DIRECTION ( 'NONE',  ( 0.7071067811865487940, 0.7071067811865463515, -0.000000000000000000 ) ) ;
#35188 = CARTESIAN_POINT ( 'NONE',  ( -51.48921356237309510, -27.52281430457091460, 5.000000000000000000 ) ) ;
#35189 = EDGE_LOOP ( 'NONE', ( #70584, #5601, #56491, #108282 ) ) ;
#35190 = EDGE_CURVE ( 'NONE', #106541, #82440, #48456, .T. ) ;
#35191 = EDGE_CURVE ( 'NONE', #103105, #56655, #25999, .T. ) ;
#35192 = VECTOR ( 'NONE', #27355, 1000.000000000000000 ) ;
#35193 = DIRECTION ( 'NONE',  ( 0.7071067811865487940, -0.7071067811865463515, 0.000000000000000000 ) ) ;
#35194 = VECTOR ( 'NONE', #64817, 1000.000000000000000 ) ;
#35195 = CARTESIAN_POINT ( 'NONE',  ( -2.510786437626908008, -27.52281430457053446, 5.000000000000000000 ) ) ;
#35196 = CARTESIAN_POINT ( 'NONE',  ( 68.25043019189810423, 3.055000000000002824, -5.291415217122919401 ) ) ;
#35197 = VECTOR ( 'NONE', #7046, 1000.000000000000227 ) ;
#35198 = ORIENTED_EDGE ( 'NONE', *, *, #59925, .F. ) ;
#35199 = ORIENTED_EDGE ( 'NONE', *, *, #60241, .F. ) ;
#35200 = VECTOR ( 'NONE', #96116, 1000.000000000000000 ) ;
#35201 = LINE ( 'NONE', #79445, #112386 ) ;
#35202 = FACE_OUTER_BOUND ( 'NONE', #16111, .T. ) ;
#35203 = EDGE_CURVE ( 'NONE', #131513, #71093, #110298, .T. ) ;
#35204 = CARTESIAN_POINT ( 'NONE',  ( -20.99999999999984368, -22.22500000000000142, 4.412002311790043763 ) ) ;
#35205 = EDGE_CURVE ( 'NONE', #133079, #103220, #61514, .T. ) ;
#35206 = DIRECTION ( 'NONE',  ( 0.7071067811865487940, 0.7071067811865463515, 0.000000000000000000 ) ) ;
#35208 = ORIENTED_EDGE ( 'NONE', *, *, #123890, .T. ) ;
#35207 = CARTESIAN_POINT ( 'NONE',  ( 86.45833333333332860, 3.974999999999997424, 6.884901960086288852 ) ) ;
#35209 = PLANE ( 'NONE',  #48415 ) ;
#35210 = DIRECTION ( 'NONE',  ( 0.3543493200069162685, -0.000000000000000000, -0.9351131265310288487 ) ) ;
#35211 = CARTESIAN_POINT ( 'NONE',  ( 0.7928932188134545367, 0.7592924766157086447, 5.000000000000000000 ) ) ;
#35212 = VECTOR ( 'NONE', #25765, 1000.000000000000000 ) ;
#35213 = CARTESIAN_POINT ( 'NONE',  ( -30.32816939922330945, -12.74070752338414891, 4.000000000000000000 ) ) ;
#35214 = ORIENTED_EDGE ( 'NONE', *, *, #116159, .T. ) ;
#35215 = EDGE_CURVE ( 'NONE', #20082, #63324, #50602, .T. ) ;
#35216 = ORIENTED_EDGE ( 'NONE', *, *, #122793, .T. ) ;
#35217 = CARTESIAN_POINT ( 'NONE',  ( 54.97959685856476852, 6.109999999999999432, 1.637169565754164280 ) ) ;
#35218 = ORIENTED_EDGE ( 'NONE', *, *, #36030, .T. ) ;
#35219 = CARTESIAN_POINT ( 'NONE',  ( 18.48921356237309510, -27.52281430457068367, 5.000000000000000000 ) ) ;
#35220 = LINE ( 'NONE', #56279, #43285 ) ;
#35221 = VECTOR ( 'NONE', #18753, 1000.000000000000000 ) ;
#35222 = FACE_OUTER_BOUND ( 'NONE', #101527, .T. ) ;
#35223 = CARTESIAN_POINT ( 'NONE',  ( 53.64583333333331439, 2.130196079827356037, -7.950000000000043698 ) ) ;
#35224 = ORIENTED_EDGE ( 'NONE', *, *, #37226, .F. ) ;
#35226 = EDGE_CURVE ( 'NONE', #20647, #82847, #9987, .T. ) ;
#35225 = VERTEX_POINT ( 'NONE', #82520 ) ;
#35227 = AXIS2_PLACEMENT_3D ( 'NONE', #140500, #129622, #9231 ) ;
#35228 = CARTESIAN_POINT ( 'NONE',  ( 24.09999999999999787, 9.521314400968980422E-16, 0.000000000000000000 ) ) ;
#35229 = CARTESIAN_POINT ( 'NONE',  ( -19.71993606672559096, -1.561048305595850838, -32.18456460708710409 ) ) ;
#35230 = ORIENTED_EDGE ( 'NONE', *, *, #60401, .F. ) ;
#35231 = CARTESIAN_POINT ( 'NONE',  ( -1.591674519009985467, -0.7407075233842770334, 14.76736230305380282 ) ) ;
#35232 = DIRECTION ( 'NONE',  ( 0.7071067811865487940, 0.7071067811865463515, 0.000000000000000000 ) ) ;
#35233 = EDGE_CURVE ( 'NONE', #52005, #10836, #125311, .T. ) ;
#35234 = LINE ( 'NONE', #22861, #58543 ) ;
#35235 = VECTOR ( 'NONE', #16739, 1000.000000000000227 ) ;
#35236 =( BOUNDED_CURVE ( )  B_SPLINE_CURVE ( 3, ( #56988, #112759, #57700, #101879 ),
 .UNSPECIFIED., .F., .T. ) 
 B_SPLINE_CURVE_WITH_KNOTS ( ( 4, 4 ),
 ( 1.500914606003787677, 1.515984175831967429 ),
 .UNSPECIFIED. ) 
 CURVE ( )  GEOMETRIC_REPRESENTATION_ITEM ( )  RATIONAL_B_SPLINE_CURVE ( ( 1.000000000000000000, 0.9999810757616318657, 0.9999810757616318657, 1.000000000000000000 ) ) 
 REPRESENTATION_ITEM ( '' )  );
#35237 = ORIENTED_EDGE ( 'NONE', *, *, #109620, .T. ) ;
#35238 = FACE_BOUND ( 'NONE', #66414, .T. ) ;
#35239 = DIRECTION ( 'NONE',  ( 0.5735764363510451602, 0.8191520442889924647, 0.000000000000000000 ) ) ;
#35240 = EDGE_CURVE ( 'NONE', #21068, #48074, #3795, .T. ) ;
#35241 = CARTESIAN_POINT ( 'NONE',  ( 1.179999999999999716, 6.391994993740215847, 10.00000000000000000 ) ) ;
#35242 = LINE ( 'NONE', #114191, #64432 ) ;
#35243 = EDGE_CURVE ( 'NONE', #37784, #112545, #59367, .T. ) ;
#35244 = LINE ( 'NONE', #36628, #119769 ) ;
#35245 = CARTESIAN_POINT ( 'NONE',  ( -10.82816939922345689, -2.240707523384257716, 4.000000000000000000 ) ) ;
#35247 = ADVANCED_FACE ( 'NONE', ( #37597 ), #70945, .F. ) ;
#35246 = DIRECTION ( 'NONE',  ( -1.000000000000000000, -1.238249065775561804E-31, 2.449293598294707400E-16 ) ) ;
#35248 = ORIENTED_EDGE ( 'NONE', *, *, #22202, .F. ) ;
#35249 = VERTEX_POINT ( 'NONE', #81842 ) ;
#35250 = CARTESIAN_POINT ( 'NONE',  ( 99.66209685856478018, -5.291415217122919401, 3.054999999999997939 ) ) ;
#35251 = ORIENTED_EDGE ( 'NONE', *, *, #129310, .T. ) ;
#35252 = DIRECTION ( 'NONE',  ( 0.7071067811865487940, -0.7071067811865463515, 0.000000000000000000 ) ) ;
#35253 = VERTEX_POINT ( 'NONE', #15773 ) ;
#35254 = CARTESIAN_POINT ( 'NONE',  ( 26.99999999999981881, -3.485240976185050243, -4.108735105802335141 ) ) ;
#35255 = MECHANICAL_DESIGN_GEOMETRIC_PRESENTATION_REPRESENTATION (  '', ( #32764 ), #72325 ) ;
#35256 = AXIS2_PLACEMENT_3D ( 'NONE', #44206, #55075, #99243 ) ;
#35257 = VECTOR ( 'NONE', #87617, 1000.000000000000000 ) ;
#35258 = CARTESIAN_POINT ( 'NONE',  ( 3.837472949537105826, 6.094999999999989981, -1.119633336120465690E-15 ) ) ;
#35259 =( GEOMETRIC_REPRESENTATION_CONTEXT ( 3 ) GLOBAL_UNCERTAINTY_ASSIGNED_CONTEXT ( ( #93945 ) ) GLOBAL_UNIT_ASSIGNED_CONTEXT ( ( #44005, #46170, #45455 ) ) REPRESENTATION_CONTEXT ( 'NONE', 'WORKASPACE' ) );
#35260 = VECTOR ( 'NONE', #102463, 1000.000000000000000 ) ;
#35261 = DIRECTION ( 'NONE',  ( 0.6830127018922181881, 0.6830127018922202975, -0.2588190451025214056 ) ) ;
#35262 = ORIENTED_EDGE ( 'NONE', *, *, #65668, .T. ) ;
#35263 = CARTESIAN_POINT ( 'NONE',  ( -37.82334089840004054, 5.259292476615672562, 15.86257073897106729 ) ) ;
#35264 = CARTESIAN_POINT ( 'NONE',  ( -20.67183060077632106, -3.740707523384244837, 4.000000000000000000 ) ) ;
#35265 = EDGE_CURVE ( 'NONE', #76165, #51777, #104236, .T. ) ;
#35266 = SURFACE_SIDE_STYLE ('',( #80196 ) ) ;
#35268 = CARTESIAN_POINT ( 'NONE',  ( -2.999999999999978240, 2.342191155542447500, -5.001666872980077727 ) ) ;
#35267 = LINE ( 'NONE', #102649, #41088 ) ;
#35269 = LINE ( 'NONE', #79509, #78616 ) ;
#35270 = AXIS2_PLACEMENT_3D ( 'NONE', #122885, #67839, #101121 ) ;
#35271 = AXIS2_PLACEMENT_3D ( 'NONE', #68360, #54602, #159 ) ;
#35272 =( GEOMETRIC_REPRESENTATION_CONTEXT ( 3 ) GLOBAL_UNCERTAINTY_ASSIGNED_CONTEXT ( ( #11181 ) ) GLOBAL_UNIT_ASSIGNED_CONTEXT ( ( #23420, #71063, #44514 ) ) REPRESENTATION_CONTEXT ( 'NONE', 'WORKASPACE' ) );
#35273 = DIRECTION ( 'NONE',  ( 0.000000000000000000, -1.000000000000000000, 0.000000000000000000 ) ) ;
#35274 = ORIENTED_EDGE ( 'NONE', *, *, #12746, .T. ) ;
#35275 = LINE ( 'NONE', #24357, #33423 ) ;
#35276 = CARTESIAN_POINT ( 'NONE',  ( 2.510786437626908008, -27.52281430457053446, 5.000000000000000000 ) ) ;
#35277 = EDGE_LOOP ( 'NONE', ( #125027, #134681, #137717, #129416 ) ) ;
#35278 = ORIENTED_EDGE ( 'NONE', *, *, #130147, .F. ) ;
#35279 = EDGE_CURVE ( 'NONE', #111457, #46699, #5635, .T. ) ;
#35280 = ORIENTED_EDGE ( 'NONE', *, *, #76529, .T. ) ;
#35281 = CARTESIAN_POINT ( 'NONE',  ( 52.20876352523143282, -7.482591942790329030E-16, 6.110000000000001208 ) ) ;
#35282 = ORIENTED_EDGE ( 'NONE', *, *, #132588, .F. ) ;
#35283 = DIRECTION ( 'NONE',  ( 0.000000000000000000, 0.000000000000000000, 1.000000000000000000 ) ) ;
#35284 = CARTESIAN_POINT ( 'NONE',  ( 7.483306282870440640, 6.094999999999991758, 1.633150327867687102 ) ) ;
#35285 = CARTESIAN_POINT ( 'NONE',  ( 88.08376352523144703, -6.110000000000001208, -3.741295971395164515E-16 ) ) ;
#35286 = CARTESIAN_POINT ( 'NONE',  ( -20.72174548431414465, 8.259292476615634371, 11.78515199841145744 ) ) ;
#35287 = ORIENTED_EDGE ( 'NONE', *, *, #2129, .F. ) ;
#35288 = CARTESIAN_POINT ( 'NONE',  ( -60.29974487139158867, -27.71228299555248142, 4.000000000000000000 ) ) ;
#35289 = ORIENTED_EDGE ( 'NONE', *, *, #120926, .F. ) ;
#35290 = DIRECTION ( 'NONE',  ( 0.000000000000000000, 0.000000000000000000, -1.000000000000000000 ) ) ;
#35291 = FACE_OUTER_BOUND ( 'NONE', #8439, .T. ) ;
#35292 = ORIENTED_EDGE ( 'NONE', *, *, #60290, .F. ) ;
#35293 = VECTOR ( 'NONE', #39171, 1000.000000000000227 ) ;
#35294 = CARTESIAN_POINT ( 'NONE',  ( -23.99451991528749062, 28.92564299267954908, 4.000000000000000000 ) ) ;
#35295 = CARTESIAN_POINT ( 'NONE',  ( 126.9329301918981088, 1.637169565754156730, 6.110000000000001208 ) ) ;
#35296 = ORIENTED_EDGE ( 'NONE', *, *, #137292, .F. ) ;
#35297 = FACE_OUTER_BOUND ( 'NONE', #120784, .T. ) ;
#35299 = VERTEX_POINT ( 'NONE', #52033 ) ;
#35298 = ADVANCED_FACE ( 'NONE', ( #117248 ), #122086, .T. ) ;
#35300 = EDGE_LOOP ( 'NONE', ( #52579, #117382, #40455, #7968 ) ) ;
#35301 = ORIENTED_EDGE ( 'NONE', *, *, #68463, .F. ) ;
#35302 = DIRECTION ( 'NONE',  ( -0.7071067811865487940, 0.7071067811865463515, -0.000000000000000000 ) ) ;
#35303 = VECTOR ( 'NONE', #138409, 1000.000000000000000 ) ;
#35304 = DIRECTION ( 'NONE',  ( -0.7071067811865486830, -0.7071067811865464625, 0.000000000000000000 ) ) ;
#35306 = EDGE_CURVE ( 'NONE', #26996, #86210, #119395, .T. ) ;
#35305 = LINE ( 'NONE', #79547, #121142 ) ;
#35307 = DIRECTION ( 'NONE',  ( 0.7071067811865487940, 0.7071067811865463515, 0.000000000000000000 ) ) ;
#35308 = EDGE_CURVE ( 'NONE', #93715, #64105, #138723, .T. ) ;
#35309 = CARTESIAN_POINT ( 'NONE',  ( -8.999999999999952038, 17.58746187583908238, 4.000000000000000000 ) ) ;
#35310 = ORIENTED_EDGE ( 'NONE', *, *, #133971, .T. ) ;
#35311 = VECTOR ( 'NONE', #78394, 1000.000000000000114 ) ;
#35312 = LINE ( 'NONE', #23685, #119076 ) ;
#35313 = CARTESIAN_POINT ( 'NONE',  ( 21.56206980810188512, -7.934999999999991616, -2.126176841940955242 ) ) ;
#35314 = CARTESIAN_POINT ( 'NONE',  ( -5.700255128608413102, -27.71228299555201957, 4.000000000000000000 ) ) ;
#35315 = CARTESIAN_POINT ( 'NONE',  ( -56.99451991528749062, 28.92564299267978001, 4.000000000000000000 ) ) ;
#35316 = ADVANCED_FACE ( 'NONE', ( #128862 ), #28855, .F. ) ;
#35317 = CARTESIAN_POINT ( 'NONE',  ( -33.18123773989405834, 22.27000000000001378, -14.20145869268583638 ) ) ;
#35318 = ORIENTED_EDGE ( 'NONE', *, *, #53692, .T. ) ;
#35319 = ORIENTED_EDGE ( 'NONE', *, *, #97449, .T. ) ;
#35320 = AXIS2_PLACEMENT_3D ( 'NONE', #87269, #55367, #107576 ) ;
#35321 = ORIENTED_EDGE ( 'NONE', *, *, #141882, .F. ) ;
#35322 = CARTESIAN_POINT ( 'NONE',  ( 33.48921356237309510, -27.52281430457078670, 5.000000000000000000 ) ) ;
#35323 = VECTOR ( 'NONE', #61411, 1000.000000000000000 ) ;
#35324 = DIRECTION ( 'NONE',  ( -0.7071067811865487940, 0.7071067811865463515, 0.000000000000000000 ) ) ;
#35325 = CARTESIAN_POINT ( 'NONE',  ( 24.79289321881329045, 0.7592924766157156391, 5.000000000000000000 ) ) ;
#35326 = DIRECTION ( 'NONE',  ( -0.000000000000000000, 0.000000000000000000, 1.000000000000000000 ) ) ;
#35327 = EDGE_CURVE ( 'NONE', #89438, #117423, #29539, .T. ) ;
#35328 = LINE ( 'NONE', #67972, #13629 ) ;
#35329 = DIRECTION ( 'NONE',  ( -0.7071067811865487940, 0.7071067811865463515, 0.000000000000000000 ) ) ;
#35330 = PLANE ( 'NONE',  #81425 ) ;
#35331 = CARTESIAN_POINT ( 'NONE',  ( 19.88840764549667384, 9.139736423841732040E-16, 0.000000000000000000 ) ) ;
#35332 = FACE_OUTER_BOUND ( 'NONE', #141339, .T. ) ;
#35333 = VERTEX_POINT ( 'NONE', #96214 ) ;
#35334 = EDGE_CURVE ( 'NONE', #84329, #88412, #53455, .T. ) ;
#35335 = COLOUR_RGB ( '', 0.40784314, 0.44705882, 0.49803922) ;
#35336 = FILL_AREA_STYLE ('',( #135357 ) ) ;
#35337 = VERTEX_POINT ( 'NONE', #107107 ) ;
#35338 = CARTESIAN_POINT ( 'NONE',  ( 60.48921356237309510, -27.52281430457097500, 5.000000000000000000 ) ) ;
#35340 = ORIENTED_EDGE ( 'NONE', *, *, #121511, .T. ) ;
#35339 = LINE ( 'NONE', #81701, #53344 ) ;
#35341 = CARTESIAN_POINT ( 'NONE',  ( -54.48921356237310221, -27.52281430457093236, 5.000000000000000000 ) ) ;
#35342 = DIRECTION ( 'NONE',  ( -0.7071067811865486830, -0.7071067811865464625, 0.000000000000000000 ) ) ;
#35343 = EDGE_LOOP ( 'NONE', ( #58011, #18955, #81950, #33091 ) ) ;
#35344 = DIRECTION ( 'NONE',  ( -0.000000000000000000, -0.3543493200069152693, 0.9351131265310292928 ) ) ;
#35346 = VERTEX_POINT ( 'NONE', #7047 ) ;
#35345 = VECTOR ( 'NONE', #74774, 1000.000000000000000 ) ;
#35347 = FACE_OUTER_BOUND ( 'NONE', #25243, .T. ) ;
#35348 = ORIENTED_EDGE ( 'NONE', *, *, #252, .F. ) ;
#35349 = LINE ( 'NONE', #131783, #33731 ) ;
#35350 = CARTESIAN_POINT ( 'NONE',  ( 105.2250270504628986, 5.819803920172573086, -5.819803920172572198 ) ) ;
#35351 = DIRECTION ( 'NONE',  ( -0.000000000000000000, 0.3543493200069153248, 0.9351131265310292928 ) ) ;
#35352 = ORIENTED_EDGE ( 'NONE', *, *, #80849, .F. ) ;
#35353 = CARTESIAN_POINT ( 'NONE',  ( -33.29974487139158867, -27.71228299555229313, 4.000000000000000000 ) ) ;
#35355 = EDGE_CURVE ( 'NONE', #104658, #28238, #51327, .T. ) ;
#35354 = CARTESIAN_POINT ( 'NONE',  ( 2.999999999999999112, 0.000000000000000000, 2.500000000000000000 ) ) ;
#35356 = DIRECTION ( 'NONE',  ( -0.3543493200069162685, -0.000000000000000000, -0.9351131265310288487 ) ) ;
#35357 = CARTESIAN_POINT ( 'NONE',  ( 15.02083333333333570, -6.094999999999989981, -1.633150327867689100 ) ) ;
#35358 = LINE ( 'NONE', #56415, #58449 ) ;
#35359 = VECTOR ( 'NONE', #108541, 1000.000000000000000 ) ;
#35360 = VECTOR ( 'NONE', #64711, 1000.000000000000000 ) ;
#35362 = LINE ( 'NONE', #12837, #109255 ) ;
#35361 = AXIS2_PLACEMENT_3D ( 'NONE', #52490, #129333, #4106 ) ;
#35363 = CARTESIAN_POINT ( 'NONE',  ( -29.28769006033951783, -21.73547319004780931, 4.999917730833664642 ) ) ;
#35364 = EDGE_LOOP ( 'NONE', ( #92721, #68807, #59020, #66938, #54156 ) ) ;
#35365 = EDGE_CURVE ( 'NONE', #95118, #97786, #17928, .T. ) ;
#35367 = ADVANCED_FACE ( 'NONE', ( #18657 ), #11892, .F. ) ;
#35366 = VECTOR ( 'NONE', #41682, 1000.000000000000000 ) ;
#35368 = STYLED_ITEM ( 'NONE', ( #118843 ), #16183 ) ;
#35369 = DIRECTION ( 'NONE',  ( 0.7071067811865486830, -0.7071067811865464625, -0.000000000000000000 ) ) ;
#35370 = ORIENTED_EDGE ( 'NONE', *, *, #102664, .T. ) ;
#35371 = CARTESIAN_POINT ( 'NONE',  ( 92.89626352523143282, 4.472830434245840259, -4.472830434245839371 ) ) ;
#35372 = CARTESIAN_POINT ( 'NONE',  ( -27.29974487139158512, -27.71228299555225405, 4.000000000000000000 ) ) ;
#35373 = VECTOR ( 'NONE', #41408, 1000.000000000000000 ) ;
#35375 = AXIS2_PLACEMENT_3D ( 'NONE', #69051, #36407, #113232 ) ;
#35374 = PLANE ( 'NONE',  #44706 ) ;
#35376 = COLOUR_RGB ( '', 0.66274510, 0.83137255, 0.94901961) ;
#35377 = CARTESIAN_POINT ( 'NONE',  ( 32.99999999999977263, 20.70535890316564220, 1.956823837851840775 ) ) ;
#35378 = EDGE_LOOP ( 'NONE', ( #1026, #100507, #139416, #102264 ) ) ;
#35379 = ADVANCED_FACE ( 'NONE', ( #95516 ), #107809, .F. ) ;
#35380 = SURFACE_SIDE_STYLE ('',( #78873 ) ) ;
#35381 = DIRECTION ( 'NONE',  ( 0.5735764363510448272, -0.8191520442889927978, 1.003171929053526103E-16 ) ) ;
#35382 = EDGE_CURVE ( 'NONE', #39036, #73921, #44591, .T. ) ;
#35383 = ORIENTED_EDGE ( 'NONE', *, *, #15872, .F. ) ;
#35384 = LINE ( 'NONE', #135401, #60134 ) ;
#35385 = EDGE_CURVE ( 'NONE', #53474, #18032, #56182, .T. ) ;
#35387 = EDGE_LOOP ( 'NONE', ( #67695, #123178, #115947, #138924 ) ) ;
#35386 = DIRECTION ( 'NONE',  ( -0.6830127018922180770, -0.6830127018922204085, -0.2588190451025213501 ) ) ;
#35388 = CARTESIAN_POINT ( 'NONE',  ( 78.18398860626899705, 28.73617430169841924, 5.000000000000000000 ) ) ;
#35389 = CARTESIAN_POINT ( 'NONE',  ( 102.1625270504628844, 7.949999999999998401, 1.460391307983218338E-15 ) ) ;
#35390 = DIRECTION ( 'NONE',  ( -0.7071067811865487940, 0.7071067811865463515, 0.000000000000000000 ) ) ;
#35391 = CARTESIAN_POINT ( 'NONE',  ( -60.48921356237309510, -27.52281430457097500, 5.000000000000000000 ) ) ;
#35392 = CARTESIAN_POINT ( 'NONE',  ( 6.852250093007166143, 4.584330080086930965E-16, 0.000000000000000000 ) ) ;
#35393 = ORIENTED_EDGE ( 'NONE', *, *, #40069, .T. ) ;
#35394 = EDGE_LOOP ( 'NONE', ( #47353, #101206, #42177, #20403 ) ) ;
#35395 = ORIENTED_EDGE ( 'NONE', *, *, #19898, .T. ) ;
#35397 = ADVANCED_FACE ( 'NONE', ( #20088 ), #64336, .F. ) ;
#35396 = CARTESIAN_POINT ( 'NONE',  ( 83.12543019189810423, 5.291415217122919401, 3.055000000000002824 ) ) ;
#35398 = VECTOR ( 'NONE', #99648, 1000.000000000000000 ) ;
#35399 = ORIENTED_EDGE ( 'NONE', *, *, #65602, .F. ) ;
#35400 = ADVANCED_FACE ( 'NONE', ( #7783 ), #139046, .F. ) ;
#35401 = CARTESIAN_POINT ( 'NONE',  ( 69.29974487139159578, -27.71228299555254537, 4.000000000000000000 ) ) ;
#35402 = DIRECTION ( 'NONE',  ( 0.7071067811865487940, 0.7071067811865463515, -0.000000000000000000 ) ) ;
#35403 = CARTESIAN_POINT ( 'NONE',  ( 34.49999999999975842, 16.46425560840032531, 4.994342998332160555 ) ) ;
#35404 = CARTESIAN_POINT ( 'NONE',  ( -11.51078643762690490, -27.52281430457047406, 5.000000000000000000 ) ) ;
#35405 = ORIENTED_EDGE ( 'NONE', *, *, #108121, .F. ) ;
#35406 = EDGE_CURVE ( 'NONE', #20788, #97211, #133014, .T. ) ;
#35407 = CARTESIAN_POINT ( 'NONE',  ( 103.0833333333333286, 6.884901960086290629, -3.974999999999994316 ) ) ;
#35408 = DIRECTION ( 'NONE',  ( -0.7071067811865487940, 0.7071067811865463515, -0.000000000000000000 ) ) ;
#35409 = VECTOR ( 'NONE', #74674, 1000.000000000000227 ) ;
#35410 = LINE ( 'NONE', #47024, #83590 ) ;
#35411 = CARTESIAN_POINT ( 'NONE',  ( 88.87043019189810877, -3.055000000000001492, 5.291415217122917625 ) ) ;
#35412 = VERTEX_POINT ( 'NONE', #73780 ) ;
#35413 = COLOUR_RGB ( '', 0.31764706, 0.68627451, 0.89019608) ;
#35414 = LINE ( 'NONE', #91885, #16509 ) ;
#35415 = EDGE_CURVE ( 'NONE', #3888, #72508, #91619, .T. ) ;
#35417 = AXIS2_PLACEMENT_3D ( 'NONE', #50338, #130037, #118425 ) ;
#35416 = CARTESIAN_POINT ( 'NONE',  ( 3.707106781186523481, 20.25929247661551713, 5.000000000000000000 ) ) ;
#35418 = VECTOR ( 'NONE', #33943, 1000.000000000000000 ) ;
#35419 = VERTEX_POINT ( 'NONE', #135839 ) ;
#35420 = VERTEX_POINT ( 'NONE', #124244 ) ;
#35421 = LINE ( 'NONE', #112238, #39911 ) ;
#35422 = CARTESIAN_POINT ( 'NONE',  ( 25.39999999999999858, 0.000000000000000000, 0.000000000000000000 ) ) ;
#35423 = FACE_BOUND ( 'NONE', #107494, .T. ) ;
#35424 = EDGE_CURVE ( 'NONE', #82359, #60304, #37238, .T. ) ;
#35425 = CARTESIAN_POINT ( 'NONE',  ( 19.89359858452208130, -2.055000000000000160, 2.789133085058097101E-16 ) ) ;
#35426 = CARTESIAN_POINT ( 'NONE',  ( -11.99999999999992006, 10.21212019023808004, -2.019456568337770985 ) ) ;
#35427 = VECTOR ( 'NONE', #97888, 1000.000000000000227 ) ;
#35428 = PLANE ( 'NONE',  #65943 ) ;
#35430 = EDGE_CURVE ( 'NONE', #86472, #20317, #90178, .T. ) ;
#35429 = SURFACE_SIDE_STYLE ('',( #46306 ) ) ;
#35431 = ORIENTED_EDGE ( 'NONE', *, *, #99554, .F. ) ;
#35432 = ORIENTED_EDGE ( 'NONE', *, *, #7291, .T. ) ;
#35433 = DIRECTION ( 'NONE',  ( -0.000000000000000000, 0.000000000000000000, 1.000000000000000000 ) ) ;
#35434 = ORIENTED_EDGE ( 'NONE', *, *, #28033, .F. ) ;
#35435 = ORIENTED_EDGE ( 'NONE', *, *, #47132, .F. ) ;
#35436 = VECTOR ( 'NONE', #39327, 1000.000000000000000 ) ;
#35437 = AXIS2_PLACEMENT_3D ( 'NONE', #117329, #58759, #61583 ) ;
#35438 = EDGE_CURVE ( 'NONE', #6466, #12348, #13316, .T. ) ;
#35439 = LINE ( 'NONE', #123142, #17264 ) ;
#35440 = ORIENTED_EDGE ( 'NONE', *, *, #124506, .F. ) ;
#35441 = DIRECTION ( 'NONE',  ( 1.000000000000000000, 0.000000000000000000, 0.000000000000000000 ) ) ;
#35442 = LINE ( 'NONE', #81064, #84207 ) ;
#35443 = DIRECTION ( 'NONE',  ( -0.3543493200069163240, 4.681814790819596721E-17, -0.9351131265310288487 ) ) ;
#35444 = CARTESIAN_POINT ( 'NONE',  ( -8.700255128608413102, -27.71228299555199825, 4.000000000000000000 ) ) ;
#35445 = VECTOR ( 'NONE', #54832, 999.9999999999998863 ) ;
#35446 = CARTESIAN_POINT ( 'NONE',  ( -23.99999999999982947, 14.96639925780211122, 5.000000000000000000 ) ) ;
#35447 = ORIENTED_EDGE ( 'NONE', *, *, #21569, .F. ) ;
#35448 = DIRECTION ( 'NONE',  ( 0.3543493200069162685, -0.000000000000000000, -0.9351131265310288487 ) ) ;
#35449 = ORIENTED_EDGE ( 'NONE', *, *, #127599, .T. ) ;
#35450 = CARTESIAN_POINT ( 'NONE',  ( 1.499999999999987566, -4.796895815301019717, -3.611700055028677525 ) ) ;
#35451 = ORIENTED_EDGE ( 'NONE', *, *, #72395, .T. ) ;
#35452 = LINE ( 'NONE', #133317, #21367 ) ;
#35453 = ORIENTED_EDGE ( 'NONE', *, *, #3332, .T. ) ;
#35454 = FACE_OUTER_BOUND ( 'NONE', #111694, .T. ) ;
#35455 = ORIENTED_EDGE ( 'NONE', *, *, #62059, .F. ) ;
#35456 = ORIENTED_EDGE ( 'NONE', *, *, #29243, .T. ) ;
#35457 = ORIENTED_EDGE ( 'NONE', *, *, #93272, .T. ) ;
#35458 = DIRECTION ( 'NONE',  ( 1.000000000000000000, -0.000000000000000000, -0.000000000000000000 ) ) ;
#35459 = DIRECTION ( 'NONE',  ( -1.000000000000000000, -1.224606353822377258E-16, -0.000000000000000000 ) ) ;
#35460 = CARTESIAN_POINT ( 'NONE',  ( 122.3545968585647614, -1.637169565754161615, 6.110000000000000320 ) ) ;
#35461 = DIRECTION ( 'NONE',  ( 0.6830127018922180770, -0.6830127018922204085, -0.2588190451025213501 ) ) ;
#35462 = ADVANCED_FACE ( 'NONE', ( #134425 ), #133706, .F. ) ;
#35463 = PLANE ( 'NONE',  #92207 ) ;
#35465 = DIRECTION ( 'NONE',  ( 0.7071067811865486830, -0.7071067811865464625, -0.000000000000000000 ) ) ;
#35464 = LINE ( 'NONE', #123886, #99108 ) ;
#35466 = AXIS2_PLACEMENT_3D ( 'NONE', #125344, #92688, #24587 ) ;
#35467 = DIRECTION ( 'NONE',  ( -0.000000000000000000, 0.000000000000000000, 1.000000000000000000 ) ) ;
#35468 = VECTOR ( 'NONE', #98045, 1000.000000000000114 ) ;
#35469 = AXIS2_PLACEMENT_3D ( 'NONE', #103168, #79332, #25596 ) ;
#35470 =( LENGTH_UNIT ( ) NAMED_UNIT ( * ) SI_UNIT ( .MILLI., .METRE. ) );
#35471 = VERTEX_POINT ( 'NONE', #46000 ) ;
#35472 = SURFACE_STYLE_FILL_AREA ( #134780 ) ;
#35473 = DIRECTION ( 'NONE',  ( 0.7071067811865487940, 0.7071067811865463515, 0.000000000000000000 ) ) ;
#35474 = CARTESIAN_POINT ( 'NONE',  ( 0.000000000000000000, 0.000000000000000000, 5.000000000000000000 ) ) ;
#35475 = EDGE_LOOP ( 'NONE', ( #26296, #133001, #95211, #59875 ) ) ;
#35476 = EDGE_LOOP ( 'NONE', ( #18647, #28386, #48076, #98387 ) ) ;
#35477 = AXIS2_PLACEMENT_3D ( 'NONE', #109779, #997, #22733 ) ;
#35478 = AXIS2_PLACEMENT_3D ( 'NONE', #133620, #114692, #124160 ) ;
#35479 = STYLED_ITEM ( 'NONE', ( #85290 ), #53301 ) ;
#35480 = DIRECTION ( 'NONE',  ( -0.000000000000000000, -0.000000000000000000, -1.000000000000000000 ) ) ;
#35481 = ORIENTED_EDGE ( 'NONE', *, *, #71725, .F. ) ;
#35482 = ADVANCED_FACE ( 'NONE', ( #114766 ), #12616, .T. ) ;
#35483 = DIRECTION ( 'NONE',  ( 0.7071067811865487940, -0.7071067811865463515, 0.000000000000000000 ) ) ;
#35484 = DIRECTION ( 'NONE',  ( -0.6830127018922180770, -0.6830127018922204085, -0.2588190451025213501 ) ) ;
#35485 = ADVANCED_FACE ( 'NONE', ( #90929 ), #24229, .F. ) ;
#35486 = CARTESIAN_POINT ( 'NONE',  ( 8.207106781186492839, 0.7592924766157086447, 5.000000000000000000 ) ) ;
#35487 = ORIENTED_EDGE ( 'NONE', *, *, #44194, .T. ) ;
#35488 = DIRECTION ( 'NONE',  ( -0.7071067811865486830, -0.7071067811865464625, 0.000000000000000000 ) ) ;
#35489 = VERTEX_POINT ( 'NONE', #112654 ) ;
#35491 = ADVANCED_FACE ( 'NONE', ( #69912 ), #24920, .F. ) ;
#35490 = DIRECTION ( 'NONE',  ( 0.7071067811865486830, -0.7071067811865464625, -0.000000000000000000 ) ) ;
#35492 = EDGE_CURVE ( 'NONE', #58967, #84831, #35852, .T. ) ;
#35493 = VECTOR ( 'NONE', #19780, 1000.000000000000000 ) ;
#35494 = CARTESIAN_POINT ( 'NONE',  ( 31.27540314143522693, -2.126176841940958351, -7.934999999999989839 ) ) ;
#35495 = ORIENTED_EDGE ( 'NONE', *, *, #775, .T. ) ;
#35496 = CARTESIAN_POINT ( 'NONE',  ( 82.16209685856479439, -5.291415217122919401, 3.054999999999998384 ) ) ;
#35497 = CARTESIAN_POINT ( 'NONE',  ( 5.292893218813420120, 14.25929247661557753, 5.000000000000000000 ) ) ;
#35498 = EDGE_CURVE ( 'NONE', #29089, #139138, #2434, .T. ) ;
#35499 = CARTESIAN_POINT ( 'NONE',  ( 97.78752705046289861, 0.000000000000000000, -7.949999999999998401 ) ) ;
#35500 = VERTEX_POINT ( 'NONE', #34385 ) ;
#35501 = EDGE_LOOP ( 'NONE', ( #69491, #82081, #132152, #30671, #33362 ) ) ;
#35502 = EDGE_LOOP ( 'NONE', ( #97350, #2196, #38409, #102602, #82874 ) ) ;
#35503 = CARTESIAN_POINT ( 'NONE',  ( 0.4000000000000001887, 1.530808498934154593E-16, 1.249999999999969802 ) ) ;
#35504 = DIRECTION ( 'NONE',  ( 0.7071067811865487940, 0.7071067811865463515, 0.000000000000000000 ) ) ;
#35505 = CARTESIAN_POINT ( 'NONE',  ( -32.99999999999976552, 1.931123077392167264, 4.000000000000000000 ) ) ;
#35506 = CARTESIAN_POINT ( 'NONE',  ( 0.000000000000000000, 0.000000000000000000, 5.000000000000000000 ) ) ;
#35507 = EDGE_LOOP ( 'NONE', ( #13244, #20762, #100338, #39378 ) ) ;
#35508 = VECTOR ( 'NONE', #24378, 1000.000000000000227 ) ;
#35509 = DIRECTION ( 'NONE',  ( 0.7071067811865487940, 0.7071067811865463515, -0.000000000000000000 ) ) ;
#35510 = EDGE_CURVE ( 'NONE', #66568, #91210, #58334, .T. ) ;
#35511 = AXIS2_PLACEMENT_3D ( 'NONE', #124947, #14765, #67766 ) ;
#35512 = FACE_OUTER_BOUND ( 'NONE', #87613, .T. ) ;
#35513 = PLANE ( 'NONE',  #130216 ) ;
#35514 = ORIENTED_EDGE ( 'NONE', *, *, #112612, .F. ) ;
#35515 = ADVANCED_FACE ( 'NONE', ( #45295 ), #59044, .F. ) ;
#35516 = CYLINDRICAL_SURFACE ( 'NONE', #63303, 0.5000000000000004441 ) ;
#35517 = ORIENTED_EDGE ( 'NONE', *, *, #93089, .F. ) ;
#35518 = VECTOR ( 'NONE', #56193, 1000.000000000000227 ) ;
#35520 = VERTEX_POINT ( 'NONE', #78604 ) ;
#35519 = CARTESIAN_POINT ( 'NONE',  ( 58.16711163708656329, -46.44928942427644358, -35.85226645763125219 ) ) ;
#35521 = EDGE_LOOP ( 'NONE', ( #34530, #99856, #58927 ) ) ;
#35522 = CYLINDRICAL_SURFACE ( 'NONE', #116412, 0.5000000000000000000 ) ;
#35523 = FACE_OUTER_BOUND ( 'NONE', #37803, .T. ) ;
#35524 = ADVANCED_FACE ( 'NONE', ( #5992 ), #72777, .F. ) ;
#35525 = EDGE_LOOP ( 'NONE', ( #37343, #65284, #138302, #95868 ) ) ;
#35527 = EDGE_CURVE ( 'NONE', #30609, #93966, #35220, .T. ) ;
#35526 = CARTESIAN_POINT ( 'NONE',  ( 29.99451991528749417, 28.92564299267958816, 4.000000000000000000 ) ) ;
#35528 = ORIENTED_EDGE ( 'NONE', *, *, #76881, .F. ) ;
#35529 = CARTESIAN_POINT ( 'NONE',  ( 1.301042606982605321E-15, -21.03360074219752462, 5.000000000000000000 ) ) ;
#35530 = CARTESIAN_POINT ( 'NONE',  ( -30.29974487139158867, -27.71228299555227537, 4.000000000000000000 ) ) ;
#35532 = VECTOR ( 'NONE', #91635, 1000.000000000000000 ) ;
#35531 = LINE ( 'NONE', #124635, #73960 ) ;
#35533 = CARTESIAN_POINT ( 'NONE',  ( 32.99999999999977263, -10.77435723561691994, -9.972017380717304036 ) ) ;
#35534 = PLANE ( 'NONE',  #2550 ) ;
#35535 = DIRECTION ( 'NONE',  ( -0.000000000000000000, 1.000000000000000000, -0.000000000000000000 ) ) ;
#35537 = ADVANCED_FACE ( 'NONE', ( #24316 ), #89624, .T. ) ;
#35536 = CARTESIAN_POINT ( 'NONE',  ( -25.49999999999981526, -4.912538124160705344, 4.000000000000000000 ) ) ;
#35538 = LINE ( 'NONE', #13006, #131747 ) ;
#35539 = CARTESIAN_POINT ( 'NONE',  ( 21.56206980810188512, -7.934999999999991616, -2.126176841940955242 ) ) ;
#35540 = LINE ( 'NONE', #80452, #81503 ) ;
#35541 = CARTESIAN_POINT ( 'NONE',  ( 0.000000000000000000, 0.000000000000000000, 5.000000000000000000 ) ) ;
#35542 = FACE_OUTER_BOUND ( 'NONE', #58562, .T. ) ;
#35543 = DIRECTION ( 'NONE',  ( 1.000000000000000000, 0.000000000000000000, 0.000000000000000000 ) ) ;
#35544 = EDGE_LOOP ( 'NONE', ( #104207, #86017, #91465, #57168 ) ) ;
#35546 = ORIENTED_EDGE ( 'NONE', *, *, #43837, .T. ) ;
#35545 = EDGE_CURVE ( 'NONE', #53228, #7053, #90271, .T. ) ;
#35547 = EDGE_CURVE ( 'NONE', #141465, #73316, #20171, .T. ) ;
#35548 = CARTESIAN_POINT ( 'NONE',  ( 92.00000000000000000, 0.000000000000000000, -7.950000000000000178 ) ) ;
#35549 = EDGE_LOOP ( 'NONE', ( #744, #68169, #1271, #98429 ) ) ;
#35550 = ORIENTED_EDGE ( 'NONE', *, *, #118263, .T. ) ;
#35551 = EDGE_CURVE ( 'NONE', #121120, #20950, #22437, .T. ) ;
#35552 = EDGE_LOOP ( 'NONE', ( #103122, #77110, #55223, #104043 ) ) ;
#35553 = CARTESIAN_POINT ( 'NONE',  ( 2.999999999999980016, -15.03360074219758680, 5.000000000000000000 ) ) ;
#35554 = CARTESIAN_POINT ( 'NONE',  ( 0.000000000000000000, 0.000000000000000000, 0.000000000000000000 ) ) ;
#35555 = CARTESIAN_POINT ( 'NONE',  ( 14.11365817810131240, 9.243498355973924774, 2.206088284637460983 ) ) ;
#35556 = ORIENTED_EDGE ( 'NONE', *, *, #89113, .T. ) ;
#35557 = DIRECTION ( 'NONE',  ( -0.7071067811865487940, 0.7071067811865463515, 0.000000000000000000 ) ) ;
#35558 = EDGE_CURVE ( 'NONE', #22536, #54738, #77998, .T. ) ;
#35559 = CARTESIAN_POINT ( 'NONE',  ( -11.51078643762690490, -27.52281430457047406, 5.000000000000000000 ) ) ;
#35560 = LINE ( 'NONE', #23938, #115821 ) ;
#35561 = CARTESIAN_POINT ( 'NONE',  ( 126.0875899665068403, 5.292509191841936023, -5.124245105880927298 ) ) ;
#35562 = EDGE_CURVE ( 'NONE', #109374, #26207, #79463, .T. ) ;
#35563 = DIRECTION ( 'NONE',  ( 0.7071067811865487940, 0.7071067811865463515, -0.000000000000000000 ) ) ;
#35564 = PLANE ( 'NONE',  #84069 ) ;
#35566 = CIRCLE ( 'NONE', #40213, 9.524999999999991473 ) ;
#35565 = DIRECTION ( 'NONE',  ( 1.000000000000000000, 0.000000000000000000, 0.000000000000000000 ) ) ;
#35567 = CARTESIAN_POINT ( 'NONE',  ( 6.183988606268994381, 28.73617430169791476, 5.000000000000000000 ) ) ;
#35568 = CARTESIAN_POINT ( 'NONE',  ( 26.99999999999999645, 5.837062628940091535, 2.500239961634333596 ) ) ;
#35569 = DIRECTION ( 'NONE',  ( 0.000000000000000000, -1.000000000000000000, 0.000000000000000000 ) ) ;
#35570 = DIRECTION ( 'NONE',  ( 0.7071067811865487940, 0.7071067811865463515, -0.000000000000000000 ) ) ;
#35571 = CARTESIAN_POINT ( 'NONE',  ( 9.994118527364397764, 4.584330080086930965E-16, 0.000000000000000000 ) ) ;
#35572 = DIRECTION ( 'NONE',  ( 0.000000000000000000, -1.000000000000000000, 0.000000000000000000 ) ) ;
#35573 = ORIENTED_EDGE ( 'NONE', *, *, #3055, .T. ) ;
#35574 = VERTEX_POINT ( 'NONE', #58426 ) ;
#35575 = CARTESIAN_POINT ( 'NONE',  ( 113.8962635252314328, 4.472830434245840259, -4.472830434245839371 ) ) ;
#35576 = VECTOR ( 'NONE', #109948, 1000.000000000000000 ) ;
#35577 = ORIENTED_EDGE ( 'NONE', *, *, #38789, .F. ) ;
#35578 = EDGE_CURVE ( 'NONE', #133129, #63294, #3256, .T. ) ;
#35579 = CARTESIAN_POINT ( 'NONE',  ( 100.1666666666666714, 6.884901960086285300, 3.975000000000003642 ) ) ;
#35580 =( LENGTH_UNIT ( ) NAMED_UNIT ( * ) SI_UNIT ( .MILLI., .METRE. ) );
#35581 = EDGE_CURVE ( 'NONE', #86059, #66739, #25008, .T. ) ;
#35582 = PLANE ( 'NONE',  #51452 ) ;
#35584 = VECTOR ( 'NONE', #52180, 1000.000000000000000 ) ;
#35583 = LINE ( 'NONE', #58044, #32779 ) ;
#35585 = CARTESIAN_POINT ( 'NONE',  ( 115.4120968585647944, 5.291415217122921177, -3.054999999999994831 ) ) ;
#35586 = ORIENTED_EDGE ( 'NONE', *, *, #108867, .T. ) ;
#35587 = ORIENTED_EDGE ( 'NONE', *, *, #785, .T. ) ;
#35588 = CARTESIAN_POINT ( 'NONE',  ( 16.30000000000000071, 9.521314400968980422E-16, 0.000000000000000000 ) ) ;
#35589 = AXIS2_PLACEMENT_3D ( 'NONE', #116926, #6692, #106744 ) ;
#35590 = AXIS2_PLACEMENT_3D ( 'NONE', #113470, #14163, #58452 ) ;
#35591 = LINE ( 'NONE', #123995, #133486 ) ;
#35592 = ORIENTED_EDGE ( 'NONE', *, *, #105743, .F. ) ;
#35593 = ORIENTED_EDGE ( 'NONE', *, *, #70888, .T. ) ;
#35594 = ORIENTED_EDGE ( 'NONE', *, *, #138766, .T. ) ;
#35595 = CARTESIAN_POINT ( 'NONE',  ( -1.500000000000001332, 16.08746187583908949, 4.000000000000000000 ) ) ;
#35596 = APPLICATION_CONTEXT ( 'automotive_design' ) ;
#35597 = CARTESIAN_POINT ( 'NONE',  ( 1.817069808101886341, -2.126176841940956130, 7.934999999999990727 ) ) ;
#35598 = VECTOR ( 'NONE', #69856, 1000.000000000000227 ) ;
#35599 = EDGE_CURVE ( 'NONE', #45797, #10935, #111304, .T. ) ;
#35600 = CIRCLE ( 'NONE', #107371, 2.500000000000000444 ) ;
#35601 = CARTESIAN_POINT ( 'NONE',  ( 34.62043019189811588, 3.055000000000001936, -5.291415217122916737 ) ) ;
#35602 = VERTEX_POINT ( 'NONE', #45389 ) ;
#35603 = ORIENTED_EDGE ( 'NONE', *, *, #46548, .F. ) ;
#35604 = CARTESIAN_POINT ( 'NONE',  ( -26.28242261357414122, -21.73023691814492508, 5.000000000000000888 ) ) ;
#35605 = VERTEX_POINT ( 'NONE', #47548 ) ;
#35606 = ORIENTED_EDGE ( 'NONE', *, *, #36850, .F. ) ;
#35607 = ORIENTED_EDGE ( 'NONE', *, *, #75234, .T. ) ;
#35608 = AXIS2_PLACEMENT_3D ( 'NONE', #132835, #13846, #47281 ) ;
#35609 = CARTESIAN_POINT ( 'NONE',  ( 0.000000000000000000, 0.000000000000000000, 0.000000000000000000 ) ) ;
#35610 = CARTESIAN_POINT ( 'NONE',  ( 36.48921356237310221, -27.52281430457080802, 5.000000000000000000 ) ) ;
#35611 = DIRECTION ( 'NONE',  ( 0.000000000000000000, -1.000000000000000000, 0.000000000000000000 ) ) ;
#35612 = VERTEX_POINT ( 'NONE', #91704 ) ;
#35613 = VECTOR ( 'NONE', #53084, 1000.000000000000000 ) ;
#35614 = CARTESIAN_POINT ( 'NONE',  ( -30.48921356237309510, -27.52281430457076894, 5.000000000000000000 ) ) ;
#35615 = AXIS2_PLACEMENT_3D ( 'NONE', #71323, #95187, #126390 ) ;
#35616 = FACE_BOUND ( 'NONE', #131875, .T. ) ;
#35617 = ORIENTED_EDGE ( 'NONE', *, *, #17351, .T. ) ;
#35618 = LINE ( 'NONE', #88555, #126690 ) ;
#35619 = DIRECTION ( 'NONE',  ( 0.7071067811865486830, -0.7071067811865464625, -0.000000000000000000 ) ) ;
#35620 = CARTESIAN_POINT ( 'NONE',  ( 0.000000000000000000, 0.000000000000000000, 5.000000000000000000 ) ) ;
#35621 = ORIENTED_EDGE ( 'NONE', *, *, #49062, .F. ) ;
#35622 = CARTESIAN_POINT ( 'NONE',  ( 27.79289321881326558, -14.24070752338414003, 5.000000000000000000 ) ) ;
#35623 = ORIENTED_EDGE ( 'NONE', *, *, #104312, .T. ) ;
#35624 = ORIENTED_EDGE ( 'NONE', *, *, #16668, .T. ) ;
#35625 = VERTEX_POINT ( 'NONE', #67865 ) ;
#35626 = AXIS2_PLACEMENT_3D ( 'NONE', #94583, #84466, #82316 ) ;
#35627 = CARTESIAN_POINT ( 'NONE',  ( 40.89126352523144448, -4.472830434245838482, -4.472830434245838482 ) ) ;
#35629 = EDGE_LOOP ( 'NONE', ( #105836, #57895, #53331, #133060, #81630, #36500 ) ) ;
#35628 = VECTOR ( 'NONE', #55063, 1000.000000000000000 ) ;
#35630 = DIRECTION ( 'NONE',  ( -0.000000000000000000, -0.000000000000000000, 1.000000000000000000 ) ) ;
#35631 = DIRECTION ( 'NONE',  ( 0.000000000000000000, 0.000000000000000000, -1.000000000000000000 ) ) ;
#35632 = ORIENTED_EDGE ( 'NONE', *, *, #83055, .F. ) ;
#35633 = DIRECTION ( 'NONE',  ( 0.7071067811865486830, -0.7071067811865464625, -0.000000000000000000 ) ) ;
#35634 = DIRECTION ( 'NONE',  ( -0.6830127018922180770, -0.6830127018922204085, -0.2588190451025213501 ) ) ;
#35635 = VECTOR ( 'NONE', #138231, 1000.000000000000000 ) ;
#35636 =( BOUNDED_CURVE ( )  B_SPLINE_CURVE ( 3, ( #37307, #80130, #45364, #136602 ),
 .UNSPECIFIED., .F., .F. ) 
 B_SPLINE_CURVE_WITH_KNOTS ( ( 4, 4 ),
 ( 5.106027341939284980, 6.645403452391244414 ),
 .UNSPECIFIED. ) 
 CURVE ( )  GEOMETRIC_REPRESENTATION_ITEM ( )  RATIONAL_B_SPLINE_CURVE ( ( 1.000000000000000000, 0.8120851936182289510, 0.8120851936182289510, 1.000000000000000000 ) ) 
 REPRESENTATION_ITEM ( '' )  );
#35637 =( NAMED_UNIT ( * ) SI_UNIT ( $, .STERADIAN. ) SOLID_ANGLE_UNIT ( ) );
#35638 = CARTESIAN_POINT ( 'NONE',  ( 5.207106781186502609, 15.75929247661555976, 5.000000000000000000 ) ) ;
#35639 = CARTESIAN_POINT ( 'NONE',  ( 6.940000000000001279, 9.521314400968980422E-16, 0.000000000000000000 ) ) ;
#35640 = EDGE_CURVE ( 'NONE', #23427, #111757, #57690, .T. ) ;
#35641 = ORIENTED_EDGE ( 'NONE', *, *, #12524, .F. ) ;
#35642 = ORIENTED_EDGE ( 'NONE', *, *, #66725, .F. ) ;
#35643 = ADVANCED_FACE ( 'NONE', ( #46838 ), #91025, .T. ) ;
#35645 = ORIENTED_EDGE ( 'NONE', *, *, #40173, .T. ) ;
#35644 = AXIS2_PLACEMENT_3D ( 'NONE', #103891, #60452, #6699 ) ;
#35646 = ORIENTED_EDGE ( 'NONE', *, *, #138619, .F. ) ;
#35647 = LINE ( 'NONE', #41302, #128223 ) ;
#35648 = VERTEX_POINT ( 'NONE', #34482 ) ;
#35650 = ORIENTED_EDGE ( 'NONE', *, *, #116467, .F. ) ;
#35649 = EDGE_CURVE ( 'NONE', #66948, #59938, #122917, .T. ) ;
#35651 = CARTESIAN_POINT ( 'NONE',  ( -6.489213562373093325, -27.52281430457059841, 5.000000000000000000 ) ) ;
#35652 = PLANE ( 'NONE',  #89619 ) ;
#35653 = EDGE_CURVE ( 'NONE', #107445, #120101, #23595, .T. ) ;
#35654 = EDGE_CURVE ( 'NONE', #119678, #76576, #92401, .T. ) ;
#35655 = LINE ( 'NONE', #122612, #62477 ) ;
#35656 = VECTOR ( 'NONE', #82624, 1000.000000000000000 ) ;
#35657 = ORIENTED_EDGE ( 'NONE', *, *, #97206, .T. ) ;
#35658 = FACE_OUTER_BOUND ( 'NONE', #87492, .T. ) ;
#35659 = ORIENTED_EDGE ( 'NONE', *, *, #9960, .T. ) ;
#35661 = EDGE_CURVE ( 'NONE', #36236, #101036, #103534, .T. ) ;
#35660 = DIRECTION ( 'NONE',  ( 0.000000000000000000, -1.000000000000000000, 0.000000000000000000 ) ) ;
#35662 = EDGE_CURVE ( 'NONE', #119988, #109534, #61822, .T. ) ;
#35663 = CARTESIAN_POINT ( 'NONE',  ( 27.48373647476854842, -5.808823158059035485, -5.808823158059033709 ) ) ;
#35664 = AXIS2_PLACEMENT_3D ( 'NONE', #34035, #657, #66656 ) ;
#35665 = CARTESIAN_POINT ( 'NONE',  ( -9.489213562373095101, -27.52281430457062328, 5.000000000000000000 ) ) ;
#35666 = ORIENTED_EDGE ( 'NONE', *, *, #107835, .T. ) ;
#35668 = DIRECTION ( 'NONE',  ( -1.000000000000000000, -1.224606353822377258E-16, -0.000000000000000000 ) ) ;
#35667 = CARTESIAN_POINT ( 'NONE',  ( 110.0162635252314374, -4.472830434245839371, 4.472830434245839371 ) ) ;
#35669 = EDGE_CURVE ( 'NONE', #141895, #140903, #17008, .T. ) ;
#35670 = CARTESIAN_POINT ( 'NONE',  ( -9.328169399223463998, 5.259292476615662792, 4.000000000000000000 ) ) ;
#35671 = CARTESIAN_POINT ( 'NONE',  ( -34.49999999999975842, -7.535744391599424219, 4.994342998332167660 ) ) ;
#35672 = ORIENTED_EDGE ( 'NONE', *, *, #25009, .F. ) ;
#35673 = CARTESIAN_POINT ( 'NONE',  ( 63.29974487139158867, -27.71228299555250274, 4.000000000000000000 ) ) ;
#35675 = VERTEX_POINT ( 'NONE', #126461 ) ;
#35674 = FACE_OUTER_BOUND ( 'NONE', #141656, .T. ) ;
#35676 = DIRECTION ( 'NONE',  ( 0.7071067811865487940, 0.7071067811865463515, -0.000000000000000000 ) ) ;
#35677 = ORIENTED_EDGE ( 'NONE', *, *, #116409, .T. ) ;
#35678 = EDGE_CURVE ( 'NONE', #52654, #31895, #3932, .T. ) ;
#35679 = CARTESIAN_POINT ( 'NONE',  ( -25.39999999999996305, 3.061616997868383141E-16, -2.500000000000000000 ) ) ;
#35680 = CARTESIAN_POINT ( 'NONE',  ( -20.99999999999985079, 12.25461709320619086, -10.07315571508702057 ) ) ;
#35681 = DIRECTION ( 'NONE',  ( -0.7071067811865486830, 0.7071067811865464625, 0.000000000000000000 ) ) ;
#35682 = CARTESIAN_POINT ( 'NONE',  ( 120.1458333333333428, 2.130196079827394229, -7.950000000000021494 ) ) ;
#35684 = EDGE_LOOP ( 'NONE', ( #84510, #89150, #90089, #117183 ) ) ;
#35683 = VECTOR ( 'NONE', #1347, 1000.000000000000000 ) ;
#35685 = DIRECTION ( 'NONE',  ( 0.7071067811865487940, 0.7071067811865463515, 0.000000000000000000 ) ) ;
#35686 = EDGE_CURVE ( 'NONE', #106062, #135320, #6082, .T. ) ;
#35687 = CARTESIAN_POINT ( 'NONE',  ( 1.499999999999992673, -10.53360074219763476, 5.000000000000000000 ) ) ;
#35688 = CARTESIAN_POINT ( 'NONE',  ( -11.29298673570688649, -21.74070752338406720, 4.999753212805217117 ) ) ;
#35689 = EDGE_LOOP ( 'NONE', ( #134119, #127009, #85151, #31022 ) ) ;
#35690 = DIRECTION ( 'NONE',  ( 0.7071067811865487940, 0.7071067811865463515, 0.000000000000000000 ) ) ;
#35691 = ORIENTED_EDGE ( 'NONE', *, *, #110437, .F. ) ;
#35692 = EDGE_CURVE ( 'NONE', #120761, #89471, #72145, .T. ) ;
#35693 = DIRECTION ( 'NONE',  ( -0.000000000000000000, 0.3543493200069153248, 0.9351131265310292928 ) ) ;
#35695 = ORIENTED_EDGE ( 'NONE', *, *, #8768, .T. ) ;
#35694 = CARTESIAN_POINT ( 'NONE',  ( 30.48921356237309510, -27.52281430457076894, 5.000000000000000000 ) ) ;
#35696 = VERTEX_POINT ( 'NONE', #127928 ) ;
#35697 = CARTESIAN_POINT ( 'NONE',  ( 34.40832548098979515, -0.7407075233842770334, 14.76736230305388631 ) ) ;
#35698 = SURFACE_STYLE_USAGE ( .BOTH. , #88627 ) ;
#35700 = EDGE_CURVE ( 'NONE', #77699, #27215, #39490, .T. ) ;
#35699 = AXIS2_PLACEMENT_3D ( 'NONE', #107077, #119360, #30232 ) ;
#35701 = VERTEX_POINT ( 'NONE', #61961 ) ;
#35702 = VECTOR ( 'NONE', #83496, 1000.000000000000000 ) ;
#35703 =( NAMED_UNIT ( * ) PLANE_ANGLE_UNIT ( ) SI_UNIT ( $, .RADIAN. ) );
#35704 = VERTEX_POINT ( 'NONE', #114170 ) ;
#35705 = CARTESIAN_POINT ( 'NONE',  ( 15.20840764549667767, 9.139736423841732040E-16, 0.000000000000000000 ) ) ;
#35706 = CARTESIAN_POINT ( 'NONE',  ( 62.99451991528749772, 28.92564299267982264, 4.000000000000000000 ) ) ;
#35708 = EDGE_CURVE ( 'NONE', #117516, #30259, #6794, .T. ) ;
#35707 = DIRECTION ( 'NONE',  ( 0.000000000000000000, 0.000000000000000000, 1.000000000000000000 ) ) ;
#35709 = CARTESIAN_POINT ( 'NONE',  ( 66.18398860626901126, 28.73617430169833753, 5.000000000000000000 ) ) ;
#35710 = LINE ( 'NONE', #103070, #83096 ) ;
#35711 = LINE ( 'NONE', #137129, #76697 ) ;
#35712 = EDGE_LOOP ( 'NONE', ( #56759, #132324, #71948, #86998 ) ) ;
#35713 = VERTEX_POINT ( 'NONE', #28077 ) ;
#35714 = ORIENTED_EDGE ( 'NONE', *, *, #60016, .F. ) ;
#35715 = EDGE_CURVE ( 'NONE', #9875, #106324, #6985, .T. ) ;
#35716 = CARTESIAN_POINT ( 'NONE',  ( 124.2291666666666714, 7.950000000000001954, -2.130196079827421762 ) ) ;
#35717 = ORIENTED_EDGE ( 'NONE', *, *, #33278, .F. ) ;
#35718 = AXIS2_PLACEMENT_3D ( 'NONE', #22578, #133533, #101595 ) ;
#35719 = ORIENTED_EDGE ( 'NONE', *, *, #91957, .F. ) ;
#35720 = EDGE_CURVE ( 'NONE', #134437, #97146, #124189, .T. ) ;
#35721 = ORIENTED_EDGE ( 'NONE', *, *, #90997, .T. ) ;
#35722 = CARTESIAN_POINT ( 'NONE',  ( 0.8453006047648484733, -6.493492593015893100, -3.237972208483580694 ) ) ;
#35723 = CARTESIAN_POINT ( 'NONE',  ( -32.67183060077623935, 17.25929247661554200, 4.000000000000000000 ) ) ;
#35724 = VERTEX_POINT ( 'NONE', #69114 ) ;
#35725 = SPHERICAL_SURFACE ( 'NONE', #69342, 0.5000000000000000000 ) ;
#35728 = EDGE_CURVE ( 'NONE', #128989, #57042, #90873, .T. ) ;
#35727 = VECTOR ( 'NONE', #112499, 1000.000000000000000 ) ;
#35726 = CARTESIAN_POINT ( 'NONE',  ( 25.39999999999998792, 5.550253899293828397, 4.161426631299068646 ) ) ;
#35729 = CARTESIAN_POINT ( 'NONE',  ( 27.42327845806336839, 11.25929247661559884, 17.85071094206578124 ) ) ;
#35730 = VECTOR ( 'NONE', #54550, 999.9999999999998863 ) ;
#35731 = DIRECTION ( 'NONE',  ( -1.000000000000000000, -1.224606353822377258E-16, -0.000000000000000000 ) ) ;
#35732 = CARTESIAN_POINT ( 'NONE',  ( 125.1254301918981184, 5.291415217122919401, 3.055000000000002824 ) ) ;
#35733 = ORIENTED_EDGE ( 'NONE', *, *, #105834, .T. ) ;
#35734 = FACE_OUTER_BOUND ( 'NONE', #83806, .T. ) ;
#35735 = LINE ( 'NONE', #1593, #33430 ) ;
#35736 = CARTESIAN_POINT ( 'NONE',  ( 1.315494349410903485, 0.8306144699724272717, 6.741090620970949132 ) ) ;
#35737 = DIRECTION ( 'NONE',  ( 0.7071067811865487940, -0.7071067811865463515, 0.000000000000000000 ) ) ;
#35738 = CARTESIAN_POINT ( 'NONE',  ( 2.510786437626908008, -27.52281430457053446, 5.000000000000000000 ) ) ;
#35739 = CARTESIAN_POINT ( 'NONE',  ( 4.184256412735922304, 4.202752102959690472E-16, 0.000000000000000000 ) ) ;
#35740 = VECTOR ( 'NONE', #18817, 1000.000000000000000 ) ;
#35741 = CARTESIAN_POINT ( 'NONE',  ( 48.78752705046289151, 0.000000000000000000, -7.949999999999998401 ) ) ;
#35742 = DIRECTION ( 'NONE',  ( 0.7071067811865487940, 0.7071067811865463515, -0.000000000000000000 ) ) ;
#35743 = VECTOR ( 'NONE', #28514, 999.9999999999998863 ) ;
#35744 = DIRECTION ( 'NONE',  ( 0.7071067811865487940, -0.7071067811865463515, 0.000000000000000000 ) ) ;
#35745 = EDGE_LOOP ( 'NONE', ( #7300, #25959, #114475, #70058, #7914, #88003, #22303, #119946, #34850, #109401, #136926, #19626, #126465, #31491, #3099, #109093, #92620, #132456, #13764, #66176, #67552, #84111, #113819, #80536, #68055, #70923, #134881, #118904, #136632, #51469, #117353, #52646, #29489, #59539, #83054, #49191, #141123, #37999, #14191, #102061, #91043, #37053, #103156, #75553, #30361, #83825, #117265, #108274, #65525, #115205, #91777, #141927, #37276, #140911, #97274, #86211, #13802, #105251, #2967, #2176, #75019, #110141, #15942, #54045, #102149, #39525, #142490, #32889, #9214, #17376, #111427, #64006, #23820, #30808, #61050, #54222, #104518, #76237, #101378, #116878, #106935, #79916, #87697, #121651, #8398, #77830, #86636, #97913, #71133, #80323, #99591, #39135, #141498, #99096, #42460, #22678, #98141, #134624, #141506, #121922, #72086, #50850, #42922, #72220, #85646 ) ) ;
#35746 = ORIENTED_EDGE ( 'NONE', *, *, #91681, .T. ) ;
#35747 = CARTESIAN_POINT ( 'NONE',  ( 42.27083333333331439, -7.949999999999999289, -2.130196079827426203 ) ) ;
#35748 = VERTEX_POINT ( 'NONE', #110432 ) ;
#35749 = EDGE_CURVE ( 'NONE', #22223, #78390, #228, .T. ) ;
#35750 = DIRECTION ( 'NONE',  ( -0.000000000000000000, 0.3543493200069152138, -0.9351131265310292928 ) ) ;
#35751 = EDGE_LOOP ( 'NONE', ( #2793, #88351, #111578, #409 ) ) ;
#35752 = CARTESIAN_POINT ( 'NONE',  ( -30.79289321881324071, -11.24070752338416668, 5.000000000000000000 ) ) ;
#35753 = DIRECTION ( 'NONE',  ( -0.000000000000000000, 0.000000000000000000, 1.000000000000000000 ) ) ;
#35754 = CARTESIAN_POINT ( 'NONE',  ( 41.85459685856477563, -1.637169565754161615, 6.110000000000000320 ) ) ;
#35755 = ADVANCED_FACE ( 'NONE', ( #49522 ), #114024, .F. ) ;
#35756 = VERTEX_POINT ( 'NONE', #3787 ) ;
#35757 = CARTESIAN_POINT ( 'NONE',  ( 27.70710678118635428, 5.259292476615659240, 5.000000000000000000 ) ) ;
#35758 = VERTEX_POINT ( 'NONE', #6638 ) ;
#35759 = AXIS2_PLACEMENT_3D ( 'NONE', #19051, #63313, #111591 ) ;
#35760 = DIRECTION ( 'NONE',  ( 0.7071067811865486830, -0.7071067811865464625, -0.000000000000000000 ) ) ;
#35761 = CARTESIAN_POINT ( 'NONE',  ( 2.999999999999975131, -22.06887692260758982, 4.000000000000000000 ) ) ;
#35762 = LINE ( 'NONE', #65531, #83719 ) ;
#35763 = DIRECTION ( 'NONE',  ( -1.000000000000000000, -1.224606353822377258E-16, -0.000000000000000000 ) ) ;
#35764 = ORIENTED_EDGE ( 'NONE', *, *, #114337, .F. ) ;
#35765 = EDGE_CURVE ( 'NONE', #115630, #132022, #50643, .T. ) ;
#35766 = CARTESIAN_POINT ( 'NONE',  ( 2.510786437626908008, -27.52281430457053446, 5.000000000000000000 ) ) ;
#35767 = VERTEX_POINT ( 'NONE', #59672 ) ;
#35768 = CARTESIAN_POINT ( 'NONE',  ( 38.72502705046289151, 5.819803920172573974, -5.819803920172573086 ) ) ;
#35769 = DIRECTION ( 'NONE',  ( 0.000000000000000000, 0.3543493200069153248, 0.9351131265310291818 ) ) ;
#35770 = CARTESIAN_POINT ( 'NONE',  ( -16.06996025486399304, -0.7407075233842735917, 13.87443053587614905 ) ) ;
#35771 = CARTESIAN_POINT ( 'NONE',  ( -15.48921356237309510, -27.52281430457066236, 5.000000000000000000 ) ) ;
#35772 = LINE ( 'NONE', #80679, #29950 ) ;
#35773 = CARTESIAN_POINT ( 'NONE',  ( -6.299744871391586898, -27.71228299555210484, 4.000000000000000000 ) ) ;
#35774 = CARTESIAN_POINT ( 'NONE',  ( 55.18293019189810877, -1.637169565754158951, -6.109999999999998543 ) ) ;
#35775 = CARTESIAN_POINT ( 'NONE',  ( -0.3281693992235306667, 8.259292476615636147, 4.000000000000000000 ) ) ;
#35776 = DIRECTION ( 'NONE',  ( -0.7071067811865486830, -0.7071067811865464625, -0.000000000000000000 ) ) ;
#35778 = ORIENTED_EDGE ( 'NONE', *, *, #22089, .T. ) ;
#35777 = CARTESIAN_POINT ( 'NONE',  ( 5.999999999999960032, -1.068876922607809421, 4.000000000000000000 ) ) ;
#35779 = ORIENTED_EDGE ( 'NONE', *, *, #34003, .F. ) ;
#35780 = CARTESIAN_POINT ( 'NONE',  ( 11.84387692260750136, -22.22500000000000497, 4.000000000000000000 ) ) ;
#35781 = ORIENTED_EDGE ( 'NONE', *, *, #85963, .T. ) ;
#35783 = ADVANCED_FACE ( 'NONE', ( #115407 ), #105970, .F. ) ;
#35782 = AXIS2_PLACEMENT_3D ( 'NONE', #42209, #141505, #89263 ) ;
#35784 = EDGE_CURVE ( 'NONE', #125467, #93695, #80707, .T. ) ;
#35785 = FACE_OUTER_BOUND ( 'NONE', #8485, .T. ) ;
#35786 = ORIENTED_EDGE ( 'NONE', *, *, #139898, .T. ) ;
#35787 = DIRECTION ( 'NONE',  ( -0.000000000000000000, 0.000000000000000000, 1.000000000000000000 ) ) ;
#35788 = FACE_BOUND ( 'NONE', #127693, .T. ) ;
#35789 = EDGE_CURVE ( 'NONE', #137119, #88854, #105283, .T. ) ;
#35790 = CARTESIAN_POINT ( 'NONE',  ( 81.18398860626899705, 28.73617430169844056, 5.000000000000000000 ) ) ;
#35791 = LINE ( 'NONE', #133649, #76762 ) ;
#35792 = DIRECTION ( 'NONE',  ( 0.7071067811865487940, 0.7071067811865463515, 0.000000000000000000 ) ) ;
#35794 = ORIENTED_EDGE ( 'NONE', *, *, #43640, .T. ) ;
#35793 = CARTESIAN_POINT ( 'NONE',  ( 12.29974487139158512, -27.71228299555214747, 4.000000000000000000 ) ) ;
#35795 = VECTOR ( 'NONE', #132817, 999.9999999999998863 ) ;
#35796 = ORIENTED_EDGE ( 'NONE', *, *, #111668, .T. ) ;
#35797 = LINE ( 'NONE', #126329, #85672 ) ;
#35798 = ORIENTED_EDGE ( 'NONE', *, *, #29284, .F. ) ;
#35799 = VECTOR ( 'NONE', #37683, 1000.000000000000000 ) ;
#35800 = ORIENTED_EDGE ( 'NONE', *, *, #56704, .T. ) ;
#35801 = CARTESIAN_POINT ( 'NONE',  ( 72.09959685856479439, -6.109999999999997655, -1.637169565754160283 ) ) ;
#35802 = VERTEX_POINT ( 'NONE', #92252 ) ;
#35803 =( BOUNDED_CURVE ( )  B_SPLINE_CURVE ( 2, ( #6579, #105225, #114658, #71197, #115345, #18179, #49462, #82777, #103771, #93650, #139322, #137879, #95775 ),
 .UNSPECIFIED., .F., .T. ) 
 B_SPLINE_CURVE_WITH_KNOTS ( ( 3, 2, 2, 2, 2, 2, 3 ),
 ( 0.4333333333333333481, 0.4361111111111111160, 0.4388888888888888840, 0.4416666666666666519, 0.4444444444444444198, 0.4472222222222222432, 0.4500000000000000111 ),
 .UNSPECIFIED. ) 
 CURVE ( )  GEOMETRIC_REPRESENTATION_ITEM ( )  RATIONAL_B_SPLINE_CURVE ( ( 1.000000000000000000, 0.9659258262890683122, 1.000000000000000000, 0.9659258262890683122, 1.000000000000000000, 0.9659258262890683122, 1.000000000000000000, 0.9659258262890683122, 1.000000000000000000, 0.9659258262890683122, 1.000000000000000000, 0.9659258262890683122, 1.000000000000000000 ) ) 
 REPRESENTATION_ITEM ( '' )  );
#35804 = LINE ( 'NONE', #59002, #39732 ) ;
#35805 = VECTOR ( 'NONE', #133754, 999.9999999999998863 ) ;
#35806 = ORIENTED_EDGE ( 'NONE', *, *, #76899, .T. ) ;
#35807 = DIRECTION ( 'NONE',  ( 0.7071067811865487940, -0.7071067811865463515, 0.000000000000000000 ) ) ;
#35808 = CARTESIAN_POINT ( 'NONE',  ( -33.18398860626899705, 28.73617430169810305, 5.000000000000000000 ) ) ;
#35809 = PLANE ( 'NONE',  #22262 ) ;
#35810 = VECTOR ( 'NONE', #29562, 1000.000000000000000 ) ;
#35812 = FACE_OUTER_BOUND ( 'NONE', #11571, .T. ) ;
#35811 = LINE ( 'NONE', #59012, #106009 ) ;
#35813 = DIRECTION ( 'NONE',  ( -0.3543493200069162685, -0.000000000000000000, -0.9351131265310288487 ) ) ;
#35814 = DIRECTION ( 'NONE',  ( 0.7071067811865487940, 0.7071067811865463515, 0.000000000000000000 ) ) ;
#35815 = ORIENTED_EDGE ( 'NONE', *, *, #131562, .T. ) ;
#35816 = VERTEX_POINT ( 'NONE', #26312 ) ;
#35817 = DIRECTION ( 'NONE',  ( -0.7071067811865487940, 0.7071067811865463515, 0.000000000000000000 ) ) ;
#35818 = DIRECTION ( 'NONE',  ( 0.5735764363510444941, 0.8191520442889929088, 0.000000000000000000 ) ) ;
#35819 = ORIENTED_EDGE ( 'NONE', *, *, #113382, .T. ) ;
#35820 = ORIENTED_EDGE ( 'NONE', *, *, #7677, .F. ) ;
#35821 = ORIENTED_EDGE ( 'NONE', *, *, #81920, .F. ) ;
#35822 = EDGE_CURVE ( 'NONE', #97476, #9196, #5236, .T. ) ;
#35823 = CARTESIAN_POINT ( 'NONE',  ( 31.06293019189809712, 1.637169565754157174, 6.110000000000002984 ) ) ;
#35824 = VERTEX_POINT ( 'NONE', #137932 ) ;
#35825 = DIRECTION ( 'NONE',  ( -0.7071067811865486830, -0.7071067811865464625, -0.000000000000000000 ) ) ;
#35826 =( BOUNDED_CURVE ( )  B_SPLINE_CURVE ( 2, ( #68139, #78264, #69539, #670, #47796, #81120, #112316, #90564, #102157, #136188, #122446, #23111, #35499 ),
 .UNSPECIFIED., .F., .F. ) 
 B_SPLINE_CURVE_WITH_KNOTS ( ( 3, 2, 2, 2, 2, 2, 3 ),
 ( 0.2833333333333333259, 0.2861111111111110938, 0.2888888888888888618, 0.2916666666666666852, 0.2944444444444444531, 0.2972222222222222210, 0.2999999999999999889 ),
 .UNSPECIFIED. ) 
 CURVE ( )  GEOMETRIC_REPRESENTATION_ITEM ( )  RATIONAL_B_SPLINE_CURVE ( ( 1.000000000000000000, 0.9659258262890683122, 1.000000000000000000, 0.9659258262890683122, 1.000000000000000000, 0.9659258262890683122, 1.000000000000000000, 0.9659258262890683122, 1.000000000000000000, 0.9659258262890683122, 1.000000000000000000, 0.9659258262890683122, 1.000000000000000000 ) ) 
 REPRESENTATION_ITEM ( '' )  );
#35827 = AXIS2_PLACEMENT_3D ( 'NONE', #80934, #124419, #36010 ) ;
#35829 = EDGE_CURVE ( 'NONE', #32049, #102811, #65505, .T. ) ;
#35828 = PRESENTATION_STYLE_ASSIGNMENT (( #115446 ) ) ;
#35830 = EDGE_CURVE ( 'NONE', #83534, #10814, #82843, .T. ) ;
#35831 = CIRCLE ( 'NONE', #26586, 2.055000000000001048 ) ;
#35832 = CARTESIAN_POINT ( 'NONE',  ( 30.37913961620377634, -5.278424836066145431, -3.047499999999993658 ) ) ;
#35833 = AXIS2_PLACEMENT_3D ( 'NONE', #131577, #54742, #128196 ) ;
#35834 = LINE ( 'NONE', #80055, #139866 ) ;
#35835 = EDGE_CURVE ( 'NONE', #110472, #61053, #139388, .T. ) ;
#35836 = ORIENTED_EDGE ( 'NONE', *, *, #96654, .T. ) ;
#35837 = AXIS2_PLACEMENT_3D ( 'NONE', #125261, #33981, #114379 ) ;
#35838 = CARTESIAN_POINT ( 'NONE',  ( -34.92500000000001137, 21.72500000000000142, 5.000000000000000000 ) ) ;
#35839 = ADVANCED_FACE ( 'NONE', ( #25575 ), #28461, .F. ) ;
#35840 = DIRECTION ( 'NONE',  ( -0.7071067811865486830, -0.7071067811865464625, 0.000000000000000000 ) ) ;
#35841 = FACE_OUTER_BOUND ( 'NONE', #26744, .T. ) ;
#35843 = EDGE_LOOP ( 'NONE', ( #107781, #141760, #108185, #83098 ) ) ;
#35842 = LINE ( 'NONE', #133696, #51829 ) ;
#35844 = ORIENTED_EDGE ( 'NONE', *, *, #79594, .T. ) ;
#35845 = EDGE_CURVE ( 'NONE', #63680, #126408, #69850, .T. ) ;
#35846 = CARTESIAN_POINT ( 'NONE',  ( 3.183988606268992161, 28.73617430169789699, 5.000000000000000000 ) ) ;
#35847 = CARTESIAN_POINT ( 'NONE',  ( 24.70701326429286482, -21.74070752338406365, 4.999753212805220670 ) ) ;
#35848 = PLANE ( 'NONE',  #123571 ) ;
#35849 = EDGE_LOOP ( 'NONE', ( #93357, #113284, #7500, #108196, #131005 ) ) ;
#35850 = VECTOR ( 'NONE', #46136, 1000.000000000000000 ) ;
#35851 = DIRECTION ( 'NONE',  ( -0.7071067811865486830, -0.7071067811865464625, 0.000000000000000000 ) ) ;
#35852 = LINE ( 'NONE', #14035, #71127 ) ;
#35853 = ADVANCED_FACE ( 'NONE', ( #17548 ), #48071, .F. ) ;
#35854 = CARTESIAN_POINT ( 'NONE',  ( -24.70679250724059628, 20.25929247661551358, 20.83292124670820655 ) ) ;
#35855 = CARTESIAN_POINT ( 'NONE',  ( 28.70833333333332149, -3.974999999999999201, -6.884901960086287964 ) ) ;
#35856 = PLANE ( 'NONE',  #116622 ) ;
#35857 = ORIENTED_EDGE ( 'NONE', *, *, #90330, .F. ) ;
#35858 = CARTESIAN_POINT ( 'NONE',  ( -12.69999999999998153, 0.000000000000000000, 1.749999999999999778 ) ) ;
#35859 = CARTESIAN_POINT ( 'NONE',  ( 78.48921356237309510, -27.52281430457109934, 5.000000000000000000 ) ) ;
#35860 = CARTESIAN_POINT ( 'NONE',  ( 0.2569208697893815008, -0.3999999999999998002, -2.015694669338588429 ) ) ;
#35861 = EDGE_CURVE ( 'NONE', #27927, #26527, #70570, .T. ) ;
#35862 = CARTESIAN_POINT ( 'NONE',  ( 71.99451991528749772, 28.92564299267988304, 4.000000000000000000 ) ) ;
#35863 = LINE ( 'NONE', #56896, #80754 ) ;
#35864 = EDGE_CURVE ( 'NONE', #48713, #4046, #42912, .T. ) ;
#35865 = ORIENTED_EDGE ( 'NONE', *, *, #11759, .T. ) ;
#35866 = ORIENTED_EDGE ( 'NONE', *, *, #90268, .T. ) ;
#35867 = CARTESIAN_POINT ( 'NONE',  ( 25.60725813788241112, -3.175000000000001155, -5.499261314031188341 ) ) ;
#35868 = DIRECTION ( 'NONE',  ( -0.3543493200069163795, -9.265275131829747941E-33, -0.9351131265310288487 ) ) ;
#35869 = EDGE_CURVE ( 'NONE', #73316, #141465, #94844, .T. ) ;
#35870 = DIRECTION ( 'NONE',  ( 0.000000000000000000, -1.000000000000000000, 0.000000000000000000 ) ) ;
#35871 = CARTESIAN_POINT ( 'NONE',  ( -39.18398860626899705, 28.73617430169814568, 5.000000000000000000 ) ) ;
#35872 = CARTESIAN_POINT ( 'NONE',  ( 13.11151487241214930, 3.778085383357085547, 4.109577000315250750 ) ) ;
#35873 = ORIENTED_EDGE ( 'NONE', *, *, #21550, .F. ) ;
#35874 = FACE_OUTER_BOUND ( 'NONE', #73600, .T. ) ;
#35875 = DIRECTION ( 'NONE',  ( -1.000000000000000000, -1.224606353822377258E-16, -0.000000000000000000 ) ) ;
#35876 = DIRECTION ( 'NONE',  ( -0.7071067811865486830, -0.7071067811865464625, 0.000000000000000000 ) ) ;
#35877 = CARTESIAN_POINT ( 'NONE',  ( 57.22459685856476597, -1.637169565754161171, 6.109999999999998543 ) ) ;
#35878 = AXIS2_PLACEMENT_3D ( 'NONE', #104402, #82677, #29691 ) ;
#35879 = DIRECTION ( 'NONE',  ( 0.7071067811865487940, 0.7071067811865463515, 0.000000000000000000 ) ) ;
#35880 = PLANE ( 'NONE',  #76612 ) ;
#35881 = CARTESIAN_POINT ( 'NONE',  ( -44.99451991528749772, 28.92564299267969474, 4.000000000000000000 ) ) ;
#35882 = EDGE_LOOP ( 'NONE', ( #127178, #126353, #62015, #44145 ) ) ;
#35883 = ADVANCED_FACE ( 'NONE', ( #131326 ), #21126, .F. ) ;
#35884 = EDGE_LOOP ( 'NONE', ( #42072, #31736, #41738, #57694 ) ) ;
#35885 = CARTESIAN_POINT ( 'NONE',  ( 20.97999999999999687, 9.521314400968980422E-16, 0.000000000000000000 ) ) ;
#35886 = DIRECTION ( 'NONE',  ( -0.5735764363510507113, 0.8191520442889885789, 1.003171929053520926E-16 ) ) ;
#35887 = DIRECTION ( 'NONE',  ( 0.6830127018922181881, 0.6830127018922202975, -0.2588190451025214056 ) ) ;
#35888 = LINE ( 'NONE', #38017, #18499 ) ;
#35889 = LINE ( 'NONE', #99667, #53320 ) ;
#35890 = CARTESIAN_POINT ( 'NONE',  ( 26.28242261357414122, -21.73023691814492864, 5.000000000000000888 ) ) ;
#35891 = ORIENTED_EDGE ( 'NONE', *, *, #38594, .F. ) ;
#35892 = VERTEX_POINT ( 'NONE', #119696 ) ;
#35893 = CARTESIAN_POINT ( 'NONE',  ( -27.70710678118634718, -3.740707523384238176, 5.000000000000000000 ) ) ;
#35894 = CARTESIAN_POINT ( 'NONE',  ( -8.149948714589710264, -8.240707523384200428, 17.25253755692237334 ) ) ;
#35895 = UNCERTAINTY_MEASURE_WITH_UNIT (LENGTH_MEASURE( 1.000000000000000082E-05 ), #35580, 'distance_accuracy_value', 'NONE');
#35896 = DIRECTION ( 'NONE',  ( 0.000000000000000000, 0.000000000000000000, 1.000000000000000000 ) ) ;
#35897 = ADVANCED_FACE ( 'NONE', ( #84964 ), #32009, .F. ) ;
#35898 = DIRECTION ( 'NONE',  ( 0.000000000000000000, -1.000000000000000000, 0.000000000000000000 ) ) ;
#35899 = CARTESIAN_POINT ( 'NONE',  ( 76.35002705046288440, -5.819803920172572198, -5.819803920172572198 ) ) ;
#35900 = DIRECTION ( 'NONE',  ( 0.7071067811865487940, 0.7071067811865463515, 0.000000000000000000 ) ) ;
#35901 = CIRCLE ( 'NONE', #47509, 9.524999999999998579 ) ;
#35902 = FACE_OUTER_BOUND ( 'NONE', #79164, .T. ) ;
#35903 = ORIENTED_EDGE ( 'NONE', *, *, #48628, .T. ) ;
#35904 = CARTESIAN_POINT ( 'NONE',  ( 77.70833333333332860, -3.974999999999999201, -6.884901960086287964 ) ) ;
#35905 = DIRECTION ( 'NONE',  ( 0.7071067811865486830, -0.7071067811865464625, -0.000000000000000000 ) ) ;
#35906 = EDGE_CURVE ( 'NONE', #121857, #55125, #134209, .T. ) ;
#35907 = CARTESIAN_POINT ( 'NONE',  ( -34.92500000000001137, 21.72500000000000142, 5.000000000000000000 ) ) ;
#35908 = CARTESIAN_POINT ( 'NONE',  ( -69.29974487139159578, -27.71228299555254537, 4.000000000000000000 ) ) ;
#35909 = VERTEX_POINT ( 'NONE', #75526 ) ;
#35910 = CARTESIAN_POINT ( 'NONE',  ( -11.99999999999990763, -12.03360074219761700, 5.000000000000000000 ) ) ;
#35911 = VECTOR ( 'NONE', #106225, 1000.000000000000000 ) ;
#35912 = EDGE_CURVE ( 'NONE', #18521, #25422, #142227, .T. ) ;
#35913 = DIRECTION ( 'NONE',  ( 0.7071067811865487940, 0.7071067811865463515, 0.000000000000000000 ) ) ;
#35914 = CARTESIAN_POINT ( 'NONE',  ( 66.06293019189810423, 1.637169565754157174, 6.110000000000002984 ) ) ;
#35915 = PLANE ( 'NONE',  #46053 ) ;
#35916 = ORIENTED_EDGE ( 'NONE', *, *, #47562, .F. ) ;
#35917 = VERTEX_POINT ( 'NONE', #76240 ) ;
#35918 = LINE ( 'NONE', #112729, #132359 ) ;
#35919 = DIRECTION ( 'NONE',  ( -0.6830127018922181881, 0.6830127018922202975, -0.2588190451025214056 ) ) ;
#35920 = EDGE_CURVE ( 'NONE', #7608, #16626, #51641, .T. ) ;
#35921 = CARTESIAN_POINT ( 'NONE',  ( 12.87729808236044704, 22.22500000000000142, -13.11407768714525623 ) ) ;
#35923 = ORIENTED_EDGE ( 'NONE', *, *, #87489, .T. ) ;
#35922 = CARTESIAN_POINT ( 'NONE',  ( 85.72916666666665719, 7.950000000000001954, -2.130196079827421762 ) ) ;
#35924 = PLANE ( 'NONE',  #36820 ) ;
#35925 = DIRECTION ( 'NONE',  ( -1.000000000000000000, -0.000000000000000000, -0.000000000000000000 ) ) ;
#35926 = CARTESIAN_POINT ( 'NONE',  ( 9.707106781186478628, -3.740707523384246613, 5.000000000000000000 ) ) ;
#35927 = CARTESIAN_POINT ( 'NONE',  ( 15.29974487139158867, -27.71228299555216879, 4.000000000000000000 ) ) ;
#35928 = ORIENTED_EDGE ( 'NONE', *, *, #66847, .F. ) ;
#35929 = VECTOR ( 'NONE', #96115, 1000.000000000000227 ) ;
#35930 = VERTEX_POINT ( 'NONE', #107426 ) ;
#35931 = CARTESIAN_POINT ( 'NONE',  ( 56.00043019189809712, -3.055000000000002380, 5.291415217122920289 ) ) ;
#35932 = AXIS2_PLACEMENT_3D ( 'NONE', #42423, #18460, #76472 ) ;
#35933 = EDGE_LOOP ( 'NONE', ( #18087, #9704, #67844, #57403 ) ) ;
#35934 = VECTOR ( 'NONE', #17922, 1000.000000000000000 ) ;
#35935 = CARTESIAN_POINT ( 'NONE',  ( 2.700255128608413990, -27.71228299555204089, 4.000000000000000000 ) ) ;
#35936 = DIRECTION ( 'NONE',  ( 0.7071067811865487940, 0.7071067811865463515, -0.000000000000000000 ) ) ;
#35937 = FACE_OUTER_BOUND ( 'NONE', #76963, .T. ) ;
#35938 = CARTESIAN_POINT ( 'NONE',  ( 53.93750000000000000, 5.819803920172574863, -5.819803920172573086 ) ) ;
#35939 = ORIENTED_EDGE ( 'NONE', *, *, #111919, .F. ) ;
#35940 = VERTEX_POINT ( 'NONE', #64643 ) ;
#35941 = PLANE ( 'NONE',  #93141 ) ;
#35942 = CARTESIAN_POINT ( 'NONE',  ( -16.98224699891571277, -0.6362351928176004368, -31.34040500397710005 ) ) ;
#35943 = EDGE_CURVE ( 'NONE', #3467, #91787, #18994, .T. ) ;
#35944 = ORIENTED_EDGE ( 'NONE', *, *, #13676, .F. ) ;
#35945 = ADVANCED_FACE ( 'NONE', ( #8772 ), #53030, .F. ) ;
#35946 = FACE_OUTER_BOUND ( 'NONE', #93582, .T. ) ;
#35947 = VERTEX_POINT ( 'NONE', #95835 ) ;
#35948 = CARTESIAN_POINT ( 'NONE',  ( 112.2250270504628702, 5.819803920172573974, -5.819803920172573086 ) ) ;
#35949 = LINE ( 'NONE', #89576, #123507 ) ;
#35950 = EDGE_LOOP ( 'NONE', ( #9750, #16698, #20293, #99952, #32776 ) ) ;
#35951 = FACE_BOUND ( 'NONE', #21652, .T. ) ;
#35952 = EDGE_CURVE ( 'NONE', #115605, #12661, #8087, .T. ) ;
#35953 = DIRECTION ( 'NONE',  ( -0.7071067811865486830, -0.7071067811865464625, 0.000000000000000000 ) ) ;
#35954 = LINE ( 'NONE', #133124, #136959 ) ;
#35955 = PLANE ( 'NONE',  #59891 ) ;
#35956 = DIRECTION ( 'NONE',  ( 0.000000000000000000, 0.000000000000000000, 1.000000000000000000 ) ) ;
#35957 = CARTESIAN_POINT ( 'NONE',  ( 29.99999999999999645, 2.375000000000000000, -4.320000000000002061 ) ) ;
#35958 = DIRECTION ( 'NONE',  ( 0.000000000000000000, 0.000000000000000000, 1.000000000000000000 ) ) ;
#35959 = EDGE_LOOP ( 'NONE', ( #101464, #18624, #126711, #98620 ) ) ;
#35960 = ORIENTED_EDGE ( 'NONE', *, *, #81166, .T. ) ;
#35961 = CARTESIAN_POINT ( 'NONE',  ( 100.8287635252314516, 0.000000000000000000, -6.109999999999998543 ) ) ;
#35962 = ORIENTED_EDGE ( 'NONE', *, *, #99577, .T. ) ;
#35963 = DIRECTION ( 'NONE',  ( -0.7071067811865487940, 0.7071067811865463515, -0.000000000000000000 ) ) ;
#35964 = ORIENTED_EDGE ( 'NONE', *, *, #76790, .F. ) ;
#35965 = LINE ( 'NONE', #33815, #49296 ) ;
#35966 = CARTESIAN_POINT ( 'NONE',  ( -30.29974487139158867, -27.71228299555227537, 4.000000000000000000 ) ) ;
#35967 = CARTESIAN_POINT ( 'NONE',  ( 6.852250093007166143, 4.584330080086930965E-16, 0.000000000000000000 ) ) ;
#35968 = ORIENTED_EDGE ( 'NONE', *, *, #13378, .F. ) ;
#35969 = CYLINDRICAL_SURFACE ( 'NONE', #20635, 1.249999999999970690 ) ;
#35970 = CARTESIAN_POINT ( 'NONE',  ( 15.81349135397628558, -15.74070752338412760, 8.904080028138903202 ) ) ;
#35971 = FACE_OUTER_BOUND ( 'NONE', #71458, .T. ) ;
#35972 = DIRECTION ( 'NONE',  ( -0.6830127018922180770, -0.6830127018922204085, -0.2588190451025213501 ) ) ;
#35973 = DIRECTION ( 'NONE',  ( -0.7071067811865486830, 0.7071067811865464625, 0.000000000000000000 ) ) ;
#35974 = CARTESIAN_POINT ( 'NONE',  ( -48.48921356237309510, -27.52281430457089328, 5.000000000000000000 ) ) ;
#35975 = ORIENTED_EDGE ( 'NONE', *, *, #122883, .T. ) ;
#35976 = CARTESIAN_POINT ( 'NONE',  ( 2.999999999999978240, 13.55218569542903140, 5.000000000000000000 ) ) ;
#35977 = DIRECTION ( 'NONE',  ( 0.6830127018922181881, 0.6830127018922202975, -0.2588190451025214056 ) ) ;
#35978 = ORIENTED_EDGE ( 'NONE', *, *, #52666, .T. ) ;
#35979 = EDGE_LOOP ( 'NONE', ( #8082, #81981, #98121, #55749 ) ) ;
#35980 = ORIENTED_EDGE ( 'NONE', *, *, #98675, .F. ) ;
#35981 = CARTESIAN_POINT ( 'NONE',  ( 52.35459685856476852, -1.637169565754161615, 6.110000000000000320 ) ) ;
#35982 = ORIENTED_EDGE ( 'NONE', *, *, #77504, .T. ) ;
#35983 = VECTOR ( 'NONE', #67102, 1000.000000000000000 ) ;
#35984 = EDGE_CURVE ( 'NONE', #97600, #109094, #41448, .T. ) ;
#35985 = CARTESIAN_POINT ( 'NONE',  ( 9.233306282870437087, -6.094999999999989981, -1.633150327867689100 ) ) ;
#35986 = CARTESIAN_POINT ( 'NONE',  ( 91.43793019189810423, -6.110000000000001208, 1.637169565754158951 ) ) ;
#35987 = DIRECTION ( 'NONE',  ( -0.6830127018922181881, 0.6830127018922202975, -0.2588190451025214056 ) ) ;
#35988 = ORIENTED_EDGE ( 'NONE', *, *, #93125, .F. ) ;
#35989 = EDGE_CURVE ( 'NONE', #81079, #108304, #129896, .T. ) ;
#35990 = CIRCLE ( 'NONE', #49953, 2.055000000000001048 ) ;
#35991 = CARTESIAN_POINT ( 'NONE',  ( 11.99999999999992539, -1.447814304570815169, 5.000000000000000000 ) ) ;
#35993 = ORIENTED_EDGE ( 'NONE', *, *, #113178, .T. ) ;
#35992 = ADVANCED_FACE ( 'NONE', ( #67526 ), #89252, .F. ) ;
#35994 = CARTESIAN_POINT ( 'NONE',  ( 60.48921356237309510, -27.52281430457097500, 5.000000000000000000 ) ) ;
#35995 = DIRECTION ( 'NONE',  ( 0.7071067811865487940, 0.7071067811865463515, -0.000000000000000000 ) ) ;
#35996 = EDGE_LOOP ( 'NONE', ( #109353, #40639, #58348, #35916 ) ) ;
#35997 = ADVANCED_FACE ( 'NONE', ( #68256 ), #23250, .T. ) ;
#35998 = DIRECTION ( 'NONE',  ( 0.7071067811865487940, 0.7071067811865463515, 0.000000000000000000 ) ) ;
#35999 = LINE ( 'NONE', #114244, #96924 ) ;
#36000 = CARTESIAN_POINT ( 'NONE',  ( 127.9537635252314658, -6.109999999999999432, -3.741295971395163529E-16 ) ) ;
#36001 = ORIENTED_EDGE ( 'NONE', *, *, #34001, .T. ) ;
#36002 = DIRECTION ( 'NONE',  ( -0.6830127018922180770, -0.6830127018922204085, -0.2588190451025214056 ) ) ;
#36003 = VECTOR ( 'NONE', #2095, 1000.000000000000227 ) ;
#36004 = ORIENTED_EDGE ( 'NONE', *, *, #47644, .T. ) ;
#36005 = ORIENTED_EDGE ( 'NONE', *, *, #77932, .F. ) ;
#36006 = ORIENTED_EDGE ( 'NONE', *, *, #42917, .F. ) ;
#36007 = DIRECTION ( 'NONE',  ( -0.7071067811865487940, 0.7071067811865463515, -0.000000000000000000 ) ) ;
#36008 = PLANE ( 'NONE',  #116289 ) ;
#36009 = ADVANCED_FACE ( 'NONE', ( #10934 ), #45776, .F. ) ;
#36010 = DIRECTION ( 'NONE',  ( -0.7071067811865486830, 0.7071067811865464625, 0.000000000000000000 ) ) ;
#36011 = DIRECTION ( 'NONE',  ( 0.7071067811865486830, -0.7071067811865464625, -0.000000000000000000 ) ) ;
#36012 = EDGE_CURVE ( 'NONE', #8053, #645, #2191, .T. ) ;
#36013 = CARTESIAN_POINT ( 'NONE',  ( 1.499999999999987566, -1.592773361805372545, -6.492772025301233541 ) ) ;
#36014 = VERTEX_POINT ( 'NONE', #56672 ) ;
#36015 = DIRECTION ( 'NONE',  ( -0.000000000000000000, -0.3543493200069152693, 0.9351131265310292928 ) ) ;
#36016 = ADVANCED_FACE ( 'NONE', ( #99376 ), #34890, .F. ) ;
#36017 = AXIS2_PLACEMENT_3D ( 'NONE', #31086, #109340, #18736 ) ;
#36018 = CARTESIAN_POINT ( 'NONE',  ( 19.81206980810188156, 7.934999999999993392, 2.126176841940951689 ) ) ;
#36019 = LINE ( 'NONE', #80240, #141190 ) ;
#36020 = VECTOR ( 'NONE', #135569, 1000.000000000000000 ) ;
#36021 = LINE ( 'NONE', #1197, #73850 ) ;
#36022 = VECTOR ( 'NONE', #42383, 1000.000000000000000 ) ;
#36023 = CARTESIAN_POINT ( 'NONE',  ( -9.299744871391588674, -27.71228299555212971, 4.000000000000000000 ) ) ;
#36024 = ORIENTED_EDGE ( 'NONE', *, *, #109016, .F. ) ;
#36025 = EDGE_LOOP ( 'NONE', ( #88606, #40614, #16312, #51333 ) ) ;
#36026 = ORIENTED_EDGE ( 'NONE', *, *, #36653, .T. ) ;
#36027 = LINE ( 'NONE', #135342, #27830 ) ;
#36028 = CARTESIAN_POINT ( 'NONE',  ( 30.48921356237309510, -27.52281430457076894, 5.000000000000000000 ) ) ;
#36029 = UNCERTAINTY_MEASURE_WITH_UNIT (LENGTH_MEASURE( 1.000000000000000082E-05 ), #89960, 'distance_accuracy_value', 'NONE');
#36030 = EDGE_CURVE ( 'NONE', #92661, #133264, #46513, .T. ) ;
#36031 = VECTOR ( 'NONE', #119271, 1000.000000000000000 ) ;
#36032 = CARTESIAN_POINT ( 'NONE',  ( 21.29974487139158512, -27.71228299555221142, 4.000000000000000000 ) ) ;
#36033 = CARTESIAN_POINT ( 'NONE',  ( -6.183988606268994381, 28.73617430169791476, 5.000000000000000000 ) ) ;
#36034 = CARTESIAN_POINT ( 'NONE',  ( 8.899418659112473762, 8.548380951428034891, 4.146088043936330791 ) ) ;
#36035 = DIRECTION ( 'NONE',  ( -0.7071067811865487940, 0.7071067811865463515, -0.000000000000000000 ) ) ;
#36036 = DIRECTION ( 'NONE',  ( 0.7071067811865487940, 0.7071067811865463515, 0.000000000000000000 ) ) ;
#36037 = DIRECTION ( 'NONE',  ( -0.7071067811865487940, 0.7071067811865463515, -0.000000000000000000 ) ) ;
#36038 = CARTESIAN_POINT ( 'NONE',  ( 18.01107201284014536, 3.821174125832445049E-16, 0.000000000000000000 ) ) ;
#36039 = LINE ( 'NONE', #2649, #16397 ) ;
#36040 = EDGE_CURVE ( 'NONE', #18692, #143444, #142912, .T. ) ;
#36041 = VERTEX_POINT ( 'NONE', #88557 ) ;
#36042 = CARTESIAN_POINT ( 'NONE',  ( 16.98219951865394606, -0.6360915077794555561, -31.34035742411751713 ) ) ;
#36043 = VERTEX_POINT ( 'NONE', #100834 ) ;
#36044 = CARTESIAN_POINT ( 'NONE',  ( 54.18398860626899705, 28.73617430169825226, 5.000000000000000000 ) ) ;
#36046 = EDGE_LOOP ( 'NONE', ( #52525, #136401, #57907, #11515 ) ) ;
#36045 = CARTESIAN_POINT ( 'NONE',  ( 2.483345613589531542, 22.22500000000000142, 4.500000000000000888 ) ) ;
#36047 = FACE_OUTER_BOUND ( 'NONE', #131310, .T. ) ;
#36048 = CARTESIAN_POINT ( 'NONE',  ( 26.21837311707487572, 21.74787736706806740, 4.999607392498048419 ) ) ;
#36049 = ORIENTED_EDGE ( 'NONE', *, *, #9807, .F. ) ;
#36050 = CARTESIAN_POINT ( 'NONE',  ( 3.799968779831609744, 8.259292476615627265, 16.85664084051840206 ) ) ;
#36051 = ORIENTED_EDGE ( 'NONE', *, *, #126864, .F. ) ;
#36052 = CARTESIAN_POINT ( 'NONE',  ( 45.29974487139158867, -27.71228299555237840, 4.000000000000000000 ) ) ;
#36053 = ORIENTED_EDGE ( 'NONE', *, *, #99117, .T. ) ;
#36054 = LINE ( 'NONE', #14272, #40649 ) ;
#36055 = EDGE_CURVE ( 'NONE', #137381, #62440, #110965, .T. ) ;
#36056 = CARTESIAN_POINT ( 'NONE',  ( 104.4958603837962272, -3.974999999999998312, -6.884901960086286188 ) ) ;
#36057 = CARTESIAN_POINT ( 'NONE',  ( 29.29289321881324781, 20.25929247661551713, 5.000000000000000000 ) ) ;
#36058 = ORIENTED_EDGE ( 'NONE', *, *, #24463, .T. ) ;
#36059 = FACE_OUTER_BOUND ( 'NONE', #105938, .T. ) ;
#36060 = PLANE ( 'NONE',  #91257 ) ;
#36061 = CARTESIAN_POINT ( 'NONE',  ( 9.299744871391588674, -27.71228299555212971, 4.000000000000000000 ) ) ;
#36062 = CARTESIAN_POINT ( 'NONE',  ( 11.52083333333333393, -6.094999999999989981, -1.633150327867689100 ) ) ;
#36063 = DIRECTION ( 'NONE',  ( 0.7071067811865486830, -0.7071067811865464625, -0.000000000000000000 ) ) ;
#36064 = CARTESIAN_POINT ( 'NONE',  ( -60.48921356237309510, -27.52281430457097500, 5.000000000000000000 ) ) ;
#36065 = DIRECTION ( 'NONE',  ( 0.7071067811865487940, 0.7071067811865463515, 0.000000000000000000 ) ) ;
#36066 = VERTEX_POINT ( 'NONE', #76980 ) ;
#36067 = FACE_OUTER_BOUND ( 'NONE', #136843, .T. ) ;
#36068 = VERTEX_POINT ( 'NONE', #121148 ) ;
#36069 = EDGE_CURVE ( 'NONE', #123911, #626, #78382, .T. ) ;
#36070 = CARTESIAN_POINT ( 'NONE',  ( 97.85459685856477563, -1.637169565754161615, 6.110000000000000320 ) ) ;
#36071 = DIRECTION ( 'NONE',  ( -0.7071067811865486830, 0.7071067811865464625, 0.000000000000000000 ) ) ;
#36072 = DIRECTION ( 'NONE',  ( -0.000000000000000000, -0.3543493200069152693, 0.9351131265310292928 ) ) ;
#36073 = PLANE ( 'NONE',  #30806 ) ;
#36074 = CARTESIAN_POINT ( 'NONE',  ( -6.183988606268994381, 28.73617430169791476, 5.000000000000000000 ) ) ;
#36075 = EDGE_LOOP ( 'NONE', ( #58018, #138690, #19871, #130948, #12366, #28392, #79437, #68239, #119767, #74514, #19024, #141863, #33295, #79184 ) ) ;
#36076 = CARTESIAN_POINT ( 'NONE',  ( -21.18398860626899349, 28.73617430169802134, 5.000000000000000000 ) ) ;
#36077 =( BOUNDED_CURVE ( )  B_SPLINE_CURVE ( 3, ( #7279, #129077, #30503, #42817 ),
 .UNSPECIFIED., .F., .T. ) 
 B_SPLINE_CURVE_WITH_KNOTS ( ( 4, 4 ),
 ( 5.005968288816727174, 5.074607125596342527 ),
 .UNSPECIFIED. ) 
 CURVE ( )  GEOMETRIC_REPRESENTATION_ITEM ( )  RATIONAL_B_SPLINE_CURVE ( ( 1.000000000000000000, 0.9996074310407763175, 0.9996074310407763175, 1.000000000000000000 ) ) 
 REPRESENTATION_ITEM ( '' )  );
#36078 = CARTESIAN_POINT ( 'NONE',  ( -22.49999999999984723, 16.18958161055400069, -11.56426086740816217 ) ) ;
#36079 = ORIENTED_EDGE ( 'NONE', *, *, #9422, .T. ) ;
#36080 = LINE ( 'NONE', #25168, #23030 ) ;
#36081 = ADVANCED_FACE ( 'NONE', ( #1489 ), #110257, .F. ) ;
#36082 = CARTESIAN_POINT ( 'NONE',  ( 29.99451991528749417, 28.92564299267958816, 4.000000000000000000 ) ) ;
#36084 = VERTEX_POINT ( 'NONE', #121845 ) ;
#36083 = LINE ( 'NONE', #38215, #17334 ) ;
#36085 = CARTESIAN_POINT ( 'NONE',  ( 32.67183060077624646, -21.74070752338406010, 4.000000000000000000 ) ) ;
#36086 = DIRECTION ( 'NONE',  ( -0.000000000000000000, 0.000000000000000000, 1.000000000000000000 ) ) ;
#36087 = LINE ( 'NONE', #124500, #47073 ) ;
#36088 = CARTESIAN_POINT ( 'NONE',  ( -27.79289321881326558, -2.240707523384257716, 5.000000000000000000 ) ) ;
#36089 = DIRECTION ( 'NONE',  ( -0.000000000000000000, -1.000000000000000000, -0.000000000000000000 ) ) ;
#36090 = ORIENTED_EDGE ( 'NONE', *, *, #25926, .T. ) ;
#36091 = CONICAL_SURFACE ( 'NONE', #89361, 2.500000000000000444, 0.9599310885968830309 ) ;
#36092 = ORIENTED_EDGE ( 'NONE', *, *, #57189, .F. ) ;
#36093 = ORIENTED_EDGE ( 'NONE', *, *, #68249, .T. ) ;
#36094 = CARTESIAN_POINT ( 'NONE',  ( 87.79209685856477563, -5.291415217122921177, 3.054999999999999272 ) ) ;
#36095 = ORIENTED_EDGE ( 'NONE', *, *, #45996, .F. ) ;
#36096 = CIRCLE ( 'NONE', #135628, 2.500000000000000444 ) ;
#36097 = LINE ( 'NONE', #36776, #23140 ) ;
#36098 = EDGE_CURVE ( 'NONE', #106128, #75266, #784, .T. ) ;
#36099 = DIRECTION ( 'NONE',  ( 0.000000000000000000, 0.000000000000000000, -1.000000000000000000 ) ) ;
#36100 = CARTESIAN_POINT ( 'NONE',  ( 14.08373646989360317, 3.821174125832445049E-16, 0.000000000000000000 ) ) ;
#36101 = PLANE ( 'NONE',  #75520 ) ;
#36102 = ORIENTED_EDGE ( 'NONE', *, *, #56927, .T. ) ;
#36103 = LINE ( 'NONE', #12175, #123000 ) ;
#36104 = LINE ( 'NONE', #3427, #127551 ) ;
#36105 = CARTESIAN_POINT ( 'NONE',  ( 77.05793019189810877, 6.110000000000000320, -1.637169565754156064 ) ) ;
#36106 = VERTEX_POINT ( 'NONE', #123332 ) ;
#36107 = EDGE_CURVE ( 'NONE', #140203, #42790, #52091, .T. ) ;
#36108 = DIRECTION ( 'NONE',  ( -0.6830127018922180770, -0.6830127018922204085, -0.2588190451025213501 ) ) ;
#36109 = LINE ( 'NONE', #81772, #19161 ) ;
#36110 = ORIENTED_EDGE ( 'NONE', *, *, #33602, .T. ) ;
#36111 = ORIENTED_EDGE ( 'NONE', *, *, #73514, .T. ) ;
#36112 = EDGE_CURVE ( 'NONE', #113088, #15312, #75990, .T. ) ;
#36113 = DIRECTION ( 'NONE',  ( -0.000000000000000000, -0.3543493200069152693, 0.9351131265310292928 ) ) ;
#36114 = EDGE_CURVE ( 'NONE', #90068, #108003, #42672, .T. ) ;
#36115 = CARTESIAN_POINT ( 'NONE',  ( 28.49999999999980815, 12.43112307739205669, 4.000000000000000000 ) ) ;
#36116 = CARTESIAN_POINT ( 'NONE',  ( 24.42123647476855552, -9.717572351234235426E-16, -7.934999999999990727 ) ) ;
#36117 = CARTESIAN_POINT ( 'NONE',  ( 6.299744871391586898, -27.71228299555210484, 4.000000000000000000 ) ) ;
#36118 =( LENGTH_UNIT ( ) NAMED_UNIT ( * ) SI_UNIT ( .MILLI., .METRE. ) );
#36119 = CIRCLE ( 'NONE', #117101, 2.500000000000000444 ) ;
#36120 = LINE ( 'NONE', #80345, #20966 ) ;
#36121 = FACE_OUTER_BOUND ( 'NONE', #61391, .T. ) ;
#36122 = VECTOR ( 'NONE', #100265, 1000.000000000000000 ) ;
#36123 = ORIENTED_EDGE ( 'NONE', *, *, #25908, .F. ) ;
#36125 = ORIENTED_EDGE ( 'NONE', *, *, #107903, .F. ) ;
#36124 = AXIS2_PLACEMENT_3D ( 'NONE', #107992, #111588, #12267 ) ;
#36126 = VECTOR ( 'NONE', #120346, 1000.000000000000000 ) ;
#36127 = CARTESIAN_POINT ( 'NONE',  ( 9.625000000000001776, 6.094999999999989981, -1.119633336120465690E-15 ) ) ;
#36128 = ORIENTED_EDGE ( 'NONE', *, *, #72165, .F. ) ;
#36129 = ORIENTED_EDGE ( 'NONE', *, *, #23139, .F. ) ;
#36130 = ADVANCED_FACE ( 'NONE', ( #118018 ), #83290, .T. ) ;
#36131 = DIRECTION ( 'NONE',  ( -0.000000000000000000, -0.3543493200069152693, 0.9351131265310292928 ) ) ;
#36132 = VERTEX_POINT ( 'NONE', #143375 ) ;
#36133 = DIRECTION ( 'NONE',  ( -0.7071067811865487940, 0.7071067811865463515, -0.000000000000000000 ) ) ;
#36134 = CARTESIAN_POINT ( 'NONE',  ( 127.0000000000000000, 0.000000000000000000, 0.000000000000000000 ) ) ;
#36135 = DIRECTION ( 'NONE',  ( -0.000000000000000000, 0.3543493200069153248, 0.9351131265310292928 ) ) ;
#36136 = CARTESIAN_POINT ( 'NONE',  ( 54.48921356237310221, -27.52281430457093236, 5.000000000000000000 ) ) ;
#36137 = EDGE_LOOP ( 'NONE', ( #38640, #8921, #112849, #64653 ) ) ;
#36138 = CARTESIAN_POINT ( 'NONE',  ( -9.183988606268997046, 28.73617430169793607, 5.000000000000000000 ) ) ;
#36139 = CARTESIAN_POINT ( 'NONE',  ( 34.42499999999998295, 0.000000000000000000, 4.500000000000000888 ) ) ;
#36140 = ORIENTED_EDGE ( 'NONE', *, *, #61936, .F. ) ;
#36141 = PLANE ( 'NONE',  #140697 ) ;
#36142 = EDGE_LOOP ( 'NONE', ( #78302, #41273, #22125, #94739 ) ) ;
#36143 = ORIENTED_EDGE ( 'NONE', *, *, #72802, .F. ) ;
#36144 = FACE_OUTER_BOUND ( 'NONE', #84147, .T. ) ;
#36145 = ORIENTED_EDGE ( 'NONE', *, *, #104833, .T. ) ;
#36146 = ORIENTED_EDGE ( 'NONE', *, *, #15457, .T. ) ;
#36147 = DIRECTION ( 'NONE',  ( 1.734723475976806848E-16, -1.000000000000000000, 0.000000000000000000 ) ) ;
#36148 = ORIENTED_EDGE ( 'NONE', *, *, #136100, .F. ) ;
#36149 = ADVANCED_FACE ( 'NONE', ( #65137 ), #96269, .T. ) ;
#36150 = CARTESIAN_POINT ( 'NONE',  ( -5.187538124160488984, -22.22500000000000142, 4.000000000000000000 ) ) ;
#36151 = CARTESIAN_POINT ( 'NONE',  ( 115.5004301918981042, -3.055000000000002380, 5.291415217122920289 ) ) ;
#36152 = DIRECTION ( 'NONE',  ( -0.6830127018922181881, 0.6830127018922202975, -0.2588190451025214056 ) ) ;
#36153 = EDGE_CURVE ( 'NONE', #81705, #122500, #41204, .T. ) ;
#36154 = DIRECTION ( 'NONE',  ( -0.7071067811865486830, -0.7071067811865464625, 0.000000000000000000 ) ) ;
#36155 = CARTESIAN_POINT ( 'NONE',  ( 55.56056557994608625, -49.14999999999999147, 39.86617647058822200 ) ) ;
#36156 = CARTESIAN_POINT ( 'NONE',  ( -1.171830600776463838, 6.759292476615656575, 4.000000000000000000 ) ) ;
#36157 = VECTOR ( 'NONE', #28036, 1000.000000000000000 ) ;
#36158 = FACE_OUTER_BOUND ( 'NONE', #2121, .T. ) ;
#36159 = EDGE_CURVE ( 'NONE', #2613, #123729, #21610, .T. ) ;
#36160 = EDGE_CURVE ( 'NONE', #49304, #2022, #30337, .T. ) ;
#36161 = CARTESIAN_POINT ( 'NONE',  ( 34.49999999999976552, 4.464255608400454101, 4.994342998332159667 ) ) ;
#36162 = VERTEX_POINT ( 'NONE', #120159 ) ;
#36163 = CARTESIAN_POINT ( 'NONE',  ( 66.18398860626901126, 28.73617430169833753, 5.000000000000000000 ) ) ;
#36164 = DIRECTION ( 'NONE',  ( 0.6830127018922180770, -0.6830127018922204085, -0.2588190451025213501 ) ) ;
#36165 = ORIENTED_EDGE ( 'NONE', *, *, #56773, .T. ) ;
#36166 = VERTEX_POINT ( 'NONE', #75293 ) ;
#36167 = CARTESIAN_POINT ( 'NONE',  ( -22.49999999999983302, 16.46639925780209879, 5.000000000000000000 ) ) ;
#36168 = ORIENTED_EDGE ( 'NONE', *, *, #75287, .F. ) ;
#36169 = DIRECTION ( 'NONE',  ( -1.000000000000000000, -1.224606353822377258E-16, -0.000000000000000000 ) ) ;
#36170 = CARTESIAN_POINT ( 'NONE',  ( 114.3124999999999858, 5.819803920172571310, 5.819803920172576639 ) ) ;
#36171 = EDGE_CURVE ( 'NONE', #566, #4002, #44085, .T. ) ;
#36172 = DIRECTION ( 'NONE',  ( 0.3543493200069162685, -0.000000000000000000, -0.9351131265310288487 ) ) ;
#36173 = EDGE_CURVE ( 'NONE', #131559, #91102, #119458, .T. ) ;
#36174 = DIRECTION ( 'NONE',  ( 0.6830127018922180770, -0.6830127018922204085, -0.2588190451025213501 ) ) ;
#36175 = ORIENTED_EDGE ( 'NONE', *, *, #121610, .F. ) ;
#36176 =( LENGTH_UNIT ( ) NAMED_UNIT ( * ) SI_UNIT ( .MILLI., .METRE. ) );
#36177 = VERTEX_POINT ( 'NONE', #141228 ) ;
#36178 = FACE_OUTER_BOUND ( 'NONE', #31978, .T. ) ;
#36179 = CIRCLE ( 'NONE', #119534, 5.999999999999998224 ) ;
#36180 = CARTESIAN_POINT ( 'NONE',  ( 30.98373647476855552, -5.808823158059035485, -5.808823158059033709 ) ) ;
#36181 = VERTEX_POINT ( 'NONE', #128933 ) ;
#36182 = EDGE_CURVE ( 'NONE', #118081, #127894, #41943, .T. ) ;
#36183 = DIRECTION ( 'NONE',  ( 0.7071067811865487940, 0.7071067811865463515, -0.000000000000000000 ) ) ;
#36184 = VECTOR ( 'NONE', #124534, 1000.000000000000000 ) ;
#36185 = DIRECTION ( 'NONE',  ( -0.7071067811865486830, -0.7071067811865464625, 0.000000000000000000 ) ) ;
#36186 = VERTEX_POINT ( 'NONE', #73844 ) ;
#36187 = VERTEX_POINT ( 'NONE', #63000 ) ;
#36188 = ORIENTED_EDGE ( 'NONE', *, *, #130696, .T. ) ;
#36189 = CARTESIAN_POINT ( 'NONE',  ( -1.499999999999987566, -8.568876922607726598, 4.000000000000000000 ) ) ;
#36190 = EDGE_CURVE ( 'NONE', #9326, #10796, #107174, .T. ) ;
#36191 = FACE_OUTER_BOUND ( 'NONE', #120811, .T. ) ;
#36192 = DIRECTION ( 'NONE',  ( -0.6830127018922180770, -0.6830127018922204085, -0.2588190451025213501 ) ) ;
#36193 = ORIENTED_EDGE ( 'NONE', *, *, #69297, .F. ) ;
#36194 = CARTESIAN_POINT ( 'NONE',  ( 0.005480084712502889671, 28.92564299267938210, 4.000000000000000000 ) ) ;
#36195 = LINE ( 'NONE', #56564, #36451 ) ;
#36196 = DIRECTION ( 'NONE',  ( -0.7071067811865486830, -0.7071067811865464625, 0.000000000000000000 ) ) ;
#36197 = DIRECTION ( 'NONE',  ( -0.000000000000000000, 0.3543493200069153248, 0.9351131265310292928 ) ) ;
#36198 = VERTEX_POINT ( 'NONE', #12144 ) ;
#36199 = EDGE_CURVE ( 'NONE', #86975, #70673, #22280, .T. ) ;
#36200 = CARTESIAN_POINT ( 'NONE',  ( -34.49999999999975842, 22.08746187583901843, 4.000000000000000000 ) ) ;
#36201 = ORIENTED_EDGE ( 'NONE', *, *, #74291, .F. ) ;
#36203 = ORIENTED_EDGE ( 'NONE', *, *, #127176, .F. ) ;
#36202 = CARTESIAN_POINT ( 'NONE',  ( 57.48282408946054289, -47.13357697190244266, -36.34567044386321299 ) ) ;
#36204 = CIRCLE ( 'NONE', #68928, 6.000000000000000000 ) ;
#36205 = ORIENTED_EDGE ( 'NONE', *, *, #31217, .T. ) ;
#36206 = EDGE_CURVE ( 'NONE', #52654, #2296, #124485, .T. ) ;
#36207 = LINE ( 'NONE', #69569, #132701 ) ;
#36209 = ADVANCED_FACE ( 'NONE', ( #102024 ), #102747, .T. ) ;
#36208 = CARTESIAN_POINT ( 'NONE',  ( 105.7083333333333286, -3.974999999999999201, -6.884901960086287964 ) ) ;
#36210 = ORIENTED_EDGE ( 'NONE', *, *, #48686, .F. ) ;
#36211 = UNCERTAINTY_MEASURE_WITH_UNIT (LENGTH_MEASURE( 1.000000000000000082E-05 ), #137323, 'distance_accuracy_value', 'NONE');
#36212 = ORIENTED_EDGE ( 'NONE', *, *, #55197, .T. ) ;
#36213 = AXIS2_PLACEMENT_3D ( 'NONE', #93132, #82976, #103274 ) ;
#36214 = VECTOR ( 'NONE', #93849, 1000.000000000000000 ) ;
#36215 = DIRECTION ( 'NONE',  ( -0.000000000000000000, 0.000000000000000000, 1.000000000000000000 ) ) ;
#36216 = DIRECTION ( 'NONE',  ( -0.000000000000000000, 0.000000000000000000, 1.000000000000000000 ) ) ;
#36217 = EDGE_CURVE ( 'NONE', #124676, #13638, #66547, .T. ) ;
#36218 = CARTESIAN_POINT ( 'NONE',  ( -33.29974487139158867, -27.71228299555229313, 4.000000000000000000 ) ) ;
#36219 = DIRECTION ( 'NONE',  ( -1.000000000000000000, -0.000000000000000000, -0.000000000000000000 ) ) ;
#36220 = CARTESIAN_POINT ( 'NONE',  ( 54.18398860626899705, 28.73617430169825226, 5.000000000000000000 ) ) ;
#36221 = FACE_OUTER_BOUND ( 'NONE', #19429, .T. ) ;
#36222 = CARTESIAN_POINT ( 'NONE',  ( 8.897059064271770623, -2.055000000000000160, 0.000000000000000000 ) ) ;
#36223 = DIRECTION ( 'NONE',  ( -0.000000000000000000, 1.000000000000000000, -0.000000000000000000 ) ) ;
#36224 = CARTESIAN_POINT ( 'NONE',  ( 20.10373647476854941, 5.808823158059036373, 5.808823158059032821 ) ) ;
#36225 = CARTESIAN_POINT ( 'NONE',  ( 54.18398860626899705, 28.73617430169825226, 5.000000000000000000 ) ) ;
#36226 = DIRECTION ( 'NONE',  ( -0.3543493200069162685, -0.000000000000000000, -0.9351131265310288487 ) ) ;
#36227 = VECTOR ( 'NONE', #135386, 1000.000000000000227 ) ;
#36228 = EDGE_CURVE ( 'NONE', #73728, #140080, #68701, .T. ) ;
#36229 = LINE ( 'NONE', #80455, #120739 ) ;
#36230 = PLANE ( 'NONE',  #94044 ) ;
#36231 = EDGE_LOOP ( 'NONE', ( #27364, #54235, #10106, #103006 ) ) ;
#36232 = ORIENTED_EDGE ( 'NONE', *, *, #86404, .F. ) ;
#36233 = CARTESIAN_POINT ( 'NONE',  ( 88.50000000000000000, 0.000000000000000000, -7.950000000000000178 ) ) ;
#36234 = ORIENTED_EDGE ( 'NONE', *, *, #36482, .F. ) ;
#36235 = ORIENTED_EDGE ( 'NONE', *, *, #67824, .T. ) ;
#36236 = VERTEX_POINT ( 'NONE', #77449 ) ;
#36237 = CARTESIAN_POINT ( 'NONE',  ( -24.70710678118636139, -18.74070752338408852, 5.000000000000000000 ) ) ;
#36238 = CARTESIAN_POINT ( 'NONE',  ( -34.92500000000001137, 5.816654386410375466, 4.500000000000000888 ) ) ;
#36239 = LINE ( 'NONE', #68882, #31552 ) ;
#36240 = ORIENTED_EDGE ( 'NONE', *, *, #92054, .F. ) ;
#36241 = DIRECTION ( 'NONE',  ( 1.000000000000000000, 0.000000000000000000, 0.000000000000000000 ) ) ;
#36242 = PLANE ( 'NONE',  #39560 ) ;
#36243 = CARTESIAN_POINT ( 'NONE',  ( 0.000000000000000000, 0.000000000000000000, 5.000000000000000000 ) ) ;
#36244 = DIRECTION ( 'NONE',  ( 0.7071067811865486830, -0.7071067811865464625, -0.000000000000000000 ) ) ;
#36245 = FACE_OUTER_BOUND ( 'NONE', #17342, .T. ) ;
#36246 = DIRECTION ( 'NONE',  ( 1.000000000000000000, 0.000000000000000000, 0.000000000000000000 ) ) ;
#36247 = LINE ( 'NONE', #80477, #10283 ) ;
#36248 = PLANE ( 'NONE',  #111611 ) ;
#36249 = CARTESIAN_POINT ( 'NONE',  ( 27.00000000000001066, 4.895760287860418281, 5.464752967159129504 ) ) ;
#36250 = LINE ( 'NONE', #125399, #28396 ) ;
#36251 = DIRECTION ( 'NONE',  ( -1.000000000000000000, -1.224606353822377258E-16, -0.000000000000000000 ) ) ;
#36252 = CARTESIAN_POINT ( 'NONE',  ( 153.4000000000000057, 26.96999999999993847, 34.92499999999998295 ) ) ;
#36253 = DIRECTION ( 'NONE',  ( 0.6830127018922181881, 0.6830127018922202975, -0.2588190451025214056 ) ) ;
#36254 = ORIENTED_EDGE ( 'NONE', *, *, #91620, .F. ) ;
#36255 = VERTEX_POINT ( 'NONE', #100608 ) ;
#36256 = CARTESIAN_POINT ( 'NONE',  ( 113.1670968585647756, -3.055000000000000160, -5.291415217122921177 ) ) ;
#36257 = VECTOR ( 'NONE', #25266, 1000.000000000000227 ) ;
#36258 = EDGE_LOOP ( 'NONE', ( #81019, #117487, #72812, #96289 ) ) ;
#36259 = EDGE_CURVE ( 'NONE', #19670, #107544, #11397, .T. ) ;
#36260 = DIRECTION ( 'NONE',  ( -0.3543493200069162685, -0.000000000000000000, -0.9351131265310288487 ) ) ;
#36261 = VECTOR ( 'NONE', #108770, 1000.000000000000000 ) ;
#36263 = AXIS2_PLACEMENT_3D ( 'NONE', #27943, #106182, #29353 ) ;
#36262 = LINE ( 'NONE', #123287, #15556 ) ;
#36264 = CARTESIAN_POINT ( 'NONE',  ( 13.18000000000000149, 9.521314400968980422E-16, 0.000000000000000000 ) ) ;
#36265 = CARTESIAN_POINT ( 'NONE',  ( -26.99999999999980815, -19.44781430457063465, 5.000000000000000000 ) ) ;
#36266 = CARTESIAN_POINT ( 'NONE',  ( 107.8287635252314516, 0.000000000000000000, -6.109999999999998543 ) ) ;
#36267 = VERTEX_POINT ( 'NONE', #78866 ) ;
#36268 = VERTEX_POINT ( 'NONE', #45536 ) ;
#36269 = CARTESIAN_POINT ( 'NONE',  ( 45.18398860626900415, 28.73617430169818832, 5.000000000000000000 ) ) ;
#36270 = VECTOR ( 'NONE', #98946, 1000.000000000000000 ) ;
#36271 = DIRECTION ( 'NONE',  ( -0.3543493200069163240, 4.681814790819596721E-17, -0.9351131265310288487 ) ) ;
#36272 = ORIENTED_EDGE ( 'NONE', *, *, #88963, .T. ) ;
#36273 = ORIENTED_EDGE ( 'NONE', *, *, #141008, .T. ) ;
#36274 = EDGE_CURVE ( 'NONE', #134985, #135515, #111461, .T. ) ;
#36275 = EDGE_LOOP ( 'NONE', ( #116662, #65456, #4099, #136208 ) ) ;
#36276 = CARTESIAN_POINT ( 'NONE',  ( 5.691592354503320905, 9.902892378096218942E-16, 0.000000000000000000 ) ) ;
#36277 = EDGE_CURVE ( 'NONE', #33545, #108193, #23750, .T. ) ;
#36278 =( NAMED_UNIT ( * ) SI_UNIT ( $, .STERADIAN. ) SOLID_ANGLE_UNIT ( ) );
#36279 = CARTESIAN_POINT ( 'NONE',  ( 27.76626352523143737, 4.472830434245839371, -4.472830434245838482 ) ) ;
#36280 = EDGE_LOOP ( 'NONE', ( #11678, #121479, #38536, #22817 ) ) ;
#36281 = MECHANICAL_DESIGN_GEOMETRIC_PRESENTATION_REPRESENTATION (  '', ( #10780 ), #103410 ) ;
#36283 = ORIENTED_EDGE ( 'NONE', *, *, #123186, .F. ) ;
#36282 = EDGE_CURVE ( 'NONE', #26660, #76331, #88305, .T. ) ;
#36284 = FACE_OUTER_BOUND ( 'NONE', #71984, .T. ) ;
#36285 = ORIENTED_EDGE ( 'NONE', *, *, #47505, .T. ) ;
#36286 = COLOUR_RGB ( '', 0.31764706, 0.68627451, 0.89019608) ;
#36287 = VERTEX_POINT ( 'NONE', #121612 ) ;
#36288 = LINE ( 'NONE', #69651, #3073 ) ;
#36289 = EDGE_CURVE ( 'NONE', #57345, #106069, #99878, .T. ) ;
#36290 = CARTESIAN_POINT ( 'NONE',  ( -8.510786437626906675, -27.52281430457049183, 5.000000000000000000 ) ) ;
#36291 = CARTESIAN_POINT ( 'NONE',  ( 6.938893903907228378E-15, 1.552185695429151080, 5.000000000000000000 ) ) ;
#36292 = ORIENTED_EDGE ( 'NONE', *, *, #5719, .T. ) ;
#36293 = FACE_OUTER_BOUND ( 'NONE', #124424, .T. ) ;
#36294 = DIRECTION ( 'NONE',  ( -0.000000000000000000, 0.3543493200069153248, 0.9351131265310292928 ) ) ;
#36295 = EDGE_CURVE ( 'NONE', #94183, #6499, #544, .T. ) ;
#36296 = SURFACE_STYLE_FILL_AREA ( #36989 ) ;
#36298 = FACE_BOUND ( 'NONE', #111974, .T. ) ;
#36297 = VECTOR ( 'NONE', #18397, 1000.000000000000000 ) ;
#36299 = ORIENTED_EDGE ( 'NONE', *, *, #71559, .F. ) ;
#36300 = LINE ( 'NONE', #115229, #87495 ) ;
#36301 = LINE ( 'NONE', #90695, #9004 ) ;
#36302 = LINE ( 'NONE', #102984, #90829 ) ;
#36303 = ORIENTED_EDGE ( 'NONE', *, *, #97767, .T. ) ;
#36304 = CARTESIAN_POINT ( 'NONE',  ( 31.82816939922330945, 3.759292476615683665, 4.000000000000000000 ) ) ;
#36305 = ORIENTED_EDGE ( 'NONE', *, *, #65291, .T. ) ;
#36307 = ORIENTED_EDGE ( 'NONE', *, *, #56724, .F. ) ;
#36306 = EDGE_CURVE ( 'NONE', #93602, #77576, #89029, .T. ) ;
#36308 = AXIS2_PLACEMENT_3D ( 'NONE', #8065, #42173, #28434 ) ;
#36309 = VERTEX_POINT ( 'NONE', #80297 ) ;
#36310 = VECTOR ( 'NONE', #39322, 1000.000000000000000 ) ;
#36311 = VECTOR ( 'NONE', #55329, 1000.000000000000000 ) ;
#36312 = CARTESIAN_POINT ( 'NONE',  ( 40.30793019189810877, -6.109999999999998543, 1.637169565754158507 ) ) ;
#36313 = VERTEX_POINT ( 'NONE', #133247 ) ;
#36314 = LINE ( 'NONE', #136321, #11634 ) ;
#36315 = PLANE ( 'NONE',  #126094 ) ;
#36316 = ADVANCED_FACE ( 'NONE', ( #13555 ), #33925, .T. ) ;
#36317 = VERTEX_POINT ( 'NONE', #57125 ) ;
#36318 = CARTESIAN_POINT ( 'NONE',  ( 33.48921356237309510, -27.52281430457078670, 5.000000000000000000 ) ) ;
#36319 = FACE_OUTER_BOUND ( 'NONE', #8582, .T. ) ;
#36320 = VECTOR ( 'NONE', #101671, 1000.000000000000000 ) ;
#36321 = CARTESIAN_POINT ( 'NONE',  ( 11.99999999999991296, 10.21212019023810136, -2.019456568337826496 ) ) ;
#36322 = ADVANCED_FACE ( 'NONE', ( #101304 ), #1941, .F. ) ;
#36323 = ADVANCED_FACE ( 'NONE', ( #103423 ), #8202, .F. ) ;
#36324 = CARTESIAN_POINT ( 'NONE',  ( 15.18398860626900237, 28.73617430169797871, 5.000000000000000000 ) ) ;
#36325 = LINE ( 'NONE', #71109, #122725 ) ;
#36326 = LINE ( 'NONE', #55955, #104956 ) ;
#36327 = ORIENTED_EDGE ( 'NONE', *, *, #120380, .T. ) ;
#36328 = ORIENTED_EDGE ( 'NONE', *, *, #62528, .T. ) ;
#36329 = ORIENTED_EDGE ( 'NONE', *, *, #127291, .T. ) ;
#36330 = ORIENTED_EDGE ( 'NONE', *, *, #114337, .T. ) ;
#36331 = CARTESIAN_POINT ( 'NONE',  ( 0.000000000000000000, 0.000000000000000000, 5.000000000000000000 ) ) ;
#36332 = EDGE_LOOP ( 'NONE', ( #25328, #33665, #125621, #27262 ) ) ;
#36333 = EDGE_CURVE ( 'NONE', #69752, #68093, #91847, .T. ) ;
#36334 = ORIENTED_EDGE ( 'NONE', *, *, #50733, .T. ) ;
#36335 = CARTESIAN_POINT ( 'NONE',  ( -5.908046338136182740, 22.22500000000000142, 15.99560845316876012 ) ) ;
#36336 = ADVANCED_FACE ( 'NONE', ( #136072 ), #19112, .F. ) ;
#36337 = EDGE_CURVE ( 'NONE', #29986, #100160, #64056, .T. ) ;
#36338 = CARTESIAN_POINT ( 'NONE',  ( 29.99999999999979039, 13.93112307739203715, 4.000000000000000000 ) ) ;
#36339 = VERTEX_POINT ( 'NONE', #4069 ) ;
#36340 = VECTOR ( 'NONE', #76278, 1000.000000000000000 ) ;
#36341 = DIRECTION ( 'NONE',  ( 0.000000000000000000, -1.000000000000000000, 0.000000000000000000 ) ) ;
#36342 = VERTEX_POINT ( 'NONE', #130019 ) ;
#36343 = LINE ( 'NONE', #89983, #127759 ) ;
#36344 = CARTESIAN_POINT ( 'NONE',  ( 26.90040314143521627, -7.934999999999989839, 2.126176841940957907 ) ) ;
#36345 = AXIS2_PLACEMENT_3D ( 'NONE', #122816, #103196, #48126 ) ;
#36346 = CARTESIAN_POINT ( 'NONE',  ( -0.07876352523144723727, -9.717572351234235426E-16, -7.934999999999990727 ) ) ;
#36347 = ORIENTED_EDGE ( 'NONE', *, *, #81767, .F. ) ;
#36348 = CARTESIAN_POINT ( 'NONE',  ( 114.8287635252314516, 0.000000000000000000, -6.109999999999999432 ) ) ;
#36349 = EDGE_CURVE ( 'NONE', #56532, #23830, #110882, .T. ) ;
#36350 = DIRECTION ( 'NONE',  ( -0.7071067811865486830, -0.7071067811865464625, 0.000000000000000000 ) ) ;
#36351 = CARTESIAN_POINT ( 'NONE',  ( 12.79333936457838483, 21.75929247661549937, 4.998822639870715179 ) ) ;
#36352 = ORIENTED_EDGE ( 'NONE', *, *, #139821, .F. ) ;
#36353 = ORIENTED_EDGE ( 'NONE', *, *, #53457, .T. ) ;
#36354 = VECTOR ( 'NONE', #5564, 1000.000000000000000 ) ;
#36355 = DIRECTION ( 'NONE',  ( 0.7071067811865486830, -0.7071067811865464625, -0.000000000000000000 ) ) ;
#36356 = DIRECTION ( 'NONE',  ( 0.6830127018922180770, -0.6830127018922204085, -0.2588190451025213501 ) ) ;
#36357 = FACE_BOUND ( 'NONE', #59109, .T. ) ;
#36359 = ADVANCED_FACE ( 'NONE', ( #92543 ), #127899, .F. ) ;
#36358 = DIRECTION ( 'NONE',  ( -0.000000000000000000, -0.000000000000000000, -1.000000000000000000 ) ) ;
#36360 = LINE ( 'NONE', #113905, #16912 ) ;
#36361 = DIRECTION ( 'NONE',  ( -0.7071067811865486830, -0.7071067811865464625, -0.000000000000000000 ) ) ;
#36362 = ORIENTED_EDGE ( 'NONE', *, *, #105600, .T. ) ;
#36363 = FACE_OUTER_BOUND ( 'NONE', #27411, .T. ) ;
#36364 = DIRECTION ( 'NONE',  ( 0.6830127018922181881, 0.6830127018922202975, -0.2588190451025214056 ) ) ;
#36365 = DIRECTION ( 'NONE',  ( -0.000000000000000000, 0.000000000000000000, 1.000000000000000000 ) ) ;
#36366 = VECTOR ( 'NONE', #29087, 1000.000000000000000 ) ;
#36367 = ORIENTED_EDGE ( 'NONE', *, *, #134822, .T. ) ;
#36368 = FACE_OUTER_BOUND ( 'NONE', #105559, .T. ) ;
#36369 = LINE ( 'NONE', #24061, #67870 ) ;
#36370 = ORIENTED_EDGE ( 'NONE', *, *, #143059, .F. ) ;
#36371 = VECTOR ( 'NONE', #139904, 1000.000000000000000 ) ;
#36373 = VERTEX_POINT ( 'NONE', #106817 ) ;
#36372 = CARTESIAN_POINT ( 'NONE',  ( 26.75159235450331963, 9.902892378096218942E-16, 0.000000000000000000 ) ) ;
#36374 = ORIENTED_EDGE ( 'NONE', *, *, #134348, .T. ) ;
#36375 = FACE_OUTER_BOUND ( 'NONE', #70413, .T. ) ;
#36376 = CARTESIAN_POINT ( 'NONE',  ( -3.792893218813429446, -14.24070752338413826, 5.000000000000000000 ) ) ;
#36377 = ORIENTED_EDGE ( 'NONE', *, *, #37649, .F. ) ;
#36378 = EDGE_CURVE ( 'NONE', #86911, #68309, #40877, .T. ) ;
#36379 = PLANE ( 'NONE',  #6745 ) ;
#36380 = VECTOR ( 'NONE', #123329, 1000.000000000000000 ) ;
#36381 = VERTEX_POINT ( 'NONE', #29977 ) ;
#36382 = LINE ( 'NONE', #114631, #78551 ) ;
#36383 = DIRECTION ( 'NONE',  ( 0.7071067811865486830, -0.7071067811865464625, -0.000000000000000000 ) ) ;
#36384 = PLANE ( 'NONE',  #39771 ) ;
#36385 = DIRECTION ( 'NONE',  ( 1.000000000000000000, 0.000000000000000000, 0.000000000000000000 ) ) ;
#36386 = CARTESIAN_POINT ( 'NONE',  ( 125.7291446111226350, -5.312392442408975235, 5.610871146360816297 ) ) ;
#36387 = CARTESIAN_POINT ( 'NONE',  ( 8.999999999999941380, -3.033600742197707145, 5.000000000000000000 ) ) ;
#36388 = LINE ( 'NONE', #124817, #47741 ) ;
#36389 = EDGE_LOOP ( 'NONE', ( #121122, #1293, #139625, #86633 ) ) ;
#36390 = ORIENTED_EDGE ( 'NONE', *, *, #316, .T. ) ;
#36391 = ORIENTED_EDGE ( 'NONE', *, *, #4635, .F. ) ;
#36392 = CARTESIAN_POINT ( 'NONE',  ( 119.2708333333333144, -7.949999999999999289, -2.130196079827426203 ) ) ;
#36393 = EDGE_LOOP ( 'NONE', ( #78071, #22616, #2586, #94508 ) ) ;
#36394 = EDGE_LOOP ( 'NONE', ( #19985, #85200, #120642, #51973 ) ) ;
#36395 = EDGE_LOOP ( 'NONE', ( #69009, #139042, #21391, #53054 ) ) ;
#36396 = CARTESIAN_POINT ( 'NONE',  ( 0.1600000000000009748, -7.113645484598424495, 3.515717980648092045 ) ) ;
#36397 = DIRECTION ( 'NONE',  ( -0.6830127018922180770, -0.6830127018922204085, -0.2588190451025213501 ) ) ;
#36398 = EDGE_LOOP ( 'NONE', ( #136381, #116032, #74308, #9106, #54345 ) ) ;
#36399 = PLANE ( 'NONE',  #55478 ) ;
#36400 = CARTESIAN_POINT ( 'NONE',  ( 25.40000000000002345, 4.454858951346302831, 4.767764854533462326 ) ) ;
#36401 = LINE ( 'NONE', #37105, #48656 ) ;
#36402 = VECTOR ( 'NONE', #57513, 1000.000000000000000 ) ;
#36403 = FACE_OUTER_BOUND ( 'NONE', #58199, .T. ) ;
#36404 = CARTESIAN_POINT ( 'NONE',  ( 115.7920968585647756, -5.291415217122921177, 3.054999999999999272 ) ) ;
#36405 = EDGE_LOOP ( 'NONE', ( #16341, #33344, #65031, #123384 ) ) ;
#36406 = CARTESIAN_POINT ( 'NONE',  ( 23.57322811595262380, -0.7198850472490201380, 4.205258209906643785 ) ) ;
#36407 = DIRECTION ( 'NONE',  ( -0.6830127018922180770, -0.6830127018922204085, -0.2588190451025213501 ) ) ;
#36408 = CARTESIAN_POINT ( 'NONE',  ( 21.29974487139158512, -27.71228299555221142, 4.000000000000000000 ) ) ;
#36409 = CARTESIAN_POINT ( 'NONE',  ( 1.369639479247480862, 4.811953009385816285E-13, 6.725360520752516891 ) ) ;
#36410 =( NAMED_UNIT ( * ) PLANE_ANGLE_UNIT ( ) SI_UNIT ( $, .RADIAN. ) );
#36411 = VECTOR ( 'NONE', #21767, 1000.000000000000000 ) ;
#36412 = DIRECTION ( 'NONE',  ( 1.000000000000000000, 0.000000000000000000, 0.000000000000000000 ) ) ;
#36413 = FACE_OUTER_BOUND ( 'NONE', #30955, .T. ) ;
#36414 = VECTOR ( 'NONE', #8944, 1000.000000000000000 ) ;
#36415 = CARTESIAN_POINT ( 'NONE',  ( 46.74586038379622011, 3.974999999999996980, 6.884901960086287964 ) ) ;
#36416 = DIRECTION ( 'NONE',  ( -0.3543493200069162685, -0.000000000000000000, -0.9351131265310288487 ) ) ;
#36417 = AXIS2_PLACEMENT_3D ( 'NONE', #11602, #131281, #121806 ) ;
#36418 = SURFACE_STYLE_FILL_AREA ( #27662 ) ;
#36419 = EDGE_LOOP ( 'NONE', ( #137868, #17611, #132416, #2900 ) ) ;
#36420 = ORIENTED_EDGE ( 'NONE', *, *, #31211, .T. ) ;
#36421 = CARTESIAN_POINT ( 'NONE',  ( 39.64583333333332860, 2.130196079827431976, -7.949999999999999289 ) ) ;
#36422 = EDGE_LOOP ( 'NONE', ( #115202, #20323, #15249, #51765 ) ) ;
#36423 = ORIENTED_EDGE ( 'NONE', *, *, #12699, .F. ) ;
#36424 = DIRECTION ( 'NONE',  ( -0.000000000000000000, 0.000000000000000000, 1.000000000000000000 ) ) ;
#36425 = DIRECTION ( 'NONE',  ( -0.7071067811865486830, 0.7071067811865464625, 0.000000000000000000 ) ) ;
#36426 = VECTOR ( 'NONE', #141081, 1000.000000000000000 ) ;
#36427 = ORIENTED_EDGE ( 'NONE', *, *, #33959, .T. ) ;
#36428 = DIRECTION ( 'NONE',  ( -0.000000000000000000, 0.000000000000000000, 1.000000000000000000 ) ) ;
#36429 = PLANE ( 'NONE',  #545 ) ;
#36430 = CARTESIAN_POINT ( 'NONE',  ( 128.3912635252314374, -4.472830434245839371, -4.472830434245839371 ) ) ;
#36431 = ORIENTED_EDGE ( 'NONE', *, *, #110579, .T. ) ;
#36432 = DIRECTION ( 'NONE',  ( -0.3543493200069163240, -0.000000000000000000, -0.9351131265310288487 ) ) ;
#36433 = ORIENTED_EDGE ( 'NONE', *, *, #33995, .F. ) ;
#36434 = CARTESIAN_POINT ( 'NONE',  ( 13.92145407031093818, 0.000000000000000000, 2.500000000000000444 ) ) ;
#36435 = CARTESIAN_POINT ( 'NONE',  ( -62.99451991528749772, 28.92564299267982264, 4.000000000000000000 ) ) ;
#36436 = SURFACE_SIDE_STYLE ('',( #91537 ) ) ;
#36437 = EDGE_CURVE ( 'NONE', #20187, #75689, #25888, .T. ) ;
#36438 = LINE ( 'NONE', #88692, #118239 ) ;
#36439 = ORIENTED_EDGE ( 'NONE', *, *, #37815, .T. ) ;
#36440 = EDGE_CURVE ( 'NONE', #9403, #104700, #118409, .T. ) ;
#36441 = ADVANCED_FACE ( 'NONE', ( #140870 ), #136786, .F. ) ;
#36442 = EDGE_LOOP ( 'NONE', ( #127407, #69839, #128142, #40777 ) ) ;
#36443 = FACE_OUTER_BOUND ( 'NONE', #52557, .T. ) ;
#36444 = DIRECTION ( 'NONE',  ( -0.000000000000000000, 0.3543493200069152138, -0.9351131265310292928 ) ) ;
#36445 = DIRECTION ( 'NONE',  ( -0.000000000000000000, 0.3543493200069153248, 0.9351131265310292928 ) ) ;
#36446 = VECTOR ( 'NONE', #87330, 1000.000000000000000 ) ;
#36447 = LINE ( 'NONE', #60365, #134285 ) ;
#36448 = CARTESIAN_POINT ( 'NONE',  ( -68.99451991528748351, 28.92564299267986172, 4.000000000000000000 ) ) ;
#36449 = EDGE_CURVE ( 'NONE', #99997, #128260, #127150, .T. ) ;
#36450 = EDGE_CURVE ( 'NONE', #101750, #49090, #143036, .T. ) ;
#36451 = VECTOR ( 'NONE', #123215, 1000.000000000000000 ) ;
#36452 = CARTESIAN_POINT ( 'NONE',  ( 61.59959685856478018, -6.109999999999997655, -1.637169565754160283 ) ) ;
#36453 = LINE ( 'NONE', #4456, #127427 ) ;
#36454 = EDGE_CURVE ( 'NONE', #44302, #82135, #56063, .T. ) ;
#36455 = DIRECTION ( 'NONE',  ( 1.000000000000000000, 0.000000000000000000, 0.000000000000000000 ) ) ;
#36456 = EDGE_LOOP ( 'NONE', ( #47561, #143044, #60991, #20422 ) ) ;
#36457 = ORIENTED_EDGE ( 'NONE', *, *, #17977, .F. ) ;
#36458 = VECTOR ( 'NONE', #55529, 1000.000000000000000 ) ;
#36459 = CARTESIAN_POINT ( 'NONE',  ( 31.49999999999977263, 8.319652575858409449, -8.582050562765751067 ) ) ;
#36460 = EDGE_LOOP ( 'NONE', ( #75346, #66623, #54762, #72317 ) ) ;
#36461 =( BOUNDED_CURVE ( )  B_SPLINE_CURVE ( 2, ( #120131, #99103, #32463, #120871, #55645, #52754, #88272, #141196, #78110, #122289, #131055, #111426, #108538 ),
 .UNSPECIFIED., .F., .F. ) 
 B_SPLINE_CURVE_WITH_KNOTS ( ( 3, 2, 2, 2, 2, 2, 3 ),
 ( 0.8000000000000000444, 0.8027777777777778123, 0.8055555555555555802, 0.8083333333333333481, 0.8111111111111111160, 0.8138888888888888840, 0.8166666666666666519 ),
 .UNSPECIFIED. ) 
 CURVE ( )  GEOMETRIC_REPRESENTATION_ITEM ( )  RATIONAL_B_SPLINE_CURVE ( ( 1.000000000000000000, 0.9659258262890683122, 1.000000000000000000, 0.9659258262890683122, 1.000000000000000000, 0.9659258262890683122, 1.000000000000000000, 0.9659258262890683122, 1.000000000000000000, 0.9659258262890683122, 1.000000000000000000, 0.9659258262890683122, 1.000000000000000000 ) ) 
 REPRESENTATION_ITEM ( '' )  );
#36462 = ADVANCED_FACE ( 'NONE', ( #31429 ), #98800, .F. ) ;
#36463 = LINE ( 'NONE', #68413, #127566 ) ;
#36464 = ORIENTED_EDGE ( 'NONE', *, *, #27801, .F. ) ;
#36465 = VECTOR ( 'NONE', #44267, 1000.000000000000114 ) ;
#36466 = EDGE_CURVE ( 'NONE', #97559, #16532, #100253, .T. ) ;
#36467 = PRESENTATION_STYLE_ASSIGNMENT (( #15381 ) ) ;
#36468 = FACE_BOUND ( 'NONE', #100319, .T. ) ;
#36469 = PLANE ( 'NONE',  #61958 ) ;
#36470 = DIRECTION ( 'NONE',  ( -0.7071067811865487940, 0.7071067811865463515, -0.000000000000000000 ) ) ;
#36471 = LINE ( 'NONE', #119698, #85135 ) ;
#36473 = ORIENTED_EDGE ( 'NONE', *, *, #126495, .T. ) ;
#36472 = LINE ( 'NONE', #3789, #138438 ) ;
#36474 = EDGE_CURVE ( 'NONE', #27138, #9302, #95091, .T. ) ;
#36475 = CARTESIAN_POINT ( 'NONE',  ( 33.70710678118631165, -6.740707523384205757, 5.000000000000000000 ) ) ;
#36476 = ORIENTED_EDGE ( 'NONE', *, *, #8183, .F. ) ;
#36477 = ORIENTED_EDGE ( 'NONE', *, *, #84093, .T. ) ;
#36478 = CARTESIAN_POINT ( 'NONE',  ( 62.62043019189811588, 3.055000000000001936, -5.291415217122916737 ) ) ;
#36479 = ORIENTED_EDGE ( 'NONE', *, *, #62245, .F. ) ;
#36480 = VECTOR ( 'NONE', #135613, 999.9999999999998863 ) ;
#36481 = DIRECTION ( 'NONE',  ( 0.7071067811865487940, 0.7071067811865463515, -0.000000000000000000 ) ) ;
#36482 = EDGE_CURVE ( 'NONE', #109252, #13343, #34280, .T. ) ;
#36483 = EDGE_LOOP ( 'NONE', ( #74757, #80495, #52796, #61491 ) ) ;
#36484 = LINE ( 'NONE', #38629, #118789 ) ;
#36485 = DIRECTION ( 'NONE',  ( -0.7071067811865487940, 0.7071067811865463515, 0.000000000000000000 ) ) ;
#36486 = EDGE_CURVE ( 'NONE', #138848, #106932, #33592, .T. ) ;
#36487 = CARTESIAN_POINT ( 'NONE',  ( 34.42499999999998295, 1.541399257802028577, 5.000000000000000000 ) ) ;
#36488 = CYLINDRICAL_SURFACE ( 'NONE', #64414, 9.524999999999995026 ) ;
#36489 = CARTESIAN_POINT ( 'NONE',  ( -12.29974487139158512, -27.71228299555214747, 4.000000000000000000 ) ) ;
#36490 = ADVANCED_FACE ( 'NONE', ( #23384 ), #53153, .F. ) ;
#36491 = CARTESIAN_POINT ( 'NONE',  ( 9.328169399223456892, -18.74070752338409562, 4.000000000000000000 ) ) ;
#36492 = CARTESIAN_POINT ( 'NONE',  ( -21.18398860626899349, 28.73617430169802134, 5.000000000000000000 ) ) ;
#36493 = ORIENTED_EDGE ( 'NONE', *, *, #101440, .F. ) ;
#36494 = EDGE_LOOP ( 'NONE', ( #131780, #68722, #3470, #106206 ) ) ;
#36495 = DIRECTION ( 'NONE',  ( 0.000000000000000000, -1.000000000000000000, 0.000000000000000000 ) ) ;
#36497 = CARTESIAN_POINT ( 'NONE',  ( 50.99451991528749062, 28.92564299267973738, 4.000000000000000000 ) ) ;
#36496 = VECTOR ( 'NONE', #15086, 1000.000000000000227 ) ;
#36498 = ORIENTED_EDGE ( 'NONE', *, *, #18426, .T. ) ;
#36499 = ADVANCED_FACE ( 'NONE', ( #8885 ), #54616, .F. ) ;
#36500 = ORIENTED_EDGE ( 'NONE', *, *, #141495, .F. ) ;
#36502 = VERTEX_POINT ( 'NONE', #99504 ) ;
#36501 = VECTOR ( 'NONE', #122199, 1000.000000000000227 ) ;
#36503 = CARTESIAN_POINT ( 'NONE',  ( 29.14583333333332504, 2.130196079827431976, -7.949999999999998401 ) ) ;
#36504 = VERTEX_POINT ( 'NONE', #77793 ) ;
#36505 = DIRECTION ( 'NONE',  ( -1.000000000000000000, -1.224606353822377258E-16, -0.000000000000000000 ) ) ;
#36506 = VECTOR ( 'NONE', #139202, 1000.000000000000000 ) ;
#36507 = CARTESIAN_POINT ( 'NONE',  ( 26.99999999999981526, 7.552185695429090906, 5.000000000000000000 ) ) ;
#36508 = CARTESIAN_POINT ( 'NONE',  ( -0.9537635252314473622, -7.934999999999990727, 4.858786175617117713E-16 ) ) ;
#36509 = DIRECTION ( 'NONE',  ( 0.3543493200069162685, -0.000000000000000000, -0.9351131265310288487 ) ) ;
#36510 = ORIENTED_EDGE ( 'NONE', *, *, #38630, .T. ) ;
#36511 = EDGE_CURVE ( 'NONE', #53146, #7053, #120531, .T. ) ;
#36512 = CARTESIAN_POINT ( 'NONE',  ( -26.93988928955963402, -9.740707523384187994, 10.89222023123386940 ) ) ;
#36513 = CARTESIAN_POINT ( 'NONE',  ( 120.2458603837962272, 3.974999999999996980, 6.884901960086287964 ) ) ;
#36514 = AXIS2_PLACEMENT_3D ( 'NONE', #97185, #47016, #44869 ) ;
#36515 = FACE_OUTER_BOUND ( 'NONE', #99944, .T. ) ;
#36517 = EDGE_LOOP ( 'NONE', ( #26361, #16947, #127076, #56074 ) ) ;
#36516 = DIRECTION ( 'NONE',  ( -0.7071067811865486830, 0.7071067811865464625, 0.000000000000000000 ) ) ;
#36518 = VERTEX_POINT ( 'NONE', #21255 ) ;
#36519 = LINE ( 'NONE', #27777, #128325 ) ;
#36520 = DIRECTION ( 'NONE',  ( 0.7071067811865487940, 0.7071067811865463515, -0.000000000000000000 ) ) ;
#36521 = CARTESIAN_POINT ( 'NONE',  ( 9.299744871391588674, -27.71228299555212971, 4.000000000000000000 ) ) ;
#36522 = EDGE_LOOP ( 'NONE', ( #83862, #2774, #93455, #109891 ) ) ;
#36523 = CARTESIAN_POINT ( 'NONE',  ( 18.18398860626898994, 28.73617430169800002, 5.000000000000000000 ) ) ;
#36524 = DIRECTION ( 'NONE',  ( 0.7071067811865487940, 0.7071067811865463515, 0.000000000000000000 ) ) ;
#36525 = CARTESIAN_POINT ( 'NONE',  ( -21.79289321881329755, -5.240707523384227073, 5.000000000000000000 ) ) ;
#36526 = DIRECTION ( 'NONE',  ( 0.6830127018922181881, 0.6830127018922202975, -0.2588190451025214056 ) ) ;
#36527 = LINE ( 'NONE', #12621, #142109 ) ;
#36528 = ORIENTED_EDGE ( 'NONE', *, *, #53858, .T. ) ;
#36529 = FACE_OUTER_BOUND ( 'NONE', #133430, .T. ) ;
#36530 = CARTESIAN_POINT ( 'NONE',  ( -25.56661756231483906, -22.22500000000000142, 8.546240940345063208 ) ) ;
#36531 = DIRECTION ( 'NONE',  ( -0.7071067811865487940, 0.7071067811865463515, 0.000000000000000000 ) ) ;
#36532 = PLANE ( 'NONE',  #3081 ) ;
#36533 = EDGE_CURVE ( 'NONE', #14111, #86570, #27593, .T. ) ;
#36534 = DIRECTION ( 'NONE',  ( 0.000000000000000000, -1.000000000000000000, 0.000000000000000000 ) ) ;
#36535 = ORIENTED_EDGE ( 'NONE', *, *, #136940, .T. ) ;
#36536 = VERTEX_POINT ( 'NONE', #32876 ) ;
#36537 = AXIS2_PLACEMENT_3D ( 'NONE', #108124, #17053, #116360 ) ;
#36538 = CARTESIAN_POINT ( 'NONE',  ( 30.72281430457039875, -21.72499999999999432, 5.000000000000000000 ) ) ;
#36539 = DIRECTION ( 'NONE',  ( -0.000000000000000000, 0.000000000000000000, 1.000000000000000000 ) ) ;
#36540 = CARTESIAN_POINT ( 'NONE',  ( 1.874569808101886226, 6.871911579029510442, -3.967499999999998916 ) ) ;
#36541 = LINE ( 'NONE', #27803, #6456 ) ;
#36542 = STYLED_ITEM ( 'NONE', ( #85514 ), #34948 ) ;
#36543 = CARTESIAN_POINT ( 'NONE',  ( 11.51078643762690490, -27.52281430457047406, 5.000000000000000000 ) ) ;
#36544 = LINE ( 'NONE', #81508, #55241 ) ;
#36545 = CARTESIAN_POINT ( 'NONE',  ( -32.29387692260781506, 22.22500000000000142, 4.000000000000000000 ) ) ;
#36546 = ORIENTED_EDGE ( 'NONE', *, *, #56795, .T. ) ;
#36547 = CARTESIAN_POINT ( 'NONE',  ( -20.51078643762690490, -27.52281430457041012, 5.000000000000000000 ) ) ;
#36548 = LINE ( 'NONE', #27092, #37752 ) ;
#36549 = DIRECTION ( 'NONE',  ( 0.7071067811865487940, -0.7071067811865463515, 0.000000000000000000 ) ) ;
#36550 = CARTESIAN_POINT ( 'NONE',  ( 60.57876352523145158, -7.482591942790327058E-16, 6.109999999999999432 ) ) ;
#36551 = LINE ( 'NONE', #70650, #106540 ) ;
#36552 = EDGE_CURVE ( 'NONE', #31122, #99410, #141618, .T. ) ;
#36553 = VERTEX_POINT ( 'NONE', #22644 ) ;
#36554 = CARTESIAN_POINT ( 'NONE',  ( -5.994519915287488843, 28.92564299267942118, 4.000000000000000000 ) ) ;
#36555 = ORIENTED_EDGE ( 'NONE', *, *, #79475, .T. ) ;
#36556 = CARTESIAN_POINT ( 'NONE',  ( -8.999999999999932498, 5.966399257802200040, 5.000000000000000000 ) ) ;
#36557 = DIRECTION ( 'NONE',  ( -0.000000000000000000, 0.3543493200069153248, 0.9351131265310292928 ) ) ;
#36558 = DIRECTION ( 'NONE',  ( 0.6830127018922180770, -0.6830127018922204085, -0.2588190451025213501 ) ) ;
#36559 = LINE ( 'NONE', #59767, #124918 ) ;
#36560 = ADVANCED_FACE ( 'NONE', ( #89370 ), #42321, .F. ) ;
#36561 = FACE_OUTER_BOUND ( 'NONE', #99751, .T. ) ;
#36562 = CARTESIAN_POINT ( 'NONE',  ( 128.6786164994711044, -49.14501756083437556, 40.36361034346624166 ) ) ;
#36563 = ORIENTED_EDGE ( 'NONE', *, *, #59143, .T. ) ;
#36564 = ORIENTED_EDGE ( 'NONE', *, *, #59432, .F. ) ;
#36565 = DIRECTION ( 'NONE',  ( -0.000000000000000000, 1.000000000000000000, -0.000000000000000000 ) ) ;
#36566 = DIRECTION ( 'NONE',  ( -0.7071067811865487940, 0.7071067811865463515, -0.000000000000000000 ) ) ;
#36567 = CARTESIAN_POINT ( 'NONE',  ( 5.277185695429377432, -21.72500000000000853, 5.000000000000000000 ) ) ;
#36568 = DIRECTION ( 'NONE',  ( 0.000000000000000000, -1.000000000000000000, 0.000000000000000000 ) ) ;
#36569 = CARTESIAN_POINT ( 'NONE',  ( 79.55836038379622721, -7.949999999999997513, -2.130196079827425759 ) ) ;
#36570 = DIRECTION ( 'NONE',  ( -0.7071067811865486830, -0.7071067811865464625, 0.000000000000000000 ) ) ;
#36571 = ORIENTED_EDGE ( 'NONE', *, *, #82180, .F. ) ;
#36572 = VECTOR ( 'NONE', #130457, 999.9999999999998863 ) ;
#36573 = CARTESIAN_POINT ( 'NONE',  ( 61.95833333333332149, 3.974999999999997424, 6.884901960086288852 ) ) ;
#36574 = DIRECTION ( 'NONE',  ( -1.000000000000000000, 0.000000000000000000, -0.000000000000000000 ) ) ;
#36575 = CARTESIAN_POINT ( 'NONE',  ( 19.49999999999987210, 13.08746187583910725, 4.000000000000000000 ) ) ;
#36576 = LINE ( 'NONE', #59785, #100685 ) ;
#36577 = EDGE_LOOP ( 'NONE', ( #135875, #16772, #47586, #12639 ) ) ;
#36578 = CARTESIAN_POINT ( 'NONE',  ( 24.79333936457830134, 21.75929247661549226, 4.998822639870711626 ) ) ;
#36579 = AXIS2_PLACEMENT_3D ( 'NONE', #33583, #20503, #32865 ) ;
#36580 = SPHERICAL_SURFACE ( 'NONE', #83778, 0.5000000000000000000 ) ;
#36581 = CARTESIAN_POINT ( 'NONE',  ( 68.54209685856477563, 5.291415217122923842, -3.054999999999996163 ) ) ;
#36582 = CARTESIAN_POINT ( 'NONE',  ( -48.18398860626899705, 28.73617430169820608, 5.000000000000000000 ) ) ;
#36583 = VERTEX_POINT ( 'NONE', #64771 ) ;
#36584 = ORIENTED_EDGE ( 'NONE', *, *, #27142, .T. ) ;
#36585 = CARTESIAN_POINT ( 'NONE',  ( 78.48921356237309510, -27.52281430457109934, 5.000000000000000000 ) ) ;
#36586 = CARTESIAN_POINT ( 'NONE',  ( 18.41161490594819128, 22.22500000000000142, 4.777194822843815913 ) ) ;
#36587 = VECTOR ( 'NONE', #139390, 1000.000000000000000 ) ;
#36588 = LINE ( 'NONE', #56959, #94950 ) ;
#36589 = CARTESIAN_POINT ( 'NONE',  ( -12.69999999999999929, -59.76999999999998892, 24.34531699603381938 ) ) ;
#36590 = EDGE_CURVE ( 'NONE', #95889, #56990, #32132, .T. ) ;
#36592 = ORIENTED_EDGE ( 'NONE', *, *, #41185, .T. ) ;
#36591 = DIRECTION ( 'NONE',  ( 0.6830127018922180770, -0.6830127018922204085, -0.2588190451025214056 ) ) ;
#36593 = DIRECTION ( 'NONE',  ( -0.5735764363510501562, 0.8191520442889890230, 1.003171929053521419E-16 ) ) ;
#36594 = CARTESIAN_POINT ( 'NONE',  ( 0.000000000000000000, 0.000000000000000000, 0.000000000000000000 ) ) ;
#36595 = DIRECTION ( 'NONE',  ( 0.000000000000000000, 0.000000000000000000, 1.000000000000000000 ) ) ;
#36596 = AXIS2_PLACEMENT_3D ( 'NONE', #119721, #121870, #32770 ) ;
#36597 = AXIS2_PLACEMENT_3D ( 'NONE', #26140, #124026, #82667 ) ;
#36599 = ORIENTED_EDGE ( 'NONE', *, *, #112417, .T. ) ;
#36598 = EDGE_CURVE ( 'NONE', #70234, #113156, #87939, .T. ) ;
#36600 = EDGE_CURVE ( 'NONE', #68320, #25758, #21961, .T. ) ;
#36601 = ORIENTED_EDGE ( 'NONE', *, *, #13040, .T. ) ;
#36602 = ADVANCED_FACE ( 'NONE', ( #4426 ), #20660, .T. ) ;
#36603 =( BOUNDED_CURVE ( )  B_SPLINE_CURVE ( 3, ( #139360, #83539, #84263, #71961 ),
 .UNSPECIFIED., .F., .T. ) 
 B_SPLINE_CURVE_WITH_KNOTS ( ( 4, 4 ),
 ( 5.005968288816718292, 5.074607125596354962 ),
 .UNSPECIFIED. ) 
 CURVE ( )  GEOMETRIC_REPRESENTATION_ITEM ( )  RATIONAL_B_SPLINE_CURVE ( ( 1.000000000000000000, 0.9996074310407762065, 0.9996074310407762065, 1.000000000000000000 ) ) 
 REPRESENTATION_ITEM ( '' )  );
#36604 = DIRECTION ( 'NONE',  ( 0.000000000000000000, 0.000000000000000000, -1.000000000000000000 ) ) ;
#36605 = DIRECTION ( 'NONE',  ( -0.7071067811865486830, -0.7071067811865464625, 0.000000000000000000 ) ) ;
#36606 = EDGE_CURVE ( 'NONE', #85671, #142121, #135056, .T. ) ;
#36607 = DIRECTION ( 'NONE',  ( 0.000000000000000000, 0.000000000000000000, 1.000000000000000000 ) ) ;
#36608 = LINE ( 'NONE', #111308, #103430 ) ;
#36609 = ORIENTED_EDGE ( 'NONE', *, *, #49325, .T. ) ;
#36610 = ORIENTED_EDGE ( 'NONE', *, *, #96612, .F. ) ;
#36611 = EDGE_CURVE ( 'NONE', #22039, #21922, #126285, .T. ) ;
#36612 = CARTESIAN_POINT ( 'NONE',  ( 5.816011393731002066, 28.73617430169783304, 5.000000000000000000 ) ) ;
#36613 = FACE_OUTER_BOUND ( 'NONE', #95961, .T. ) ;
#36614 = EDGE_CURVE ( 'NONE', #111099, #13267, #44599, .T. ) ;
#36615 = ORIENTED_EDGE ( 'NONE', *, *, #1564, .T. ) ;
#36616 =( NAMED_UNIT ( * ) PLANE_ANGLE_UNIT ( ) SI_UNIT ( $, .RADIAN. ) );
#36617 = ORIENTED_EDGE ( 'NONE', *, *, #136444, .F. ) ;
#36618 = CARTESIAN_POINT ( 'NONE',  ( -2.816011393730999401, 28.73617430169785436, 5.000000000000000000 ) ) ;
#36619 = DIRECTION ( 'NONE',  ( -0.000000000000000000, 0.000000000000000000, 1.000000000000000000 ) ) ;
#36620 = ORIENTED_EDGE ( 'NONE', *, *, #64119, .T. ) ;
#36621 = VECTOR ( 'NONE', #71325, 1000.000000000000114 ) ;
#36622 = ADVANCED_FACE ( 'NONE', ( #21375 ), #77210, .F. ) ;
#36623 = FACE_BOUND ( 'NONE', #36258, .T. ) ;
#36624 = DIRECTION ( 'NONE',  ( 1.318980745116185161E-16, -1.000000000000000000, 0.000000000000000000 ) ) ;
#36625 = LINE ( 'NONE', #44713, #60626 ) ;
#36626 = DIRECTION ( 'NONE',  ( -0.7071067811865486830, -0.7071067811865464625, -0.000000000000000000 ) ) ;
#36627 = VECTOR ( 'NONE', #18823, 1000.000000000000000 ) ;
#36628 = CARTESIAN_POINT ( 'NONE',  ( -12.29974487139158512, -27.71228299555214747, 4.000000000000000000 ) ) ;
#36629 = EDGE_CURVE ( 'NONE', #95062, #28555, #19924, .T. ) ;
#36630 = CARTESIAN_POINT ( 'NONE',  ( 17.20710678118642534, -14.24070752338414181, 5.000000000000000000 ) ) ;
#36631 = DIRECTION ( 'NONE',  ( -1.000000000000000000, 0.000000000000000000, 0.000000000000000000 ) ) ;
#36632 = ORIENTED_EDGE ( 'NONE', *, *, #12093, .T. ) ;
#36633 = EDGE_LOOP ( 'NONE', ( #132694, #17206, #36285, #90556 ) ) ;
#36634 = CARTESIAN_POINT ( 'NONE',  ( 95.57876352523145158, -7.482591942790325086E-16, 6.109999999999998543 ) ) ;
#36635 = ORIENTED_EDGE ( 'NONE', *, *, #21276, .T. ) ;
#36636 = CARTESIAN_POINT ( 'NONE',  ( 30.48921356237309510, -27.52281430457076894, 5.000000000000000000 ) ) ;
#36637 = LINE ( 'NONE', #104756, #35212 ) ;
#36638 = VECTOR ( 'NONE', #97059, 1000.000000000000000 ) ;
#36639 = CARTESIAN_POINT ( 'NONE',  ( 17.20666063542140733, 21.75929247661550292, 4.998822639870701856 ) ) ;
#36640 = AXIS2_PLACEMENT_3D ( 'NONE', #36033, #46940, #124437 ) ;
#36641 = CARTESIAN_POINT ( 'NONE',  ( 34.42499999999998295, -21.72500000000000142, 4.500000000000000888 ) ) ;
#36642 = EDGE_LOOP ( 'NONE', ( #44160, #67527, #64982, #59692, #134697, #89303, #87881, #59506 ) ) ;
#36643 = LINE ( 'NONE', #61317, #11297 ) ;
#36644 = CARTESIAN_POINT ( 'NONE',  ( -34.92500000000001137, 22.22500000000000142, 4.000000000000000000 ) ) ;
#36645 = CARTESIAN_POINT ( 'NONE',  ( 19.22674160717822289, -11.24070752338415780, 18.24660765846986621 ) ) ;
#36647 = DIRECTION ( 'NONE',  ( 0.000000000000000000, 0.000000000000000000, 1.000000000000000000 ) ) ;
#36646 = CARTESIAN_POINT ( 'NONE',  ( 68.66666666666665719, 6.884901960086285300, 3.975000000000003642 ) ) ;
#36648 = ADVANCED_FACE ( 'NONE', ( #33698 ), #109804, .F. ) ;
#36649 = CARTESIAN_POINT ( 'NONE',  ( 16.92580874392867685, 8.754106587137664874, 4.662926800793069759 ) ) ;
#36650 = CARTESIAN_POINT ( 'NONE',  ( 34.17183060077622514, 12.75929247661558641, 4.000000000000000000 ) ) ;
#36651 = ORIENTED_EDGE ( 'NONE', *, *, #61278, .F. ) ;
#36652 = DIRECTION ( 'NONE',  ( -0.7071067811865486830, -0.7071067811865464625, 0.000000000000000000 ) ) ;
#36653 = EDGE_CURVE ( 'NONE', #65837, #14111, #134111, .T. ) ;
#36654 = LINE ( 'NONE', #14900, #14104 ) ;
#36655 = ORIENTED_EDGE ( 'NONE', *, *, #127046, .T. ) ;
#36656 = ORIENTED_EDGE ( 'NONE', *, *, #142604, .T. ) ;
#36657 = ORIENTED_EDGE ( 'NONE', *, *, #78775, .T. ) ;
#36658 = CARTESIAN_POINT ( 'NONE',  ( 58.04209685856477563, 5.291415217122923842, -3.054999999999996163 ) ) ;
#36659 = VERTEX_POINT ( 'NONE', #131565 ) ;
#36660 = EDGE_CURVE ( 'NONE', #128291, #13057, #22752, .T. ) ;
#36661 = CARTESIAN_POINT ( 'NONE',  ( 2.379139616203772789, -5.278424836066145431, -3.047499999999993658 ) ) ;
#36662 = VECTOR ( 'NONE', #98870, 1000.000000000000227 ) ;
#36663 = FILL_AREA_STYLE_COLOUR ( '', #74984 ) ;
#36664 = VERTEX_POINT ( 'NONE', #132308 ) ;
#36665 = EDGE_CURVE ( 'NONE', #5945, #66770, #30842, .T. ) ;
#36666 = DIRECTION ( 'NONE',  ( -0.000000000000000000, 0.3543493200069153248, 0.9351131265310292928 ) ) ;
#36667 = VERTEX_POINT ( 'NONE', #42440 ) ;
#36668 = DIRECTION ( 'NONE',  ( 0.6830127018922180770, -0.6830127018922204085, -0.2588190451025213501 ) ) ;
#36670 = EDGE_LOOP ( 'NONE', ( #16278, #723, #102002, #80716 ) ) ;
#36669 = LINE ( 'NONE', #45453, #88781 ) ;
#36671 = VERTEX_POINT ( 'NONE', #86649 ) ;
#36672 = CARTESIAN_POINT ( 'NONE',  ( 23.99451991528749062, 28.92564299267954908, 4.000000000000000000 ) ) ;
#36673 = CARTESIAN_POINT ( 'NONE',  ( 32.29289321881323360, 8.259292476615643253, 5.000000000000000000 ) ) ;
#36674 = CARTESIAN_POINT ( 'NONE',  ( 127.3704301918981088, -3.055000000000001936, 5.291415217122918513 ) ) ;
#36675 = ORIENTED_EDGE ( 'NONE', *, *, #13152, .T. ) ;
#36676 = DIRECTION ( 'NONE',  ( -0.6830127018922181881, 0.6830127018922202975, -0.2588190451025214056 ) ) ;
#36677 = ORIENTED_EDGE ( 'NONE', *, *, #88721, .T. ) ;
#36678 = ORIENTED_EDGE ( 'NONE', *, *, #105022, .T. ) ;
#36679 = ORIENTED_EDGE ( 'NONE', *, *, #126743, .T. ) ;
#36680 = CARTESIAN_POINT ( 'NONE',  ( -28.49999999999980460, -12.08601207473291161, -10.46905243149087461 ) ) ;
#36681 = VECTOR ( 'NONE', #41261, 1000.000000000000000 ) ;
#36682 = VECTOR ( 'NONE', #115111, 1000.000000000000000 ) ;
#36683 = DIRECTION ( 'NONE',  ( -0.000000000000000000, -0.3543493200069152693, 0.9351131265310292928 ) ) ;
#36684 = VECTOR ( 'NONE', #97220, 999.9999999999998863 ) ;
#36685 = LINE ( 'NONE', #105502, #58717 ) ;
#36686 = EDGE_CURVE ( 'NONE', #69641, #64405, #130872, .T. ) ;
#36687 = CARTESIAN_POINT ( 'NONE',  ( 74.99451991528749772, 28.92564299267990435, 4.000000000000000000 ) ) ;
#36688 = AXIS2_PLACEMENT_3D ( 'NONE', #143333, #77406, #88256 ) ;
#36689 = EDGE_CURVE ( 'NONE', #91593, #44215, #142451, .T. ) ;
#36690 = DIRECTION ( 'NONE',  ( -0.7071067811865487940, 0.7071067811865463515, 0.000000000000000000 ) ) ;
#36691 = ORIENTED_EDGE ( 'NONE', *, *, #99676, .T. ) ;
#36692 = VECTOR ( 'NONE', #77538, 1000.000000000000000 ) ;
#36693 = VECTOR ( 'NONE', #57664, 1000.000000000000000 ) ;
#36694 = DIRECTION ( 'NONE',  ( -0.7071067811865487940, 0.7071067811865463515, 0.000000000000000000 ) ) ;
#36695 = CARTESIAN_POINT ( 'NONE',  ( 26.95790314143522437, 6.871911579029515771, 3.967499999999989146 ) ) ;
#36696 = PLANE ( 'NONE',  #23093 ) ;
#36697 = DIRECTION ( 'NONE',  ( 1.000000000000000000, 0.000000000000000000, 0.000000000000000000 ) ) ;
#36698 = CARTESIAN_POINT ( 'NONE',  ( -5.292986735706916690, -21.74070752338406010, 4.999753212805220670 ) ) ;
#36699 = ORIENTED_EDGE ( 'NONE', *, *, #16118, .T. ) ;
#36700 = ORIENTED_EDGE ( 'NONE', *, *, #17324, .T. ) ;
#36701 = ORIENTED_EDGE ( 'NONE', *, *, #142187, .T. ) ;
#36702 = LINE ( 'NONE', #80249, #71838 ) ;
#36703 = DIRECTION ( 'NONE',  ( -0.7071067811865486830, -0.7071067811865464625, -0.000000000000000000 ) ) ;
#36704 = DIRECTION ( 'NONE',  ( 0.000000000000000000, 0.000000000000000000, 1.000000000000000000 ) ) ;
#36705 = AXIS2_PLACEMENT_3D ( 'NONE', #94473, #39412, #117629 ) ;
#36706 = CARTESIAN_POINT ( 'NONE',  ( -69.18398860626899705, 28.73617430169835529, 5.000000000000000000 ) ) ;
#36707 = DIRECTION ( 'NONE',  ( -0.7071067811865486830, -0.7071067811865464625, 0.000000000000000000 ) ) ;
#36708 = CARTESIAN_POINT ( 'NONE',  ( 10.03137119346127726, 8.432637487761468265, 4.375000000000001776 ) ) ;
#36709 = ADVANCED_FACE ( 'NONE', ( #55438 ), #103951, .T. ) ;
#36710 = DIRECTION ( 'NONE',  ( 1.000000000000000000, 0.000000000000000000, 0.000000000000000000 ) ) ;
#36712 = CARTESIAN_POINT ( 'NONE',  ( -22.41009064519818494, 9.759292476615618384, 11.28811694763773588 ) ) ;
#36711 = AXIS2_PLACEMENT_3D ( 'NONE', #67828, #357, #66372 ) ;
#36713 = EDGE_CURVE ( 'NONE', #22536, #121049, #140987, .T. ) ;
#36714 = DIRECTION ( 'NONE',  ( -0.7071067811865487940, 0.7071067811865463515, -0.000000000000000000 ) ) ;
#36715 = CARTESIAN_POINT ( 'NONE',  ( 6.792893218813405909, 15.75929247661555976, 5.000000000000000000 ) ) ;
#36716 = DIRECTION ( 'NONE',  ( -0.000000000000000000, 0.3543493200069153248, 0.9351131265310292928 ) ) ;
#36717 = CARTESIAN_POINT ( 'NONE',  ( -19.49999999999986855, 19.39370406404965408, 1.459788787078246886 ) ) ;
#36718 = EDGE_LOOP ( 'NONE', ( #117080, #82200, #130530, #61167 ) ) ;
#36719 = VECTOR ( 'NONE', #125368, 1000.000000000000000 ) ;
#36720 = CARTESIAN_POINT ( 'NONE',  ( 17.39690951308662648, -2.395832017967521654, -33.23817995126653813 ) ) ;
#36721 = EDGE_LOOP ( 'NONE', ( #10631, #1331, #76070, #43260 ) ) ;
#36722 = VECTOR ( 'NONE', #70815, 1000.000000000000227 ) ;
#36723 = VECTOR ( 'NONE', #65232, 1000.000000000000227 ) ;
#36724 = DIRECTION ( 'NONE',  ( 0.7071067811865487940, -0.7071067811865463515, 0.000000000000000000 ) ) ;
#36726 = EDGE_LOOP ( 'NONE', ( #104431, #137592, #86162, #46270 ) ) ;
#36725 = DIRECTION ( 'NONE',  ( 0.7071067811865486830, -0.7071067811865464625, -0.000000000000000000 ) ) ;
#36727 = EDGE_CURVE ( 'NONE', #54018, #6851, #20638, .T. ) ;
#36728 = LINE ( 'NONE', #68676, #33367 ) ;
#36729 = ORIENTED_EDGE ( 'NONE', *, *, #7958, .T. ) ;
#36730 = PLANE ( 'NONE',  #20659 ) ;
#36731 = ORIENTED_EDGE ( 'NONE', *, *, #132604, .T. ) ;
#36732 = CARTESIAN_POINT ( 'NONE',  ( 121.2666937171295700, -7.949999999999998401, 2.130196079827423983 ) ) ;
#36733 = EDGE_LOOP ( 'NONE', ( #91542, #48998, #37066, #39176 ) ) ;
#36734 = AXIS2_PLACEMENT_3D ( 'NONE', #49957, #26754, #72451 ) ;
#36735 = VECTOR ( 'NONE', #112973, 999.9999999999998863 ) ;
#36736 = CARTESIAN_POINT ( 'NONE',  ( 7.499999999999951150, -7.420205493532891161, -2.617629953481236615 ) ) ;
#36737 = CARTESIAN_POINT ( 'NONE',  ( 102.6000270504628844, 5.819803920172570422, 5.819803920172574863 ) ) ;
#36738 = DIRECTION ( 'NONE',  ( -0.6830127018922180770, -0.6830127018922204085, -0.2588190451025213501 ) ) ;
#36739 =( NAMED_UNIT ( * ) PLANE_ANGLE_UNIT ( ) SI_UNIT ( $, .RADIAN. ) );
#36740 = ORIENTED_EDGE ( 'NONE', *, *, #54143, .T. ) ;
#36741 = LINE ( 'NONE', #69396, #88608 ) ;
#36742 = DIRECTION ( 'NONE',  ( 0.7071067811865486830, -0.7071067811865464625, -0.000000000000000000 ) ) ;
#36743 = CARTESIAN_POINT ( 'NONE',  ( 33.45983838949720024, 18.75929247661552779, 8.305906642995562805 ) ) ;
#36744 = CARTESIAN_POINT ( 'NONE',  ( 21.00000000000000000, 0.000000000000000000, 6.094999999999989981 ) ) ;
#36745 = DIRECTION ( 'NONE',  ( -0.000000000000000000, 0.000000000000000000, 1.000000000000000000 ) ) ;
#36746 = VECTOR ( 'NONE', #23509, 999.9999999999998863 ) ;
#36747 = FACE_OUTER_BOUND ( 'NONE', #109112, .T. ) ;
#36748 = DIRECTION ( 'NONE',  ( 0.000000000000000000, 1.000000000000000000, 0.000000000000000000 ) ) ;
#36749 = ORIENTED_EDGE ( 'NONE', *, *, #104011, .F. ) ;
#36750 = CARTESIAN_POINT ( 'NONE',  ( 36.48921356237310221, -27.52281430457080802, 5.000000000000000000 ) ) ;
#36751 = VERTEX_POINT ( 'NONE', #88790 ) ;
#36752 = CARTESIAN_POINT ( 'NONE',  ( 95.37543019189810423, -5.291415217122920289, -3.055000000000001492 ) ) ;
#36753 = CARTESIAN_POINT ( 'NONE',  ( 3.516654386410431599, 22.22500000000000142, 4.500000000000000888 ) ) ;
#36754 = DIRECTION ( 'NONE',  ( -0.7071067811865487940, 0.7071067811865463515, -0.000000000000000000 ) ) ;
#36755 = DIRECTION ( 'NONE',  ( 0.7071067811865486830, -0.7071067811865464625, -0.000000000000000000 ) ) ;
#36756 = CARTESIAN_POINT ( 'NONE',  ( 6.938893903907228378E-15, 14.96639925780210767, 5.000000000000000000 ) ) ;
#36757 = ORIENTED_EDGE ( 'NONE', *, *, #54193, .F. ) ;
#36758 = CARTESIAN_POINT ( 'NONE',  ( 3.792893218813436551, -11.24070752338417201, 5.000000000000000000 ) ) ;
#36759 = ORIENTED_EDGE ( 'NONE', *, *, #135511, .T. ) ;
#36760 = LINE ( 'NONE', #57136, #32382 ) ;
#36761 = CARTESIAN_POINT ( 'NONE',  ( 14.20666063542142687, 21.75929247661549937, 4.998822639870700080 ) ) ;
#36763 = ORIENTED_EDGE ( 'NONE', *, *, #135841, .F. ) ;
#36762 = DIRECTION ( 'NONE',  ( -0.7071067811865486830, -0.7071067811865464625, 0.000000000000000000 ) ) ;
#36764 = DIRECTION ( 'NONE',  ( 0.7071067811865486830, -0.7071067811865464625, -0.000000000000000000 ) ) ;
#36765 = CARTESIAN_POINT ( 'NONE',  ( -7.499999999999940492, 4.087461875839200509, 4.000000000000000000 ) ) ;
#36766 = DIRECTION ( 'NONE',  ( 0.6830127018922181881, 0.6830127018922202975, -0.2588190451025214056 ) ) ;
#36767 = FACE_OUTER_BOUND ( 'NONE', #5161, .T. ) ;
#36768 = ORIENTED_EDGE ( 'NONE', *, *, #127323, .F. ) ;
#36769 = ORIENTED_EDGE ( 'NONE', *, *, #3352, .F. ) ;
#36770 = ORIENTED_EDGE ( 'NONE', *, *, #41838, .F. ) ;
#36771 = EDGE_CURVE ( 'NONE', #34970, #86645, #143404, .T. ) ;
#36772 = CARTESIAN_POINT ( 'NONE',  ( 81.95876352523143282, 0.000000000000000000, -6.110000000000001208 ) ) ;
#36773 = ORIENTED_EDGE ( 'NONE', *, *, #51544, .F. ) ;
#36774 = ADVANCED_FACE ( 'NONE', ( #32253 ), #130149, .F. ) ;
#36775 = EDGE_CURVE ( 'NONE', #84947, #34514, #43138, .T. ) ;
#36776 = CARTESIAN_POINT ( 'NONE',  ( 0.4892135623730947680, -27.52281430457055578, 5.000000000000000000 ) ) ;
#36777 = DIRECTION ( 'NONE',  ( 0.7071067811865486830, -0.7071067811865464625, -0.000000000000000000 ) ) ;
#36778 = EDGE_CURVE ( 'NONE', #64204, #135652, #110490, .T. ) ;
#36779 = DIRECTION ( 'NONE',  ( 0.000000000000000000, -1.000000000000000000, 0.000000000000000000 ) ) ;
#36780 = DIRECTION ( 'NONE',  ( 0.7071067811865487940, 0.7071067811865463515, 0.000000000000000000 ) ) ;
#36781 = VERTEX_POINT ( 'NONE', #143144 ) ;
#36782 = ADVANCED_FACE ( 'NONE', ( #43844 ), #13320, .F. ) ;
#36783 = CARTESIAN_POINT ( 'NONE',  ( -38.99451991528749062, 28.92564299267965211, 4.000000000000000000 ) ) ;
#36784 = LINE ( 'NONE', #33958, #102216 ) ;
#36785 = CARTESIAN_POINT ( 'NONE',  ( 76.32876352523145158, 0.000000000000000000, -6.109999999999998543 ) ) ;
#36786 = EDGE_LOOP ( 'NONE', ( #89808, #27678, #15416, #61529 ) ) ;
#36787 = VECTOR ( 'NONE', #121040, 1000.000000000000000 ) ;
#36788 = EDGE_CURVE ( 'NONE', #137207, #87397, #18360, .T. ) ;
#36789 = CARTESIAN_POINT ( 'NONE',  ( -21.48921356237309155, -27.52281430457070499, 5.000000000000000000 ) ) ;
#36790 = LINE ( 'NONE', #55177, #22396 ) ;
#36791 = DIRECTION ( 'NONE',  ( 0.3543493200069162685, -0.000000000000000000, -0.9351131265310288487 ) ) ;
#36792 = VECTOR ( 'NONE', #64842, 1000.000000000000000 ) ;
#36793 = VECTOR ( 'NONE', #8325, 1000.000000000000000 ) ;
#36794 = AXIS2_PLACEMENT_3D ( 'NONE', #103646, #105101, #18050 ) ;
#36795 = ORIENTED_EDGE ( 'NONE', *, *, #17314, .F. ) ;
#36796 = ORIENTED_EDGE ( 'NONE', *, *, #95378, .T. ) ;
#36797 =( GEOMETRIC_REPRESENTATION_CONTEXT ( 3 ) GLOBAL_UNCERTAINTY_ASSIGNED_CONTEXT ( ( #16965 ) ) GLOBAL_UNIT_ASSIGNED_CONTEXT ( ( #43590, #55921, #23240 ) ) REPRESENTATION_CONTEXT ( 'NONE', 'WORKASPACE' ) );
#36798 = EDGE_CURVE ( 'NONE', #33598, #141915, #37245, .T. ) ;
#36799 = DIRECTION ( 'NONE',  ( 0.6830127018922181881, 0.6830127018922202975, -0.2588190451025214056 ) ) ;
#36800 = EDGE_CURVE ( 'NONE', #111053, #105971, #14773, .T. ) ;
#36801 = DIRECTION ( 'NONE',  ( -1.000000000000000000, -0.000000000000000000, -0.000000000000000000 ) ) ;
#36802 = CARTESIAN_POINT ( 'NONE',  ( 4.828169399223495084, -14.24070752338413648, 4.000000000000000000 ) ) ;
#36803 = VECTOR ( 'NONE', #94310, 1000.000000000000000 ) ;
#36804 = DIRECTION ( 'NONE',  ( 0.000000000000000000, -1.000000000000000000, 0.000000000000000000 ) ) ;
#36805 = EDGE_CURVE ( 'NONE', #101569, #4002, #46003, .T. ) ;
#36806 = FACE_OUTER_BOUND ( 'NONE', #45433, .T. ) ;
#36807 = CARTESIAN_POINT ( 'NONE',  ( -11.99999999999992006, -7.068876922607741697, 4.000000000000000000 ) ) ;
#36808 = VERTEX_POINT ( 'NONE', #111966 ) ;
#36809 = ORIENTED_EDGE ( 'NONE', *, *, #34882, .T. ) ;
#36810 = CARTESIAN_POINT ( 'NONE',  ( -1.499999999999990896, -14.56887692260766443, 4.000000000000000000 ) ) ;
#36811 = EDGE_LOOP ( 'NONE', ( #59704, #116421, #114878, #60761 ) ) ;
#36812 = AXIS2_PLACEMENT_3D ( 'NONE', #26913, #137837, #14615 ) ;
#36813 = CONICAL_SURFACE ( 'NONE', #36711, 2.055000000000000604, 0.9599310885968764806 ) ;
#36814 = FACE_OUTER_BOUND ( 'NONE', #77747, .T. ) ;
#36815 = ORIENTED_EDGE ( 'NONE', *, *, #97259, .F. ) ;
#36816 = DIRECTION ( 'NONE',  ( -0.7071067811865487940, 0.7071067811865463515, 0.000000000000000000 ) ) ;
#36817 = FACE_OUTER_BOUND ( 'NONE', #69566, .T. ) ;
#36818 = EDGE_CURVE ( 'NONE', #35075, #103659, #69918, .T. ) ;
#36819 = PLANE ( 'NONE',  #90189 ) ;
#36820 = AXIS2_PLACEMENT_3D ( 'NONE', #80845, #57676, #101858 ) ;
#36821 = CARTESIAN_POINT ( 'NONE',  ( -16.49999999999988987, 22.22500000000000853, 4.362957392718826988 ) ) ;
#36822 = ORIENTED_EDGE ( 'NONE', *, *, #59381, .T. ) ;
#36823 = VECTOR ( 'NONE', #124285, 1000.000000000000000 ) ;
#36824 = DIRECTION ( 'NONE',  ( -0.7071067811865486830, -0.7071067811865464625, 0.000000000000000000 ) ) ;
#36825 = AXIS2_PLACEMENT_3D ( 'NONE', #143336, #10654, #54921 ) ;
#36826 = VERTEX_POINT ( 'NONE', #14041 ) ;
#36827 = DIRECTION ( 'NONE',  ( -0.6830127018922180770, -0.6830127018922204085, -0.2588190451025213501 ) ) ;
#36828 = ORIENTED_EDGE ( 'NONE', *, *, #20755, .T. ) ;
#36829 = ORIENTED_EDGE ( 'NONE', *, *, #26100, .F. ) ;
#36830 = CARTESIAN_POINT ( 'NONE',  ( 29.99999999999979039, 18.08204922493375477, 0.9627537363044178509 ) ) ;
#36831 = ORIENTED_EDGE ( 'NONE', *, *, #125123, .T. ) ;
#36832 = VERTEX_POINT ( 'NONE', #122825 ) ;
#36833 = CARTESIAN_POINT ( 'NONE',  ( 4.969723521325230209, 2.055000000000001048, 0.000000000000000000 ) ) ;
#36834 = ORIENTED_EDGE ( 'NONE', *, *, #7869, .T. ) ;
#36835 = AXIS2_PLACEMENT_3D ( 'NONE', #33326, #77528, #34006 ) ;
#36836 = EDGE_CURVE ( 'NONE', #139503, #12106, #114772, .T. ) ;
#36837 = CARTESIAN_POINT ( 'NONE',  ( 20.99999999999985789, 16.93112307739201583, 4.000000000000000000 ) ) ;
#36838 = CARTESIAN_POINT ( 'NONE',  ( -59.99451991528749772, 28.92564299267980132, 4.000000000000000000 ) ) ;
#36839 = CARTESIAN_POINT ( 'NONE',  ( 117.2504301918981042, 3.055000000000002824, -5.291415217122919401 ) ) ;
#36840 = CARTESIAN_POINT ( 'NONE',  ( -48.18398860626899705, 28.73617430169820608, 5.000000000000000000 ) ) ;
#36841 = EDGE_CURVE ( 'NONE', #41034, #13806, #53616, .T. ) ;
#36842 = CARTESIAN_POINT ( 'NONE',  ( -51.29974487139158867, -27.71228299555242103, 4.000000000000000000 ) ) ;
#36843 = DIRECTION ( 'NONE',  ( 0.3543493200069162685, -0.000000000000000000, -0.9351131265310288487 ) ) ;
#36844 =( GEOMETRIC_REPRESENTATION_CONTEXT ( 3 ) GLOBAL_UNCERTAINTY_ASSIGNED_CONTEXT ( ( #44989 ) ) GLOBAL_UNIT_ASSIGNED_CONTEXT ( ( #81499, #61198, #120471 ) ) REPRESENTATION_CONTEXT ( 'NONE', 'WORKASPACE' ) );
#36845 = PLANE ( 'NONE',  #56314 ) ;
#36846 = CARTESIAN_POINT ( 'NONE',  ( 11.30840764549667554, 3.061616997868380183E-16, -2.500000000000001332 ) ) ;
#36847 = LINE ( 'NONE', #15761, #39013 ) ;
#36848 = ORIENTED_EDGE ( 'NONE', *, *, #86219, .T. ) ;
#36849 = DIRECTION ( 'NONE',  ( -1.000000000000000000, -1.224606353822377258E-16, -0.000000000000000000 ) ) ;
#36850 = EDGE_CURVE ( 'NONE', #68092, #93258, #12622, .T. ) ;
#36851 = EDGE_LOOP ( 'NONE', ( #116800, #48598, #93268, #105089 ) ) ;
#36852 = ORIENTED_EDGE ( 'NONE', *, *, #77404, .F. ) ;
#36853 = CARTESIAN_POINT ( 'NONE',  ( 7.828169399223476432, 12.75929247661558996, 4.000000000000000000 ) ) ;
#36854 = ORIENTED_EDGE ( 'NONE', *, *, #49916, .F. ) ;
#36855 = DIRECTION ( 'NONE',  ( 0.7071067811865486830, -0.7071067811865464625, -0.000000000000000000 ) ) ;
#36856 = CARTESIAN_POINT ( 'NONE',  ( 114.1666666666666714, 6.884901960086285300, 3.975000000000003642 ) ) ;
#36857 = CARTESIAN_POINT ( 'NONE',  ( 0.4000000000000001887, 0.000000000000000000, 0.000000000000000000 ) ) ;
#36858 = ADVANCED_FACE ( 'NONE', ( #100370 ), #134431, .T. ) ;
#36859 = DIRECTION ( 'NONE',  ( 0.6830127018922180770, -0.6830127018922204085, -0.2588190451025213501 ) ) ;
#36860 = ORIENTED_EDGE ( 'NONE', *, *, #91229, .F. ) ;
#36861 = CARTESIAN_POINT ( 'NONE',  ( -27.29974487139158512, -27.71228299555225405, 4.000000000000000000 ) ) ;
#36862 = ORIENTED_EDGE ( 'NONE', *, *, #34820, .T. ) ;
#36863 = PLANE ( 'NONE',  #104758 ) ;
#36864 = CARTESIAN_POINT ( 'NONE',  ( 28.94206980810188767, 7.934999999999993392, 2.126176841940951689 ) ) ;
#36865 = DIRECTION ( 'NONE',  ( -1.000000000000000000, -1.224606353822377258E-16, -0.000000000000000000 ) ) ;
#36866 = CARTESIAN_POINT ( 'NONE',  ( -33.70710678118631165, 14.25929247661557397, 5.000000000000000000 ) ) ;
#36867 = ORIENTED_EDGE ( 'NONE', *, *, #121567, .F. ) ;
#36868 = ORIENTED_EDGE ( 'NONE', *, *, #138230, .F. ) ;
#36869 = VERTEX_POINT ( 'NONE', #135162 ) ;
#36870 = CARTESIAN_POINT ( 'NONE',  ( 5.755190629914537226, 4.202752102959690472E-16, 0.000000000000000000 ) ) ;
#36871 = DIRECTION ( 'NONE',  ( 0.000000000000000000, -1.000000000000000000, 0.000000000000000000 ) ) ;
#36872 = DIRECTION ( 'NONE',  ( -0.7071067811865487940, 0.7071067811865463515, -0.000000000000000000 ) ) ;
#36873 = LINE ( 'NONE', #69549, #139901 ) ;
#36874 = ORIENTED_EDGE ( 'NONE', *, *, #93914, .T. ) ;
#36875 = DIRECTION ( 'NONE',  ( 0.7071067811865487940, 0.7071067811865463515, 0.000000000000000000 ) ) ;
#36876 = LINE ( 'NONE', #49224, #1723 ) ;
#36877 = EDGE_CURVE ( 'NONE', #37329, #22290, #45301, .T. ) ;
#36879 = EDGE_CURVE ( 'NONE', #117911, #143396, #101780, .T. ) ;
#36878 = LINE ( 'NONE', #4927, #46683 ) ;
#36880 = CARTESIAN_POINT ( 'NONE',  ( 34.92499999999998295, -9.183345613589446899, 4.500000000000000888 ) ) ;
#36881 = ORIENTED_EDGE ( 'NONE', *, *, #68873, .F. ) ;
#36882 = VECTOR ( 'NONE', #21101, 1000.000000000000000 ) ;
#36883 = VECTOR ( 'NONE', #113328, 999.9999999999998863 ) ;
#36884 = VECTOR ( 'NONE', #27804, 1000.000000000000000 ) ;
#36885 = VECTOR ( 'NONE', #84423, 1000.000000000000227 ) ;
#36886 = FACE_OUTER_BOUND ( 'NONE', #108547, .T. ) ;
#36887 = ORIENTED_EDGE ( 'NONE', *, *, #104810, .F. ) ;
#36888 =( BOUNDED_CURVE ( )  B_SPLINE_CURVE ( 3, ( #46367, #136898, #2056, #57952 ),
 .UNSPECIFIED., .F., .F. ) 
 B_SPLINE_CURVE_WITH_KNOTS ( ( 4, 4 ),
 ( 5.536208752217765650, 5.573248253235213667 ),
 .UNSPECIFIED. ) 
 CURVE ( )  GEOMETRIC_REPRESENTATION_ITEM ( )  RATIONAL_B_SPLINE_CURVE ( ( 1.000000000000000000, 0.9998856762146628441, 0.9998856762146628441, 1.000000000000000000 ) ) 
 REPRESENTATION_ITEM ( '' )  );
#36889 = VECTOR ( 'NONE', #114894, 1000.000000000000227 ) ;
#36890 = EDGE_CURVE ( 'NONE', #109601, #101394, #46753, .T. ) ;
#36892 = ORIENTED_EDGE ( 'NONE', *, *, #50718, .T. ) ;
#36891 = CARTESIAN_POINT ( 'NONE',  ( -20.99999999999985789, 15.45873954670183004, -0.03131636524289407170 ) ) ;
#36893 = VERTEX_POINT ( 'NONE', #69174 ) ;
#36894 = EDGE_CURVE ( 'NONE', #74888, #85582, #1020, .T. ) ;
#36895 = DIRECTION ( 'NONE',  ( 0.7071067811865487940, 0.7071067811865463515, -0.000000000000000000 ) ) ;
#36896 = CARTESIAN_POINT ( 'NONE',  ( 105.4166666666666572, -6.884901960086287076, -3.975000000000000977 ) ) ;
#36897 = ORIENTED_EDGE ( 'NONE', *, *, #5956, .F. ) ;
#36898 = CARTESIAN_POINT ( 'NONE',  ( 25.39999999999999858, 7.464222240803104598E-16, -6.094999999999989093 ) ) ;
#36899 = AXIS2_PLACEMENT_3D ( 'NONE', #695, #133392, #23151 ) ;
#36900 = EDGE_LOOP ( 'NONE', ( #62119, #120729, #21318, #26267 ) ) ;
#36901 = CARTESIAN_POINT ( 'NONE',  ( 15.45983838949730860, 18.75929247661552779, 8.305906642995520173 ) ) ;
#36902 = FACE_OUTER_BOUND ( 'NONE', #17251, .T. ) ;
#36903 = CARTESIAN_POINT ( 'NONE',  ( 127.1000270504628986, 5.819803920172570422, 5.819803920172574863 ) ) ;
#36904 = CARTESIAN_POINT ( 'NONE',  ( -18.48921356237309510, -27.52281430457068367, 5.000000000000000000 ) ) ;
#36905 = DIRECTION ( 'NONE',  ( -0.3543493200069162685, -0.000000000000000000, -0.9351131265310288487 ) ) ;
#36906 = FACE_OUTER_BOUND ( 'NONE', #76600, .T. ) ;
#36907 = CARTESIAN_POINT ( 'NONE',  ( -30.15612307739222331, -22.22500000000000853, 4.000000000000000000 ) ) ;
#36908 = DIRECTION ( 'NONE',  ( 0.7071067811865487940, 0.7071067811865463515, 0.000000000000000000 ) ) ;
#36909 = DIRECTION ( 'NONE',  ( -0.7071067811865486830, 0.7071067811865464625, 0.000000000000000000 ) ) ;
#36910 = CARTESIAN_POINT ( 'NONE',  ( 31.47873647476854941, -5.808823158059033709, 5.808823158059035485 ) ) ;
#36912 = VECTOR ( 'NONE', #23720, 1000.000000000000000 ) ;
#36911 = CARTESIAN_POINT ( 'NONE',  ( 0.9995698081018860037, -3.967499999999998028, -6.871911579029511330 ) ) ;
#36913 = CARTESIAN_POINT ( 'NONE',  ( -15.32816939922343202, 11.25929247661560595, 4.000000000000000000 ) ) ;
#36914 = VECTOR ( 'NONE', #90936, 1000.000000000000000 ) ;
#36915 = CARTESIAN_POINT ( 'NONE',  ( 48.48921356237309510, -27.52281430457089328, 5.000000000000000000 ) ) ;
#36916 = DIRECTION ( 'NONE',  ( 1.000000000000000000, 0.000000000000000000, 0.000000000000000000 ) ) ;
#36917 = EDGE_LOOP ( 'NONE', ( #139450, #21444, #78577, #136144 ) ) ;
#36918 = EDGE_CURVE ( 'NONE', #77610, #40891, #3170, .T. ) ;
#36919 = VERTEX_POINT ( 'NONE', #89476 ) ;
#36920 = CARTESIAN_POINT ( 'NONE',  ( 91.56250000000000000, -5.819803920172572198, -5.819803920172573086 ) ) ;
#36921 = VECTOR ( 'NONE', #137334, 999.9999999999998863 ) ;
#36922 = ORIENTED_EDGE ( 'NONE', *, *, #71221, .F. ) ;
#36923 = ORIENTED_EDGE ( 'NONE', *, *, #43045, .F. ) ;
#36924 = SURFACE_STYLE_USAGE ( .BOTH. , #47854 ) ;
#36925 = CARTESIAN_POINT ( 'NONE',  ( 34.92499999999998295, 22.22500000000000142, 4.500000000000000888 ) ) ;
#36926 = DIRECTION ( 'NONE',  ( -1.000000000000000000, -0.000000000000000000, -0.000000000000000000 ) ) ;
#36927 = ORIENTED_EDGE ( 'NONE', *, *, #101358, .F. ) ;
#36928 = VECTOR ( 'NONE', #50187, 999.9999999999998863 ) ;
#36929 = CARTESIAN_POINT ( 'NONE',  ( 29.67183060077626777, 11.25929247661560595, 4.000000000000000000 ) ) ;
#36930 = CIRCLE ( 'NONE', #60143, 2.500000000000000444 ) ;
#36931 = DIRECTION ( 'NONE',  ( 0.7071067811865487940, 0.7071067811865463515, 0.000000000000000000 ) ) ;
#36932 = AXIS2_PLACEMENT_3D ( 'NONE', #51549, #8000, #60295 ) ;
#36933 = CARTESIAN_POINT ( 'NONE',  ( 5.293207492759216315, 20.25929247661550647, 20.83292124670813550 ) ) ;
#36934 = LINE ( 'NONE', #115894, #23408 ) ;
#36935 = VECTOR ( 'NONE', #66754, 1000.000000000000000 ) ;
#36936 = DIRECTION ( 'NONE',  ( 0.000000000000000000, 0.000000000000000000, 1.000000000000000000 ) ) ;
#36937 = DIRECTION ( 'NONE',  ( -1.000000000000000000, 0.000000000000000000, 0.000000000000000000 ) ) ;
#36938 = VECTOR ( 'NONE', #3224, 999.9999999999998863 ) ;
#36939 = DIRECTION ( 'NONE',  ( 0.7071067811865486830, -0.7071067811865464625, -0.000000000000000000 ) ) ;
#36940 = CARTESIAN_POINT ( 'NONE',  ( 24.79996877983148096, 8.259292476615630818, 16.85664084051835232 ) ) ;
#36941 = PLANE ( 'NONE',  #52341 ) ;
#36942 = DIRECTION ( 'NONE',  ( 0.7071067811865487940, 0.7071067811865463515, -0.000000000000000000 ) ) ;
#36943 = DIRECTION ( 'NONE',  ( -0.7071067811865486830, -0.7071067811865464625, 0.000000000000000000 ) ) ;
#36944 = VERTEX_POINT ( 'NONE', #135846 ) ;
#36945 = ORIENTED_EDGE ( 'NONE', *, *, #107993, .F. ) ;
#36946 = ADVANCED_FACE ( 'NONE', ( #36529 ), #13803, .T. ) ;
#36947 = CARTESIAN_POINT ( 'NONE',  ( 109.5212635252314612, -4.472830434245839371, -4.472830434245840259 ) ) ;
#36948 = ORIENTED_EDGE ( 'NONE', *, *, #81725, .T. ) ;
#36949 = EDGE_CURVE ( 'NONE', #10046, #44215, #114090, .T. ) ;
#36950 = CARTESIAN_POINT ( 'NONE',  ( -27.29974487139158512, -27.71228299555225405, 4.000000000000000000 ) ) ;
#36951 = VECTOR ( 'NONE', #19966, 1000.000000000000227 ) ;
#36952 = CARTESIAN_POINT ( 'NONE',  ( -60.48921356237309510, -27.52281430457097500, 5.000000000000000000 ) ) ;
#36953 = ORIENTED_EDGE ( 'NONE', *, *, #17744, .F. ) ;
#36954 = EDGE_CURVE ( 'NONE', #80135, #116730, #41562, .T. ) ;
#36955 = EDGE_CURVE ( 'NONE', #70831, #44164, #95178, .T. ) ;
#36956 = FACE_OUTER_BOUND ( 'NONE', #52832, .T. ) ;
#36957 = DIRECTION ( 'NONE',  ( 0.000000000000000000, 0.000000000000000000, 1.000000000000000000 ) ) ;
#36958 = CARTESIAN_POINT ( 'NONE',  ( 101.9954301918981230, 5.291415217122916737, 3.055000000000001936 ) ) ;
#36959 = VERTEX_POINT ( 'NONE', #127843 ) ;
#36960 = ORIENTED_EDGE ( 'NONE', *, *, #95698, .F. ) ;
#36961 = DIRECTION ( 'NONE',  ( -0.000000000000000000, -0.000000000000000000, 1.000000000000000000 ) ) ;
#36962 = LINE ( 'NONE', #23406, #98137 ) ;
#36963 = CARTESIAN_POINT ( 'NONE',  ( -1.171830600776463838, -5.240707523384232402, 4.000000000000000000 ) ) ;
#36964 = ORIENTED_EDGE ( 'NONE', *, *, #30142, .T. ) ;
#36965 = VERTEX_POINT ( 'NONE', #137994 ) ;
#36966 = ADVANCED_FACE ( 'NONE', ( #71315 ), #16164, .F. ) ;
#36967 = ORIENTED_EDGE ( 'NONE', *, *, #75745, .T. ) ;
#36968 = CARTESIAN_POINT ( 'NONE',  ( 9.770042794577866729, 21.73644205237998506, 5.000000000000000888 ) ) ;
#36969 = EDGE_CURVE ( 'NONE', #13095, #141411, #82211, .T. ) ;
#36970 = EDGE_CURVE ( 'NONE', #43634, #110134, #5301, .T. ) ;
#36971 = LINE ( 'NONE', #82638, #91742 ) ;
#36972 = VERTEX_POINT ( 'NONE', #117617 ) ;
#36973 = EDGE_LOOP ( 'NONE', ( #27154, #48549, #116792, #47056 ) ) ;
#36974 = CARTESIAN_POINT ( 'NONE',  ( -11.99999999999991296, 11.96639925780213964, 5.000000000000000000 ) ) ;
#36975 = ORIENTED_EDGE ( 'NONE', *, *, #91955, .F. ) ;
#36976 = ORIENTED_EDGE ( 'NONE', *, *, #84694, .F. ) ;
#36977 = EDGE_CURVE ( 'NONE', #118451, #83429, #83634, .T. ) ;
#36978 = LINE ( 'NONE', #81234, #51732 ) ;
#36979 = FACE_OUTER_BOUND ( 'NONE', #115322, .T. ) ;
#36980 = ORIENTED_EDGE ( 'NONE', *, *, #79198, .T. ) ;
#36981 = DIRECTION ( 'NONE',  ( -0.7071067811865486830, -0.7071067811865464625, 0.000000000000000000 ) ) ;
#36982 = AXIS2_PLACEMENT_3D ( 'NONE', #128803, #49138, #125974 ) ;
#36983 = CARTESIAN_POINT ( 'NONE',  ( -23.20666063542136470, 21.75929247661548516, 4.998822639870711626 ) ) ;
#36984 = ADVANCED_FACE ( 'NONE', ( #61874 ), #27790, .T. ) ;
#36985 = LINE ( 'NONE', #60195, #1982 ) ;
#36986 = VECTOR ( 'NONE', #7955, 999.9999999999998863 ) ;
#36987 = VECTOR ( 'NONE', #33868, 999.9999999999998863 ) ;
#36988 = VECTOR ( 'NONE', #123486, 999.9999999999998863 ) ;
#36989 = FILL_AREA_STYLE ('',( #58083 ) ) ;
#36990 = VECTOR ( 'NONE', #25597, 1000.000000000000000 ) ;
#36991 = DIRECTION ( 'NONE',  ( 2.781805975412905890E-17, -0.3543493200069152693, 0.9351131265310292928 ) ) ;
#36992 = FACE_BOUND ( 'NONE', #32086, .T. ) ;
#36993 = ORIENTED_EDGE ( 'NONE', *, *, #116962, .T. ) ;
#36994 = CARTESIAN_POINT ( 'NONE',  ( 5.671830600776432973, 17.25929247661555266, 4.000000000000000000 ) ) ;
#36995 = DIRECTION ( 'NONE',  ( 1.000000000000000000, 1.224606353822377258E-16, 0.000000000000000000 ) ) ;
#36996 = CARTESIAN_POINT ( 'NONE',  ( 25.39999999999999858, -14.29000000000013593, -12.70000000000045404 ) ) ;
#36997 = ORIENTED_EDGE ( 'NONE', *, *, #53007, .T. ) ;
#36998 = ADVANCED_FACE ( 'NONE', ( #72054 ), #61192, .T. ) ;
#36999 = CARTESIAN_POINT ( 'NONE',  ( -23.81601139373100295, 28.73617430169770870, 5.000000000000000000 ) ) ;
#37000 = ORIENTED_EDGE ( 'NONE', *, *, #121060, .T. ) ;
#37001 = EDGE_CURVE ( 'NONE', #62199, #87041, #104633, .T. ) ;
#37002 = ORIENTED_EDGE ( 'NONE', *, *, #7969, .T. ) ;
#37003 = AXIS2_PLACEMENT_3D ( 'NONE', #22115, #12668, #44651 ) ;
#37004 = ORIENTED_EDGE ( 'NONE', *, *, #28252, .F. ) ;
#37005 = ADVANCED_FACE ( 'NONE', ( #49583 ), #40818, .F. ) ;
#37006 = CARTESIAN_POINT ( 'NONE',  ( 38.84959685856477307, 6.109999999999996767, 1.637169565754163836 ) ) ;
#37007 = ORIENTED_EDGE ( 'NONE', *, *, #29657, .T. ) ;
#37008 = VECTOR ( 'NONE', #82541, 999.9999999999998863 ) ;
#37009 =( BOUNDED_CURVE ( )  B_SPLINE_CURVE ( 2, ( #95358, #140996, #38849, #127269, #41702, #115648, #84511, #61361, #117098, #27970, #72240, #105505, #6171 ),
 .UNSPECIFIED., .F., .T. ) 
 B_SPLINE_CURVE_WITH_KNOTS ( ( 3, 2, 2, 2, 2, 2, 3 ),
 ( 0.5666666666666666519, 0.5694444444444444198, 0.5722222222222221877, 0.5749999999999999556, 0.5777777777777777235, 0.5805555555555556024, 0.5833333333333333703 ),
 .UNSPECIFIED. ) 
 CURVE ( )  GEOMETRIC_REPRESENTATION_ITEM ( )  RATIONAL_B_SPLINE_CURVE ( ( 1.000000000000000000, 0.9659258262890683122, 1.000000000000000000, 0.9659258262890683122, 1.000000000000000000, 0.9659258262890683122, 1.000000000000000000, 0.9659258262890683122, 1.000000000000000000, 0.9659258262890683122, 1.000000000000000000, 0.9659258262890683122, 1.000000000000000000 ) ) 
 REPRESENTATION_ITEM ( '' )  );
#37010 = DIRECTION ( 'NONE',  ( -0.7071067811865486830, -0.7071067811865464625, 0.000000000000000000 ) ) ;
#37011 = SURFACE_STYLE_FILL_AREA ( #58833 ) ;
#37012 = CARTESIAN_POINT ( 'NONE',  ( -41.99451991528749062, 28.92564299267967343, 4.000000000000000000 ) ) ;
#37013 = B_SPLINE_CURVE_WITH_KNOTS ( 'NONE', 3,
 ( #42069, #43479, #86283, #130507, #31186, #669, #87691, #121026, #75401, #120278, #32619, #20994, #10125, #143492, #131927, #10816, #65979, #110136, #77559, #44213, #9375, #88428, #34047, #132668, #44960, #89137, #121728, #53651, #119576, #20273, #92666, #134800, #69538, #100721, #114433, #135498 ),
 .UNSPECIFIED., .F., .F.,
 ( 4, 2, 2, 2, 2, 2, 2, 2, 2, 2, 2, 2, 2, 2, 2, 2, 2, 4 ),
 ( 0.02080955487772951848, 0.02167635536089138754, 0.02254315584405326006, 0.02340995632721513259, 0.02427675681037700164, 0.02514355729353887070, 0.02557695753511981043, 0.02601035777670074670, 0.02687715825986262269, 0.02774395874302449522, 0.02861075922618637468, 0.02947755970934824721, 0.03034436019251012667, 0.03121116067567199920, 0.03207796115883387866, 0.03294476164199575813, 0.03381156212515763065, 0.03467836260831951012 ),
 .UNSPECIFIED. ) ;
#37014 = ORIENTED_EDGE ( 'NONE', *, *, #110949, .T. ) ;
#37015 = DIRECTION ( 'NONE',  ( -1.000000000000000000, 0.000000000000000000, 0.000000000000000000 ) ) ;
#37016 = PLANE ( 'NONE',  #8749 ) ;
#37017 = VECTOR ( 'NONE', #89343, 1000.000000000000227 ) ;
#37018 = VECTOR ( 'NONE', #109326, 1000.000000000000000 ) ;
#37019 = FACE_OUTER_BOUND ( 'NONE', #19298, .T. ) ;
#37020 = MECHANICAL_DESIGN_GEOMETRIC_PRESENTATION_REPRESENTATION (  '', ( #4466 ), #29981 ) ;
#37021 = CARTESIAN_POINT ( 'NONE',  ( 59.99451991528749772, 28.92564299267980132, 4.000000000000000000 ) ) ;
#37022 = PLANE ( 'NONE',  #6882 ) ;
#37023 = DIRECTION ( 'NONE',  ( 0.000000000000000000, 1.000000000000000000, -0.000000000000000000 ) ) ;
#37024 = LINE ( 'NONE', #81272, #47087 ) ;
#37025 = EDGE_LOOP ( 'NONE', ( #12878, #10621, #100805, #104360 ) ) ;
#37026 = ORIENTED_EDGE ( 'NONE', *, *, #24647, .F. ) ;
#37027 = ORIENTED_EDGE ( 'NONE', *, *, #113275, .T. ) ;
#37028 = ORIENTED_EDGE ( 'NONE', *, *, #5719, .F. ) ;
#37029 = DIRECTION ( 'NONE',  ( -0.000000000000000000, 0.3543493200069153248, 0.9351131265310292928 ) ) ;
#37030 = VERTEX_POINT ( 'NONE', #103895 ) ;
#37031 = VECTOR ( 'NONE', #133415, 1000.000000000000114 ) ;
#37032 = ORIENTED_EDGE ( 'NONE', *, *, #119297, .F. ) ;
#37033 = PLANE ( 'NONE',  #72266 ) ;
#37034 = DIRECTION ( 'NONE',  ( -0.6830127018922181881, 0.6830127018922202975, -0.2588190451025214056 ) ) ;
#37035 = VECTOR ( 'NONE', #135417, 1000.000000000000227 ) ;
#37036 = DIRECTION ( 'NONE',  ( 0.000000000000000000, 1.000000000000000000, 0.000000000000000000 ) ) ;
#37037 = VERTEX_POINT ( 'NONE', #82905 ) ;
#37038 = VECTOR ( 'NONE', #18191, 1000.000000000000000 ) ;
#37039 = CARTESIAN_POINT ( 'NONE',  ( 57.48921356237308800, -27.52281430457095368, 5.000000000000000000 ) ) ;
#37040 = VERTEX_POINT ( 'NONE', #139451 ) ;
#37041 = CARTESIAN_POINT ( 'NONE',  ( -29.20710678118634007, 9.759292476615621936, 5.000000000000000000 ) ) ;
#37042 = DIRECTION ( 'NONE',  ( -1.000000000000000000, -0.000000000000000000, -0.000000000000000000 ) ) ;
#37043 = VECTOR ( 'NONE', #120594, 1000.000000000000000 ) ;
#37044 = CARTESIAN_POINT ( 'NONE',  ( 3.275403141435220267, -2.126176841940958351, -7.934999999999989839 ) ) ;
#37045 = ORIENTED_EDGE ( 'NONE', *, *, #10259, .F. ) ;
#37046 = CARTESIAN_POINT ( 'NONE',  ( 105.6412635252314658, 4.472830434245837594, 4.472830434245841147 ) ) ;
#37047 = DIRECTION ( 'NONE',  ( -1.000000000000000000, -1.224606353822377258E-16, -0.000000000000000000 ) ) ;
#37048 = PRESENTATION_STYLE_ASSIGNMENT (( #92129 ) ) ;
#37049 = ORIENTED_EDGE ( 'NONE', *, *, #115714, .F. ) ;
#37050 = EDGE_LOOP ( 'NONE', ( #61141, #95158, #115236, #137456, #91381 ) ) ;
#37051 = DIRECTION ( 'NONE',  ( 0.7071067811865487940, 0.7071067811865463515, 0.000000000000000000 ) ) ;
#37052 = AXIS2_PLACEMENT_3D ( 'NONE', #69959, #69212, #124287 ) ;
#37053 = ORIENTED_EDGE ( 'NONE', *, *, #95395, .T. ) ;
#37054 = DIRECTION ( 'NONE',  ( 0.7071067811865487940, 0.7071067811865463515, -0.000000000000000000 ) ) ;
#37055 = DIRECTION ( 'NONE',  ( -0.7071067811865487940, 0.7071067811865463515, 0.000000000000000000 ) ) ;
#37056 = CARTESIAN_POINT ( 'NONE',  ( 26.99999999999981171, -21.84840872380821963, 2.849755605029670846 ) ) ;
#37057 = CARTESIAN_POINT ( 'NONE',  ( 15.98840764549667703, 2.500000000000003553, 3.061616997868386099E-16 ) ) ;
#37058 = VERTEX_POINT ( 'NONE', #5997 ) ;
#37059 = CARTESIAN_POINT ( 'NONE',  ( 20.29387692260790743, 22.22500000000000142, 4.000000000000000000 ) ) ;
#37060 = CARTESIAN_POINT ( 'NONE',  ( -34.49999999999975842, -8.568876922607724822, 4.000000000000000000 ) ) ;
#37061 = LINE ( 'NONE', #26903, #67733 ) ;
#37062 = ORIENTED_EDGE ( 'NONE', *, *, #67562, .F. ) ;
#37063 = DIRECTION ( 'NONE',  ( 0.7071067811865487940, 0.7071067811865463515, 0.000000000000000000 ) ) ;
#37064 = VECTOR ( 'NONE', #53068, 999.9999999999998863 ) ;
#37065 = DIRECTION ( 'NONE',  ( -0.3543493200069162685, -0.000000000000000000, -0.9351131265310288487 ) ) ;
#37066 = ORIENTED_EDGE ( 'NONE', *, *, #133855, .T. ) ;
#37067 = ADVANCED_FACE ( 'NONE', ( #40137 ), #50273, .F. ) ;
#37069 = ORIENTED_EDGE ( 'NONE', *, *, #12717, .F. ) ;
#37068 = CARTESIAN_POINT ( 'NONE',  ( 26.20710678118636494, 12.75929247661558996, 5.000000000000000000 ) ) ;
#37071 = ORIENTED_EDGE ( 'NONE', *, *, #92566, .F. ) ;
#37070 = EDGE_CURVE ( 'NONE', #72412, #135854, #29917, .T. ) ;
#37072 = CARTESIAN_POINT ( 'NONE',  ( 18.48921356237309510, -27.52281430457068367, 5.000000000000000000 ) ) ;
#37074 = ORIENTED_EDGE ( 'NONE', *, *, #140727, .F. ) ;
#37073 = AXIS2_PLACEMENT_3D ( 'NONE', #75110, #119279, #86686 ) ;
#37075 = DIRECTION ( 'NONE',  ( 0.000000000000000000, 0.000000000000000000, 1.000000000000000000 ) ) ;
#37076 = CLOSED_SHELL ( 'NONE', ( #43315, #107423, #133130, #97814, #41546, #131185, #69596, #112026 ) ) ;
#37077 = LINE ( 'NONE', #49424, #89184 ) ;
#37078 = DIRECTION ( 'NONE',  ( -0.6830127018922181881, 0.6830127018922202975, -0.2588190451025214056 ) ) ;
#37079 = EDGE_LOOP ( 'NONE', ( #62720, #81116, #19623, #131902 ) ) ;
#37080 = ADVANCED_FACE ( 'NONE', ( #116936 ), #50985, .F. ) ;
#37081 = PLANE ( 'NONE',  #87850 ) ;
#37082 = DIRECTION ( 'NONE',  ( 0.000000000000000000, 0.000000000000000000, 1.000000000000000000 ) ) ;
#37083 = CARTESIAN_POINT ( 'NONE',  ( -84.18398860626899705, 28.73617430169846187, 5.000000000000000000 ) ) ;
#37084 = CARTESIAN_POINT ( 'NONE',  ( 0.000000000000000000, 0.000000000000000000, 5.000000000000000000 ) ) ;
#37085 = DIRECTION ( 'NONE',  ( 0.000000000000000000, -0.000000000000000000, -1.000000000000000000 ) ) ;
#37086 = CARTESIAN_POINT ( 'NONE',  ( -34.92499999999999005, 1.196650378695320427, -30.59010235425025215 ) ) ;
#37087 = LINE ( 'NONE', #14630, #100986 ) ;
#37088 = ORIENTED_EDGE ( 'NONE', *, *, #138060, .T. ) ;
#37089 = EDGE_CURVE ( 'NONE', #59942, #51133, #95898, .T. ) ;
#37090 = ORIENTED_EDGE ( 'NONE', *, *, #33250, .T. ) ;
#37091 = ORIENTED_EDGE ( 'NONE', *, *, #133318, .T. ) ;
#37092 = CARTESIAN_POINT ( 'NONE',  ( 116.6458333333333428, 2.130196079827431976, -7.949999999999999289 ) ) ;
#37093 = TOROIDAL_SURFACE ( 'NONE', #127328, 2.500000000000000000, 0.5000000000000000000 ) ;
#37094 = ORIENTED_EDGE ( 'NONE', *, *, #113549, .T. ) ;
#37095 = ORIENTED_EDGE ( 'NONE', *, *, #8587, .F. ) ;
#37096 = EDGE_LOOP ( 'NONE', ( #118959, #142014, #82402, #100003 ) ) ;
#37097 = VECTOR ( 'NONE', #13948, 1000.000000000000000 ) ;
#37098 = CARTESIAN_POINT ( 'NONE',  ( -23.72174548431413044, 8.259292476615634371, 11.78515199841145034 ) ) ;
#37100 = EDGE_CURVE ( 'NONE', #19920, #138101, #15445, .T. ) ;
#37099 = VECTOR ( 'NONE', #57229, 1000.000000000000000 ) ;
#37101 = VECTOR ( 'NONE', #58165, 1000.000000000000227 ) ;
#37102 = MECHANICAL_DESIGN_GEOMETRIC_PRESENTATION_REPRESENTATION (  '', ( #108784 ), #30165 ) ;
#37103 = VERTEX_POINT ( 'NONE', #65452 ) ;
#37104 = VECTOR ( 'NONE', #53434, 1000.000000000000000 ) ;
#37105 = CARTESIAN_POINT ( 'NONE',  ( -12.69999999999998153, 3.061616997868383634E-16, -2.500000000000000444 ) ) ;
#37106 = CARTESIAN_POINT ( 'NONE',  ( 17.67183060077634948, -9.740707523384180888, 4.000000000000000000 ) ) ;
#37107 = CARTESIAN_POINT ( 'NONE',  ( 113.0212635252314186, -4.472830434245839371, -4.472830434245840259 ) ) ;
#37108 = VERTEX_POINT ( 'NONE', #87882 ) ;
#37109 = PLANE ( 'NONE',  #62715 ) ;
#37110 = CARTESIAN_POINT ( 'NONE',  ( -15.32816939922342137, 17.25929247661553489, 4.000000000000000000 ) ) ;
#37111 = CYLINDRICAL_SURFACE ( 'NONE', #14936, 0.5000000000000004441 ) ;
#37112 = VECTOR ( 'NONE', #102924, 1000.000000000000000 ) ;
#37113 = CARTESIAN_POINT ( 'NONE',  ( 1.233494112018948430, 2.059985402953470324, 6.548285138816920536 ) ) ;
#37114 = CARTESIAN_POINT ( 'NONE',  ( 47.99451991528749062, 28.92564299267971251, 4.000000000000000000 ) ) ;
#37115 = DIRECTION ( 'NONE',  ( 1.000000000000000000, 0.000000000000000000, 0.000000000000000000 ) ) ;
#37116 = FACE_OUTER_BOUND ( 'NONE', #92996, .T. ) ;
#37117 = CARTESIAN_POINT ( 'NONE',  ( 36.10002705046289151, 5.819803920172570422, 5.819803920172574863 ) ) ;
#37118 = PLANE ( 'NONE',  #18916 ) ;
#37119 = FACE_OUTER_BOUND ( 'NONE', #114533, .T. ) ;
#37120 = EDGE_LOOP ( 'NONE', ( #45437, #129677, #70879, #70349, #55405 ) ) ;
#37121 = VERTEX_POINT ( 'NONE', #129968 ) ;
#37122 = CARTESIAN_POINT ( 'NONE',  ( 40.37499999999999289, 7.950000000000000178, 1.460391307983218535E-15 ) ) ;
#37123 = EDGE_LOOP ( 'NONE', ( #102101, #62154, #134795, #140801 ) ) ;
#37124 = ORIENTED_EDGE ( 'NONE', *, *, #68395, .T. ) ;
#37125 = FACE_OUTER_BOUND ( 'NONE', #57718, .T. ) ;
#37126 = EDGE_CURVE ( 'NONE', #87956, #64810, #107487, .T. ) ;
#37127 = CIRCLE ( 'NONE', #127358, 2.500000000000000444 ) ;
#37128 = FACE_OUTER_BOUND ( 'NONE', #114268, .T. ) ;
#37129 = ORIENTED_EDGE ( 'NONE', *, *, #101009, .T. ) ;
#37130 = DIRECTION ( 'NONE',  ( -1.000000000000000000, -0.000000000000000000, -0.000000000000000000 ) ) ;
#37132 = EDGE_CURVE ( 'NONE', #65560, #17549, #81023, .T. ) ;
#37131 = CARTESIAN_POINT ( 'NONE',  ( -24.29974487139158867, -27.71228299555223273, 4.000000000000000000 ) ) ;
#37133 = EDGE_CURVE ( 'NONE', #68247, #83424, #19763, .T. ) ;
#37134 = CARTESIAN_POINT ( 'NONE',  ( 24.29974487139158867, -27.71228299555223273, 4.000000000000000000 ) ) ;
#37135 = VECTOR ( 'NONE', #85986, 1000.000000000000000 ) ;
#37136 = VECTOR ( 'NONE', #98694, 1000.000000000000000 ) ;
#37137 = CARTESIAN_POINT ( 'NONE',  ( 32.37543019189810423, -5.291415217122920289, -3.055000000000001492 ) ) ;
#37138 = VERTEX_POINT ( 'NONE', #52390 ) ;
#37139 = VECTOR ( 'NONE', #46796, 999.9999999999998863 ) ;
#37140 = CARTESIAN_POINT ( 'NONE',  ( -36.48921356237310221, -27.52281430457080802, 5.000000000000000000 ) ) ;
#37141 = VERTEX_POINT ( 'NONE', #132123 ) ;
#37142 = DIRECTION ( 'NONE',  ( -0.000000000000000000, 0.9647414015272155474, -0.2631995976047525887 ) ) ;
#37144 = EDGE_CURVE ( 'NONE', #122865, #13632, #77037, .T. ) ;
#37143 = VECTOR ( 'NONE', #121410, 1000.000000000000000 ) ;
#37145 = LINE ( 'NONE', #81399, #52337 ) ;
#37146 =( LENGTH_UNIT ( ) NAMED_UNIT ( * ) SI_UNIT ( .MILLI., .METRE. ) );
#37147 = FACE_OUTER_BOUND ( 'NONE', #125644, .T. ) ;
#37148 = VERTEX_POINT ( 'NONE', #140814 ) ;
#37149 = EDGE_CURVE ( 'NONE', #27619, #86236, #48506, .T. ) ;
#37150 = VERTEX_POINT ( 'NONE', #85728 ) ;
#37151 = AXIS2_PLACEMENT_3D ( 'NONE', #11349, #53475, #86827 ) ;
#37152 = CARTESIAN_POINT ( 'NONE',  ( 15.18398860626900237, 28.73617430169797871, 5.000000000000000000 ) ) ;
#37153 = ADVANCED_FACE ( 'NONE', ( #119071 ), #97292, .F. ) ;
#37154 = DIRECTION ( 'NONE',  ( -0.7071067811865486830, -0.7071067811865464625, 0.000000000000000000 ) ) ;
#37155 = CARTESIAN_POINT ( 'NONE',  ( -6.793339364578430128, 21.75929247661548871, 4.998822639870703632 ) ) ;
#37156 = EDGE_CURVE ( 'NONE', #33217, #59038, #44414, .T. ) ;
#37157 = VECTOR ( 'NONE', #88090, 1000.000000000000000 ) ;
#37158 = EDGE_CURVE ( 'NONE', #84039, #139138, #55265, .T. ) ;
#37159 = CARTESIAN_POINT ( 'NONE',  ( 50.66209685856478018, -5.291415217122919401, 3.054999999999997939 ) ) ;
#37160 = DIRECTION ( 'NONE',  ( -1.000000000000000000, -0.000000000000000000, -0.000000000000000000 ) ) ;
#37161 = LINE ( 'NONE', #124174, #84833 ) ;
#37162 = ORIENTED_EDGE ( 'NONE', *, *, #92943, .T. ) ;
#37163 = ORIENTED_EDGE ( 'NONE', *, *, #82817, .F. ) ;
#37164 = VECTOR ( 'NONE', #4979, 999.9999999999998863 ) ;
#37165 = CARTESIAN_POINT ( 'NONE',  ( 34.92499999999998295, 14.19452376399133442, 8.043047640789311004 ) ) ;
#37166 = ADVANCED_FACE ( 'NONE', ( #120467 ), #121212, .F. ) ;
#37167 = ORIENTED_EDGE ( 'NONE', *, *, #21580, .T. ) ;
#37168 = FACE_OUTER_BOUND ( 'NONE', #22047, .T. ) ;
#37169 = EDGE_LOOP ( 'NONE', ( #129195, #47106, #13212, #86086 ) ) ;
#37170 = CARTESIAN_POINT ( 'NONE',  ( -28.17183060077627488, 3.759292476615683665, 4.000000000000000000 ) ) ;
#37171 = DIRECTION ( 'NONE',  ( 0.000000000000000000, 1.000000000000000000, 0.000000000000000000 ) ) ;
#37172 = CIRCLE ( 'NONE', #4717, 2.500000000000000444 ) ;
#37173 = DIRECTION ( 'NONE',  ( 0.7071067811865486830, -0.7071067811865464625, -0.000000000000000000 ) ) ;
#37174 = FACE_BOUND ( 'NONE', #49938, .T. ) ;
#37175 = DIRECTION ( 'NONE',  ( 0.7071067811865487940, 0.7071067811865463515, -0.000000000000000000 ) ) ;
#37176 = LINE ( 'NONE', #92251, #65273 ) ;
#37177 = CARTESIAN_POINT ( 'NONE',  ( 30.29974487139158867, -27.71228299555227537, 4.000000000000000000 ) ) ;
#37178 = FILL_AREA_STYLE ('',( #136484 ) ) ;
#37180 = ORIENTED_EDGE ( 'NONE', *, *, #9833, .F. ) ;
#37179 = DIRECTION ( 'NONE',  ( -0.7071067811865486830, -0.7071067811865464625, -0.000000000000000000 ) ) ;
#37181 = AXIS2_PLACEMENT_3D ( 'NONE', #16782, #82770, #102394 ) ;
#37182 = CONICAL_SURFACE ( 'NONE', #23287, 2.552699999999928693, 1.029744258676634772 ) ;
#37183 = DIRECTION ( 'NONE',  ( -0.7071067811865486830, -0.7071067811865464625, 0.000000000000000000 ) ) ;
#37184 = VERTEX_POINT ( 'NONE', #86473 ) ;
#37185 = ADVANCED_FACE ( 'NONE', ( #130703 ), #142287, .T. ) ;
#37186 = EDGE_CURVE ( 'NONE', #94430, #118518, #53090, .T. ) ;
#37187 = ORIENTED_EDGE ( 'NONE', *, *, #51509, .F. ) ;
#37188 = CARTESIAN_POINT ( 'NONE',  ( 70.64126352523145158, 4.472830434245835818, 4.472830434245840259 ) ) ;
#37189 = ORIENTED_EDGE ( 'NONE', *, *, #65628, .F. ) ;
#37190 = CARTESIAN_POINT ( 'NONE',  ( -2.510786437626908008, -27.52281430457053446, 5.000000000000000000 ) ) ;
#37191 = CARTESIAN_POINT ( 'NONE',  ( 2.999999999999981792, -19.06887692260762179, 4.000000000000000000 ) ) ;
#37192 = ORIENTED_EDGE ( 'NONE', *, *, #39102, .T. ) ;
#37193 = DIRECTION ( 'NONE',  ( 0.000000000000000000, 1.000000000000000000, 0.000000000000000000 ) ) ;
#37195 = ADVANCED_FACE ( 'NONE', ( #9580 ), #53853, .F. ) ;
#37194 = VECTOR ( 'NONE', #66800, 999.9999999999998863 ) ;
#37196 = AXIS2_PLACEMENT_3D ( 'NONE', #136856, #58653, #47750 ) ;
#37197 = AXIS2_PLACEMENT_3D ( 'NONE', #51797, #73542, #107571 ) ;
#37198 = DIRECTION ( 'NONE',  ( -0.7071067811865487940, 0.7071067811865463515, -0.000000000000000000 ) ) ;
#37199 = CARTESIAN_POINT ( 'NONE',  ( -15.29974487139158867, -27.71228299555216879, 4.000000000000000000 ) ) ;
#37200 = CARTESIAN_POINT ( 'NONE',  ( -26.01088028653930451, -22.02621442084248216, 4.990779571109225543 ) ) ;
#37201 = CARTESIAN_POINT ( 'NONE',  ( -21.48921356237309155, -27.52281430457070499, 5.000000000000000000 ) ) ;
#37202 = FACE_OUTER_BOUND ( 'NONE', #47631, .T. ) ;
#37203 = VERTEX_POINT ( 'NONE', #87169 ) ;
#37204 = VECTOR ( 'NONE', #114610, 1000.000000000000000 ) ;
#37205 = AXIS2_PLACEMENT_3D ( 'NONE', #510, #131774, #76700 ) ;
#37206 = STYLED_ITEM ( 'NONE', ( #31722 ), #64289 ) ;
#37207 = ORIENTED_EDGE ( 'NONE', *, *, #101118, .T. ) ;
#37208 = AXIS2_PLACEMENT_3D ( 'NONE', #56205, #5897, #105247 ) ;
#37209 = DIRECTION ( 'NONE',  ( -0.6830127018922180770, -0.6830127018922204085, -0.2588190451025213501 ) ) ;
#37210 = CARTESIAN_POINT ( 'NONE',  ( 5.999999999999960032, 10.55218569542906160, 5.000000000000000000 ) ) ;
#37211 = ORIENTED_EDGE ( 'NONE', *, *, #121943, .F. ) ;
#37212 = ORIENTED_EDGE ( 'NONE', *, *, #44357, .T. ) ;
#37213 = EDGE_LOOP ( 'NONE', ( #51935, #25685, #24876, #99439 ) ) ;
#37214 = CARTESIAN_POINT ( 'NONE',  ( 11.99999999999991651, -16.06887692260765377, 4.000000000000000000 ) ) ;
#37215 = ORIENTED_EDGE ( 'NONE', *, *, #115762, .T. ) ;
#37216 = VECTOR ( 'NONE', #83136, 1000.000000000000000 ) ;
#37217 = CARTESIAN_POINT ( 'NONE',  ( -2.206660635421508143, 21.75929247661549937, 4.998822639870708073 ) ) ;
#37218 = CARTESIAN_POINT ( 'NONE',  ( 42.22502705046289861, 5.819803920172573974, -5.819803920172573086 ) ) ;
#37219 = CARTESIAN_POINT ( 'NONE',  ( 6.192069808101887674, -7.934999999999991616, -2.126176841940955242 ) ) ;
#37220 = DIRECTION ( 'NONE',  ( 0.7071067811865487940, 0.7071067811865463515, 0.000000000000000000 ) ) ;
#37221 = VERTEX_POINT ( 'NONE', #131395 ) ;
#37222 = VECTOR ( 'NONE', #43586, 1000.000000000000000 ) ;
#37223 = DIRECTION ( 'NONE',  ( 0.7071067811865487940, -0.7071067811865463515, 0.000000000000000000 ) ) ;
#37225 = EDGE_CURVE ( 'NONE', #95580, #58969, #32076, .T. ) ;
#37224 = LINE ( 'NONE', #113337, #85950 ) ;
#37226 = EDGE_CURVE ( 'NONE', #78422, #86060, #98742, .T. ) ;
#37227 = AXIS2_PLACEMENT_3D ( 'NONE', #109836, #85941, #73646 ) ;
#37228 = LINE ( 'NONE', #115456, #8126 ) ;
#37230 = VERTEX_POINT ( 'NONE', #142969 ) ;
#37229 = DIRECTION ( 'NONE',  ( 0.000000000000000000, 1.000000000000000000, 0.000000000000000000 ) ) ;
#37231 = ORIENTED_EDGE ( 'NONE', *, *, #52803, .F. ) ;
#37232 = DIRECTION ( 'NONE',  ( 0.7071067811865487940, 0.7071067811865463515, 0.000000000000000000 ) ) ;
#37233 = CARTESIAN_POINT ( 'NONE',  ( -20.52663903635772513, -5.240707523384225297, 16.25846745537490889 ) ) ;
#37234 = PLANE ( 'NONE',  #135062 ) ;
#37235 = ORIENTED_EDGE ( 'NONE', *, *, #102896, .F. ) ;
#37236 = AXIS2_PLACEMENT_3D ( 'NONE', #46302, #3441, #91897 ) ;
#37237 = CARTESIAN_POINT ( 'NONE',  ( -1.019877749285469370, -17.24070752338410273, 20.23474786156469207 ) ) ;
#37238 = LINE ( 'NONE', #79367, #142823 ) ;
#37239 = CONICAL_SURFACE ( 'NONE', #118240, 2.500000000000000444, 0.9599310885968830309 ) ;
#37241 = LINE ( 'NONE', #37974, #19360 ) ;
#37240 = AXIS2_PLACEMENT_3D ( 'NONE', #55141, #44280, #77620 ) ;
#37242 = LINE ( 'NONE', #116227, #21049 ) ;
#37243 = CARTESIAN_POINT ( 'NONE',  ( 81.29974487139159578, -27.71228299555262709, 4.000000000000000000 ) ) ;
#37244 = ORIENTED_EDGE ( 'NONE', *, *, #28073, .F. ) ;
#37245 = LINE ( 'NONE', #56892, #73976 ) ;
#37246 = VECTOR ( 'NONE', #7292, 1000.000000000000000 ) ;
#37247 = LINE ( 'NONE', #36530, #130380 ) ;
#37248 = CARTESIAN_POINT ( 'NONE',  ( 63.18398860626900415, 28.73617430169831621, 5.000000000000000000 ) ) ;
#37249 = EDGE_CURVE ( 'NONE', #107457, #117579, #43663, .T. ) ;
#37250 = DIRECTION ( 'NONE',  ( -0.000000000000000000, -0.3543493200069152693, 0.9351131265310292928 ) ) ;
#37251 = CARTESIAN_POINT ( 'NONE',  ( 16.30000000000000071, 9.521314400968980422E-16, 0.000000000000000000 ) ) ;
#37252 = EDGE_CURVE ( 'NONE', #18669, #136089, #4188, .T. ) ;
#37253 = ORIENTED_EDGE ( 'NONE', *, *, #69640, .F. ) ;
#37254 = AXIS2_PLACEMENT_3D ( 'NONE', #83654, #28543, #72801 ) ;
#37255 = ORIENTED_EDGE ( 'NONE', *, *, #24623, .F. ) ;
#37256 = CARTESIAN_POINT ( 'NONE',  ( -34.92500000000001137, -15.18334561358941315, 4.500000000000000888 ) ) ;
#37257 = PRESENTATION_STYLE_ASSIGNMENT (( #92322 ) ) ;
#37258 = EDGE_CURVE ( 'NONE', #73784, #82859, #113009, .T. ) ;
#37259 = ADVANCED_FACE ( 'NONE', ( #69551 ), #60830, .F. ) ;
#37260 = CARTESIAN_POINT ( 'NONE',  ( 7.416236474768552966, -7.934999999999990727, 4.858786175617117713E-16 ) ) ;
#37261 = CARTESIAN_POINT ( 'NONE',  ( 65.99586038379622721, -3.974999999999998312, -6.884901960086286188 ) ) ;
#37262 = AXIS2_PLACEMENT_3D ( 'NONE', #47732, #4843, #49855 ) ;
#37263 = DIRECTION ( 'NONE',  ( 0.7071067811865486830, -0.7071067811865464625, -0.000000000000000000 ) ) ;
#37264 = CARTESIAN_POINT ( 'NONE',  ( 20.99999999999985079, 10.93112307739207267, 4.000000000000000000 ) ) ;
#37265 = CARTESIAN_POINT ( 'NONE',  ( -9.643187427517323940, -20.24070752338407075, 21.22881796311210323 ) ) ;
#37266 = ORIENTED_EDGE ( 'NONE', *, *, #112583, .T. ) ;
#37267 = EDGE_CURVE ( 'NONE', #56327, #137982, #70289, .T. ) ;
#37268 = DIRECTION ( 'NONE',  ( 0.7071067811865486830, -0.7071067811865464625, -0.000000000000000000 ) ) ;
#37269 = VECTOR ( 'NONE', #56433, 1000.000000000000227 ) ;
#37270 = CARTESIAN_POINT ( 'NONE',  ( 11.67183060077639389, -21.74070752338406365, 4.000000000000000000 ) ) ;
#37271 = VECTOR ( 'NONE', #91983, 1000.000000000000000 ) ;
#37272 = PLANE ( 'NONE',  #50530 ) ;
#37273 = CARTESIAN_POINT ( 'NONE',  ( 46.28709685856477307, 3.054999999999997939, 5.291415217122920289 ) ) ;
#37274 = CARTESIAN_POINT ( 'NONE',  ( -0.7816268829249449768, 21.74787736706806029, 4.999607392498049308 ) ) ;
#37275 = ADVANCED_FACE ( 'NONE', ( #126729 ), #70967, .F. ) ;
#37276 = ORIENTED_EDGE ( 'NONE', *, *, #13043, .T. ) ;
#37277 = DIRECTION ( 'NONE',  ( -0.6830127018922180770, -0.6830127018922204085, -0.2588190451025213501 ) ) ;
#37278 = EDGE_LOOP ( 'NONE', ( #49187, #63202, #31434, #82938 ) ) ;
#37279 = LINE ( 'NONE', #96426, #113695 ) ;
#37280 = ORIENTED_EDGE ( 'NONE', *, *, #31247, .F. ) ;
#37281 = AXIS2_PLACEMENT_3D ( 'NONE', #46188, #137454, #91110 ) ;
#37282 = LINE ( 'NONE', #79409, #61738 ) ;
#37283 = EDGE_CURVE ( 'NONE', #71611, #91617, #92677, .T. ) ;
#37284 = CARTESIAN_POINT ( 'NONE',  ( 33.79289321881321939, -20.24070752338407786, 5.000000000000000000 ) ) ;
#37285 = CARTESIAN_POINT ( 'NONE',  ( -36.29974487139159578, -27.71228299555231445, 4.000000000000000000 ) ) ;
#37286 = DIRECTION ( 'NONE',  ( 0.3543493200069162685, -0.000000000000000000, -0.9351131265310288487 ) ) ;
#37287 = CARTESIAN_POINT ( 'NONE',  ( 23.99999999999984368, 14.58746187583909837, 4.000000000000000000 ) ) ;
#37288 = CARTESIAN_POINT ( 'NONE',  ( 131.6371832251699914, -49.11905619111313115, 40.21880474160069241 ) ) ;
#37289 = ORIENTED_EDGE ( 'NONE', *, *, #58843, .F. ) ;
#37290 = FACE_OUTER_BOUND ( 'NONE', #26842, .T. ) ;
#37291 = UNCERTAINTY_MEASURE_WITH_UNIT (LENGTH_MEASURE( 1.000000000000000082E-05 ), #132329, 'distance_accuracy_value', 'NONE');
#37292 = EDGE_CURVE ( 'NONE', #56990, #82053, #104991, .T. ) ;
#37293 = VECTOR ( 'NONE', #8709, 1000.000000000000000 ) ;
#37294 = CARTESIAN_POINT ( 'NONE',  ( -34.92500000000001137, 22.22500000000000142, 4.000000000000000000 ) ) ;
#37295 = CARTESIAN_POINT ( 'NONE',  ( 118.1041666666666430, 2.130196079827479050, 7.949999999999969091 ) ) ;
#37296 = CARTESIAN_POINT ( 'NONE',  ( 79.85002705046289861, -5.819803920172572198, -5.819803920172572198 ) ) ;
#37297 = LINE ( 'NONE', #125749, #78542 ) ;
#37298 = VERTEX_POINT ( 'NONE', #49928 ) ;
#37299 = ORIENTED_EDGE ( 'NONE', *, *, #553, .T. ) ;
#37300 = CARTESIAN_POINT ( 'NONE',  ( 65.31250000000000000, 5.819803920172571310, 5.819803920172575751 ) ) ;
#37301 = DIRECTION ( 'NONE',  ( 0.7071067811865487940, -0.7071067811865463515, 0.000000000000000000 ) ) ;
#37302 = CARTESIAN_POINT ( 'NONE',  ( 30.48921356237309510, -27.52281430457076894, 5.000000000000000000 ) ) ;
#37303 = LINE ( 'NONE', #5357, #96003 ) ;
#37304 = EDGE_CURVE ( 'NONE', #43201, #94183, #115122, .T. ) ;
#37305 = ORIENTED_EDGE ( 'NONE', *, *, #8588, .T. ) ;
#37306 =( BOUNDED_CURVE ( )  B_SPLINE_CURVE ( 3, ( #123660, #122920, #57692, #101870 ),
 .UNSPECIFIED., .F., .F. ) 
 B_SPLINE_CURVE_WITH_KNOTS ( ( 4, 4 ),
 ( 1.208578181583237932, 1.359146454359414724 ),
 .UNSPECIFIED. ) 
 CURVE ( )  GEOMETRIC_REPRESENTATION_ITEM ( )  RATIONAL_B_SPLINE_CURVE ( ( 1.000000000000000000, 0.9981116584018959736, 0.9981116584018959736, 1.000000000000000000 ) ) 
 REPRESENTATION_ITEM ( '' )  );
#37307 = CARTESIAN_POINT ( 'NONE',  ( -12.70701326429296252, -21.74070752338406010, 4.999753212805220670 ) ) ;
#37309 = EDGE_CURVE ( 'NONE', #75424, #113572, #94107, .T. ) ;
#37308 = VECTOR ( 'NONE', #48252, 1000.000000000000000 ) ;
#37310 = VECTOR ( 'NONE', #89068, 1000.000000000000000 ) ;
#37311 = CARTESIAN_POINT ( 'NONE',  ( 39.29974487139159578, -27.71228299555233576, 4.000000000000000000 ) ) ;
#37312 = CARTESIAN_POINT ( 'NONE',  ( 54.39626352523144703, 4.472830434245840259, -4.472830434245839371 ) ) ;
#37313 = EDGE_CURVE ( 'NONE', #42725, #101750, #113738, .T. ) ;
#37314 = DIRECTION ( 'NONE',  ( -0.7071067811865486830, -0.7071067811865464625, 0.000000000000000000 ) ) ;
#37315 = VERTEX_POINT ( 'NONE', #25287 ) ;
#37317 = ORIENTED_EDGE ( 'NONE', *, *, #102549, .F. ) ;
#37316 = AXIS2_PLACEMENT_3D ( 'NONE', #102170, #81134, #49227 ) ;
#37318 = VECTOR ( 'NONE', #54768, 1000.000000000000000 ) ;
#37319 = VECTOR ( 'NONE', #52234, 1000.000000000000000 ) ;
#37320 = AXIS2_PLACEMENT_3D ( 'NONE', #26800, #82615, #115193 ) ;
#37321 = DIRECTION ( 'NONE',  ( -0.7071067811865487940, 0.7071067811865463515, 0.000000000000000000 ) ) ;
#37322 = EDGE_CURVE ( 'NONE', #16237, #24858, #15111, .T. ) ;
#37324 = DIRECTION ( 'NONE',  ( -1.000000000000000000, -1.224606353822377258E-16, -0.000000000000000000 ) ) ;
#37323 = AXIS2_PLACEMENT_3D ( 'NONE', #94446, #16903, #129213 ) ;
#37325 = CARTESIAN_POINT ( 'NONE',  ( 32.99999999999977263, -21.84840872380821608, 2.849755605029683281 ) ) ;
#37326 = DIRECTION ( 'NONE',  ( -0.7071067811865486830, 0.7071067811865464625, 0.000000000000000000 ) ) ;
#37327 = CARTESIAN_POINT ( 'NONE',  ( -30.18398860626900060, 28.73617430169808173, 5.000000000000000000 ) ) ;
#37329 = VERTEX_POINT ( 'NONE', #15793 ) ;
#37328 = CARTESIAN_POINT ( 'NONE',  ( 8.161706124526148187, -6.740707523384205757, 16.75550250614869086 ) ) ;
#37330 = DIRECTION ( 'NONE',  ( -0.000000000000000000, 0.3543493200069153248, 0.9351131265310292928 ) ) ;
#37331 = DIRECTION ( 'NONE',  ( 0.3543493200069162685, -0.000000000000000000, -0.9351131265310288487 ) ) ;
#37332 = CARTESIAN_POINT ( 'NONE',  ( -25.39999999999996305, 3.061616997868383141E-16, -2.500000000000000000 ) ) ;
#37333 = AXIS2_PLACEMENT_3D ( 'NONE', #67848, #112034, #71379 ) ;
#37334 = FACE_OUTER_BOUND ( 'NONE', #12220, .T. ) ;
#37335 = ORIENTED_EDGE ( 'NONE', *, *, #111004, .T. ) ;
#37336 = ORIENTED_EDGE ( 'NONE', *, *, #35430, .F. ) ;
#37338 = ADVANCED_FACE ( 'NONE', ( #102168 ), #59391, .F. ) ;
#37337 = VECTOR ( 'NONE', #129694, 1000.000000000000000 ) ;
#37339 = CYLINDRICAL_SURFACE ( 'NONE', #73051, 0.5000000000000004441 ) ;
#37340 = CARTESIAN_POINT ( 'NONE',  ( -11.99999999999992006, -22.06887692260758982, 4.000000000000000000 ) ) ;
#37341 = DIRECTION ( 'NONE',  ( -0.7071067811865487940, 0.7071067811865463515, -0.000000000000000000 ) ) ;
#37342 = DIRECTION ( 'NONE',  ( 0.7071067811865487940, -0.7071067811865463515, 0.000000000000000000 ) ) ;
#37343 = ORIENTED_EDGE ( 'NONE', *, *, #29800, .T. ) ;
#37344 = ORIENTED_EDGE ( 'NONE', *, *, #4713, .T. ) ;
#37345 = DIRECTION ( 'NONE',  ( 1.000000000000000000, 0.000000000000000000, 0.000000000000000000 ) ) ;
#37347 = EDGE_CURVE ( 'NONE', #34296, #47990, #38326, .T. ) ;
#37346 = FACE_OUTER_BOUND ( 'NONE', #49973, .T. ) ;
#37348 = VECTOR ( 'NONE', #12555, 1000.000000000000000 ) ;
#37349 = ORIENTED_EDGE ( 'NONE', *, *, #13743, .T. ) ;
#37350 = VECTOR ( 'NONE', #10731, 1000.000000000000000 ) ;
#37351 = DIRECTION ( 'NONE',  ( -0.7071067811865486830, 0.7071067811865464625, 0.000000000000000000 ) ) ;
#37352 = ORIENTED_EDGE ( 'NONE', *, *, #63525, .T. ) ;
#37353 = AXIS2_PLACEMENT_3D ( 'NONE', #30244, #74496, #107786 ) ;
#37354 = LINE ( 'NONE', #26470, #89584 ) ;
#37355 = LINE ( 'NONE', #125058, #3004 ) ;
#37356 = CIRCLE ( 'NONE', #132381, 2.500000000000000444 ) ;
#37357 = FACE_BOUND ( 'NONE', #20405, .T. ) ;
#37358 = VECTOR ( 'NONE', #34083, 1000.000000000000227 ) ;
#37359 = DIRECTION ( 'NONE',  ( -0.6830127018922181881, 0.6830127018922202975, -0.2588190451025214056 ) ) ;
#37360 = DIRECTION ( 'NONE',  ( -1.000000000000000000, 0.000000000000000000, -0.000000000000000000 ) ) ;
#37361 = DIRECTION ( 'NONE',  ( -1.000000000000000000, -0.000000000000000000, -0.000000000000000000 ) ) ;
#37362 = CARTESIAN_POINT ( 'NONE',  ( -31.49999999999977973, 1.466399257802248446, 5.000000000000000000 ) ) ;
#37363 = PRODUCT_CONTEXT ( 'NONE', #67989, 'mechanical' ) ;
#37364 = EDGE_LOOP ( 'NONE', ( #105220, #31047, #1079, #95387 ) ) ;
#37365 = EDGE_CURVE ( 'NONE', #46917, #56980, #115837, .T. ) ;
#37366 = VECTOR ( 'NONE', #32843, 1000.000000000000227 ) ;
#37367 = ORIENTED_EDGE ( 'NONE', *, *, #52673, .T. ) ;
#37368 = CARTESIAN_POINT ( 'NONE',  ( 89.89126352523143737, -4.472830434245838482, -4.472830434245838482 ) ) ;
#37369 = ORIENTED_EDGE ( 'NONE', *, *, #138625, .F. ) ;
#37370 = DIRECTION ( 'NONE',  ( -0.7071067811865486830, 0.7071067811865464625, 0.000000000000000000 ) ) ;
#37371 = VECTOR ( 'NONE', #73355, 1000.000000000000000 ) ;
#37372 = CARTESIAN_POINT ( 'NONE',  ( -59.99451991528749772, 28.92564299267980132, 4.000000000000000000 ) ) ;
#37373 = AXIS2_PLACEMENT_3D ( 'NONE', #96940, #75260, #50628 ) ;
#37374 = LINE ( 'NONE', #73573, #117378 ) ;
#37375 = LINE ( 'NONE', #72184, #105010 ) ;
#37376 = ORIENTED_EDGE ( 'NONE', *, *, #89962, .F. ) ;
#37377 = DIRECTION ( 'NONE',  ( 0.000000000000000000, 0.000000000000000000, -1.000000000000000000 ) ) ;
#37378 = DIRECTION ( 'NONE',  ( 3.115803279706882722E-16, -1.000000000000000000, -1.016133275908817741E-16 ) ) ;
#37379 = DIRECTION ( 'NONE',  ( -0.6830127018922180770, -0.6830127018922204085, -0.2588190451025213501 ) ) ;
#37381 = DIRECTION ( 'NONE',  ( -0.3543493200069162685, -0.000000000000000000, -0.9351131265310288487 ) ) ;
#37380 = CARTESIAN_POINT ( 'NONE',  ( 1.734723475976807094E-15, 2.966399257802227130, 5.000000000000000000 ) ) ;
#37382 = CARTESIAN_POINT ( 'NONE',  ( -12.20000000000000284, -25.33999999999998209, 15.47043909406156104 ) ) ;
#37383 = AXIS2_PLACEMENT_3D ( 'NONE', #109462, #134081, #23130 ) ;
#37384 = CARTESIAN_POINT ( 'NONE',  ( 29.68342038867192656, -6.740707523384212863, 11.88629033278117575 ) ) ;
#37385 = ORIENTED_EDGE ( 'NONE', *, *, #122350, .T. ) ;
#37386 = DIRECTION ( 'NONE',  ( -0.000000000000000000, -0.3543493200069152693, 0.9351131265310292928 ) ) ;
#37387 = CARTESIAN_POINT ( 'NONE',  ( 22.17183060077631751, -2.240707523384257716, 4.000000000000000000 ) ) ;
#37388 = VERTEX_POINT ( 'NONE', #125337 ) ;
#37389 = EDGE_LOOP ( 'NONE', ( #117903, #122809, #40661, #10884 ) ) ;
#37390 = VERTEX_POINT ( 'NONE', #66854 ) ;
#37391 = CARTESIAN_POINT ( 'NONE',  ( 42.00043019189809712, -3.055000000000002380, 5.291415217122920289 ) ) ;
#37392 = CIRCLE ( 'NONE', #11910, 1.249999999999971578 ) ;
#37393 = VERTEX_POINT ( 'NONE', #103548 ) ;
#37394 = CARTESIAN_POINT ( 'NONE',  ( 6.608306282870438864, 1.633150327867687324, -6.094999999999991758 ) ) ;
#37395 = CARTESIAN_POINT ( 'NONE',  ( -16.67979525387081807, 0.3337821591035541879, -30.81818940114110816 ) ) ;
#37396 = ORIENTED_EDGE ( 'NONE', *, *, #24835, .T. ) ;
#37397 = LINE ( 'NONE', #123717, #135888 ) ;
#37398 = ORIENTED_EDGE ( 'NONE', *, *, #36378, .F. ) ;
#37399 = CARTESIAN_POINT ( 'NONE',  ( -6.005480084712508493, 28.92564299267933947, 4.000000000000000000 ) ) ;
#37400 = CARTESIAN_POINT ( 'NONE',  ( -34.92500000000001137, -22.22500000000000142, 4.500000000000000888 ) ) ;
#37401 = VECTOR ( 'NONE', #55620, 1000.000000000000000 ) ;
#37403 = ORIENTED_EDGE ( 'NONE', *, *, #84518, .F. ) ;
#37402 = LINE ( 'NONE', #80222, #766 ) ;
#37404 = ORIENTED_EDGE ( 'NONE', *, *, #12373, .F. ) ;
#37405 = DIRECTION ( 'NONE',  ( 0.000000000000000000, 0.000000000000000000, 1.000000000000000000 ) ) ;
#37406 = CARTESIAN_POINT ( 'NONE',  ( 38.16170612452596345, -6.740707523384209310, 16.75550250614876546 ) ) ;
#37407 = VECTOR ( 'NONE', #35818, 1000.000000000000000 ) ;
#37409 = VERTEX_POINT ( 'NONE', #48476 ) ;
#37408 = VECTOR ( 'NONE', #45406, 1000.000000000000000 ) ;
#37410 = CARTESIAN_POINT ( 'NONE',  ( -36.18398860626899705, 28.73617430169812437, 5.000000000000000000 ) ) ;
#37411 = VERTEX_POINT ( 'NONE', #13679 ) ;
#37412 = EDGE_LOOP ( 'NONE', ( #70072, #99344, #131097, #29380 ) ) ;
#37413 = EDGE_LOOP ( 'NONE', ( #49343, #31559, #21832, #21498 ) ) ;
#37414 = ORIENTED_EDGE ( 'NONE', *, *, #803, .F. ) ;
#37415 = ADVANCED_FACE ( 'NONE', ( #57971 ), #47118, .F. ) ;
#37416 = CARTESIAN_POINT ( 'NONE',  ( -6.349999999999999645, 0.000000000000000000, 1.249999999999970690 ) ) ;
#37417 = VECTOR ( 'NONE', #85939, 999.9999999999998863 ) ;
#37418 =( GEOMETRIC_REPRESENTATION_CONTEXT ( 3 ) GLOBAL_UNCERTAINTY_ASSIGNED_CONTEXT ( ( #15625 ) ) GLOBAL_UNIT_ASSIGNED_CONTEXT ( ( #51391, #140512, #94853 ) ) REPRESENTATION_CONTEXT ( 'NONE', 'WORKASPACE' ) );
#37419 = AXIS2_PLACEMENT_3D ( 'NONE', #121591, #45510, #13531 ) ;
#37420 = CIRCLE ( 'NONE', #72235, 2.999999999999999112 ) ;
#37421 = COLOUR_RGB ( '', 0.40784314, 0.44705882, 0.49803922) ;
#37422 = FILL_AREA_STYLE ('',( #104063 ) ) ;
#37423 = CARTESIAN_POINT ( 'NONE',  ( 22.17183060077631396, 9.759292476615614831, 4.000000000000000000 ) ) ;
#37424 = DIRECTION ( 'NONE',  ( -0.3543493200069162685, -0.000000000000000000, -0.9351131265310288487 ) ) ;
#37425 = EDGE_CURVE ( 'NONE', #80458, #33564, #3514, .T. ) ;
#37426 = EDGE_CURVE ( 'NONE', #108226, #62844, #117972, .T. ) ;
#37427 = CARTESIAN_POINT ( 'NONE',  ( 27.32816939922333432, 2.259292476615690770, 4.000000000000000000 ) ) ;
#37429 = ORIENTED_EDGE ( 'NONE', *, *, #71520, .F. ) ;
#37428 = COLOUR_RGB ( '', 0.66274510, 0.83137255, 0.94901961) ;
#37430 = FILL_AREA_STYLE_COLOUR ( '', #40185 ) ;
#37431 = ADVANCED_FACE ( 'NONE', ( #41895 ), #28161, .F. ) ;
#37432 = ADVANCED_FACE ( 'NONE', ( #39030 ), #106382, .T. ) ;
#37433 = CARTESIAN_POINT ( 'NONE',  ( 21.70790314143522082, -6.871911579029513106, -3.967499999999993587 ) ) ;
#37434 = DIRECTION ( 'NONE',  ( 0.000000000000000000, -1.000000000000000000, 0.000000000000000000 ) ) ;
#37435 = EDGE_CURVE ( 'NONE', #73261, #114456, #140472, .T. ) ;
#37436 = DIRECTION ( 'NONE',  ( 0.000000000000000000, -1.000000000000000000, 0.000000000000000000 ) ) ;
#37437 = CARTESIAN_POINT ( 'NONE',  ( -5.282422613574296655, -21.73023691814493930, 5.000000000000000888 ) ) ;
#37438 = VERTEX_POINT ( 'NONE', #130338 ) ;
#37439 = ORIENTED_EDGE ( 'NONE', *, *, #18103, .T. ) ;
#37440 = EDGE_CURVE ( 'NONE', #49004, #9326, #51349, .T. ) ;
#37441 = ORIENTED_EDGE ( 'NONE', *, *, #98917, .T. ) ;
#37442 = LINE ( 'NONE', #70110, #74201 ) ;
#37443 = CARTESIAN_POINT ( 'NONE',  ( 23.51078643762690490, -27.52281430457038880, 5.000000000000000000 ) ) ;
#37444 = UNCERTAINTY_MEASURE_WITH_UNIT (LENGTH_MEASURE( 1.000000000000000082E-05 ), #33711, 'distance_accuracy_value', 'NONE');
#37445 = CARTESIAN_POINT ( 'NONE',  ( -22.49999999999984723, 18.43112307739199807, 4.000000000000000000 ) ) ;
#37446 = ADVANCED_FACE ( 'NONE', ( #107827 ), #52742, .F. ) ;
#37447 = CARTESIAN_POINT ( 'NONE',  ( -24.48921356237309510, -27.52281430457072631, 5.000000000000000000 ) ) ;
#37448 = CARTESIAN_POINT ( 'NONE',  ( 34.49999999999975131, 11.52377502935406106, -1.522421517564165550 ) ) ;
#37449 = CARTESIAN_POINT ( 'NONE',  ( 77.49543019189810877, 5.291415217122917625, 3.055000000000002380 ) ) ;
#37450 = AXIS2_PLACEMENT_3D ( 'NONE', #47226, #91402, #104380 ) ;
#37451 = CARTESIAN_POINT ( 'NONE',  ( -69.48921356237309510, -27.52281430457103895, 5.000000000000000000 ) ) ;
#37452 = ADVANCED_FACE ( 'NONE', ( #129588 ), #53480, .T. ) ;
#37453 = VECTOR ( 'NONE', #74262, 1000.000000000000227 ) ;
#37454 = CARTESIAN_POINT ( 'NONE',  ( 11.99999999999992006, 9.631307414974342507, -9.079085613539515265 ) ) ;
#37455 = FACE_OUTER_BOUND ( 'NONE', #123234, .T. ) ;
#37456 = CARTESIAN_POINT ( 'NONE',  ( -15.32816939922342137, 20.25929247661551358, 4.000000000000000000 ) ) ;
#37457 = PRESENTATION_LAYER_ASSIGNMENT (  '', '', ( #90660 ) ) ;
#37458 = DIRECTION ( 'NONE',  ( 0.3543493200069162685, -0.000000000000000000, -0.9351131265310288487 ) ) ;
#37459 = ORIENTED_EDGE ( 'NONE', *, *, #102660, .F. ) ;
#37461 = AXIS2_PLACEMENT_3D ( 'NONE', #126276, #26953, #27661 ) ;
#37460 = DIRECTION ( 'NONE',  ( -0.7071067811865486830, 0.7071067811865464625, 0.000000000000000000 ) ) ;
#37462 = ORIENTED_EDGE ( 'NONE', *, *, #111628, .F. ) ;
#37463 = EDGE_CURVE ( 'NONE', #35947, #116804, #6346, .T. ) ;
#37464 = LINE ( 'NONE', #124452, #29783 ) ;
#37466 = ORIENTED_EDGE ( 'NONE', *, *, #11749, .F. ) ;
#37465 = CARTESIAN_POINT ( 'NONE',  ( -34.45011844616455221, 15.00230414159380565, 5.000000000000000888 ) ) ;
#37467 = DIRECTION ( 'NONE',  ( -0.6830127018922181881, 0.6830127018922202975, -0.2588190451025214056 ) ) ;
#37468 = DIRECTION ( 'NONE',  ( 0.7071067811865487940, 0.7071067811865463515, 0.000000000000000000 ) ) ;
#37469 =( REPRESENTATION_RELATIONSHIP ('NONE','NONE', #69070, #103311 ) REPRESENTATION_RELATIONSHIP_WITH_TRANSFORMATION ( #31484 )SHAPE_REPRESENTATION_RELATIONSHIP( ) );
#37470 = ORIENTED_EDGE ( 'NONE', *, *, #54539, .T. ) ;
#37471 = FACE_OUTER_BOUND ( 'NONE', #137672, .T. ) ;
#37472 = ORIENTED_EDGE ( 'NONE', *, *, #111550, .T. ) ;
#37473 = CARTESIAN_POINT ( 'NONE',  ( 122.2875270504628844, 0.000000000000000000, -7.949999999999998401 ) ) ;
#37474 = ORIENTED_EDGE ( 'NONE', *, *, #142324, .T. ) ;
#37475 = ADVANCED_FACE ( 'NONE', ( #7067 ), #97687, .F. ) ;
#37476 = VECTOR ( 'NONE', #62706, 1000.000000000000227 ) ;
#37477 = CARTESIAN_POINT ( 'NONE',  ( 39.29974487139159578, -27.71228299555233576, 4.000000000000000000 ) ) ;
#37478 = CARTESIAN_POINT ( 'NONE',  ( 99.39169371712955581, 2.130196079827421762, 7.950000000000001066 ) ) ;
#37479 = DIRECTION ( 'NONE',  ( -0.7071067811865486830, -0.7071067811865464625, -0.000000000000000000 ) ) ;
#37480 = DIRECTION ( 'NONE',  ( 0.000000000000000000, 0.000000000000000000, -1.000000000000000000 ) ) ;
#37481 = ORIENTED_EDGE ( 'NONE', *, *, #105231, .T. ) ;
#37482 = CARTESIAN_POINT ( 'NONE',  ( -12.18398860626900060, 28.73617430169795739, 5.000000000000000000 ) ) ;
#37483 = CARTESIAN_POINT ( 'NONE',  ( -28.17183060077627133, 15.75929247661555976, 4.000000000000000000 ) ) ;
#37484 = DIRECTION ( 'NONE',  ( -0.000000000000000000, -0.3543493200069152693, 0.9351131265310292928 ) ) ;
#37486 = VECTOR ( 'NONE', #11434, 1000.000000000000000 ) ;
#37485 = CARTESIAN_POINT ( 'NONE',  ( 23.77083333333333925, 6.094999999999991758, 1.633150327867687102 ) ) ;
#37487 = DIRECTION ( 'NONE',  ( 1.000000000000000000, 1.224606353822377258E-16, 0.000000000000000000 ) ) ;
#37489 = AXIS2_PLACEMENT_3D ( 'NONE', #5855, #116786, #37827 ) ;
#37488 = DIRECTION ( 'NONE',  ( 0.6830127018922180770, -0.6830127018922204085, -0.2588190451025213501 ) ) ;
#37490 = ORIENTED_EDGE ( 'NONE', *, *, #51785, .T. ) ;
#37491 = CARTESIAN_POINT ( 'NONE',  ( -27.48921356237309155, -27.52281430457074762, 5.000000000000000000 ) ) ;
#37492 = EDGE_CURVE ( 'NONE', #56823, #3030, #117691, .T. ) ;
#37493 = EDGE_LOOP ( 'NONE', ( #33483, #93890, #86813, #128708 ) ) ;
#37494 = CARTESIAN_POINT ( 'NONE',  ( 80.93793019189807580, -6.110000000000001208, 1.637169565754158951 ) ) ;
#37495 = ADVANCED_FACE ( 'NONE', ( #74537 ), #116589, .T. ) ;
#37496 = DIRECTION ( 'NONE',  ( -0.6830127018922181881, 0.6830127018922202975, -0.2588190451025214056 ) ) ;
#37497 = CARTESIAN_POINT ( 'NONE',  ( 51.48921356237309510, -27.52281430457091460, 5.000000000000000000 ) ) ;
#37499 = CIRCLE ( 'NONE', #95316, 2.500000000000000444 ) ;
#37498 = CARTESIAN_POINT ( 'NONE',  ( 9.707106781186482181, 14.25929247661557220, 5.000000000000000000 ) ) ;
#37500 = CARTESIAN_POINT ( 'NONE',  ( 21.76000000000000156, -2.055000000000000160, 2.789133085058098087E-16 ) ) ;
#37501 = ORIENTED_EDGE ( 'NONE', *, *, #121273, .F. ) ;
#37502 = CARTESIAN_POINT ( 'NONE',  ( 22.49999999999984723, 18.43112307739199807, 4.000000000000000000 ) ) ;
#37503 = ADVANCED_FACE ( 'NONE', ( #128199 ), #7804, .F. ) ;
#37504 = ADVANCED_FACE ( 'NONE', ( #64354 ), #127460, .F. ) ;
#37505 = DIRECTION ( 'NONE',  ( -0.000000000000000000, 0.000000000000000000, 1.000000000000000000 ) ) ;
#37506 = VERTEX_POINT ( 'NONE', #84001 ) ;
#37507 = LINE ( 'NONE', #12153, #48521 ) ;
#37508 = FACE_OUTER_BOUND ( 'NONE', #1614, .T. ) ;
#37510 = ORIENTED_EDGE ( 'NONE', *, *, #26144, .F. ) ;
#37509 = LINE ( 'NONE', #59281, #82251 ) ;
#37511 = CARTESIAN_POINT ( 'NONE',  ( 7.785015802758053383, -3.740707523384244837, 15.76143240460126194 ) ) ;
#37512 = CARTESIAN_POINT ( 'NONE',  ( 16.75173015016484968, 4.202752102959690472E-16, 0.000000000000000000 ) ) ;
#37513 = AXIS2_PLACEMENT_3D ( 'NONE', #89018, #33914, #46236 ) ;
#37514 = CARTESIAN_POINT ( 'NONE',  ( 4.001930566820951718, -22.22500000000000142, 4.500000000000000888 ) ) ;
#37515 = FILL_AREA_STYLE ('',( #49109 ) ) ;
#37516 = VERTEX_POINT ( 'NONE', #139068 ) ;
#37517 = VERTEX_POINT ( 'NONE', #73113 ) ;
#37518 = ORIENTED_EDGE ( 'NONE', *, *, #17918, .F. ) ;
#37519 = CARTESIAN_POINT ( 'NONE',  ( 84.58376352523144703, -6.110000000000001208, -3.741295971395164515E-16 ) ) ;
#37520 = VERTEX_POINT ( 'NONE', #62227 ) ;
#37521 = EDGE_CURVE ( 'NONE', #44877, #5945, #84679, .T. ) ;
#37522 = DIRECTION ( 'NONE',  ( -0.7071067811865487940, 0.7071067811865463515, 0.000000000000000000 ) ) ;
#37523 = DIRECTION ( 'NONE',  ( -0.7071067811865487940, 0.7071067811865463515, 0.000000000000000000 ) ) ;
#37524 = CARTESIAN_POINT ( 'NONE',  ( -20.99451991528748707, 28.92564299267952777, 4.000000000000000000 ) ) ;
#37525 = ORIENTED_EDGE ( 'NONE', *, *, #24609, .T. ) ;
#37526 = CONICAL_SURFACE ( 'NONE', #56065, 4.487534009422227577, 0.08726646259971666819 ) ;
#37527 = DIRECTION ( 'NONE',  ( -1.000000000000000000, -1.224606353822377258E-16, -0.000000000000000000 ) ) ;
#37528 = CARTESIAN_POINT ( 'NONE',  ( -57.18398860626899705, 28.73617430169827358, 5.000000000000000000 ) ) ;
#37529 = VECTOR ( 'NONE', #41859, 1000.000000000000000 ) ;
#37530 = AXIS2_PLACEMENT_3D ( 'NONE', #121844, #1488, #2939 ) ;
#37531 = CARTESIAN_POINT ( 'NONE',  ( 73.12043019189812298, 3.055000000000001936, -5.291415217122916737 ) ) ;
#37532 = ORIENTED_EDGE ( 'NONE', *, *, #81670, .F. ) ;
#37533 = CARTESIAN_POINT ( 'NONE',  ( 35.99451991528749772, 28.92564299267963079, 4.000000000000000000 ) ) ;
#37534 = VECTOR ( 'NONE', #28584, 1000.000000000000114 ) ;
#37535 = CARTESIAN_POINT ( 'NONE',  ( -63.18398860626900415, 28.73617430169831621, 5.000000000000000000 ) ) ;
#37536 = EDGE_LOOP ( 'NONE', ( #31424, #42120, #105609, #96693 ) ) ;
#37537 = VERTEX_POINT ( 'NONE', #85372 ) ;
#37538 = EDGE_CURVE ( 'NONE', #40356, #122205, #22243, .T. ) ;
#37539 = CARTESIAN_POINT ( 'NONE',  ( 57.48921356237308800, -27.52281430457095368, 5.000000000000000000 ) ) ;
#37540 = DIRECTION ( 'NONE',  ( -0.7071067811865487940, 0.7071067811865463515, 0.000000000000000000 ) ) ;
#37541 = CARTESIAN_POINT ( 'NONE',  ( 24.18398860626899705, 28.73617430169804265, 5.000000000000000000 ) ) ;
#37542 = DIRECTION ( 'NONE',  ( -1.000000000000000000, -1.224606353822377258E-16, -0.000000000000000000 ) ) ;
#37543 = DIRECTION ( 'NONE',  ( -0.7071067811865487940, 0.7071067811865463515, -0.000000000000000000 ) ) ;
#37544 = FACE_OUTER_BOUND ( 'NONE', #23625, .T. ) ;
#37545 = DIRECTION ( 'NONE',  ( -0.7071067811865486830, -0.7071067811865464625, -0.000000000000000000 ) ) ;
#37546 = ORIENTED_EDGE ( 'NONE', *, *, #56028, .T. ) ;
#37547 = ORIENTED_EDGE ( 'NONE', *, *, #43251, .F. ) ;
#37548 = CARTESIAN_POINT ( 'NONE',  ( -26.99999999999980815, 16.93112307739200872, 4.000000000000000000 ) ) ;
#37549 = VERTEX_POINT ( 'NONE', #141941 ) ;
#37550 = EDGE_CURVE ( 'NONE', #45664, #93680, #44791, .T. ) ;
#37551 = VECTOR ( 'NONE', #101367, 1000.000000000000000 ) ;
#37552 = VECTOR ( 'NONE', #134176, 1000.000000000000000 ) ;
#37554 = ADVANCED_FACE ( 'NONE', ( #32445 ), #22946, .T. ) ;
#37553 = SURFACE_STYLE_FILL_AREA ( #83188 ) ;
#37555 = EDGE_LOOP ( 'NONE', ( #119156, #126368, #92669, #57712 ) ) ;
#37556 = DIRECTION ( 'NONE',  ( -0.7071067811865486830, 0.7071067811865464625, 0.000000000000000000 ) ) ;
#37557 = CARTESIAN_POINT ( 'NONE',  ( -0.4751261278504552710, 14.25929247661557397, 9.797011795316636906 ) ) ;
#37558 = VECTOR ( 'NONE', #47950, 1000.000000000000000 ) ;
#37559 = CARTESIAN_POINT ( 'NONE',  ( -13.10966639810773771, 3.759292476615678336, 4.164048746910666843 ) ) ;
#37560 = AXIS2_PLACEMENT_3D ( 'NONE', #17502, #105920, #62460 ) ;
#37561 = DIRECTION ( 'NONE',  ( 0.7071067811865486830, -0.7071067811865464625, -0.000000000000000000 ) ) ;
#37562 = VERTEX_POINT ( 'NONE', #54229 ) ;
#37563 = PLANE ( 'NONE',  #37858 ) ;
#37564 = LINE ( 'NONE', #115774, #122988 ) ;
#37565 = EDGE_LOOP ( 'NONE', ( #77871, #91436, #57026, #123124 ) ) ;
#37566 = CARTESIAN_POINT ( 'NONE',  ( 2.816011393730999401, 28.73617430169785436, 5.000000000000000000 ) ) ;
#37567 = ORIENTED_EDGE ( 'NONE', *, *, #76291, .F. ) ;
#37568 = ADVANCED_FACE ( 'NONE', ( #12805 ), #65089, .F. ) ;
#37569 = VERTEX_POINT ( 'NONE', #497 ) ;
#37570 = CARTESIAN_POINT ( 'NONE',  ( 26.84387692260740366, -22.22500000000000142, 4.000000000000000000 ) ) ;
#37571 = EDGE_LOOP ( 'NONE', ( #97036, #67605, #110273, #132794 ) ) ;
#37572 = ORIENTED_EDGE ( 'NONE', *, *, #48352, .F. ) ;
#37573 = CARTESIAN_POINT ( 'NONE',  ( 70.58376352523143282, -6.110000000000001208, -3.741295971395164515E-16 ) ) ;
#37574 = VECTOR ( 'NONE', #68270, 1000.000000000000000 ) ;
#37575 = ORIENTED_EDGE ( 'NONE', *, *, #37267, .F. ) ;
#37576 = CARTESIAN_POINT ( 'NONE',  ( 34.92499999999998295, 14.81665438641030264, 4.500000000000000888 ) ) ;
#37577 = CARTESIAN_POINT ( 'NONE',  ( -10.49999999999992006, 18.43112307739199451, 4.000000000000000000 ) ) ;
#37578 = CARTESIAN_POINT ( 'NONE',  ( 107.3337635252314470, 6.110000000000001208, 1.122388791418549305E-15 ) ) ;
#37579 = FACE_OUTER_BOUND ( 'NONE', #16001, .T. ) ;
#37580 = DIRECTION ( 'NONE',  ( 0.3543493200069162685, -0.000000000000000000, -0.9351131265310288487 ) ) ;
#37583 = PLANE ( 'NONE',  #76830 ) ;
#37582 = CARTESIAN_POINT ( 'NONE',  ( 51.18398860626899705, 28.73617430169823095, 5.000000000000000000 ) ) ;
#37581 = VECTOR ( 'NONE', #18572, 1000.000000000000000 ) ;
#37584 = PLANE ( 'NONE',  #125063 ) ;
#37585 = VECTOR ( 'NONE', #4951, 1000.000000000000000 ) ;
#37586 = FACE_OUTER_BOUND ( 'NONE', #17592, .T. ) ;
#37587 = CARTESIAN_POINT ( 'NONE',  ( -28.82816939922332722, 9.759292476615623713, 4.000000000000000000 ) ) ;
#37588 = EDGE_LOOP ( 'NONE', ( #86653, #57128, #25582, #37986 ) ) ;
#37589 = DIRECTION ( 'NONE',  ( -0.6830127018922180770, -0.6830127018922204085, -0.2588190451025213501 ) ) ;
#37590 = DIRECTION ( 'NONE',  ( 0.7071067811865486830, -0.7071067811865464625, -0.000000000000000000 ) ) ;
#37591 = ORIENTED_EDGE ( 'NONE', *, *, #129911, .T. ) ;
#37592 = ORIENTED_EDGE ( 'NONE', *, *, #97667, .T. ) ;
#37593 = VECTOR ( 'NONE', #55820, 1000.000000000000000 ) ;
#37594 = DIRECTION ( 'NONE',  ( 0.7071067811865486830, -0.7071067811865464625, -0.000000000000000000 ) ) ;
#37595 = ORIENTED_EDGE ( 'NONE', *, *, #10993, .T. ) ;
#37596 = CARTESIAN_POINT ( 'NONE',  ( 0.000000000000000000, 0.000000000000000000, 5.000000000000000000 ) ) ;
#37597 = FACE_OUTER_BOUND ( 'NONE', #105445, .T. ) ;
#37598 = CARTESIAN_POINT ( 'NONE',  ( 14.99451991528749595, 28.92564299267948513, 4.000000000000000000 ) ) ;
#37599 = CARTESIAN_POINT ( 'NONE',  ( 0.7307956238753654521, 3.821174125832445049E-16, 0.000000000000000000 ) ) ;
#37600 = EDGE_CURVE ( 'NONE', #73568, #24833, #88980, .T. ) ;
#37601 = ORIENTED_EDGE ( 'NONE', *, *, #66058, .T. ) ;
#37602 = CIRCLE ( 'NONE', #5165, 3.000000000000002665 ) ;
#37603 = EDGE_LOOP ( 'NONE', ( #119210, #64964, #56605, #17711 ) ) ;
#37604 = EDGE_CURVE ( 'NONE', #34897, #72728, #33879, .T. ) ;
#37605 = CARTESIAN_POINT ( 'NONE',  ( 27.19206980810188767, -7.934999999999991616, -2.126176841940955242 ) ) ;
#37606 = EDGE_CURVE ( 'NONE', #332, #74632, #43323, .T. ) ;
#37607 = FACE_OUTER_BOUND ( 'NONE', #6278, .T. ) ;
#37608 = CARTESIAN_POINT ( 'NONE',  ( 14.11270276996059181, -9.243106346249332361, -2.207712314992021696 ) ) ;
#37609 = ORIENTED_EDGE ( 'NONE', *, *, #72832, .T. ) ;
#37610 = ORIENTED_EDGE ( 'NONE', *, *, #128815, .F. ) ;
#37611 = EDGE_CURVE ( 'NONE', #126734, #85586, #109280, .T. ) ;
#37612 = ORIENTED_EDGE ( 'NONE', *, *, #109442, .T. ) ;
#37613 = DIRECTION ( 'NONE',  ( -0.000000000000000000, -0.000000000000000000, -1.000000000000000000 ) ) ;
#37614 = CARTESIAN_POINT ( 'NONE',  ( -42.18398860626899705, 28.73617430169816700, 5.000000000000000000 ) ) ;
#37615 = VECTOR ( 'NONE', #116606, 1000.000000000000000 ) ;
#37617 = DIRECTION ( 'NONE',  ( -0.7071067811865486830, -0.7071067811865464625, 0.000000000000000000 ) ) ;
#37616 = CIRCLE ( 'NONE', #58462, 2.500000000000000888 ) ;
#37618 = VECTOR ( 'NONE', #118061, 1000.000000000000227 ) ;
#37619 = EDGE_CURVE ( 'NONE', #59256, #23231, #33193, .T. ) ;
#37620 = CARTESIAN_POINT ( 'NONE',  ( 22.07159235450331991, 9.902892378096218942E-16, 0.000000000000000000 ) ) ;
#37621 = ORIENTED_EDGE ( 'NONE', *, *, #132424, .T. ) ;
#37622 = DIRECTION ( 'NONE',  ( -0.3543493200069162685, -0.000000000000000000, -0.9351131265310288487 ) ) ;
#37623 = VECTOR ( 'NONE', #115463, 1000.000000000000000 ) ;
#37624 = CARTESIAN_POINT ( 'NONE',  ( 8.510786437626906675, -27.52281430457049183, 5.000000000000000000 ) ) ;
#37625 = PRESENTATION_LAYER_ASSIGNMENT (  '', '', ( #35368 ) ) ;
#37626 = DIRECTION ( 'NONE',  ( -0.3543493200069162685, -0.000000000000000000, -0.9351131265310288487 ) ) ;
#37627 = ADVANCED_FACE ( 'NONE', ( #1207 ), #9957, .F. ) ;
#37628 = CARTESIAN_POINT ( 'NONE',  ( 5.915086768062343126, -12.74070752338415602, 18.74364270924355935 ) ) ;
#37629 = DIRECTION ( 'NONE',  ( -0.6830127018922181881, 0.6830127018922202975, -0.2588190451025214056 ) ) ;
#37630 = ORIENTED_EDGE ( 'NONE', *, *, #23773, .T. ) ;
#37631 = CARTESIAN_POINT ( 'NONE',  ( -3.328169399223503966, 2.259292476615697876, 4.000000000000000000 ) ) ;
#37632 = VECTOR ( 'NONE', #95792, 1000.000000000000000 ) ;
#37633 = VECTOR ( 'NONE', #130743, 1000.000000000000000 ) ;
#37634 = DIRECTION ( 'NONE',  ( -0.7071067811865486830, -0.7071067811865464625, 0.000000000000000000 ) ) ;
#37635 = EDGE_LOOP ( 'NONE', ( #30500, #101276, #126699, #88419 ) ) ;
#37636 = ADVANCED_FACE ( 'NONE', ( #121571 ), #131762, .F. ) ;
#37637 = DIRECTION ( 'NONE',  ( 0.7071067811865486830, -0.7071067811865464625, -0.000000000000000000 ) ) ;
#37639 = VERTEX_POINT ( 'NONE', #44036 ) ;
#37638 = FILL_AREA_STYLE ('',( #4197 ) ) ;
#37640 = EDGE_LOOP ( 'NONE', ( #7952, #39862, #122994, #118432 ) ) ;
#37641 = EDGE_CURVE ( 'NONE', #31122, #55910, #89666, .T. ) ;
#37642 = CARTESIAN_POINT ( 'NONE',  ( 0.7071067811865432429, 20.25929247661551003, 5.000000000000000000 ) ) ;
#37643 = DIRECTION ( 'NONE',  ( -0.7071067811865487940, 0.7071067811865463515, -0.000000000000000000 ) ) ;
#37644 = DIRECTION ( 'NONE',  ( -0.6830127018922181881, 0.6830127018922202975, -0.2588190451025214056 ) ) ;
#37645 = VERTEX_POINT ( 'NONE', #54920 ) ;
#37646 = CARTESIAN_POINT ( 'NONE',  ( 180.4193221990229574, -49.14999999999999147, -40.92499999999998295 ) ) ;
#37647 = UNCERTAINTY_MEASURE_WITH_UNIT (LENGTH_MEASURE( 1.000000000000000082E-05 ), #108752, 'distance_accuracy_value', 'NONE');
#37648 = EDGE_LOOP ( 'NONE', ( #74619, #32151, #65709, #109035 ) ) ;
#37649 = EDGE_CURVE ( 'NONE', #87036, #61991, #133895, .T. ) ;
#37650 = DIRECTION ( 'NONE',  ( 0.7071067811865487940, -0.7071067811865463515, 0.000000000000000000 ) ) ;
#37651 = CARTESIAN_POINT ( 'NONE',  ( 106.1458333333333144, 2.130196079827412436, -7.950000000000009059 ) ) ;
#37652 = CARTESIAN_POINT ( 'NONE',  ( 126.8083603837962272, 7.949999999999997513, 2.130196079827431088 ) ) ;
#37653 = DIRECTION ( 'NONE',  ( 0.6830127018922181881, 0.6830127018922202975, -0.2588190451025214056 ) ) ;
#37654 = VECTOR ( 'NONE', #78634, 1000.000000000000000 ) ;
#37655 = DIRECTION ( 'NONE',  ( 0.7071067811865487940, -0.7071067811865463515, 0.000000000000000000 ) ) ;
#37656 = DIRECTION ( 'NONE',  ( 0.6830127018922180770, -0.6830127018922204085, -0.2588190451025213501 ) ) ;
#37657 = CARTESIAN_POINT ( 'NONE',  ( -12.48921356237309155, -27.52281430457064104, 5.000000000000000000 ) ) ;
#37658 = CYLINDRICAL_SURFACE ( 'NONE', #29794, 0.5000000000000004441 ) ;
#37659 = CARTESIAN_POINT ( 'NONE',  ( 28.70790314143522437, -6.871911579029513106, -3.967499999999993587 ) ) ;
#37660 = CARTESIAN_POINT ( 'NONE',  ( 9.603736474768551190, 5.808823158059035485, 5.808823158059032821 ) ) ;
#37661 = CARTESIAN_POINT ( 'NONE',  ( 25.39999999999999858, 0.000000000000000000, 6.094999999999989093 ) ) ;
#37662 = LINE ( 'NONE', #92012, #263 ) ;
#37663 = FACE_OUTER_BOUND ( 'NONE', #116574, .T. ) ;
#37664 = ORIENTED_EDGE ( 'NONE', *, *, #38478, .T. ) ;
#37665 = MECHANICAL_DESIGN_GEOMETRIC_PRESENTATION_REPRESENTATION (  '', ( #49265 ), #83931 ) ;
#37666 = ORIENTED_EDGE ( 'NONE', *, *, #53875, .F. ) ;
#37667 = CARTESIAN_POINT ( 'NONE',  ( 94.33333333333332860, -6.884901960086287964, 3.974999999999998312 ) ) ;
#37668 = ORIENTED_EDGE ( 'NONE', *, *, #50311, .T. ) ;
#37669 = EDGE_LOOP ( 'NONE', ( #32133, #86394, #47511, #8441 ) ) ;
#37670 = PRODUCT_DEFINITION_SHAPE ( 'NONE', 'NONE',  #143558 ) ;
#37671 = VECTOR ( 'NONE', #17927, 1000.000000000000227 ) ;
#37672 = EDGE_CURVE ( 'NONE', #18833, #36342, #129305, .T. ) ;
#37673 = DIRECTION ( 'NONE',  ( -0.7071067811865487940, 0.7071067811865463515, 0.000000000000000000 ) ) ;
#37674 = TOROIDAL_SURFACE ( 'NONE', #109463, 25.00000000000002487, 3.000000000000000000 ) ;
#37675 = AXIS2_PLACEMENT_3D ( 'NONE', #62118, #62840, #93999 ) ;
#37676 = FACE_OUTER_BOUND ( 'NONE', #42936, .T. ) ;
#37677 = ORIENTED_EDGE ( 'NONE', *, *, #109516, .T. ) ;
#37678 = CARTESIAN_POINT ( 'NONE',  ( 13.49999999999991296, -4.533600742197688938, 5.000000000000000000 ) ) ;
#37679 = DIRECTION ( 'NONE',  ( 1.000000000000000000, 0.000000000000000000, 0.000000000000000000 ) ) ;
#37680 = DIRECTION ( 'NONE',  ( 0.000000000000000000, -1.000000000000000000, 0.000000000000000000 ) ) ;
#37681 = CARTESIAN_POINT ( 'NONE',  ( 125.5563301804876772, -2.994143682145710805, -7.321028783668758422 ) ) ;
#37682 = PLANE ( 'NONE',  #35437 ) ;
#37683 = DIRECTION ( 'NONE',  ( -0.5735764363510507113, 0.8191520442889885789, 1.003171929053520926E-16 ) ) ;
#37684 = DIRECTION ( 'NONE',  ( 0.7071067811865486830, -0.7071067811865464625, -0.000000000000000000 ) ) ;
#37685 = LINE ( 'NONE', #73169, #80019 ) ;
#37686 = LINE ( 'NONE', #46447, #65458 ) ;
#37687 = DIRECTION ( 'NONE',  ( 0.000000000000000000, 1.000000000000000000, 0.000000000000000000 ) ) ;
#37688 = CARTESIAN_POINT ( 'NONE',  ( -32.20710678118632586, -5.240707523384223521, 5.000000000000000000 ) ) ;
#37689 = EDGE_CURVE ( 'NONE', #72412, #126512, #123022, .T. ) ;
#37690 = CARTESIAN_POINT ( 'NONE',  ( -33.18398860626899705, 28.73617430169810305, 5.000000000000000000 ) ) ;
#37691 = EDGE_LOOP ( 'NONE', ( #121077, #53756, #39227, #83202 ) ) ;
#37692 = VERTEX_POINT ( 'NONE', #120118 ) ;
#37693 = CARTESIAN_POINT ( 'NONE',  ( 109.6670968585647756, -3.055000000000000160, -5.291415217122921177 ) ) ;
#37694 = ORIENTED_EDGE ( 'NONE', *, *, #115130, .T. ) ;
#37695 = ADVANCED_FACE ( 'NONE', ( #76684 ), #20827, .F. ) ;
#37696 = VECTOR ( 'NONE', #46673, 1000.000000000000000 ) ;
#37697 = CARTESIAN_POINT ( 'NONE',  ( 30.29974487139158867, -27.71228299555227537, 4.000000000000000000 ) ) ;
#37698 = AXIS2_PLACEMENT_3D ( 'NONE', #62815, #19978, #52616 ) ;
#37699 = LINE ( 'NONE', #124685, #78125 ) ;
#37700 = ORIENTED_EDGE ( 'NONE', *, *, #43639, .F. ) ;
#37701 = CARTESIAN_POINT ( 'NONE',  ( 3.489213562373097322, -27.52281430457057709, 5.000000000000000000 ) ) ;
#37702 = CARTESIAN_POINT ( 'NONE',  ( -51.18398860626899705, 28.73617430169823095, 5.000000000000000000 ) ) ;
#37703 = CARTESIAN_POINT ( 'NONE',  ( 100.6829301918981230, -1.637169565754158951, -6.109999999999998543 ) ) ;
#37704 = ORIENTED_EDGE ( 'NONE', *, *, #79198, .F. ) ;
#37705 = EDGE_CURVE ( 'NONE', #43034, #50767, #14249, .T. ) ;
#37706 = ORIENTED_EDGE ( 'NONE', *, *, #98814, .F. ) ;
#37707 = PLANE ( 'NONE',  #6009 ) ;
#37708 = VECTOR ( 'NONE', #79656, 1000.000000000000000 ) ;
#37709 = CARTESIAN_POINT ( 'NONE',  ( -30.18398860626900060, 28.73617430169808173, 5.000000000000000000 ) ) ;
#37710 = CARTESIAN_POINT ( 'NONE',  ( -24.69524342170288023, 1.235879655689124501, 4.000000000000000000 ) ) ;
#37711 = ORIENTED_EDGE ( 'NONE', *, *, #71330, .F. ) ;
#37712 = EDGE_LOOP ( 'NONE', ( #99813, #135063, #55865, #55304 ) ) ;
#37713 = ADVANCED_FACE ( 'NONE', ( #70804 ), #135345, .T. ) ;
#37714 = ORIENTED_EDGE ( 'NONE', *, *, #50250, .F. ) ;
#37715 = CARTESIAN_POINT ( 'NONE',  ( 23.99999999999983302, -15.03360074219758147, 5.000000000000000000 ) ) ;
#37716 = CARTESIAN_POINT ( 'NONE',  ( 0.5045698081018860082, 6.871911579029510442, -3.967499999999998916 ) ) ;
#37717 =( LENGTH_UNIT ( ) NAMED_UNIT ( * ) SI_UNIT ( .MILLI., .METRE. ) );
#37718 = DIRECTION ( 'NONE',  ( -0.7071067811865486830, -0.7071067811865464625, 0.000000000000000000 ) ) ;
#37719 = ORIENTED_EDGE ( 'NONE', *, *, #39306, .T. ) ;
#37720 = ORIENTED_EDGE ( 'NONE', *, *, #56425, .F. ) ;
#37721 = LINE ( 'NONE', #126150, #91864 ) ;
#37722 = ORIENTED_EDGE ( 'NONE', *, *, #119815, .T. ) ;
#37723 = ORIENTED_EDGE ( 'NONE', *, *, #75797, .T. ) ;
#37724 = VECTOR ( 'NONE', #136366, 1000.000000000000000 ) ;
#37725 = CARTESIAN_POINT ( 'NONE',  ( -14.59122188827396549, 7.143407583703162089, 5.000000000000000000 ) ) ;
#37726 = TOROIDAL_SURFACE ( 'NONE', #51602, 14.45000000000002238, 3.000000000000000000 ) ;
#37727 = CARTESIAN_POINT ( 'NONE',  ( 63.29974487139158867, -27.71228299555250274, 4.000000000000000000 ) ) ;
#37728 = EDGE_CURVE ( 'NONE', #131836, #104249, #38166, .T. ) ;
#37729 = ORIENTED_EDGE ( 'NONE', *, *, #13072, .F. ) ;
#37730 = CARTESIAN_POINT ( 'NONE',  ( 32.99999999999977263, 1.552185695429149304, 5.000000000000000000 ) ) ;
#37732 = CARTESIAN_POINT ( 'NONE',  ( -23.24139925780185223, 21.72500000000000853, 5.000000000000000000 ) ) ;
#37731 = VECTOR ( 'NONE', #10448, 999.9999999999998863 ) ;
#37733 = VECTOR ( 'NONE', #92188, 1000.000000000000000 ) ;
#37734 = AXIS2_PLACEMENT_3D ( 'NONE', #54155, #110603, #22171 ) ;
#37735 = FACE_OUTER_BOUND ( 'NONE', #88678, .T. ) ;
#37736 = PLANE ( 'NONE',  #109146 ) ;
#37737 = LINE ( 'NONE', #60202, #53681 ) ;
#37738 = FACE_BOUND ( 'NONE', #118095, .T. ) ;
#37739 = ORIENTED_EDGE ( 'NONE', *, *, #101737, .F. ) ;
#37740 = CARTESIAN_POINT ( 'NONE',  ( 12.79289321881335617, 18.75929247661552068, 5.000000000000000000 ) ) ;
#37741 = DIRECTION ( 'NONE',  ( -1.000000000000000000, -0.000000000000000000, -0.000000000000000000 ) ) ;
#37742 = EDGE_CURVE ( 'NONE', #56522, #132816, #137473, .T. ) ;
#37743 = ORIENTED_EDGE ( 'NONE', *, *, #44984, .F. ) ;
#37744 = DIRECTION ( 'NONE',  ( 0.7071067811865487940, 0.7071067811865463515, 0.000000000000000000 ) ) ;
#37745 = ORIENTED_EDGE ( 'NONE', *, *, #106630, .F. ) ;
#37746 = AXIS2_PLACEMENT_3D ( 'NONE', #88494, #31254, #29793 ) ;
#37747 = VERTEX_POINT ( 'NONE', #80953 ) ;
#37748 = ORIENTED_EDGE ( 'NONE', *, *, #55217, .F. ) ;
#37749 = PRODUCT_DEFINITION ( 'UNKNOWN', '', #102710, #125624 ) ;
#37750 = CARTESIAN_POINT ( 'NONE',  ( 34.91209685856478018, 5.291415217122921177, -3.054999999999994831 ) ) ;
#37751 = ORIENTED_EDGE ( 'NONE', *, *, #54012, .T. ) ;
#37752 = VECTOR ( 'NONE', #83657, 1000.000000000000000 ) ;
#37753 = CARTESIAN_POINT ( 'NONE',  ( 4.785015802758072034, -3.740707523384244837, 15.76143240460125128 ) ) ;
#37754 = CARTESIAN_POINT ( 'NONE',  ( -24.32816939922335564, 20.25929247661551003, 4.000000000000000000 ) ) ;
#37755 = CARTESIAN_POINT ( 'NONE',  ( -0.08491323193762084776, -12.74070752338415602, 18.74364270924354514 ) ) ;
#37756 = ORIENTED_EDGE ( 'NONE', *, *, #118643, .F. ) ;
#37757 = DIRECTION ( 'NONE',  ( 0.5735764363510453823, -0.8191520442889923537, 1.003171929053525486E-16 ) ) ;
#37758 = DIRECTION ( 'NONE',  ( 0.7071067811865487940, 0.7071067811865463515, 0.000000000000000000 ) ) ;
#37759 = ADVANCED_FACE ( 'NONE', ( #25838 ), #13508, .F. ) ;
#37761 = DIRECTION ( 'NONE',  ( 0.000000000000000000, -1.000000000000000000, 0.000000000000000000 ) ) ;
#37760 = VECTOR ( 'NONE', #87501, 1000.000000000000000 ) ;
#37762 = CARTESIAN_POINT ( 'NONE',  ( 12.69999999999999574, 0.000000000000000000, -40.00000000000000000 ) ) ;
#37763 = CARTESIAN_POINT ( 'NONE',  ( -39.48921356237310221, -27.52281430457082934, 5.000000000000000000 ) ) ;
#37764 = CARTESIAN_POINT ( 'NONE',  ( 51.48921356237309510, -27.52281430457091460, 5.000000000000000000 ) ) ;
#37765 = CIRCLE ( 'NONE', #60976, 3.000000000000000444 ) ;
#37766 = CARTESIAN_POINT ( 'NONE',  ( 57.48921356237308800, -27.52281430457095368, 5.000000000000000000 ) ) ;
#37767 = EDGE_LOOP ( 'NONE', ( #85472, #2988, #131860, #104928 ) ) ;
#37768 = VERTEX_POINT ( 'NONE', #35325 ) ;
#37769 = ORIENTED_EDGE ( 'NONE', *, *, #40373, .F. ) ;
#37770 = ORIENTED_EDGE ( 'NONE', *, *, #37600, .T. ) ;
#37771 = ORIENTED_EDGE ( 'NONE', *, *, #57061, .T. ) ;
#37772 = ORIENTED_EDGE ( 'NONE', *, *, #17897, .F. ) ;
#37773 = LINE ( 'NONE', #26868, #137100 ) ;
#37774 = LINE ( 'NONE', #92117, #23092 ) ;
#37775 = EDGE_LOOP ( 'NONE', ( #65114, #91699, #124224, #72924 ) ) ;
#37776 = PLANE ( 'NONE',  #94993 ) ;
#37777 = ORIENTED_EDGE ( 'NONE', *, *, #64465, .T. ) ;
#37779 = VECTOR ( 'NONE', #36895, 1000.000000000000000 ) ;
#37778 = CARTESIAN_POINT ( 'NONE',  ( 26.01088028653929740, -22.02621442084248216, 4.990779571109220214 ) ) ;
#37780 = CARTESIAN_POINT ( 'NONE',  ( 29.99451991528749417, 28.92564299267958816, 4.000000000000000000 ) ) ;
#37781 = EDGE_CURVE ( 'NONE', #57095, #69883, #42615, .T. ) ;
#37782 = VECTOR ( 'NONE', #100380, 999.9999999999998863 ) ;
#37783 = CARTESIAN_POINT ( 'NONE',  ( 2.108736474768552860, -5.808823158059033709, 5.808823158059035485 ) ) ;
#37784 = VERTEX_POINT ( 'NONE', #92505 ) ;
#37786 = DIRECTION ( 'NONE',  ( -0.6830127018922180770, -0.6830127018922204085, -0.2588190451025213501 ) ) ;
#37785 = CARTESIAN_POINT ( 'NONE',  ( 96.89126352523143737, -4.472830434245839371, -4.472830434245839371 ) ) ;
#37787 = ADVANCED_FACE ( 'NONE', ( #59918 ), #90381, .F. ) ;
#37788 = SURFACE_SIDE_STYLE ('',( #16722 ) ) ;
#37789 = DIRECTION ( 'NONE',  ( 0.7071067811865486830, -0.7071067811865464625, -0.000000000000000000 ) ) ;
#37790 = EDGE_LOOP ( 'NONE', ( #128683, #63531, #128097, #58135 ) ) ;
#37791 = PRESENTATION_LAYER_ASSIGNMENT (  '', '', ( #49070 ) ) ;
#37792 = ORIENTED_EDGE ( 'NONE', *, *, #30098, .F. ) ;
#37793 = EDGE_CURVE ( 'NONE', #94260, #124605, #69369, .T. ) ;
#37794 = CARTESIAN_POINT ( 'NONE',  ( 0.000000000000000000, 12.83542986846997813, -1.025386466790367379 ) ) ;
#37795 = VERTEX_POINT ( 'NONE', #113546 ) ;
#37796 = VECTOR ( 'NONE', #129284, 1000.000000000000227 ) ;
#37797 = DIRECTION ( 'NONE',  ( 0.7071067811865486830, -0.7071067811865464625, -0.000000000000000000 ) ) ;
#37798 = CARTESIAN_POINT ( 'NONE',  ( 8.510786437626906675, -27.52281430457049183, 5.000000000000000000 ) ) ;
#37799 = DIRECTION ( 'NONE',  ( -0.7071067811865487940, 0.7071067811865463515, 0.000000000000000000 ) ) ;
#37800 = ADVANCED_FACE ( 'NONE', ( #15628 ), #34382, .T. ) ;
#37801 = ADVANCED_FACE ( 'NONE', ( #3350 ), #47641, .F. ) ;
#37802 = CARTESIAN_POINT ( 'NONE',  ( 183.9019840361162323, -51.74944211519454029, -38.65549799471444459 ) ) ;
#37803 = EDGE_LOOP ( 'NONE', ( #125217, #13372, #62101, #105116, #68128 ) ) ;
#37804 = CARTESIAN_POINT ( 'NONE',  ( -24.96654721599509941, 3.964575861396866685, 4.000000000000000000 ) ) ;
#37805 = CARTESIAN_POINT ( 'NONE',  ( 19.99806943317887686, -22.22500000000000142, 4.500000000000000888 ) ) ;
#37806 = CARTESIAN_POINT ( 'NONE',  ( 0.000000000000000000, 0.000000000000000000, 5.000000000000000000 ) ) ;
#37807 = VERTEX_POINT ( 'NONE', #126563 ) ;
#37808 = LINE ( 'NONE', #26905, #139226 ) ;
#37809 = VECTOR ( 'NONE', #112132, 1000.000000000000000 ) ;
#37810 = DIRECTION ( 'NONE',  ( -0.7071067811865487940, 0.7071067811865463515, 0.000000000000000000 ) ) ;
#37811 = ORIENTED_EDGE ( 'NONE', *, *, #134014, .F. ) ;
#37812 = EDGE_CURVE ( 'NONE', #22385, #123961, #82386, .T. ) ;
#37814 = VERTEX_POINT ( 'NONE', #123753 ) ;
#37813 = CARTESIAN_POINT ( 'NONE',  ( -32.99999999999976552, 1.552185695429151080, 5.000000000000000000 ) ) ;
#37815 = EDGE_CURVE ( 'NONE', #81604, #91460, #59230, .T. ) ;
#37816 = VERTEX_POINT ( 'NONE', #49043 ) ;
#37817 = VECTOR ( 'NONE', #101860, 1000.000000000000000 ) ;
#37818 = DIRECTION ( 'NONE',  ( -0.7071067811865487940, 0.7071067811865463515, 0.000000000000000000 ) ) ;
#37819 = FACE_OUTER_BOUND ( 'NONE', #65674, .T. ) ;
#37820 = ORIENTED_EDGE ( 'NONE', *, *, #36686, .F. ) ;
#37821 = CARTESIAN_POINT ( 'NONE',  ( -63.48921356237309510, -27.52281430457099631, 5.000000000000000000 ) ) ;
#37822 = EDGE_CURVE ( 'NONE', #78479, #74127, #101256, .T. ) ;
#37823 = CARTESIAN_POINT ( 'NONE',  ( 8.999999999999937828, 12.25461709320621928, -10.07315571508695129 ) ) ;
#37824 = EDGE_LOOP ( 'NONE', ( #39319, #141033, #120352 ) ) ;
#37825 = DIRECTION ( 'NONE',  ( 0.3543493200069162685, -0.000000000000000000, -0.9351131265310288487 ) ) ;
#37826 = LINE ( 'NONE', #61037, #106768 ) ;
#37827 = DIRECTION ( 'NONE',  ( 0.7071067811865487940, 0.7071067811865463515, 0.000000000000000000 ) ) ;
#37828 = DIRECTION ( 'NONE',  ( 0.3543493200069162685, -0.000000000000000000, -0.9351131265310288487 ) ) ;
#37829 = ADVANCED_FACE ( 'NONE', ( #81686 ), #112868, .T. ) ;
#37830 = AXIS2_PLACEMENT_3D ( 'NONE', #140481, #82549, #72432 ) ;
#37831 = PLANE ( 'NONE',  #56359 ) ;
#37832 = CARTESIAN_POINT ( 'NONE',  ( 54.29974487139159578, -27.71228299555243879, 4.000000000000000000 ) ) ;
#37833 = DIRECTION ( 'NONE',  ( 0.7071067811865487940, 0.7071067811865463515, 0.000000000000000000 ) ) ;
#37834 = CARTESIAN_POINT ( 'NONE',  ( -16.82816939922341604, -5.240707523384227073, 4.000000000000000000 ) ) ;
#37835 = ORIENTED_EDGE ( 'NONE', *, *, #126033, .T. ) ;
#37836 = VECTOR ( 'NONE', #9350, 1000.000000000000000 ) ;
#37837 = ORIENTED_EDGE ( 'NONE', *, *, #95890, .F. ) ;
#37838 = ORIENTED_EDGE ( 'NONE', *, *, #30578, .T. ) ;
#37839 = CARTESIAN_POINT ( 'NONE',  ( 118.1041666666666714, 2.130196079827422206, 7.950000000000001954 ) ) ;
#37840 = ORIENTED_EDGE ( 'NONE', *, *, #138788, .F. ) ;
#37841 = ORIENTED_EDGE ( 'NONE', *, *, #22221, .F. ) ;
#37842 = VERTEX_POINT ( 'NONE', #72964 ) ;
#37843 = EDGE_CURVE ( 'NONE', #137207, #35625, #19253, .T. ) ;
#37844 = CONICAL_SURFACE ( 'NONE', #118832, 2.500000000000000888, 0.9599310885968822538 ) ;
#37845 = SURFACE_STYLE_USAGE ( .BOTH. , #93636 ) ;
#37846 = PRODUCT_DEFINITION_FORMATION_WITH_SPECIFIED_SOURCE ( 'ANY', '', #44431, .NOT_KNOWN. ) ;
#37847 = LINE ( 'NONE', #117491, #99502 ) ;
#37848 = ORIENTED_EDGE ( 'NONE', *, *, #73374, .T. ) ;
#37849 = DIRECTION ( 'NONE',  ( 0.000000000000000000, 0.000000000000000000, 1.000000000000000000 ) ) ;
#37850 = DIRECTION ( 'NONE',  ( 1.000000000000000000, 0.000000000000000000, 0.000000000000000000 ) ) ;
#37851 = DIRECTION ( 'NONE',  ( -1.000000000000000000, -1.224606353822377258E-16, -0.000000000000000000 ) ) ;
#37852 = CARTESIAN_POINT ( 'NONE',  ( 116.2295968585647756, -6.110000000000000320, -1.637169565754161393 ) ) ;
#37853 = VERTEX_POINT ( 'NONE', #106227 ) ;
#37854 = LINE ( 'NONE', #82089, #90428 ) ;
#37855 = LINE ( 'NONE', #113961, #49232 ) ;
#37856 = DIRECTION ( 'NONE',  ( 1.000000000000000000, 0.000000000000000000, 0.000000000000000000 ) ) ;
#37857 = SURFACE_SIDE_STYLE ('',( #48720 ) ) ;
#37858 = AXIS2_PLACEMENT_3D ( 'NONE', #48419, #81800, #139012 ) ;
#37859 = CARTESIAN_POINT ( 'NONE',  ( -21.71715331601274102, -2.164967620583693630, 5.000000000000000000 ) ) ;
#37860 = DIRECTION ( 'NONE',  ( 0.7071067811865487940, -0.7071067811865463515, 0.000000000000000000 ) ) ;
#37861 = CARTESIAN_POINT ( 'NONE',  ( 38.14169371712954870, -2.130196079827424871, -7.949999999999999289 ) ) ;
#37862 = EDGE_CURVE ( 'NONE', #18615, #30768, #95375, .T. ) ;
#37863 = DIRECTION ( 'NONE',  ( -0.000000000000000000, 0.3543493200069153248, 0.9351131265310292928 ) ) ;
#37865 = DIRECTION ( 'NONE',  ( -0.7071067811865486830, -0.7071067811865464625, 0.000000000000000000 ) ) ;
#37864 = AXIS2_PLACEMENT_3D ( 'NONE', #139470, #41525, #42991 ) ;
#37866 = ORIENTED_EDGE ( 'NONE', *, *, #110283, .F. ) ;
#37867 = ORIENTED_EDGE ( 'NONE', *, *, #81097, .F. ) ;
#37868 = CARTESIAN_POINT ( 'NONE',  ( 38.77083333333331439, -7.949999999999999289, -2.130196079827426203 ) ) ;
#37869 = ORIENTED_EDGE ( 'NONE', *, *, #19743, .T. ) ;
#37870 = ORIENTED_EDGE ( 'NONE', *, *, #60751, .T. ) ;
#37871 = LINE ( 'NONE', #126976, #127057 ) ;
#37872 = LINE ( 'NONE', #95789, #98729 ) ;
#37873 = ORIENTED_EDGE ( 'NONE', *, *, #27572, .T. ) ;
#37874 = CARTESIAN_POINT ( 'NONE',  ( 48.29974487139158867, -27.71228299555239971, 4.000000000000000000 ) ) ;
#37875 = VECTOR ( 'NONE', #109058, 1000.000000000000000 ) ;
#37876 = DIRECTION ( 'NONE',  ( -0.7071067811865486830, -0.7071067811865464625, 0.000000000000000000 ) ) ;
#37877 = CARTESIAN_POINT ( 'NONE',  ( -11.29289321881337749, 14.25929247661557042, 5.000000000000000000 ) ) ;
#37878 = CARTESIAN_POINT ( 'NONE',  ( 25.81293019189810778, -1.637169565754159617, -6.110000000000001208 ) ) ;
#37879 = AXIS2_PLACEMENT_3D ( 'NONE', #30081, #118521, #19219 ) ;
#37880 = ORIENTED_EDGE ( 'NONE', *, *, #34925, .F. ) ;
#37881 = EDGE_CURVE ( 'NONE', #143315, #15762, #127718, .T. ) ;
#37882 = DIRECTION ( 'NONE',  ( -0.6830127018922181881, 0.6830127018922202975, -0.2588190451025214056 ) ) ;
#37883 = ORIENTED_EDGE ( 'NONE', *, *, #52232, .F. ) ;
#37884 = CARTESIAN_POINT ( 'NONE',  ( 19.58200623001875940, 3.821174125832445049E-16, 0.000000000000000000 ) ) ;
#37885 = LINE ( 'NONE', #28423, #5946 ) ;
#37886 = DIRECTION ( 'NONE',  ( -0.000000000000000000, -0.000000000000000000, 1.000000000000000000 ) ) ;
#37887 = VECTOR ( 'NONE', #108335, 999.9999999999998863 ) ;
#37888 = DIRECTION ( 'NONE',  ( 0.7071067811865487940, 0.7071067811865463515, -0.000000000000000000 ) ) ;
#37889 = ORIENTED_EDGE ( 'NONE', *, *, #67875, .T. ) ;
#37890 = ADVANCED_FACE ( 'NONE', ( #8335 ), #84531, .F. ) ;
#37891 = ORIENTED_EDGE ( 'NONE', *, *, #31961, .F. ) ;
#37892 = CARTESIAN_POINT ( 'NONE',  ( -18.48921356237309510, -27.52281430457068367, 5.000000000000000000 ) ) ;
#37893 = PLANE ( 'NONE',  #134220 ) ;
#37894 = CARTESIAN_POINT ( 'NONE',  ( -16.77325839282156750, -11.24070752338416135, 18.24660765846978450 ) ) ;
#37895 = LINE ( 'NONE', #35771, #97186 ) ;
#37896 = VECTOR ( 'NONE', #117744, 1000.000000000000227 ) ;
#37897 = VECTOR ( 'NONE', #37594, 1000.000000000000000 ) ;
#37898 = CARTESIAN_POINT ( 'NONE',  ( 44.09959685856477307, -6.109999999999997655, -1.637169565754160283 ) ) ;
#37899 = ORIENTED_EDGE ( 'NONE', *, *, #18884, .T. ) ;
#37900 = LINE ( 'NONE', #80683, #83579 ) ;
#37901 = FACE_OUTER_BOUND ( 'NONE', #58430, .T. ) ;
#37902 = ORIENTED_EDGE ( 'NONE', *, *, #110551, .T. ) ;
#37903 = EDGE_LOOP ( 'NONE', ( #94816, #61046, #104550, #28533 ) ) ;
#37904 = AXIS2_PLACEMENT_3D ( 'NONE', #18000, #75997, #63713 ) ;
#37905 = DIRECTION ( 'NONE',  ( -0.000000000000000000, 0.000000000000000000, 1.000000000000000000 ) ) ;
#37906 = ORIENTED_EDGE ( 'NONE', *, *, #27028, .T. ) ;
#37907 = DIRECTION ( 'NONE',  ( -0.7071067811865487940, 0.7071067811865463515, 0.000000000000000000 ) ) ;
#37908 = ADVANCED_FACE ( 'NONE', ( #44622 ), #78637, .F. ) ;
#37909 = ORIENTED_EDGE ( 'NONE', *, *, #132577, .F. ) ;
#37910 = LINE ( 'NONE', #69106, #90920 ) ;
#37911 = VECTOR ( 'NONE', #21372, 1000.000000000000000 ) ;
#37912 = CARTESIAN_POINT ( 'NONE',  ( 44.99451991528749772, 28.92564299267969474, 4.000000000000000000 ) ) ;
#37913 = EDGE_CURVE ( 'NONE', #5176, #132203, #31565, .T. ) ;
#37914 = FACE_BOUND ( 'NONE', #55670, .T. ) ;
#37915 = CARTESIAN_POINT ( 'NONE',  ( 4.499999999999962697, -12.08601207473289385, -10.46905243149095632 ) ) ;
#37916 = CARTESIAN_POINT ( 'NONE',  ( -13.06996025486400725, -0.7407075233842735917, 13.87443053587614195 ) ) ;
#37918 = EDGE_CURVE ( 'NONE', #43696, #126534, #142536, .T. ) ;
#37917 = CARTESIAN_POINT ( 'NONE',  ( -48.48921356237309510, -27.52281430457089328, 5.000000000000000000 ) ) ;
#37919 = VECTOR ( 'NONE', #110057, 1000.000000000000000 ) ;
#37920 = CARTESIAN_POINT ( 'NONE',  ( -13.26601651615776767, 1.700382741644379081, 5.000000000000000000 ) ) ;
#37922 = ORIENTED_EDGE ( 'NONE', *, *, #77113, .F. ) ;
#37921 = LINE ( 'NONE', #50926, #45933 ) ;
#37923 = LINE ( 'NONE', #46697, #47207 ) ;
#37924 = ORIENTED_EDGE ( 'NONE', *, *, #63155, .T. ) ;
#37925 = ORIENTED_EDGE ( 'NONE', *, *, #4790, .T. ) ;
#37926 = CARTESIAN_POINT ( 'NONE',  ( 63.49543019189811588, 5.291415217122916737, 3.055000000000001936 ) ) ;
#37928 = ORIENTED_EDGE ( 'NONE', *, *, #38142, .T. ) ;
#37927 = VECTOR ( 'NONE', #21526, 1000.000000000000000 ) ;
#37929 = EDGE_CURVE ( 'NONE', #27002, #64405, #1038, .T. ) ;
#37930 = DIRECTION ( 'NONE',  ( 0.7071067811865487940, -0.7071067811865463515, 0.000000000000000000 ) ) ;
#37931 = DIRECTION ( 'NONE',  ( -0.7071067811865486830, -0.7071067811865464625, -0.000000000000000000 ) ) ;
#37932 = ORIENTED_EDGE ( 'NONE', *, *, #105372, .F. ) ;
#37933 = DIRECTION ( 'NONE',  ( 0.7071067811865487940, 0.7071067811865463515, 0.000000000000000000 ) ) ;
#37934 = ADVANCED_FACE ( 'NONE', ( #75789 ), #20662, .F. ) ;
#37935 = VECTOR ( 'NONE', #99227, 999.9999999999998863 ) ;
#37936 = CARTESIAN_POINT ( 'NONE',  ( -2.292893218813446321, 17.25929247661554200, 5.000000000000000000 ) ) ;
#37937 = CARTESIAN_POINT ( 'NONE',  ( 102.0625000000000000, -5.819803920172573086, -5.819803920172573974 ) ) ;
#37938 = DIRECTION ( 'NONE',  ( -0.7071067811865487940, 0.7071067811865463515, 0.000000000000000000 ) ) ;
#37939 = CARTESIAN_POINT ( 'NONE',  ( 2.700255128608413990, -27.71228299555204089, 4.000000000000000000 ) ) ;
#37940 = ORIENTED_EDGE ( 'NONE', *, *, #141542, .F. ) ;
#37941 = ORIENTED_EDGE ( 'NONE', *, *, #6447, .T. ) ;
#37942 = DIRECTION ( 'NONE',  ( -0.7071067811865487940, 0.7071067811865463515, -0.000000000000000000 ) ) ;
#37943 = CARTESIAN_POINT ( 'NONE',  ( -14.93988928955970508, -9.740707523384180888, 10.89222023123384453 ) ) ;
#37944 = VERTEX_POINT ( 'NONE', #54755 ) ;
#37945 = ORIENTED_EDGE ( 'NONE', *, *, #101202, .F. ) ;
#37946 = ORIENTED_EDGE ( 'NONE', *, *, #95198, .T. ) ;
#37947 = FACE_OUTER_BOUND ( 'NONE', #45199, .T. ) ;
#37948 = CARTESIAN_POINT ( 'NONE',  ( 19.05000000000000071, 3.174999999999997158, 4.000000000000000000 ) ) ;
#37949 = ORIENTED_EDGE ( 'NONE', *, *, #112087, .T. ) ;
#37950 = CARTESIAN_POINT ( 'NONE',  ( -8.292986735706895374, -21.74070752338406010, 4.999753212805224223 ) ) ;
#37951 = AXIS2_PLACEMENT_3D ( 'NONE', #121153, #47064, #21850 ) ;
#37952 = VECTOR ( 'NONE', #39248, 1000.000000000000000 ) ;
#37953 = CARTESIAN_POINT ( 'NONE',  ( 7.942069808101886785, 7.934999999999993392, 2.126176841940951689 ) ) ;
#37954 = EDGE_CURVE ( 'NONE', #55140, #35701, #13767, .T. ) ;
#37955 = CARTESIAN_POINT ( 'NONE',  ( 29.99999999999979039, 10.21212019023811912, -2.019456568337869129 ) ) ;
#37956 = ORIENTED_EDGE ( 'NONE', *, *, #72555, .F. ) ;
#37957 = PLANE ( 'NONE',  #48051 ) ;
#37958 = EDGE_CURVE ( 'NONE', #2262, #28263, #109101, .T. ) ;
#37959 = FACE_OUTER_BOUND ( 'NONE', #59346, .T. ) ;
#37960 = CARTESIAN_POINT ( 'NONE',  ( 0.000000000000000000, 0.000000000000000000, 5.000000000000000000 ) ) ;
#37962 = ORIENTED_EDGE ( 'NONE', *, *, #139606, .T. ) ;
#37961 = DIRECTION ( 'NONE',  ( -1.000000000000000000, -1.224606353822377258E-16, -0.000000000000000000 ) ) ;
#37963 = CARTESIAN_POINT ( 'NONE',  ( 11.42080628287044064, 3.047499999999997655, 5.278424836066143655 ) ) ;
#37964 = ORIENTED_EDGE ( 'NONE', *, *, #136846, .T. ) ;
#37965 = CARTESIAN_POINT ( 'NONE',  ( 34.42500000000002558, -21.76999999999999247, -37.00000000000000000 ) ) ;
#37966 = DIRECTION ( 'NONE',  ( 1.000000000000000000, 0.000000000000000000, -0.000000000000000000 ) ) ;
#37967 = VECTOR ( 'NONE', #26360, 1000.000000000000227 ) ;
#37968 = EDGE_CURVE ( 'NONE', #37040, #71393, #54063, .T. ) ;
#37969 = EDGE_CURVE ( 'NONE', #66281, #63704, #11184, .T. ) ;
#37970 = CARTESIAN_POINT ( 'NONE',  ( 108.4791666666666714, -7.950000000000000178, 2.130196079827424427 ) ) ;
#37971 = ORIENTED_EDGE ( 'NONE', *, *, #122511, .T. ) ;
#37972 = DIRECTION ( 'NONE',  ( 0.3543493200069163240, -0.000000000000000000, -0.9351131265310288487 ) ) ;
#37973 = AXIS2_PLACEMENT_3D ( 'NONE', #58148, #91459, #67584 ) ;
#37974 = CARTESIAN_POINT ( 'NONE',  ( -21.69326993309585561, -3.740707523384244837, 12.88036043432872546 ) ) ;
#37975 = FACE_OUTER_BOUND ( 'NONE', #103779, .T. ) ;
#37976 = DIRECTION ( 'NONE',  ( -0.7071067811865486830, -0.7071067811865464625, 0.000000000000000000 ) ) ;
#37977 = EDGE_LOOP ( 'NONE', ( #72413, #126871, #1865, #51960 ) ) ;
#37978 = DIRECTION ( 'NONE',  ( -0.7071067811865486830, -0.7071067811865464625, 0.000000000000000000 ) ) ;
#37979 = DIRECTION ( 'NONE',  ( -0.000000000000000000, -0.3543493200069152693, 0.9351131265310292928 ) ) ;
#37981 = CONICAL_SURFACE ( 'NONE', #7818, 2.500000000000000444, 0.9599310885968830309 ) ;
#37980 = LINE ( 'NONE', #135849, #132541 ) ;
#37982 = DIRECTION ( 'NONE',  ( -0.7071067811865486830, -0.7071067811865464625, -0.000000000000000000 ) ) ;
#37983 = ADVANCED_FACE ( 'NONE', ( #86668 ), #98251, .T. ) ;
#37984 = DIRECTION ( 'NONE',  ( -0.7071067811865486830, -0.7071067811865464625, 0.000000000000000000 ) ) ;
#37985 = VECTOR ( 'NONE', #14758, 1000.000000000000000 ) ;
#37986 = ORIENTED_EDGE ( 'NONE', *, *, #82063, .T. ) ;
#37987 = EDGE_CURVE ( 'NONE', #68652, #85225, #120680, .T. ) ;
#37988 = ORIENTED_EDGE ( 'NONE', *, *, #102830, .T. ) ;
#37989 = CARTESIAN_POINT ( 'NONE',  ( 10.15640092694706453, -2.499999999999999112, 0.000000000000000000 ) ) ;
#37990 = DIRECTION ( 'NONE',  ( 0.000000000000000000, -1.000000000000000000, 0.000000000000000000 ) ) ;
#37991 = VECTOR ( 'NONE', #125288, 999.9999999999998863 ) ;
#37992 = CARTESIAN_POINT ( 'NONE',  ( 5.082903141435219929, 3.967499999999992699, -6.871911579029513994 ) ) ;
#37993 = CARTESIAN_POINT ( 'NONE',  ( 11.71998032010589519, 0.7592924766157104211, 14.27032725228011678 ) ) ;
#37994 = VECTOR ( 'NONE', #102138, 1000.000000000000000 ) ;
#37995 = LINE ( 'NONE', #138726, #113258 ) ;
#37996 = CARTESIAN_POINT ( 'NONE',  ( 11.06845177300853855, 22.22500000000000142, -12.42863820230598648 ) ) ;
#37997 = EDGE_CURVE ( 'NONE', #43835, #12885, #32281, .T. ) ;
#37998 = CARTESIAN_POINT ( 'NONE',  ( 4.499999999999968914, -7.420205493532893826, -2.617629953481243277 ) ) ;
#37999 = ORIENTED_EDGE ( 'NONE', *, *, #126342, .F. ) ;
#38000 = CARTESIAN_POINT ( 'NONE',  ( -15.48921356237309510, -27.52281430457066236, 5.000000000000000000 ) ) ;
#38001 = PLANE ( 'NONE',  #65508 ) ;
#38002 = AXIS2_PLACEMENT_3D ( 'NONE', #20686, #109126, #143190 ) ;
#38003 = EDGE_CURVE ( 'NONE', #44481, #5925, #18416, .T. ) ;
#38004 = DIRECTION ( 'NONE',  ( -0.7071067811865486830, 0.7071067811865464625, 0.000000000000000000 ) ) ;
#38005 = CARTESIAN_POINT ( 'NONE',  ( 48.03709685856477307, -3.054999999999999272, -5.291415217122919401 ) ) ;
#38006 = CARTESIAN_POINT ( 'NONE',  ( 20.99999999999985079, -15.03360074219758324, 5.000000000000000000 ) ) ;
#38007 = AXIS2_PLACEMENT_3D ( 'NONE', #58300, #68443, #67729 ) ;
#38008 = VERTEX_POINT ( 'NONE', #9030 ) ;
#38009 = CARTESIAN_POINT ( 'NONE',  ( -31.49999999999977973, 16.46639925780208813, 5.000000000000000000 ) ) ;
#38010 = ORIENTED_EDGE ( 'NONE', *, *, #53533, .F. ) ;
#38011 = ORIENTED_EDGE ( 'NONE', *, *, #105342, .F. ) ;
#38013 = EDGE_CURVE ( 'NONE', #95865, #78216, #141766, .T. ) ;
#38012 = VECTOR ( 'NONE', #14421, 1000.000000000000000 ) ;
#38014 = CARTESIAN_POINT ( 'NONE',  ( 45.18398860626900415, 28.73617430169818832, 5.000000000000000000 ) ) ;
#38015 = DIRECTION ( 'NONE',  ( -1.000000000000000000, -0.000000000000000000, -0.000000000000000000 ) ) ;
#38016 = DIRECTION ( 'NONE',  ( -1.000000000000000000, -0.000000000000000000, -0.000000000000000000 ) ) ;
#38017 = CARTESIAN_POINT ( 'NONE',  ( 9.489213562373095101, -27.52281430457062328, 5.000000000000000000 ) ) ;
#38018 = CARTESIAN_POINT ( 'NONE',  ( -45.48921356237309510, -27.52281430457087197, 5.000000000000000000 ) ) ;
#38019 = EDGE_LOOP ( 'NONE', ( #110200, #142317, #54438, #52542 ) ) ;
#38020 = DIRECTION ( 'NONE',  ( -0.6830127018922180770, -0.6830127018922204085, -0.2588190451025213501 ) ) ;
#38021 = DIRECTION ( 'NONE',  ( -0.6830127018922181881, 0.6830127018922202975, -0.2588190451025214056 ) ) ;
#38022 = EDGE_CURVE ( 'NONE', #78032, #103081, #42468, .T. ) ;
#38023 = FACE_OUTER_BOUND ( 'NONE', #50107, .T. ) ;
#38024 = PLANE ( 'NONE',  #10288 ) ;
#38025 = DIRECTION ( 'NONE',  ( -0.6830127018922180770, -0.6830127018922204085, -0.2588190451025213501 ) ) ;
#38026 = CARTESIAN_POINT ( 'NONE',  ( 64.24586038379621300, 3.974999999999996980, 6.884901960086287964 ) ) ;
#38027 = ADVANCED_FACE ( 'NONE', ( #88087 ), #77240, .F. ) ;
#38028 = AXIS2_PLACEMENT_3D ( 'NONE', #33347, #65969, #117597 ) ;
#38029 = LINE ( 'NONE', #143031, #85440 ) ;
#38030 = ORIENTED_EDGE ( 'NONE', *, *, #30201, .T. ) ;
#38031 = EDGE_LOOP ( 'NONE', ( #3139, #67933, #76208, #38537 ) ) ;
#38032 = CARTESIAN_POINT ( 'NONE',  ( 63.56249999999999289, -5.819803920172572198, -5.819803920172573086 ) ) ;
#38033 = DIRECTION ( 'NONE',  ( 0.3543493200069162685, -0.000000000000000000, -0.9351131265310288487 ) ) ;
#38034 = DIRECTION ( 'NONE',  ( 0.7071067811865487940, 0.7071067811865463515, 0.000000000000000000 ) ) ;
#38035 = DIRECTION ( 'NONE',  ( -0.000000000000000000, 0.3543493200069153248, 0.9351131265310292928 ) ) ;
#38036 = ORIENTED_EDGE ( 'NONE', *, *, #79772, .T. ) ;
#38037 = AXIS2_PLACEMENT_3D ( 'NONE', #88195, #11293, #55571 ) ;
#38038 = CARTESIAN_POINT ( 'NONE',  ( -6.183988606268994381, 28.73617430169791476, 5.000000000000000000 ) ) ;
#38039 = CARTESIAN_POINT ( 'NONE',  ( 24.29974487139158867, -27.71228299555223273, 4.000000000000000000 ) ) ;
#38040 = CARTESIAN_POINT ( 'NONE',  ( 57.02126352523143993, -4.472830434245839371, -4.472830434245840259 ) ) ;
#38041 = DIRECTION ( 'NONE',  ( -0.6830127018922181881, 0.6830127018922202975, -0.2588190451025214056 ) ) ;
#38042 = EDGE_LOOP ( 'NONE', ( #137086, #12869, #20891, #84899 ) ) ;
#38043 = VERTEX_POINT ( 'NONE', #59754 ) ;
#38044 = DIRECTION ( 'NONE',  ( 0.7071067811865486830, -0.7071067811865464625, -0.000000000000000000 ) ) ;
#38045 = CARTESIAN_POINT ( 'NONE',  ( 6.471592354503322042, -2.500000000000000444, 3.061616997868384620E-16 ) ) ;
#38046 = FACE_OUTER_BOUND ( 'NONE', #5204, .T. ) ;
#38047 = CARTESIAN_POINT ( 'NONE',  ( -6.183988606268994381, 28.73617430169791476, 5.000000000000000000 ) ) ;
#38048 = DIRECTION ( 'NONE',  ( 0.7071067811865487940, -0.7071067811865463515, 0.000000000000000000 ) ) ;
#38050 = ORIENTED_EDGE ( 'NONE', *, *, #122923, .T. ) ;
#38049 = CARTESIAN_POINT ( 'NONE',  ( 100.9958603837962272, -3.974999999999998312, -6.884901960086286188 ) ) ;
#38051 = LINE ( 'NONE', #62653, #120096 ) ;
#38052 = DIRECTION ( 'NONE',  ( 0.000000000000000000, 0.000000000000000000, 1.000000000000000000 ) ) ;
#38053 = CARTESIAN_POINT ( 'NONE',  ( -24.41161490594814509, 22.22500000000000497, 4.777194822843814137 ) ) ;
#38054 = VECTOR ( 'NONE', #109225, 999.9999999999998863 ) ;
#38055 = LINE ( 'NONE', #124328, #120163 ) ;
#38056 = ORIENTED_EDGE ( 'NONE', *, *, #140323, .T. ) ;
#38057 = AXIS2_PLACEMENT_3D ( 'NONE', #85777, #29961, #20499 ) ;
#38058 = VERTEX_POINT ( 'NONE', #101806 ) ;
#38059 = CARTESIAN_POINT ( 'NONE',  ( 0.000000000000000000, 18.08204922493373346, 0.9627537363044872398 ) ) ;
#38060 = VECTOR ( 'NONE', #57814, 1000.000000000000000 ) ;
#38061 = CARTESIAN_POINT ( 'NONE',  ( -54.48921356237310221, -27.52281430457093236, 5.000000000000000000 ) ) ;
#38062 = CARTESIAN_POINT ( 'NONE',  ( 4.184256412735922304, 2.055000000000001048, 2.516649172247811554E-16 ) ) ;
#38063 = ADVANCED_FACE ( 'NONE', ( #14795 ), #15472, .F. ) ;
#38064 = DIRECTION ( 'NONE',  ( 0.000000000000000000, 0.000000000000000000, 1.000000000000000000 ) ) ;
#38065 = LINE ( 'NONE', #50360, #64036 ) ;
#38066 = VERTEX_POINT ( 'NONE', #46027 ) ;
#38067 = ORIENTED_EDGE ( 'NONE', *, *, #70748, .F. ) ;
#38068 = CARTESIAN_POINT ( 'NONE',  ( -16.49999999999988987, -4.216083040037264418, -7.486842126848618051 ) ) ;
#38069 = DIRECTION ( 'NONE',  ( 0.7071067811865487940, 0.7071067811865463515, 0.000000000000000000 ) ) ;
#38070 = ORIENTED_EDGE ( 'NONE', *, *, #132246, .T. ) ;
#38071 = AXIS2_PLACEMENT_3D ( 'NONE', #66507, #78806, #46205 ) ;
#38072 = FACE_OUTER_BOUND ( 'NONE', #16669, .T. ) ;
#38073 = EDGE_CURVE ( 'NONE', #117034, #106208, #103915, .T. ) ;
#38074 = EDGE_LOOP ( 'NONE', ( #84523, #73916, #63869, #126118, #21778 ) ) ;
#38075 = CARTESIAN_POINT ( 'NONE',  ( 62.49586038379623432, -3.974999999999998312, -6.884901960086286188 ) ) ;
#38076 = LINE ( 'NONE', #27891, #49414 ) ;
#38077 = VECTOR ( 'NONE', #73973, 1000.000000000000227 ) ;
#38078 = EDGE_CURVE ( 'NONE', #97698, #121504, #48871, .T. ) ;
#38079 = FACE_BOUND ( 'NONE', #70654, .T. ) ;
#38080 = PLANE ( 'NONE',  #3828 ) ;
#38081 = DIRECTION ( 'NONE',  ( -1.000000000000000000, -1.224606353822377258E-16, -0.000000000000000000 ) ) ;
#38082 = ADVANCED_FACE ( 'NONE', ( #59067 ), #37272, .F. ) ;
#38083 = CARTESIAN_POINT ( 'NONE',  ( 0.000000000000000000, 0.000000000000000000, 5.000000000000000000 ) ) ;
#38084 = CARTESIAN_POINT ( 'NONE',  ( 34.49999999999975131, 8.319652575858413002, -8.582050562765747515 ) ) ;
#38086 = EDGE_CURVE ( 'NONE', #139562, #6765, #90955, .T. ) ;
#38085 = VECTOR ( 'NONE', #76103, 1000.000000000000000 ) ;
#38087 = FILL_AREA_STYLE_COLOUR ( '', #88075 ) ;
#38088 = PRODUCT_CONTEXT ( 'NONE', #30025, 'mechanical' ) ;
#38089 = ORIENTED_EDGE ( 'NONE', *, *, #106045, .F. ) ;
#38090 = VECTOR ( 'NONE', #121373, 999.9999999999998863 ) ;
#38091 = ORIENTED_EDGE ( 'NONE', *, *, #109523, .F. ) ;
#38092 = CARTESIAN_POINT ( 'NONE',  ( 97.91209685856478018, 5.291415217122921177, -3.054999999999994831 ) ) ;
#38093 = EDGE_LOOP ( 'NONE', ( #109123, #107733, #53461, #135462, #1387 ) ) ;
#38094 = ADVANCED_FACE ( 'NONE', ( #93076 ), #81515, .F. ) ;
#38095 = LINE ( 'NONE', #112082, #2527 ) ;
#38096 = DIRECTION ( 'NONE',  ( 0.000000000000000000, 0.000000000000000000, 1.000000000000000000 ) ) ;
#38097 = EDGE_CURVE ( 'NONE', #1886, #125922, #14068, .T. ) ;
#38098 = AXIS2_PLACEMENT_3D ( 'NONE', #61321, #105459, #6124 ) ;
#38099 = FACE_OUTER_BOUND ( 'NONE', #124135, .T. ) ;
#38100 = EDGE_LOOP ( 'NONE', ( #143099, #68634, #18780, #134089 ) ) ;
#38101 = DIRECTION ( 'NONE',  ( -0.000000000000000000, -1.000000000000000000, 0.000000000000000000 ) ) ;
#38102 = CARTESIAN_POINT ( 'NONE',  ( 18.95159235450331892, 9.902892378096218942E-16, 0.000000000000000000 ) ) ;
#38103 = CARTESIAN_POINT ( 'NONE',  ( -6.781626882924903121, 21.74787736706805319, 4.999607392498050196 ) ) ;
#38105 = DIRECTION ( 'NONE',  ( 0.000000000000000000, -1.000000000000000000, 0.000000000000000000 ) ) ;
#38104 = DIRECTION ( 'NONE',  ( -0.7071067811865487940, 0.7071067811865463515, -0.000000000000000000 ) ) ;
#38106 = DIRECTION ( 'NONE',  ( 0.6830127018922180770, -0.6830127018922204085, -0.2588190451025213501 ) ) ;
#38107 = CARTESIAN_POINT ( 'NONE',  ( 181.1499999999998067, -47.62213595499955687, -36.92499999999996163 ) ) ;
#38108 = EDGE_CURVE ( 'NONE', #105436, #40538, #55189, .T. ) ;
#38109 = DIRECTION ( 'NONE',  ( 0.3543493200069162685, -0.000000000000000000, -0.9351131265310288487 ) ) ;
#38110 = ORIENTED_EDGE ( 'NONE', *, *, #10991, .F. ) ;
#38111 = CARTESIAN_POINT ( 'NONE',  ( 72.18398860626899705, 28.73617430169837661, 5.000000000000000000 ) ) ;
#38112 = CARTESIAN_POINT ( 'NONE',  ( 60.29974487139158867, -27.71228299555248142, 4.000000000000000000 ) ) ;
#38113 = ORIENTED_EDGE ( 'NONE', *, *, #81954, .F. ) ;
#38114 = ORIENTED_EDGE ( 'NONE', *, *, #122546, .T. ) ;
#38115 = VERTEX_POINT ( 'NONE', #23528 ) ;
#38116 = CARTESIAN_POINT ( 'NONE',  ( 47.54209685856476852, 5.291415217122923842, -3.054999999999996163 ) ) ;
#38117 = EDGE_CURVE ( 'NONE', #64517, #61398, #113010, .T. ) ;
#38118 = EDGE_LOOP ( 'NONE', ( #89634, #51915, #74257, #132177 ) ) ;
#38119 = CARTESIAN_POINT ( 'NONE',  ( 15.50413961620377279, -3.047499999999994547, 5.278424836066145431 ) ) ;
#38120 =( NAMED_UNIT ( * ) PLANE_ANGLE_UNIT ( ) SI_UNIT ( $, .RADIAN. ) );
#38121 = VERTEX_POINT ( 'NONE', #69195 ) ;
#38122 = LINE ( 'NONE', #113510, #112796 ) ;
#38123 = EDGE_CURVE ( 'NONE', #70705, #20468, #91646, .T. ) ;
#38124 = ORIENTED_EDGE ( 'NONE', *, *, #129559, .T. ) ;
#38125 = CYLINDRICAL_SURFACE ( 'NONE', #92768, 3.999999999999996447 ) ;
#38126 = DIRECTION ( 'NONE',  ( 1.000000000000000000, 0.000000000000000000, -0.000000000000000000 ) ) ;
#38128 = ORIENTED_EDGE ( 'NONE', *, *, #116848, .F. ) ;
#38127 = DIRECTION ( 'NONE',  ( -0.3543493200069162685, -0.000000000000000000, -0.9351131265310288487 ) ) ;
#38129 = ORIENTED_EDGE ( 'NONE', *, *, #130289, .T. ) ;
#38130 = CIRCLE ( 'NONE', #47485, 2.055000000000001048 ) ;
#38131 = DIRECTION ( 'NONE',  ( -0.7071067811865486830, 0.7071067811865464625, 0.000000000000000000 ) ) ;
#38132 = DIRECTION ( 'NONE',  ( -0.7071067811865487940, 0.7071067811865463515, 0.000000000000000000 ) ) ;
#38133 = ADVANCED_FACE ( 'NONE', ( #113378 ), #35153, .F. ) ;
#38134 = ADVANCED_FACE ( 'NONE', ( #124985 ), #136561, .T. ) ;
#38135 = EDGE_LOOP ( 'NONE', ( #2269, #35746, #123783, #100918 ) ) ;
#38136 = CARTESIAN_POINT ( 'NONE',  ( -26.99999999999980815, 12.25461709320618553, -10.07315571508703478 ) ) ;
#38137 = ORIENTED_EDGE ( 'NONE', *, *, #84969, .F. ) ;
#38138 = ORIENTED_EDGE ( 'NONE', *, *, #61082, .F. ) ;
#38139 = VERTEX_POINT ( 'NONE', #74181 ) ;
#38140 = EDGE_LOOP ( 'NONE', ( #20056, #105288, #59501, #9470 ) ) ;
#38141 = PLANE ( 'NONE',  #17091 ) ;
#38142 = EDGE_CURVE ( 'NONE', #51507, #90821, #48239, .T. ) ;
#38143 = DIRECTION ( 'NONE',  ( 0.000000000000000000, 1.000000000000000000, -2.556434596176436916E-15 ) ) ;
#38144 = DIRECTION ( 'NONE',  ( -0.7071067811865486830, 0.7071067811865464625, 0.000000000000000000 ) ) ;
#38145 = ADVANCED_FACE ( 'NONE', ( #115490 ), #50298, .T. ) ;
#38146 = LINE ( 'NONE', #60644, #48347 ) ;
#38147 = DIRECTION ( 'NONE',  ( -0.000000000000000000, 0.000000000000000000, 1.000000000000000000 ) ) ;
#38148 = ORIENTED_EDGE ( 'NONE', *, *, #58347, .T. ) ;
#38149 = AXIS2_PLACEMENT_3D ( 'NONE', #129191, #18268, #62546 ) ;
#38150 = DIRECTION ( 'NONE',  ( -0.7071067811865487940, 0.7071067811865463515, 0.000000000000000000 ) ) ;
#38151 = AXIS2_PLACEMENT_3D ( 'NONE', #49285, #15167, #35565 ) ;
#38152 = CARTESIAN_POINT ( 'NONE',  ( 18.06206980810188867, -7.934999999999991616, -2.126176841940955242 ) ) ;
#38153 = DIRECTION ( 'NONE',  ( -0.000000000000000000, -0.3543493200069152693, 0.9351131265310292928 ) ) ;
#38154 = DIRECTION ( 'NONE',  ( -0.000000000000000000, 0.000000000000000000, 1.000000000000000000 ) ) ;
#38155 = EDGE_CURVE ( 'NONE', #61902, #70075, #107509, .T. ) ;
#38156 = LINE ( 'NONE', #104817, #92973 ) ;
#38157 = ORIENTED_EDGE ( 'NONE', *, *, #86511, .T. ) ;
#38158 = VECTOR ( 'NONE', #35177, 1000.000000000000000 ) ;
#38159 = ORIENTED_EDGE ( 'NONE', *, *, #33549, .F. ) ;
#38160 = ORIENTED_EDGE ( 'NONE', *, *, #136123, .T. ) ;
#38161 = FACE_OUTER_BOUND ( 'NONE', #68762, .T. ) ;
#38162 = CARTESIAN_POINT ( 'NONE',  ( 95.01669371712955581, 7.950000000000000178, -2.130196079827421318 ) ) ;
#38163 = DIRECTION ( 'NONE',  ( -1.000000000000000000, 0.000000000000000000, 0.000000000000000000 ) ) ;
#38164 = FACE_OUTER_BOUND ( 'NONE', #35364, .T. ) ;
#38165 = EDGE_CURVE ( 'NONE', #122527, #82873, #16188, .T. ) ;
#38166 = LINE ( 'NONE', #80253, #110764 ) ;
#38167 = CARTESIAN_POINT ( 'NONE',  ( 70.34959685856478018, 6.109999999999997655, 1.637169565754163836 ) ) ;
#38168 =( BOUNDED_SURFACE ( )  B_SPLINE_SURFACE ( 1, 2, ( 
 ( #33011, #12632, #24244, #68488, #101792, #2455, #50287, #60467, #27083, #115482, #94474, #3863, #6008, #104643, #103906, #81505, #36540, #106046, #61887, #72794, #59059, #93065, #5315, #17615, #26392, #4554, #27802, #116241, #92323, #82918, #138004, #49595, #137295, #72067, #16177, #93778, #80776, #38689, #37992, #47469, #127101, #103210, #16932, #48143, #138724, #61207, #105352, #39413, #91637, #48860, #82222, #124973, #83647, #135859, #37260, #127855, #28536, #116949, #70641, #125711, #25655, #69930, #114102, #14786, #136550, #114783, #15458, #59746, #126393, #71324, #140152, #86484, #74911, #40827, #85741, #42273, #6713, #74173, #50997, #95189, #40148, #141575, #107499, #96585, #139463, #85035, #140826, #129240, #29928, #41519, #118364, #19065, #30680, #63327, #119083, #8161, #129978, #108179, #19773, #51718, #84362, #52398, #62589, #8842, #128552, #29223, #73465, #64010, #117630, #18315, #53103, #97304, #106773, #7452, #95911, #132709, #79769, #123951, #33398, #134844, #102195, #77599, #34088, #68866, #101456, #68179, #44252, #113037, #110878, #11564, #57282, #56590, #89862, #112352, #78298, #89173, #79039, #69584, #58002, #122483, #123244, #36224, #133399, #22445, #88467, #702, #46418, #55844, #90601, #121769, #23918, #35539, #100050, #1407, #113767, #25317, #24612, #12304, #143538, #67437, #13709, #13007, #2104, #2852, #66704, #47152, #44998, #14457, #58736, #23159, #111634, #100755, #91330, #135540, #45692, #134107, #34796, #80451, #124642, #73145, #60864, #126088, #81898, #105714, #72452, #26055, #128228, #15144, #26755, #28905, #117309, #139104, #94840, #17981, #71004, #61565, #94139, #49958, #39807, #49258, #37659, #138377, #105024, #38357, #70317, #114466, #115154, #15828, #28192, #102905, #6374, #4218, #3545, #47842, #92008, #59425, #136225, #103584, #60124, #36910, #81160, #84032, #125366, #48511, #104291, #50650, #39063, #83286, #92713, #93448, #4954, #127497, #5691, #82572, #136948, #137683, #126765, #27447, #116620, #71708, #115874 ),
 ( #16573, #17303, #41192, #108555, #52771, #64384, #131072, #9235, #62986, #32480, #19447, #128920, #31760, #142663, #106412, #109311, #18707, #76720, #87566, #107161, #29595, #20861, #96259, #118005, #7840, #40508, #8522, #53515, #41932, #62257, #129624, #65125, #119447, #74562, #73833, #120148, #131791, #63696, #31063, #75977, #9996, #139837, #96965, #75282, #54260, #120891, #98440, #20144, #86142, #130371, #43355, #52083, #7102, #97720, #118753, #140504, #51378, #95575, #84710, #85399, #30326, #107857, #141972, #141214, #42662, #86863, #1930, #90417, #66537, #57112, #112190, #23734, #67247, #46235, #133927, #89701, #10682, #68006, #111447, #36062, #78851, #33229, #34615, #77438, #123788, #101291, #134664, #12835, #135383, #122304, #12128, #54955, #57821, #80286, #11384, #79603, #99865, #100597, #102011, #55664, #44070, #65860, #22270, #35357, #121602, #24443, #143364, #1240, #68691, #132538, #22979, #91162, #46974, #112880, #33913, #21599, #89017, #13542, #45523, #123059, #2675, #110015, #99119, #88291, #110705, #528, #44827, #133236, #78132, #56414, #82413, #94680, #3383, #50494, #48345, #115695, #138938, #126596, #4061, #103414, #127321, #93979, #47675, #6219, #36744, #92535, #39639, #124475, #17148, #116456, #25147, #136772, #83121, #16395, #71539, #61413, #70836, #59261, #60696, #27286, #59954, #91837, #136061, #37485, #81720, #49806, #69399, #28025, #25875, #113584, #14281, #58567, #102736, #138214, #70146, #125920, #104860, #80985, #137506, #105555, #125191, #26595, #114308, #14985, #114986, #93271, #15665, #104115, #72291, #38899, #5525, #4779, #49082, #38201, #109143, #7676, #85972, #117148, #130931, #107710, #72999, #19981, #64227, #17828, #75128, #42499, #62099, #117848, #9072, #41756, #8366, #128070, #53329, #51214, #95410, #141051, #140349, #30150, #52618, #18534, #29432, #19287, #9829, #54100, #98288, #28752, #142513, #97549, #128756, #51933, #130207, #106257, #96804, #119986, #83866, #129464, #6930, #139674, #20701, #30897, #40354 ) ),
 .UNSPECIFIED., .F., .F., .F. ) 
 B_SPLINE_SURFACE_WITH_KNOTS ( ( 2, 2 ),
 ( 3, 2, 2, 2, 2, 2, 2, 2, 2, 2, 2, 2, 2, 2, 2, 2, 2, 2, 2, 2, 2, 2, 2, 2, 2, 2, 2, 2, 2, 2, 2, 2, 2, 2, 2, 2, 2, 2, 2, 2, 2, 2, 2, 2, 2, 2, 2, 2, 2, 2, 2, 2, 2, 2, 2, 2, 2, 2, 2, 2, 2, 2, 2, 2, 2, 2, 2, 2, 2, 2, 2, 2, 2, 2, 2, 2, 2, 2, 2, 2, 2, 2, 2, 2, 2, 2, 2, 2, 2, 2, 2, 2, 2, 2, 2, 2, 2, 2, 2, 2, 2, 2, 2, 2, 2, 2, 2, 2, 2, 2, 2, 2, 2, 2, 2, 2, 2, 2, 2, 2, 3 ),
 ( 0.000000000000000000, 1.000000000000000000 ),
 ( 0.000000000000000000, 0.008333333333333333218, 0.01666666666666666644, 0.02500000000000000139, 0.03333333333333333287, 0.04166666666666666435, 0.05000000000000000278, 0.05833333333333333426, 0.06666666666666666574, 0.07499999999999999722, 0.08333333333333332871, 0.09166666666666666019, 0.1000000000000000056, 0.1083333333333333370, 0.1166666666666666685, 0.1250000000000000000, 0.1333333333333333315, 0.1416666666666666630, 0.1499999999999999944, 0.1583333333333333259, 0.1666666666666666574, 0.1749999999999999889, 0.1833333333333333204, 0.1916666666666666796, 0.2000000000000000111, 0.2083333333333333426, 0.2166666666666666741, 0.2250000000000000056, 0.2333333333333333370, 0.2416666666666666685, 0.2500000000000000000, 0.2583333333333333592, 0.2666666666666666630, 0.2750000000000000222, 0.2833333333333333259, 0.2916666666666666852, 0.2999999999999999889, 0.3083333333333333481, 0.3166666666666666519, 0.3250000000000000111, 0.3333333333333333148, 0.3416666666666666741, 0.3499999999999999778, 0.3583333333333333370, 0.3666666666666666408, 0.3750000000000000000, 0.3833333333333333592, 0.3916666666666666630, 0.4000000000000000222, 0.4083333333333333259, 0.4166666666666666852, 0.4249999999999999889, 0.4333333333333333481, 0.4416666666666666519, 0.4500000000000000111, 0.4583333333333333148, 0.4666666666666666741, 0.4749999999999999778, 0.4833333333333333370, 0.4916666666666666408, 0.5000000000000000000, 0.5083333333333333037, 0.5166666666666667185, 0.5250000000000000222, 0.5333333333333333259, 0.5416666666666666297, 0.5500000000000000444, 0.5583333333333333481, 0.5666666666666666519, 0.5749999999999999556, 0.5833333333333333703, 0.5916666666666666741, 0.5999999999999999778, 0.6083333333333332815, 0.6166666666666666963, 0.6250000000000000000, 0.6333333333333333037, 0.6416666666666667185, 0.6500000000000000222, 0.6583333333333333259, 0.6666666666666666297, 0.6750000000000000444, 0.6833333333333333481, 0.6916666666666666519, 0.6999999999999999556, 0.7083333333333333703, 0.7166666666666666741, 0.7249999999999999778, 0.7333333333333332815, 0.7416666666666666963, 0.7500000000000000000, 0.7583333333333333037, 0.7666666666666667185, 0.7750000000000000222, 0.7833333333333333259, 0.7916666666666666297, 0.8000000000000000444, 0.8083333333333333481, 0.8166666666666666519, 0.8249999999999999556, 0.8333333333333333703, 0.8416666666666666741, 0.8499999999999999778, 0.8583333333333332815, 0.8666666666666666963, 0.8750000000000000000, 0.8833333333333333037, 0.8916666666666667185, 0.9000000000000000222, 0.9083333333333333259, 0.9166666666666666297, 0.9250000000000000444, 0.9333333333333333481, 0.9416666666666666519, 0.9499999999999999556, 0.9583333333333333703, 0.9666666666666666741, 0.9749999999999999778, 0.9833333333333332815, 0.9916666666666666963, 1.000000000000000000 ),
 .UNSPECIFIED. ) 
 GEOMETRIC_REPRESENTATION_ITEM ( )  RATIONAL_B_SPLINE_SURFACE ( (
 ( 1.000000000000000000, 0.9659258262890683122, 1.000000000000000000, 0.9659258262890683122, 1.000000000000000000, 0.9659258262890683122, 1.000000000000000000, 0.9659258262890683122, 1.000000000000000000, 0.9659258262890683122, 1.000000000000000000, 0.9659258262890683122, 1.000000000000000000, 0.9659258262890683122, 1.000000000000000000, 0.9659258262890683122, 1.000000000000000000, 0.9659258262890683122, 1.000000000000000000, 0.9659258262890683122, 1.000000000000000000, 0.9659258262890683122, 1.000000000000000000, 0.9659258262890683122, 1.000000000000000000, 0.9659258262890683122, 1.000000000000000000, 0.9659258262890683122, 1.000000000000000000, 0.9659258262890683122, 1.000000000000000000, 0.9659258262890683122, 1.000000000000000000, 0.9659258262890683122, 1.000000000000000000, 0.9659258262890683122, 1.000000000000000000, 0.9659258262890683122, 1.000000000000000000, 0.9659258262890683122, 1.000000000000000000, 0.9659258262890683122, 1.000000000000000000, 0.9659258262890683122, 1.000000000000000000, 0.9659258262890683122, 1.000000000000000000, 0.9659258262890683122, 1.000000000000000000, 0.9659258262890683122, 1.000000000000000000, 0.9659258262890683122, 1.000000000000000000, 0.9659258262890683122, 1.000000000000000000, 0.9659258262890683122, 1.000000000000000000, 0.9659258262890683122, 1.000000000000000000, 0.9659258262890683122, 1.000000000000000000, 0.9659258262890683122, 1.000000000000000000, 0.9659258262890683122, 1.000000000000000000, 0.9659258262890683122, 1.000000000000000000, 0.9659258262890683122, 1.000000000000000000, 0.9659258262890683122, 1.000000000000000000, 0.9659258262890683122, 1.000000000000000000, 0.9659258262890683122, 1.000000000000000000, 0.9659258262890683122, 1.000000000000000000, 0.9659258262890683122, 1.000000000000000000, 0.9659258262890683122, 1.000000000000000000, 0.9659258262890683122, 1.000000000000000000, 0.9659258262890683122, 1.000000000000000000, 0.9659258262890683122, 1.000000000000000000, 0.9659258262890683122, 1.000000000000000000, 0.9659258262890683122, 1.000000000000000000, 0.9659258262890683122, 1.000000000000000000, 0.9659258262890683122, 1.000000000000000000, 0.9659258262890683122, 1.000000000000000000, 0.9659258262890683122, 1.000000000000000000, 0.9659258262890683122, 1.000000000000000000, 0.9659258262890683122, 1.000000000000000000, 0.9659258262890683122, 1.000000000000000000, 0.9659258262890683122, 1.000000000000000000, 0.9659258262890683122, 1.000000000000000000, 0.9659258262890683122, 1.000000000000000000, 0.9659258262890683122, 1.000000000000000000, 0.9659258262890683122, 1.000000000000000000, 0.9659258262890683122, 1.000000000000000000, 0.9659258262890683122, 1.000000000000000000, 0.9659258262890683122, 1.000000000000000000, 0.9659258262890683122, 1.000000000000000000, 0.9659258262890683122, 1.000000000000000000, 0.9659258262890683122, 1.000000000000000000, 0.9659258262890683122, 1.000000000000000000, 0.9659258262890683122, 1.000000000000000000, 0.9659258262890683122, 1.000000000000000000, 0.9659258262890683122, 1.000000000000000000, 0.9659258262890683122, 1.000000000000000000, 0.9659258262890683122, 1.000000000000000000, 0.9659258262890683122, 1.000000000000000000, 0.9659258262890683122, 1.000000000000000000, 0.9659258262890683122, 1.000000000000000000, 0.9659258262890683122, 1.000000000000000000, 0.9659258262890683122, 1.000000000000000000, 0.9659258262890683122, 1.000000000000000000, 0.9659258262890683122, 1.000000000000000000, 0.9659258262890683122, 1.000000000000000000, 0.9659258262890683122, 1.000000000000000000, 0.9659258262890683122, 1.000000000000000000, 0.9659258262890683122, 1.000000000000000000, 0.9659258262890683122, 1.000000000000000000, 0.9659258262890683122, 1.000000000000000000, 0.9659258262890683122, 1.000000000000000000, 0.9659258262890683122, 1.000000000000000000, 0.9659258262890683122, 1.000000000000000000, 0.9659258262890683122, 1.000000000000000000, 0.9659258262890683122, 1.000000000000000000, 0.9659258262890683122, 1.000000000000000000, 0.9659258262890683122, 1.000000000000000000, 0.9659258262890683122, 1.000000000000000000, 0.9659258262890683122, 1.000000000000000000, 0.9659258262890683122, 1.000000000000000000, 0.9659258262890683122, 1.000000000000000000, 0.9659258262890683122, 1.000000000000000000, 0.9659258262890683122, 1.000000000000000000, 0.9659258262890683122, 1.000000000000000000, 0.9659258262890683122, 1.000000000000000000, 0.9659258262890683122, 1.000000000000000000, 0.9659258262890683122, 1.000000000000000000, 0.9659258262890683122, 1.000000000000000000, 0.9659258262890683122, 1.000000000000000000, 0.9659258262890683122, 1.000000000000000000, 0.9659258262890683122, 1.000000000000000000, 0.9659258262890683122, 1.000000000000000000, 0.9659258262890683122, 1.000000000000000000, 0.9659258262890683122, 1.000000000000000000, 0.9659258262890683122, 1.000000000000000000, 0.9659258262890683122, 1.000000000000000000, 0.9659258262890683122, 1.000000000000000000, 0.9659258262890683122, 1.000000000000000000, 0.9659258262890683122, 1.000000000000000000, 0.9659258262890683122, 1.000000000000000000, 0.9659258262890683122, 1.000000000000000000, 0.9659258262890683122, 1.000000000000000000, 0.9659258262890683122, 1.000000000000000000, 0.9659258262890683122, 1.000000000000000000, 0.9659258262890683122, 1.000000000000000000, 0.9659258262890683122, 1.000000000000000000, 0.9659258262890683122, 1.000000000000000000, 0.9659258262890683122, 1.000000000000000000),
 ( 1.000000000000000000, 0.9659258262890683122, 1.000000000000000000, 0.9659258262890683122, 1.000000000000000000, 0.9659258262890683122, 1.000000000000000000, 0.9659258262890683122, 1.000000000000000000, 0.9659258262890683122, 1.000000000000000000, 0.9659258262890683122, 1.000000000000000000, 0.9659258262890683122, 1.000000000000000000, 0.9659258262890683122, 1.000000000000000000, 0.9659258262890683122, 1.000000000000000000, 0.9659258262890683122, 1.000000000000000000, 0.9659258262890683122, 1.000000000000000000, 0.9659258262890683122, 1.000000000000000000, 0.9659258262890683122, 1.000000000000000000, 0.9659258262890683122, 1.000000000000000000, 0.9659258262890683122, 1.000000000000000000, 0.9659258262890683122, 1.000000000000000000, 0.9659258262890683122, 1.000000000000000000, 0.9659258262890683122, 1.000000000000000000, 0.9659258262890683122, 1.000000000000000000, 0.9659258262890683122, 1.000000000000000000, 0.9659258262890683122, 1.000000000000000000, 0.9659258262890683122, 1.000000000000000000, 0.9659258262890683122, 1.000000000000000000, 0.9659258262890683122, 1.000000000000000000, 0.9659258262890683122, 1.000000000000000000, 0.9659258262890683122, 1.000000000000000000, 0.9659258262890683122, 1.000000000000000000, 0.9659258262890683122, 1.000000000000000000, 0.9659258262890683122, 1.000000000000000000, 0.9659258262890683122, 1.000000000000000000, 0.9659258262890683122, 1.000000000000000000, 0.9659258262890683122, 1.000000000000000000, 0.9659258262890683122, 1.000000000000000000, 0.9659258262890683122, 1.000000000000000000, 0.9659258262890683122, 1.000000000000000000, 0.9659258262890683122, 1.000000000000000000, 0.9659258262890683122, 1.000000000000000000, 0.9659258262890683122, 1.000000000000000000, 0.9659258262890683122, 1.000000000000000000, 0.9659258262890683122, 1.000000000000000000, 0.9659258262890683122, 1.000000000000000000, 0.9659258262890683122, 1.000000000000000000, 0.9659258262890683122, 1.000000000000000000, 0.9659258262890683122, 1.000000000000000000, 0.9659258262890683122, 1.000000000000000000, 0.9659258262890683122, 1.000000000000000000, 0.9659258262890683122, 1.000000000000000000, 0.9659258262890683122, 1.000000000000000000, 0.9659258262890683122, 1.000000000000000000, 0.9659258262890683122, 1.000000000000000000, 0.9659258262890683122, 1.000000000000000000, 0.9659258262890683122, 1.000000000000000000, 0.9659258262890683122, 1.000000000000000000, 0.9659258262890683122, 1.000000000000000000, 0.9659258262890683122, 1.000000000000000000, 0.9659258262890683122, 1.000000000000000000, 0.9659258262890683122, 1.000000000000000000, 0.9659258262890683122, 1.000000000000000000, 0.9659258262890683122, 1.000000000000000000, 0.9659258262890683122, 1.000000000000000000, 0.9659258262890683122, 1.000000000000000000, 0.9659258262890683122, 1.000000000000000000, 0.9659258262890683122, 1.000000000000000000, 0.9659258262890683122, 1.000000000000000000, 0.9659258262890683122, 1.000000000000000000, 0.9659258262890683122, 1.000000000000000000, 0.9659258262890683122, 1.000000000000000000, 0.9659258262890683122, 1.000000000000000000, 0.9659258262890683122, 1.000000000000000000, 0.9659258262890683122, 1.000000000000000000, 0.9659258262890683122, 1.000000000000000000, 0.9659258262890683122, 1.000000000000000000, 0.9659258262890683122, 1.000000000000000000, 0.9659258262890683122, 1.000000000000000000, 0.9659258262890683122, 1.000000000000000000, 0.9659258262890683122, 1.000000000000000000, 0.9659258262890683122, 1.000000000000000000, 0.9659258262890683122, 1.000000000000000000, 0.9659258262890683122, 1.000000000000000000, 0.9659258262890683122, 1.000000000000000000, 0.9659258262890683122, 1.000000000000000000, 0.9659258262890683122, 1.000000000000000000, 0.9659258262890683122, 1.000000000000000000, 0.9659258262890683122, 1.000000000000000000, 0.9659258262890683122, 1.000000000000000000, 0.9659258262890683122, 1.000000000000000000, 0.9659258262890683122, 1.000000000000000000, 0.9659258262890683122, 1.000000000000000000, 0.9659258262890683122, 1.000000000000000000, 0.9659258262890683122, 1.000000000000000000, 0.9659258262890683122, 1.000000000000000000, 0.9659258262890683122, 1.000000000000000000, 0.9659258262890683122, 1.000000000000000000, 0.9659258262890683122, 1.000000000000000000, 0.9659258262890683122, 1.000000000000000000, 0.9659258262890683122, 1.000000000000000000, 0.9659258262890683122, 1.000000000000000000, 0.9659258262890683122, 1.000000000000000000, 0.9659258262890683122, 1.000000000000000000, 0.9659258262890683122, 1.000000000000000000, 0.9659258262890683122, 1.000000000000000000, 0.9659258262890683122, 1.000000000000000000, 0.9659258262890683122, 1.000000000000000000, 0.9659258262890683122, 1.000000000000000000, 0.9659258262890683122, 1.000000000000000000, 0.9659258262890683122, 1.000000000000000000, 0.9659258262890683122, 1.000000000000000000, 0.9659258262890683122, 1.000000000000000000, 0.9659258262890683122, 1.000000000000000000, 0.9659258262890683122, 1.000000000000000000, 0.9659258262890683122, 1.000000000000000000, 0.9659258262890683122, 1.000000000000000000, 0.9659258262890683122, 1.000000000000000000, 0.9659258262890683122, 1.000000000000000000, 0.9659258262890683122, 1.000000000000000000, 0.9659258262890683122, 1.000000000000000000, 0.9659258262890683122, 1.000000000000000000, 0.9659258262890683122, 1.000000000000000000, 0.9659258262890683122, 1.000000000000000000, 0.9659258262890683122, 1.000000000000000000) ) ) 
 REPRESENTATION_ITEM ( '' )  SURFACE ( )  );
#38169 = CARTESIAN_POINT ( 'NONE',  ( 1.629999999999999893, -0.3999999999999997446, -2.500000000000000000 ) ) ;
#38170 = LINE ( 'NONE', #36712, #34462 ) ;
#38171 = VECTOR ( 'NONE', #118551, 1000.000000000000000 ) ;
#38172 = DIRECTION ( 'NONE',  ( -0.7071067811865486830, -0.7071067811865464625, 0.000000000000000000 ) ) ;
#38173 = DIRECTION ( 'NONE',  ( -0.7071067811865486830, -0.7071067811865464625, -0.000000000000000000 ) ) ;
#38174 = CARTESIAN_POINT ( 'NONE',  ( -25.17183060077629619, -17.24070752338409918, 4.000000000000000000 ) ) ;
#38175 = ORIENTED_EDGE ( 'NONE', *, *, #18210, .F. ) ;
#38176 = CARTESIAN_POINT ( 'NONE',  ( 17.01299344985120499, -0.9444868010259039881, -36.22218118524219932 ) ) ;
#38177 = VERTEX_POINT ( 'NONE', #28546 ) ;
#38178 =( BOUNDED_CURVE ( )  B_SPLINE_CURVE ( 2, ( #128502, #6657, #81450, #84306, #138669, #69870, #72005, #83580, #48804, #40092, #27741, #50941, #136499 ),
 .UNSPECIFIED., .F., .T. ) 
 B_SPLINE_CURVE_WITH_KNOTS ( ( 3, 2, 2, 2, 2, 2, 3 ),
 ( 0.8666666666666668073, 0.8694444444444445752, 0.8722222222222223431, 0.8750000000000001110, 0.8777777777777778789, 0.8805555555555556468, 0.8833333333333334147 ),
 .UNSPECIFIED. ) 
 CURVE ( )  GEOMETRIC_REPRESENTATION_ITEM ( )  RATIONAL_B_SPLINE_CURVE ( ( 0.9999999999999986677, 0.9659258262890696445, 1.000000000000000000, 0.9659258262890683122, 1.000000000000000000, 0.9659258262890683122, 1.000000000000000000, 0.9659258262890683122, 1.000000000000000000, 0.9659258262890683122, 1.000000000000000000, 0.9659258262890669799, 1.000000000000001332 ) ) 
 REPRESENTATION_ITEM ( '' )  );
#38179 = CARTESIAN_POINT ( 'NONE',  ( -14.70025512860841133, -27.71228299555195917, 4.000000000000000000 ) ) ;
#38181 = VERTEX_POINT ( 'NONE', #60479 ) ;
#38180 = CARTESIAN_POINT ( 'NONE',  ( -24.48921356237309510, -27.52281430457072631, 5.000000000000000000 ) ) ;
#38182 = DIRECTION ( 'NONE',  ( -0.6830127018922180770, -0.6830127018922204085, -0.2588190451025213501 ) ) ;
#38183 = CARTESIAN_POINT ( 'NONE',  ( 5.204170427930421283E-15, -0.4125381241607568028, 4.000000000000000000 ) ) ;
#38184 = ORIENTED_EDGE ( 'NONE', *, *, #85869, .F. ) ;
#38185 = PLANE ( 'NONE',  #120185 ) ;
#38186 = ORIENTED_EDGE ( 'NONE', *, *, #16168, .T. ) ;
#38187 = FILL_AREA_STYLE_COLOUR ( '', #42092 ) ;
#38188 = VERTEX_POINT ( 'NONE', #51006 ) ;
#38189 = DIRECTION ( 'NONE',  ( -0.7071067811865486830, 0.7071067811865464625, 0.000000000000000000 ) ) ;
#38190 = AXIS2_PLACEMENT_3D ( 'NONE', #85240, #74402, #118589 ) ;
#38191 = ADVANCED_FACE ( 'NONE', ( #40837 ), #8170, .F. ) ;
#38192 = CARTESIAN_POINT ( 'NONE',  ( 91.22502705046289861, 5.819803920172573086, -5.819803920172572198 ) ) ;
#38194 = VECTOR ( 'NONE', #126898, 1000.000000000000000 ) ;
#38193 = CARTESIAN_POINT ( 'NONE',  ( 0.000000000000000000, 0.000000000000000000, 5.000000000000000000 ) ) ;
#38195 = AXIS2_PLACEMENT_3D ( 'NONE', #141149, #20079, #7033 ) ;
#38196 = CARTESIAN_POINT ( 'NONE',  ( 7.940000000000001279, -33.26999999999999602, -8.101350000000008933 ) ) ;
#38197 = VERTEX_POINT ( 'NONE', #127112 ) ;
#38198 = CIRCLE ( 'NONE', #119192, 2.500000000000000888 ) ;
#38199 = PLANE ( 'NONE',  #65440 ) ;
#38200 = CARTESIAN_POINT ( 'NONE',  ( -29.99999999999979750, -13.39766691384885711, -10.96608748226458907 ) ) ;
#38201 = CARTESIAN_POINT ( 'NONE',  ( 28.14583333333333570, -1.633150327867689988, 6.094999999999989981 ) ) ;
#38202 = DIRECTION ( 'NONE',  ( 0.6830127018922181881, 0.6830127018922202975, -0.2588190451025214056 ) ) ;
#38203 = CARTESIAN_POINT ( 'NONE',  ( -18.18398860626898994, 28.73617430169800002, 5.000000000000000000 ) ) ;
#38204 = ORIENTED_EDGE ( 'NONE', *, *, #76279, .T. ) ;
#38205 = CARTESIAN_POINT ( 'NONE',  ( -6.707106781186494615, -9.740707523384186217, 5.000000000000000000 ) ) ;
#38206 = ORIENTED_EDGE ( 'NONE', *, *, #39435, .T. ) ;
#38207 = CARTESIAN_POINT ( 'NONE',  ( 84.00043019189810423, -3.055000000000002380, 5.291415217122920289 ) ) ;
#38208 = LINE ( 'NONE', #102746, #138079 ) ;
#38209 = CARTESIAN_POINT ( 'NONE',  ( 34.92499999999998295, -22.22500000000000142, 4.500000000000000888 ) ) ;
#38210 = CARTESIAN_POINT ( 'NONE',  ( 9.299744871391588674, -27.71228299555212971, 4.000000000000000000 ) ) ;
#38211 = ORIENTED_EDGE ( 'NONE', *, *, #87590, .F. ) ;
#38212 = LINE ( 'NONE', #59275, #134511 ) ;
#38213 = CARTESIAN_POINT ( 'NONE',  ( 118.7875270504628986, 0.000000000000000000, -7.949999999999998401 ) ) ;
#38214 = FACE_OUTER_BOUND ( 'NONE', #70577, .T. ) ;
#38216 = ORIENTED_EDGE ( 'NONE', *, *, #121722, .F. ) ;
#38215 = CARTESIAN_POINT ( 'NONE',  ( -12.18398860626900060, 28.73617430169795739, 5.000000000000000000 ) ) ;
#38217 = DIRECTION ( 'NONE',  ( -0.6830127018922180770, -0.6830127018922204085, -0.2588190451025213501 ) ) ;
#38218 = CARTESIAN_POINT ( 'NONE',  ( 1.783126656679975719, -5.054327988459295540, 3.799291974498469227 ) ) ;
#38219 = PLANE ( 'NONE',  #97882 ) ;
#38220 = ORIENTED_EDGE ( 'NONE', *, *, #58205, .F. ) ;
#38221 = ORIENTED_EDGE ( 'NONE', *, *, #108828, .T. ) ;
#38222 = EDGE_LOOP ( 'NONE', ( #126170, #65338, #80567, #58013 ) ) ;
#38223 = CARTESIAN_POINT ( 'NONE',  ( 79.91709685856476142, 3.054999999999998828, 5.291415217122922066 ) ) ;
#38224 = VERTEX_POINT ( 'NONE', #82926 ) ;
#38225 = CARTESIAN_POINT ( 'NONE',  ( 27.48921356237309155, -27.52281430457074762, 5.000000000000000000 ) ) ;
#38226 = DIRECTION ( 'NONE',  ( -0.000000000000000000, -0.3543493200069152693, 0.9351131265310292928 ) ) ;
#38227 = EDGE_CURVE ( 'NONE', #103631, #110059, #5325, .T. ) ;
#38228 = DIRECTION ( 'NONE',  ( 0.6830127018922181881, 0.6830127018922202975, -0.2588190451025214056 ) ) ;
#38229 = DIRECTION ( 'NONE',  ( 0.000000000000000000, 1.000000000000000000, 0.000000000000000000 ) ) ;
#38230 = EDGE_LOOP ( 'NONE', ( #107317, #28821, #67118, #61637, #75451, #53870 ) ) ;
#38231 = CARTESIAN_POINT ( 'NONE',  ( -11.99451991528749417, 28.92564299267946382, 4.000000000000000000 ) ) ;
#38232 = DIRECTION ( 'NONE',  ( -0.000000000000000000, 0.3543493200069153248, 0.9351131265310291818 ) ) ;
#38233 = ADVANCED_FACE ( 'NONE', ( #72080 ), #85046, .T. ) ;
#38234 = ORIENTED_EDGE ( 'NONE', *, *, #7298, .F. ) ;
#38235 = DIRECTION ( 'NONE',  ( 0.7071067811865486830, -0.7071067811865464625, -0.000000000000000000 ) ) ;
#38236 = LINE ( 'NONE', #6255, #10808 ) ;
#38237 = DIRECTION ( 'NONE',  ( -0.7071067811865486830, -0.7071067811865464625, -0.000000000000000000 ) ) ;
#38238 = ORIENTED_EDGE ( 'NONE', *, *, #72476, .T. ) ;
#38239 = ORIENTED_EDGE ( 'NONE', *, *, #63734, .F. ) ;
#38240 = ADVANCED_FACE ( 'NONE', ( #105362 ), #51726, .T. ) ;
#38241 = CARTESIAN_POINT ( 'NONE',  ( -12.48921356237309155, -27.52281430457064104, 5.000000000000000000 ) ) ;
#38242 = ADVANCED_FACE ( 'NONE', ( #117641 ), #19076, .F. ) ;
#38243 = EDGE_CURVE ( 'NONE', #3762, #69864, #127868, .T. ) ;
#38244 = DIRECTION ( 'NONE',  ( 1.000000000000000000, 1.224606353822377258E-16, 0.000000000000000000 ) ) ;
#38245 = CARTESIAN_POINT ( 'NONE',  ( -19.82816939922339472, 18.75929247661552779, 4.000000000000000000 ) ) ;
#38246 = CARTESIAN_POINT ( 'NONE',  ( -8.999999999999937828, 12.83542986846996570, -1.025386466790349171 ) ) ;
#38247 = DIRECTION ( 'NONE',  ( 0.000000000000000000, 0.000000000000000000, 1.000000000000000000 ) ) ;
#38248 = DIRECTION ( 'NONE',  ( -0.7071067811865486830, 0.7071067811865464625, 0.000000000000000000 ) ) ;
#38249 = ADVANCED_FACE ( 'NONE', ( #116959 ), #106784, .T. ) ;
#38250 = EDGE_CURVE ( 'NONE', #62679, #32117, #40159, .T. ) ;
#38251 = DIRECTION ( 'NONE',  ( 0.6830127018922180770, -0.6830127018922204085, -0.2588190451025213501 ) ) ;
#38253 = EDGE_LOOP ( 'NONE', ( #73883, #136570, #24, #45925 ) ) ;
#38252 = VECTOR ( 'NONE', #94696, 1000.000000000000000 ) ;
#38254 = ORIENTED_EDGE ( 'NONE', *, *, #83411, .F. ) ;
#38255 = ORIENTED_EDGE ( 'NONE', *, *, #38097, .F. ) ;
#38256 = ADVANCED_FACE ( 'NONE', ( #129250 ), #29938, .F. ) ;
#38257 = ORIENTED_EDGE ( 'NONE', *, *, #135081, .F. ) ;
#38258 = DIRECTION ( 'NONE',  ( 0.7071067811865486830, -0.7071067811865464625, -0.000000000000000000 ) ) ;
#38259 = EDGE_CURVE ( 'NONE', #112794, #132213, #110342, .T. ) ;
#38260 = EDGE_LOOP ( 'NONE', ( #125786, #59985, #82868, #64877 ) ) ;
#38261 = VECTOR ( 'NONE', #29064, 1000.000000000000000 ) ;
#38262 = LINE ( 'NONE', #106326, #28722 ) ;
#38263 = LINE ( 'NONE', #128138, #103491 ) ;
#38264 = CARTESIAN_POINT ( 'NONE',  ( 8.811592354503320124, 2.500000000000001332, 0.000000000000000000 ) ) ;
#38265 = DIRECTION ( 'NONE',  ( 0.5735764363510451602, 0.8191520442889924647, 0.000000000000000000 ) ) ;
#38266 = ORIENTED_EDGE ( 'NONE', *, *, #32945, .T. ) ;
#38267 = CARTESIAN_POINT ( 'NONE',  ( 33.85005128541003927, -8.240707523384196875, 17.25253755692247282 ) ) ;
#38268 = DIRECTION ( 'NONE',  ( -0.7071067811865486830, -0.7071067811865464625, 0.000000000000000000 ) ) ;
#38269 = ORIENTED_EDGE ( 'NONE', *, *, #127119, .T. ) ;
#38270 = CARTESIAN_POINT ( 'NONE',  ( 5.204170427930421283E-15, -6.412538124160692909, 4.000000000000000000 ) ) ;
#38271 = EDGE_LOOP ( 'NONE', ( #78463, #71491, #138918, #141176 ) ) ;
#38272 = ORIENTED_EDGE ( 'NONE', *, *, #55216, .T. ) ;
#38273 = DIRECTION ( 'NONE',  ( 0.7071067811865487940, -0.7071067811865463515, 0.000000000000000000 ) ) ;
#38274 = ORIENTED_EDGE ( 'NONE', *, *, #121811, .F. ) ;
#38275 = ORIENTED_EDGE ( 'NONE', *, *, #110847, .F. ) ;
#38276 = CARTESIAN_POINT ( 'NONE',  ( 72.62543019189810423, 5.291415217122919401, 3.055000000000002824 ) ) ;
#38277 = EDGE_CURVE ( 'NONE', #44302, #66646, #121233, .T. ) ;
#38278 = EDGE_LOOP ( 'NONE', ( #9723, #136706, #141934, #7186 ) ) ;
#38279 = VECTOR ( 'NONE', #137707, 1000.000000000000000 ) ;
#38280 = CARTESIAN_POINT ( 'NONE',  ( 95.35416666666665719, -2.130196079827425759, -7.950000000000000178 ) ) ;
#38281 = AXIS2_PLACEMENT_3D ( 'NONE', #61339, #28684, #60616 ) ;
#38282 = AXIS2_PLACEMENT_3D ( 'NONE', #35571, #13742, #730 ) ;
#38283 = LINE ( 'NONE', #107088, #79824 ) ;
#38284 = CARTESIAN_POINT ( 'NONE',  ( 111.4170968585647614, 3.054999999999998828, 5.291415217122922066 ) ) ;
#38285 = CARTESIAN_POINT ( 'NONE',  ( 33.08314806772910543, 21.75929247661549937, 7.311836541448126781 ) ) ;
#38286 = AXIS2_PLACEMENT_3D ( 'NONE', #120239, #98528, #119536 ) ;
#38287 = DIRECTION ( 'NONE',  ( 0.000000000000000000, 0.000000000000000000, 1.000000000000000000 ) ) ;
#38288 = EDGE_CURVE ( 'NONE', #58719, #69864, #11740, .T. ) ;
#38289 = LINE ( 'NONE', #81090, #48708 ) ;
#38290 = DIRECTION ( 'NONE',  ( -1.000000000000000000, -1.224606353822377258E-16, -0.000000000000000000 ) ) ;
#38291 = PLANE ( 'NONE',  #40058 ) ;
#38292 = CARTESIAN_POINT ( 'NONE',  ( 29.29289321881325847, -9.740707523384177335, 5.000000000000000000 ) ) ;
#38294 = EDGE_CURVE ( 'NONE', #134932, #89365, #74920, .T. ) ;
#38293 = CARTESIAN_POINT ( 'NONE',  ( 34.42499999999998295, -9.022814304570511368, 5.000000000000000000 ) ) ;
#38295 = VERTEX_POINT ( 'NONE', #32838 ) ;
#38296 = CARTESIAN_POINT ( 'NONE',  ( 0.000000000000000000, 0.000000000000000000, 5.000000000000000000 ) ) ;
#38297 = CARTESIAN_POINT ( 'NONE',  ( 1.042387978378689350, 0.4000000000000001332, -2.015694669338588429 ) ) ;
#38298 = ORIENTED_EDGE ( 'NONE', *, *, #18622, .F. ) ;
#38299 = EDGE_CURVE ( 'NONE', #115217, #9024, #135, .T. ) ;
#38300 = ORIENTED_EDGE ( 'NONE', *, *, #16802, .T. ) ;
#38301 = CARTESIAN_POINT ( 'NONE',  ( -45.29974487139158867, -27.71228299555237840, 4.000000000000000000 ) ) ;
#38302 = EDGE_LOOP ( 'NONE', ( #97042, #109494, #44942, #11371, #28262, #53819 ) ) ;
#38303 = EDGE_CURVE ( 'NONE', #46717, #133314, #121935, .T. ) ;
#38304 = CARTESIAN_POINT ( 'NONE',  ( -13.82816939922343025, -11.24070752338416490, 4.000000000000000000 ) ) ;
#38305 = DIRECTION ( 'NONE',  ( -1.084202172485504434E-16, 1.000000000000000000, -0.000000000000000000 ) ) ;
#38306 = FACE_OUTER_BOUND ( 'NONE', #34669, .T. ) ;
#38307 = LINE ( 'NONE', #136179, #97288 ) ;
#38308 = APPLICATION_CONTEXT ( 'automotive_design' ) ;
#38309 = ORIENTED_EDGE ( 'NONE', *, *, #14043, .T. ) ;
#38310 = CARTESIAN_POINT ( 'NONE',  ( -42.48921356237308800, -27.52281430457085065, 5.000000000000000000 ) ) ;
#38311 = ORIENTED_EDGE ( 'NONE', *, *, #71843, .T. ) ;
#38312 = EDGE_CURVE ( 'NONE', #106292, #16078, #64021, .T. ) ;
#38313 = CARTESIAN_POINT ( 'NONE',  ( -30.18398860626900060, 28.73617430169808173, 5.000000000000000000 ) ) ;
#38314 = CARTESIAN_POINT ( 'NONE',  ( 31.42123647476855552, -9.717572351234235426E-16, -7.934999999999990727 ) ) ;
#38315 = LINE ( 'NONE', #126718, #114085 ) ;
#38316 = CARTESIAN_POINT ( 'NONE',  ( -24.48921356237309510, -27.52281430457072631, 5.000000000000000000 ) ) ;
#38317 = EDGE_CURVE ( 'NONE', #45614, #25787, #21926, .T. ) ;
#38318 = DIRECTION ( 'NONE',  ( -0.3543493200069162685, -0.000000000000000000, -0.9351131265310288487 ) ) ;
#38319 = ORIENTED_EDGE ( 'NONE', *, *, #90990, .T. ) ;
#38320 = EDGE_LOOP ( 'NONE', ( #84526, #102675, #116172, #70524 ) ) ;
#38321 = EDGE_LOOP ( 'NONE', ( #68185, #58659, #75406 ) ) ;
#38322 = DIRECTION ( 'NONE',  ( 1.369518533665900312E-16, -1.000000000000000000, 0.000000000000000000 ) ) ;
#38323 = CARTESIAN_POINT ( 'NONE',  ( 35.99451991528749772, 28.92564299267963079, 4.000000000000000000 ) ) ;
#38324 = CARTESIAN_POINT ( 'NONE',  ( -21.51665438641028771, 22.22500000000000142, 4.500000000000000888 ) ) ;
#38325 = DIRECTION ( 'NONE',  ( -0.7071067811865486830, -0.7071067811865464625, 0.000000000000000000 ) ) ;
#38326 = LINE ( 'NONE', #27417, #69436 ) ;
#38327 = DIRECTION ( 'NONE',  ( -0.000000000000000000, -0.3543493200069152693, 0.9351131265310292928 ) ) ;
#38328 = FACE_OUTER_BOUND ( 'NONE', #17764, .T. ) ;
#38329 = DIRECTION ( 'NONE',  ( -0.5735764363510503783, -0.8191520442889886899, 0.000000000000000000 ) ) ;
#38330 = PLANE ( 'NONE',  #21338 ) ;
#38331 = ORIENTED_EDGE ( 'NONE', *, *, #122441, .T. ) ;
#38332 = CARTESIAN_POINT ( 'NONE',  ( 74.20833333333331439, -3.974999999999999201, -6.884901960086287964 ) ) ;
#38333 = CARTESIAN_POINT ( 'NONE',  ( 0.000000000000000000, 9.735942053221458872E-16, -7.950000000000000178 ) ) ;
#38334 = ORIENTED_EDGE ( 'NONE', *, *, #5648, .T. ) ;
#38335 = DIRECTION ( 'NONE',  ( 0.7071067811865487940, 0.7071067811865463515, 0.000000000000000000 ) ) ;
#38338 = EDGE_CURVE ( 'NONE', #41122, #84504, #32099, .T. ) ;
#38337 = ORIENTED_EDGE ( 'NONE', *, *, #78503, .T. ) ;
#38336 = CARTESIAN_POINT ( 'NONE',  ( 55.56056557994602940, -52.00875322212549889, -39.86617647058820069 ) ) ;
#38339 = ORIENTED_EDGE ( 'NONE', *, *, #58467, .F. ) ;
#38340 = CARTESIAN_POINT ( 'NONE',  ( 34.92499999999998295, 22.22500000000000142, 4.000000000000000000 ) ) ;
#38341 = CARTESIAN_POINT ( 'NONE',  ( 0.000000000000000000, 0.000000000000000000, 5.000000000000000000 ) ) ;
#38342 = CARTESIAN_POINT ( 'NONE',  ( 32.24139925780183091, 21.72499999999999432, 5.000000000000000000 ) ) ;
#38343 = VERTEX_POINT ( 'NONE', #142308 ) ;
#38344 = ORIENTED_EDGE ( 'NONE', *, *, #29068, .T. ) ;
#38345 =( BOUNDED_CURVE ( )  B_SPLINE_CURVE ( 3, ( #62359, #127603, #6472, #40601 ),
 .UNSPECIFIED., .F., .T. ) 
 B_SPLINE_CURVE_WITH_KNOTS ( ( 4, 4 ),
 ( 2.779374508378133601, 4.199602562396796301 ),
 .UNSPECIFIED. ) 
 CURVE ( )  GEOMETRIC_REPRESENTATION_ITEM ( )  RATIONAL_B_SPLINE_CURVE ( ( 1.000000000000000000, 0.8388583629366717087, 0.8388583629366717087, 1.000000000000000000 ) ) 
 REPRESENTATION_ITEM ( '' )  );
#38346 = CARTESIAN_POINT ( 'NONE',  ( -15.29974487139158867, -27.71228299555216879, 4.000000000000000000 ) ) ;
#38347 = CARTESIAN_POINT ( 'NONE',  ( 0.5685132242927012358, 0.3999999999999995226, 2.467792535850613866 ) ) ;
#38348 = CIRCLE ( 'NONE', #86891, 2.500000000000000888 ) ;
#38349 = ADVANCED_FACE ( 'NONE', ( #42992 ), #98761, .F. ) ;
#38350 = CARTESIAN_POINT ( 'NONE',  ( 30.39126352523144448, -4.472830434245839371, -4.472830434245839371 ) ) ;
#38351 = CARTESIAN_POINT ( 'NONE',  ( 24.69524342170288023, 1.235879655689124501, 4.000000000000000000 ) ) ;
#38352 = CARTESIAN_POINT ( 'NONE',  ( 9.328169399223465774, -0.7407075233842753681, 4.000000000000000000 ) ) ;
#38353 = AXIS2_PLACEMENT_3D ( 'NONE', #35219, #50355, #28614 ) ;
#38354 = LINE ( 'NONE', #15141, #120856 ) ;
#38355 = PLANE ( 'NONE',  #111942 ) ;
#38356 = CARTESIAN_POINT ( 'NONE',  ( 0.7928932188134567571, -20.24070752338406720, 5.000000000000000000 ) ) ;
#38357 = CARTESIAN_POINT ( 'NONE',  ( 29.14540314143522437, -2.126176841940958351, -7.934999999999989839 ) ) ;
#38358 = CARTESIAN_POINT ( 'NONE',  ( 7.124569808101886892, -6.871911579029512218, 3.967499999999996252 ) ) ;
#38359 = LINE ( 'NONE', #126767, #96814 ) ;
#38360 = DIRECTION ( 'NONE',  ( 1.000000000000000000, 0.000000000000000000, 0.000000000000000000 ) ) ;
#38361 = DIRECTION ( 'NONE',  ( -1.000000000000000000, -2.666458015092512939E-14, 0.000000000000000000 ) ) ;
#38362 = ORIENTED_EDGE ( 'NONE', *, *, #32397, .F. ) ;
#38363 = EDGE_CURVE ( 'NONE', #96695, #49146, #62316, .T. ) ;
#38364 = ORIENTED_EDGE ( 'NONE', *, *, #139829, .T. ) ;
#38365 = CARTESIAN_POINT ( 'NONE',  ( 92.14583333333332860, 2.130196079827431976, -7.949999999999999289 ) ) ;
#38366 = EDGE_CURVE ( 'NONE', #125144, #9222, #46599, .T. ) ;
#38367 = EDGE_LOOP ( 'NONE', ( #79097, #132989, #18651, #126741 ) ) ;
#38368 = AXIS2_PLACEMENT_3D ( 'NONE', #105547, #81711, #125910 ) ;
#38369 = ORIENTED_EDGE ( 'NONE', *, *, #7099, .T. ) ;
#38370 = CARTESIAN_POINT ( 'NONE',  ( 22.35830628287043709, -1.633150327867709528, 6.094999999999979323 ) ) ;
#38371 = CARTESIAN_POINT ( 'NONE',  ( 30.41252705046289151, -7.949999999999998401, -4.867971026610728450E-16 ) ) ;
#38372 = VERTEX_POINT ( 'NONE', #45856 ) ;
#38373 = CARTESIAN_POINT ( 'NONE',  ( -21.48921356237309155, -27.52281430457070499, 5.000000000000000000 ) ) ;
#38374 = FACE_OUTER_BOUND ( 'NONE', #75061, .T. ) ;
#38375 = DIRECTION ( 'NONE',  ( 0.000000000000000000, -1.000000000000000000, 0.000000000000000000 ) ) ;
#38376 = CARTESIAN_POINT ( 'NONE',  ( 126.7939054748679411, 4.575466593308011198, 4.853590263963833529 ) ) ;
#38377 = ADVANCED_FACE ( 'NONE', ( #113208 ), #47997, .F. ) ;
#38378 = CARTESIAN_POINT ( 'NONE',  ( 12.70710678118645198, -12.74070752338415247, 5.000000000000000000 ) ) ;
#38379 = DIRECTION ( 'NONE',  ( 0.6830127018922180770, -0.6830127018922204085, -0.2588190451025213501 ) ) ;
#38380 = LINE ( 'NONE', #125397, #20199 ) ;
#38381 = PLANE ( 'NONE',  #142501 ) ;
#38382 = CARTESIAN_POINT ( 'NONE',  ( -39.48921356237310221, -27.52281430457082934, 5.000000000000000000 ) ) ;
#38383 = LINE ( 'NONE', #84734, #68337 ) ;
#38384 = CARTESIAN_POINT ( 'NONE',  ( -25.39999999999996305, 0.000000000000000000, 0.000000000000000000 ) ) ;
#38385 = AXIS2_PLACEMENT_3D ( 'NONE', #143227, #132391, #77986 ) ;
#38386 = SURFACE_STYLE_USAGE ( .BOTH. , #136258 ) ;
#38387 = ORIENTED_EDGE ( 'NONE', *, *, #3836, .F. ) ;
#38388 = VERTEX_POINT ( 'NONE', #100913 ) ;
#38389 = VECTOR ( 'NONE', #111861, 1000.000000000000227 ) ;
#38390 = CARTESIAN_POINT ( 'NONE',  ( 114.7712635252314186, 4.472830434245839371, 4.472830434245842035 ) ) ;
#38391 = ORIENTED_EDGE ( 'NONE', *, *, #16960, .T. ) ;
#38392 = VECTOR ( 'NONE', #114416, 1000.000000000000000 ) ;
#38393 = CARTESIAN_POINT ( 'NONE',  ( 30.48921356237309510, -27.52281430457076894, 5.000000000000000000 ) ) ;
#38394 = CIRCLE ( 'NONE', #84648, 3.000000000000002665 ) ;
#38395 = LINE ( 'NONE', #7137, #87441 ) ;
#38396 = ORIENTED_EDGE ( 'NONE', *, *, #100152, .T. ) ;
#38397 = LINE ( 'NONE', #136269, #88292 ) ;
#38398 = CARTESIAN_POINT ( 'NONE',  ( -29.20710678118633297, 3.759292476615681888, 5.000000000000000000 ) ) ;
#38399 = CARTESIAN_POINT ( 'NONE',  ( 104.9120968585647802, 5.291415217122921177, -3.054999999999994831 ) ) ;
#38400 = ORIENTED_EDGE ( 'NONE', *, *, #14577, .T. ) ;
#38401 = FACE_OUTER_BOUND ( 'NONE', #57701, .T. ) ;
#38402 = EDGE_CURVE ( 'NONE', #15535, #23113, #112512, .T. ) ;
#38403 = EDGE_LOOP ( 'NONE', ( #29368, #41304, #55537, #93281 ) ) ;
#38404 = DIRECTION ( 'NONE',  ( 0.7071067811865487940, 0.7071067811865463515, -0.000000000000000000 ) ) ;
#38405 =( NAMED_UNIT ( * ) PLANE_ANGLE_UNIT ( ) SI_UNIT ( $, .RADIAN. ) );
#38406 = CARTESIAN_POINT ( 'NONE',  ( 0.000000000000000000, 0.000000000000000000, 5.000000000000000000 ) ) ;
#38407 = EDGE_CURVE ( 'NONE', #91284, #9588, #13548, .T. ) ;
#38408 = EDGE_LOOP ( 'NONE', ( #29488, #122552 ) ) ;
#38409 = ORIENTED_EDGE ( 'NONE', *, *, #111033, .T. ) ;
#38410 = ORIENTED_EDGE ( 'NONE', *, *, #124910, .T. ) ;
#38411 = LINE ( 'NONE', #27507, #58463 ) ;
#38412 = EDGE_CURVE ( 'NONE', #97187, #4056, #90784, .T. ) ;
#38413 = CARTESIAN_POINT ( 'NONE',  ( 60.18398860626900415, 28.73617430169829490, 5.000000000000000000 ) ) ;
#38414 = CARTESIAN_POINT ( 'NONE',  ( 4.879569808101885897, 3.967499999999998916, 6.871911579029510442 ) ) ;
#38415 = LINE ( 'NONE', #67691, #10906 ) ;
#38416 = ADVANCED_FACE ( 'NONE', ( #14627 ), #13169, .T. ) ;
#38417 = ADVANCED_FACE ( 'NONE', ( #90032 ), #13880, .T. ) ;
#38418 = LINE ( 'NONE', #71064, #98672 ) ;
#38419 = EDGE_CURVE ( 'NONE', #75514, #53079, #102375, .T. ) ;
#38420 = ORIENTED_EDGE ( 'NONE', *, *, #119890, .F. ) ;
#38421 = ORIENTED_EDGE ( 'NONE', *, *, #80517, .F. ) ;
#38423 = ADVANCED_FACE ( 'NONE', ( #79219 ), #47316, .F. ) ;
#38422 = CARTESIAN_POINT ( 'NONE',  ( 11.99999999999992717, 4.384688058510579189, -7.090945410444659203 ) ) ;
#38424 = ORIENTED_EDGE ( 'NONE', *, *, #91524, .T. ) ;
#38425 = ORIENTED_EDGE ( 'NONE', *, *, #116212, .F. ) ;
#38426 = EDGE_CURVE ( 'NONE', #117264, #120537, #122391, .T. ) ;
#38427 = CARTESIAN_POINT ( 'NONE',  ( -15.32816939922343202, 8.259292476615637923, 4.000000000000000000 ) ) ;
#38428 = EDGE_CURVE ( 'NONE', #76586, #139177, #35710, .T. ) ;
#38429 = LINE ( 'NONE', #139188, #136873 ) ;
#38430 = PLANE ( 'NONE',  #49586 ) ;
#38431 = VERTEX_POINT ( 'NONE', #79932 ) ;
#38432 = DIRECTION ( 'NONE',  ( -0.000000000000000000, 0.3543493200069153248, 0.9351131265310292928 ) ) ;
#38433 = CARTESIAN_POINT ( 'NONE',  ( 27.00000000000001421, 3.441786896390103934, 7.166352137582786774 ) ) ;
#38434 =( NAMED_UNIT ( * ) PLANE_ANGLE_UNIT ( ) SI_UNIT ( $, .RADIAN. ) );
#38435 = FACE_OUTER_BOUND ( 'NONE', #141260, .T. ) ;
#38436 = ORIENTED_EDGE ( 'NONE', *, *, #91940, .T. ) ;
#38437 = EDGE_CURVE ( 'NONE', #104032, #73447, #91488, .T. ) ;
#38438 = CARTESIAN_POINT ( 'NONE',  ( -20.99451991528748707, 28.92564299267952777, 4.000000000000000000 ) ) ;
#38439 = FACE_BOUND ( 'NONE', #125602, .T. ) ;
#38440 = VERTEX_POINT ( 'NONE', #138556 ) ;
#38441 = DIRECTION ( 'NONE',  ( 0.7071067811865487940, -0.7071067811865463515, 0.000000000000000000 ) ) ;
#38442 = CARTESIAN_POINT ( 'NONE',  ( 2.999999999999981792, -6.412538124160691133, 4.000000000000000000 ) ) ;
#38443 = PRESENTATION_STYLE_ASSIGNMENT (( #15917 ) ) ;
#38444 = VERTEX_POINT ( 'NONE', #103746 ) ;
#38445 = PLANE ( 'NONE',  #108277 ) ;
#38446 = ORIENTED_EDGE ( 'NONE', *, *, #93622, .F. ) ;
#38447 = ORIENTED_EDGE ( 'NONE', *, *, #137560, .T. ) ;
#38448 = ADVANCED_FACE ( 'NONE', ( #26925 ), #71174, .F. ) ;
#38449 = ORIENTED_EDGE ( 'NONE', *, *, #78486, .T. ) ;
#38450 = AXIS2_PLACEMENT_3D ( 'NONE', #140582, #41272, #30415 ) ;
#38451 = CARTESIAN_POINT ( 'NONE',  ( 40.59959685856477307, -6.109999999999997655, -1.637169565754160283 ) ) ;
#38452 = EDGE_LOOP ( 'NONE', ( #107668, #1048, #111148, #66515, #29106, #118757 ) ) ;
#38453 = CARTESIAN_POINT ( 'NONE',  ( -32.99999999999977263, 15.45873954670181938, -0.03131636524286631612 ) ) ;
#38454 = PRESENTATION_STYLE_ASSIGNMENT (( #27545 ) ) ;
#38455 = PLANE ( 'NONE',  #75192 ) ;
#38456 = FILL_AREA_STYLE ('',( #24711 ) ) ;
#38457 = DIRECTION ( 'NONE',  ( 0.000000000000000000, -1.000000000000000000, 0.000000000000000000 ) ) ;
#38458 = DIRECTION ( 'NONE',  ( 1.000000000000000000, 0.000000000000000000, 0.000000000000000000 ) ) ;
#38459 = CARTESIAN_POINT ( 'NONE',  ( 8.999999999999937828, -18.03360074219755660, 5.000000000000000000 ) ) ;
#38460 = PLANE ( 'NONE',  #143194 ) ;
#38461 = DIRECTION ( 'NONE',  ( 0.7071067811865487940, 0.7071067811865463515, 0.000000000000000000 ) ) ;
#38462 = STYLED_ITEM ( 'NONE', ( #49625 ), #33428 ) ;
#38463 = ORIENTED_EDGE ( 'NONE', *, *, #57389, .F. ) ;
#38464 = EDGE_CURVE ( 'NONE', #46474, #82404, #33323, .T. ) ;
#38465 = EDGE_LOOP ( 'NONE', ( #120071, #127971, #132759, #38091 ) ) ;
#38466 = ORIENTED_EDGE ( 'NONE', *, *, #8145, .F. ) ;
#38467 = ORIENTED_EDGE ( 'NONE', *, *, #119590, .F. ) ;
#38468 = ORIENTED_EDGE ( 'NONE', *, *, #94742, .F. ) ;
#38469 = EDGE_CURVE ( 'NONE', #40590, #42487, #62938, .T. ) ;
#38470 = EDGE_LOOP ( 'NONE', ( #9225, #28071 ) ) ;
#38471 = CARTESIAN_POINT ( 'NONE',  ( -22.49999999999984723, 10.94296225409024537, -9.576120664313309661 ) ) ;
#38472 = CARTESIAN_POINT ( 'NONE',  ( -75.18398860626899705, 28.73617430169839793, 5.000000000000000000 ) ) ;
#38473 = CONICAL_SURFACE ( 'NONE', #59405, 2.055000000000001048, 0.9599310885968758145 ) ;
#38474 = CARTESIAN_POINT ( 'NONE',  ( 12.27825451568565640, 8.259292476615634371, 11.78515199841153205 ) ) ;
#38475 = VERTEX_POINT ( 'NONE', #71894 ) ;
#38476 = DIRECTION ( 'NONE',  ( 0.000000000000000000, -1.000000000000000000, 0.000000000000000000 ) ) ;
#38477 = EDGE_LOOP ( 'NONE', ( #111533, #35013, #78287, #121200 ) ) ;
#38478 = EDGE_CURVE ( 'NONE', #14737, #96111, #105198, .T. ) ;
#38479 = VECTOR ( 'NONE', #85811, 1000.000000000000000 ) ;
#38480 = DIRECTION ( 'NONE',  ( -1.000000000000000000, 0.000000000000000000, 0.000000000000000000 ) ) ;
#38481 = CARTESIAN_POINT ( 'NONE',  ( 34.92499999999998295, 8.718490437204167165, 4.759050581649327150 ) ) ;
#38482 = AXIS2_PLACEMENT_3D ( 'NONE', #92049, #50706, #137005 ) ;
#38483 = CARTESIAN_POINT ( 'NONE',  ( 1.525403141435219379, 2.126176841940962348, 7.934999999999989839 ) ) ;
#38484 = ORIENTED_EDGE ( 'NONE', *, *, #104183, .T. ) ;
#38486 = LINE ( 'NONE', #27585, #75436 ) ;
#38485 = CARTESIAN_POINT ( 'NONE',  ( 98.05793019189812298, 6.110000000000001208, -1.637169565754156286 ) ) ;
#38487 = VECTOR ( 'NONE', #42855, 1000.000000000000000 ) ;
#38489 = EDGE_CURVE ( 'NONE', #44445, #42198, #18900, .T. ) ;
#38488 = CARTESIAN_POINT ( 'NONE',  ( 45.18398860626900415, 28.73617430169818832, 5.000000000000000000 ) ) ;
#38490 = CARTESIAN_POINT ( 'NONE',  ( 26.70025512860841488, -27.71228299555187391, 4.000000000000000000 ) ) ;
#38491 = VERTEX_POINT ( 'NONE', #48690 ) ;
#38492 = ORIENTED_EDGE ( 'NONE', *, *, #131837, .T. ) ;
#38493 = LINE ( 'NONE', #82714, #77422 ) ;
#38494 = ORIENTED_EDGE ( 'NONE', *, *, #89612, .T. ) ;
#38495 = SURFACE_STYLE_USAGE ( .BOTH. , #137819 ) ;
#38496 = DIRECTION ( 'NONE',  ( -0.000000000000000000, 0.3543493200069153248, 0.9351131265310292928 ) ) ;
#38497 = AXIS2_PLACEMENT_3D ( 'NONE', #49262, #136953, #81903 ) ;
#38498 = DIRECTION ( 'NONE',  ( 0.7071067811865487940, 0.7071067811865463515, -0.000000000000000000 ) ) ;
#38499 = CARTESIAN_POINT ( 'NONE',  ( 184.0378153480262711, -51.37040454773214293, -37.49526731630776055 ) ) ;
#38500 = VERTEX_POINT ( 'NONE', #116068 ) ;
#38501 = CARTESIAN_POINT ( 'NONE',  ( -33.18398860626899705, 28.73617430169810305, 5.000000000000000000 ) ) ;
#38502 = CARTESIAN_POINT ( 'NONE',  ( 24.48921356237309510, -27.52281430457072631, 5.000000000000000000 ) ) ;
#38503 = PLANE ( 'NONE',  #83877 ) ;
#38504 = ORIENTED_EDGE ( 'NONE', *, *, #14057, .F. ) ;
#38505 = LINE ( 'NONE', #105866, #118383 ) ;
#38506 = LINE ( 'NONE', #50810, #33191 ) ;
#38507 = ORIENTED_EDGE ( 'NONE', *, *, #49867, .F. ) ;
#38510 = EDGE_CURVE ( 'NONE', #30925, #14772, #106592, .T. ) ;
#38509 = ORIENTED_EDGE ( 'NONE', *, *, #58939, .F. ) ;
#38508 = CARTESIAN_POINT ( 'NONE',  ( 42.18398860626899705, 28.73617430169816700, 5.000000000000000000 ) ) ;
#38511 = EDGE_CURVE ( 'NONE', #93121, #121113, #82751, .T. ) ;
#38512 = VERTEX_POINT ( 'NONE', #126250 ) ;
#38513 = LINE ( 'NONE', #6534, #93333 ) ;
#38514 = ORIENTED_EDGE ( 'NONE', *, *, #138110, .T. ) ;
#38515 = CARTESIAN_POINT ( 'NONE',  ( 51.48921356237309510, -27.52281430457091460, 5.000000000000000000 ) ) ;
#38516 =( NAMED_UNIT ( * ) SI_UNIT ( $, .STERADIAN. ) SOLID_ANGLE_UNIT ( ) );
#38517 = CARTESIAN_POINT ( 'NONE',  ( -34.42500000000001137, 17.97718569542923106, 5.000000000000000000 ) ) ;
#38518 = ORIENTED_EDGE ( 'NONE', *, *, #117089, .T. ) ;
#38519 = DIRECTION ( 'NONE',  ( -1.000000000000000000, -3.115803279706882722E-16, 0.000000000000000000 ) ) ;
#38520 = CARTESIAN_POINT ( 'NONE',  ( -33.71230993966005940, -21.73547319004781642, 4.999917730833664642 ) ) ;
#38521 = DIRECTION ( 'NONE',  ( -0.7071067811865486830, -0.7071067811865464625, 0.000000000000000000 ) ) ;
#38522 = CARTESIAN_POINT ( 'NONE',  ( 2.021013337047029346, 2.847195794450450457, -5.394070523059989242 ) ) ;
#38523 = DIRECTION ( 'NONE',  ( 0.6830127018922180770, -0.6830127018922204085, -0.2588190451025213501 ) ) ;
#38525 = VECTOR ( 'NONE', #15343, 1000.000000000000000 ) ;
#38524 = LINE ( 'NONE', #95017, #35139 ) ;
#38526 = CARTESIAN_POINT ( 'NONE',  ( 5.816011393731002066, 28.73617430169783304, 5.000000000000000000 ) ) ;
#38527 = CARTESIAN_POINT ( 'NONE',  ( 29.53752705046289151, -9.735942053221456900E-16, 7.949999999999998401 ) ) ;
#38528 = EDGE_CURVE ( 'NONE', #115259, #124700, #116789, .T. ) ;
#38529 = DIRECTION ( 'NONE',  ( -0.000000000000000000, -0.3543493200069152693, 0.9351131265310292928 ) ) ;
#38530 = VERTEX_POINT ( 'NONE', #95751 ) ;
#38531 = ADVANCED_FACE ( 'NONE', ( #83464 ), #139293, .T. ) ;
#38532 = EDGE_LOOP ( 'NONE', ( #5436, #14277, #128183, #72667 ) ) ;
#38533 = ORIENTED_EDGE ( 'NONE', *, *, #69838, .T. ) ;
#38534 = CARTESIAN_POINT ( 'NONE',  ( 124.0833333333333428, 6.884901960086290629, -3.974999999999994316 ) ) ;
#38535 = ADVANCED_FACE ( 'NONE', ( #28373 ), #17471, .F. ) ;
#38536 = ORIENTED_EDGE ( 'NONE', *, *, #48782, .F. ) ;
#38537 = ORIENTED_EDGE ( 'NONE', *, *, #74661, .F. ) ;
#38538 = VERTEX_POINT ( 'NONE', #49435 ) ;
#38539 = VECTOR ( 'NONE', #69955, 1000.000000000000000 ) ;
#38540 = DIRECTION ( 'NONE',  ( 0.000000000000000000, 0.000000000000000000, -1.000000000000000000 ) ) ;
#38541 = PLANE ( 'NONE',  #2209 ) ;
#38542 = VERTEX_POINT ( 'NONE', #40675 ) ;
#38543 = DIRECTION ( 'NONE',  ( 0.7071067811865486830, -0.7071067811865464625, -0.000000000000000000 ) ) ;
#38544 = PLANE ( 'NONE',  #74112 ) ;
#38545 = DIRECTION ( 'NONE',  ( 0.3543493200069162685, -0.000000000000000000, -0.9351131265310288487 ) ) ;
#38546 = FACE_OUTER_BOUND ( 'NONE', #129315, .T. ) ;
#38547 = CARTESIAN_POINT ( 'NONE',  ( 110.2504301918981042, 3.055000000000002824, -5.291415217122919401 ) ) ;
#38548 = ORIENTED_EDGE ( 'NONE', *, *, #123410, .T. ) ;
#38549 = EDGE_CURVE ( 'NONE', #16129, #121292, #93624, .T. ) ;
#38550 = DIRECTION ( 'NONE',  ( -0.7071067811865487940, 0.7071067811865463515, -0.000000000000000000 ) ) ;
#38551 = CARTESIAN_POINT ( 'NONE',  ( -24.70710678118637205, 5.259292476615659240, 5.000000000000000000 ) ) ;
#38552 = CARTESIAN_POINT ( 'NONE',  ( -69.29974487139159578, -27.71228299555254537, 4.000000000000000000 ) ) ;
#38553 = CARTESIAN_POINT ( 'NONE',  ( -48.48921356237309510, -27.52281430457089328, 5.000000000000000000 ) ) ;
#38554 = FACE_OUTER_BOUND ( 'NONE', #125043, .T. ) ;
#38555 = CARTESIAN_POINT ( 'NONE',  ( 33.76669371712955581, -7.949999999999999289, 2.130196079827424427 ) ) ;
#38556 = VECTOR ( 'NONE', #76440, 999.9999999999998863 ) ;
#38557 = CARTESIAN_POINT ( 'NONE',  ( 4.499999999999962697, -5.568876922607757685, 4.000000000000000000 ) ) ;
#38558 = ORIENTED_EDGE ( 'NONE', *, *, #123510, .F. ) ;
#38559 = ORIENTED_EDGE ( 'NONE', *, *, #451, .T. ) ;
#38560 = CARTESIAN_POINT ( 'NONE',  ( 32.64583333333332860, 2.130196079827431976, -7.949999999999999289 ) ) ;
#38561 = AXIS2_PLACEMENT_3D ( 'NONE', #82463, #83171, #104168 ) ;
#38562 = ORIENTED_EDGE ( 'NONE', *, *, #101526, .T. ) ;
#38563 = LINE ( 'NONE', #92934, #48321 ) ;
#38564 = CARTESIAN_POINT ( 'NONE',  ( 24.32816939922336275, 11.25929247661560062, 4.000000000000000000 ) ) ;
#38565 = EDGE_LOOP ( 'NONE', ( #18845, #15778, #137760, #47257 ) ) ;
#38566 = DIRECTION ( 'NONE',  ( -0.6830127018922180770, -0.6830127018922204085, -0.2588190451025213501 ) ) ;
#38567 = DIRECTION ( 'NONE',  ( 0.000000000000000000, 0.000000000000000000, -1.000000000000000000 ) ) ;
#38568 = PLANE ( 'NONE',  #97579 ) ;
#38569 = LINE ( 'NONE', #18950, #134500 ) ;
#38570 = CARTESIAN_POINT ( 'NONE',  ( 33.10459685856476852, 1.637169565754164946, -6.109999999999999432 ) ) ;
#38572 = ORIENTED_EDGE ( 'NONE', *, *, #58584, .F. ) ;
#38571 = CIRCLE ( 'NONE', #33922, 2.500000000000000444 ) ;
#38573 = CARTESIAN_POINT ( 'NONE',  ( 15.48921356237309510, -27.52281430457066236, 5.000000000000000000 ) ) ;
#38574 = VERTEX_POINT ( 'NONE', #128399 ) ;
#38575 = DIRECTION ( 'NONE',  ( 1.000000000000000000, 0.000000000000000000, 0.000000000000000000 ) ) ;
#38576 = DIRECTION ( 'NONE',  ( 0.3543493200069162685, -0.000000000000000000, -0.9351131265310288487 ) ) ;
#38577 = CARTESIAN_POINT ( 'NONE',  ( -12.69999999999998153, 0.000000000000000000, 2.500000000000000444 ) ) ;
#38578 = CARTESIAN_POINT ( 'NONE',  ( 30.18398860626900060, 28.73617430169808173, 5.000000000000000000 ) ) ;
#38579 = EDGE_LOOP ( 'NONE', ( #101857, #57846, #94193, #110149 ) ) ;
#38580 = VECTOR ( 'NONE', #74436, 999.9999999999998863 ) ;
#38581 = CARTESIAN_POINT ( 'NONE',  ( 58.62543019189810423, 5.291415217122919401, 3.055000000000002824 ) ) ;
#38582 = ORIENTED_EDGE ( 'NONE', *, *, #130448, .F. ) ;
#38583 = CARTESIAN_POINT ( 'NONE',  ( -8.999999999999932498, 20.70535890316560312, 1.956823837851937142 ) ) ;
#38584 = LINE ( 'NONE', #61109, #141121 ) ;
#38585 = LINE ( 'NONE', #71960, #24600 ) ;
#38586 = DIRECTION ( 'NONE',  ( 0.6830127018922180770, -0.6830127018922204085, -0.2588190451025213501 ) ) ;
#38587 = VECTOR ( 'NONE', #32353, 1000.000000000000000 ) ;
#38588 = AXIS2_PLACEMENT_3D ( 'NONE', #29300, #31461, #64807 ) ;
#38590 = EDGE_CURVE ( 'NONE', #111481, #51650, #29075, .T. ) ;
#38589 = AXIS2_PLACEMENT_3D ( 'NONE', #104875, #60708, #5540 ) ;
#38591 = CARTESIAN_POINT ( 'NONE',  ( 47.59959685856478018, -6.109999999999997655, -1.637169565754160283 ) ) ;
#38592 = EDGE_CURVE ( 'NONE', #141405, #115416, #74013, .T. ) ;
#38594 = EDGE_CURVE ( 'NONE', #12864, #59481, #109489, .T. ) ;
#38593 = ORIENTED_EDGE ( 'NONE', *, *, #74351, .F. ) ;
#38595 = CARTESIAN_POINT ( 'NONE',  ( -25.39999999999996305, 0.000000000000000000, 0.000000000000000000 ) ) ;
#38597 = ADVANCED_FACE ( 'NONE', ( #87026 ), #142142, .F. ) ;
#38596 = DIRECTION ( 'NONE',  ( -0.3543493200069162685, -0.000000000000000000, -0.9351131265310288487 ) ) ;
#38598 = ORIENTED_EDGE ( 'NONE', *, *, #42840, .T. ) ;
#38599 = EDGE_LOOP ( 'NONE', ( #32603, #13670, #31014, #54651 ) ) ;
#38600 = AXIS2_PLACEMENT_3D ( 'NONE', #116625, #73149, #5695 ) ;
#38601 = DIRECTION ( 'NONE',  ( 0.7071067811865486830, -0.7071067811865464625, -0.000000000000000000 ) ) ;
#38602 = VERTEX_POINT ( 'NONE', #85577 ) ;
#38603 = EDGE_CURVE ( 'NONE', #69752, #54027, #44254, .T. ) ;
#38604 = CARTESIAN_POINT ( 'NONE',  ( -62.99451991528749772, 28.92564299267982264, 4.000000000000000000 ) ) ;
#38605 = PRODUCT_DEFINITION_CONTEXT ( 'detailed design', #50377, 'design' ) ;
#38606 = ORIENTED_EDGE ( 'NONE', *, *, #28178, .T. ) ;
#38607 = EDGE_CURVE ( 'NONE', #129409, #107840, #129806, .T. ) ;
#38608 =( NAMED_UNIT ( * ) PLANE_ANGLE_UNIT ( ) SI_UNIT ( $, .RADIAN. ) );
#38609 = ADVANCED_FACE ( 'NONE', ( #74748 ), #119617, .F. ) ;
#38610 = FACE_BOUND ( 'NONE', #28270, .T. ) ;
#38611 = EDGE_CURVE ( 'NONE', #56532, #143089, #98603, .T. ) ;
#38612 = LINE ( 'NONE', #50209, #54910 ) ;
#38613 = DIRECTION ( 'NONE',  ( -0.7071067811865486830, -0.7071067811865464625, -0.000000000000000000 ) ) ;
#38614 = ORIENTED_EDGE ( 'NONE', *, *, #88597, .F. ) ;
#38615 =( NAMED_UNIT ( * ) SI_UNIT ( $, .STERADIAN. ) SOLID_ANGLE_UNIT ( ) );
#38617 = VERTEX_POINT ( 'NONE', #10165 ) ;
#38616 = LINE ( 'NONE', #16865, #43537 ) ;
#38618 = ORIENTED_EDGE ( 'NONE', *, *, #91183, .F. ) ;
#38619 = DIRECTION ( 'NONE',  ( 0.3543493200069162685, -0.000000000000000000, -0.9351131265310288487 ) ) ;
#38620 = EDGE_CURVE ( 'NONE', #13692, #71393, #87739, .T. ) ;
#38621 = EDGE_LOOP ( 'NONE', ( #66517, #41456, #102532, #18469, #111589, #126857 ) ) ;
#38622 = VERTEX_POINT ( 'NONE', #32657 ) ;
#38623 = CARTESIAN_POINT ( 'NONE',  ( 70.05793019189810877, 6.110000000000000320, -1.637169565754156064 ) ) ;
#38624 = VECTOR ( 'NONE', #49199, 1000.000000000000000 ) ;
#38625 = ORIENTED_EDGE ( 'NONE', *, *, #75626, .T. ) ;
#38626 = CARTESIAN_POINT ( 'NONE',  ( -13.49999999999990763, 7.087461875839172087, 4.000000000000000000 ) ) ;
#38627 = PLANE ( 'NONE',  #68184 ) ;
#38628 = ORIENTED_EDGE ( 'NONE', *, *, #7147, .T. ) ;
#38629 = CARTESIAN_POINT ( 'NONE',  ( 174.7500000000000000, 7.919999999999947526, -16.42230000000009227 ) ) ;
#38630 = EDGE_CURVE ( 'NONE', #88501, #97476, #96430, .T. ) ;
#38631 = VECTOR ( 'NONE', #110214, 1000.000000000000000 ) ;
#38632 = CARTESIAN_POINT ( 'NONE',  ( 25.39999999999999858, 7.796566843815467607, 1.475727091950665537 ) ) ;
#38633 = CARTESIAN_POINT ( 'NONE',  ( -12.51665438641036410, 22.22500000000000142, 4.500000000000000888 ) ) ;
#38634 = CARTESIAN_POINT ( 'NONE',  ( -0.005480084712502889671, 28.92564299267938210, 4.000000000000000000 ) ) ;
#38635 = CARTESIAN_POINT ( 'NONE',  ( 16.77083333333333570, 6.094999999999991758, 1.633150327867686880 ) ) ;
#38636 = CARTESIAN_POINT ( 'NONE',  ( -39.18398860626899705, 28.73617430169814568, 5.000000000000000000 ) ) ;
#38637 = VERTEX_POINT ( 'NONE', #118927 ) ;
#38638 = EDGE_CURVE ( 'NONE', #11170, #118704, #65301, .T. ) ;
#38639 = MECHANICAL_DESIGN_GEOMETRIC_PRESENTATION_REPRESENTATION (  '', ( #101126 ), #3809 ) ;
#38640 = ORIENTED_EDGE ( 'NONE', *, *, #99267, .T. ) ;
#38641 = LINE ( 'NONE', #82174, #5613 ) ;
#38642 = CARTESIAN_POINT ( 'NONE',  ( 33.48921356237309510, -27.52281430457078670, 5.000000000000000000 ) ) ;
#38643 = VERTEX_POINT ( 'NONE', #88469 ) ;
#38644 = EDGE_LOOP ( 'NONE', ( #1906, #17047, #31666, #140005 ) ) ;
#38645 = ORIENTED_EDGE ( 'NONE', *, *, #76580, .T. ) ;
#38646 = DIRECTION ( 'NONE',  ( -0.000000000000000000, 0.3543493200069153248, 0.9351131265310292928 ) ) ;
#38647 = AXIS2_PLACEMENT_3D ( 'NONE', #23986, #26828, #57354 ) ;
#38648 = DIRECTION ( 'NONE',  ( 0.000000000000000000, 0.000000000000000000, -1.000000000000000000 ) ) ;
#38649 = EDGE_LOOP ( 'NONE', ( #104791, #78361, #124925, #20546 ) ) ;
#38650 = CARTESIAN_POINT ( 'NONE',  ( -32.29289321881322650, 5.259292476615659240, 5.000000000000000000 ) ) ;
#38651 = EDGE_CURVE ( 'NONE', #140112, #25422, #19618, .T. ) ;
#38652 = AXIS2_PLACEMENT_3D ( 'NONE', #66804, #24715, #68968 ) ;
#38653 = FACE_OUTER_BOUND ( 'NONE', #54206, .T. ) ;
#38654 = CARTESIAN_POINT ( 'NONE',  ( 7.504569808101886785, 6.871911579029510442, -3.967499999999998916 ) ) ;
#38655 = DIRECTION ( 'NONE',  ( 1.000000000000000000, 0.000000000000000000, 0.000000000000000000 ) ) ;
#38656 = ORIENTED_EDGE ( 'NONE', *, *, #28532, .F. ) ;
#38657 = VECTOR ( 'NONE', #100305, 1000.000000000000227 ) ;
#38658 = CARTESIAN_POINT ( 'NONE',  ( 0.000000000000000000, 0.000000000000000000, 5.000000000000000000 ) ) ;
#38660 = EDGE_CURVE ( 'NONE', #27268, #126942, #42115, .T. ) ;
#38659 = LINE ( 'NONE', #96560, #113670 ) ;
#38661 = FACE_OUTER_BOUND ( 'NONE', #124710, .T. ) ;
#38663 = ORIENTED_EDGE ( 'NONE', *, *, #142251, .F. ) ;
#38662 = LINE ( 'NONE', #128532, #116588 ) ;
#38664 = CARTESIAN_POINT ( 'NONE',  ( 10.39997294953710494, 4.461849672132297329, -4.461849672132302658 ) ) ;
#38665 = ORIENTED_EDGE ( 'NONE', *, *, #43998, .F. ) ;
#38666 = CARTESIAN_POINT ( 'NONE',  ( 7.499999999999954703, 22.08746187583901133, 4.000000000000000000 ) ) ;
#38667 = CARTESIAN_POINT ( 'NONE',  ( -29.99999999999979039, 7.931123077392108200, 4.000000000000000000 ) ) ;
#38668 = CARTESIAN_POINT ( 'NONE',  ( 109.5000000000000000, 0.000000000000000000, -7.950000000000000178 ) ) ;
#38669 = ORIENTED_EDGE ( 'NONE', *, *, #54328, .T. ) ;
#38670 = EDGE_CURVE ( 'NONE', #6460, #15180, #76895, .T. ) ;
#38671 = DIRECTION ( 'NONE',  ( 1.000000000000000000, 0.000000000000000000, 0.000000000000000000 ) ) ;
#38672 = DIRECTION ( 'NONE',  ( -0.7071067811865486830, -0.7071067811865464625, 0.000000000000000000 ) ) ;
#38673 = PLANE ( 'NONE',  #60707 ) ;
#38674 = EDGE_LOOP ( 'NONE', ( #39969, #111531, #35340, #110994 ) ) ;
#38675 = CARTESIAN_POINT ( 'NONE',  ( 42.48921356237308800, -27.52281430457085065, 5.000000000000000000 ) ) ;
#38676 = LINE ( 'NONE', #95899, #107172 ) ;
#38677 = LINE ( 'NONE', #57597, #40025 ) ;
#38678 = DIRECTION ( 'NONE',  ( 0.7071067811865487940, 0.7071067811865463515, 0.000000000000000000 ) ) ;
#38679 = COLOUR_RGB ( '', 0.66274510, 0.83137255, 0.94901961) ;
#38680 = CARTESIAN_POINT ( 'NONE',  ( -51.29974487139158867, -27.71228299555242103, 4.000000000000000000 ) ) ;
#38682 = EDGE_CURVE ( 'NONE', #13957, #126797, #110181, .T. ) ;
#38681 = EDGE_LOOP ( 'NONE', ( #52025, #18100, #113974, #15372 ) ) ;
#38683 = EDGE_CURVE ( 'NONE', #24873, #42879, #73776, .T. ) ;
#38684 = VERTEX_POINT ( 'NONE', #42827 ) ;
#38685 = DIRECTION ( 'NONE',  ( -0.7071067811865486830, -0.7071067811865464625, -0.000000000000000000 ) ) ;
#38686 = CARTESIAN_POINT ( 'NONE',  ( 5.281315875828549444, 4.584330080086930965E-16, 0.000000000000000000 ) ) ;
#38687 = AXIS2_PLACEMENT_3D ( 'NONE', #127941, #115569, #5400 ) ;
#38688 = VECTOR ( 'NONE', #85642, 1000.000000000000000 ) ;
#38689 = CARTESIAN_POINT ( 'NONE',  ( 4.937069808101886892, 2.126176841940952134, -7.934999999999993392 ) ) ;
#38690 = FACE_OUTER_BOUND ( 'NONE', #106244, .T. ) ;
#38691 = DIRECTION ( 'NONE',  ( 0.7071067811865487940, 0.7071067811865463515, -0.000000000000000000 ) ) ;
#38692 = DIRECTION ( 'NONE',  ( 0.000000000000000000, 0.000000000000000000, 1.000000000000000000 ) ) ;
#38693 = DIRECTION ( 'NONE',  ( 0.7071067811865487940, -0.7071067811865463515, 0.000000000000000000 ) ) ;
#38694 = ORIENTED_EDGE ( 'NONE', *, *, #94408, .F. ) ;
#38695 = CARTESIAN_POINT ( 'NONE',  ( -18.18398860626898994, 28.73617430169800002, 5.000000000000000000 ) ) ;
#38696 = AXIS2_PLACEMENT_3D ( 'NONE', #142687, #141997, #64408 ) ;
#38697 = FACE_OUTER_BOUND ( 'NONE', #94294, .T. ) ;
#38698 = AXIS2_PLACEMENT_3D ( 'NONE', #96639, #140197, #83700 ) ;
#38699 = DIRECTION ( 'NONE',  ( 0.7071067811865487940, 0.7071067811865463515, 0.000000000000000000 ) ) ;
#38700 = CARTESIAN_POINT ( 'NONE',  ( 51.09959685856477307, -6.109999999999998543, -1.637169565754160727 ) ) ;
#38701 = CARTESIAN_POINT ( 'NONE',  ( 4.828169399223504854, 6.759292476615653023, 4.000000000000000000 ) ) ;
#38702 = ORIENTED_EDGE ( 'NONE', *, *, #81716, .F. ) ;
#38703 =( LENGTH_UNIT ( ) NAMED_UNIT ( * ) SI_UNIT ( .MILLI., .METRE. ) );
#38704 = ADVANCED_FACE ( 'NONE', ( #107339 ), #108736, .F. ) ;
#38705 = EDGE_LOOP ( 'NONE', ( #65913, #23715, #130498 ) ) ;
#38706 = ORIENTED_EDGE ( 'NONE', *, *, #21840, .F. ) ;
#38707 = CARTESIAN_POINT ( 'NONE',  ( 14.20710678118645021, 18.75929247661552068, 5.000000000000000000 ) ) ;
#38708 = LINE ( 'NONE', #27825, #110999 ) ;
#38709 = DIRECTION ( 'NONE',  ( -1.000000000000000000, -1.224606353822377258E-16, -0.000000000000000000 ) ) ;
#38710 = DIRECTION ( 'NONE',  ( -0.6830127018922181881, 0.6830127018922202975, -0.2588190451025214056 ) ) ;
#38711 = EDGE_CURVE ( 'NONE', #26635, #81537, #75445, .T. ) ;
#38712 = LINE ( 'NONE', #19092, #97382 ) ;
#38713 = CARTESIAN_POINT ( 'NONE',  ( 36.48921356237310221, -27.52281430457080802, 5.000000000000000000 ) ) ;
#38714 = ORIENTED_EDGE ( 'NONE', *, *, #6047, .T. ) ;
#38715 = EDGE_CURVE ( 'NONE', #9875, #81835, #86327, .T. ) ;
#38716 = CARTESIAN_POINT ( 'NONE',  ( 1.720058664033062845, 0.4644975210628944362, -6.362334081593164825 ) ) ;
#38717 = FACE_OUTER_BOUND ( 'NONE', #136864, .T. ) ;
#38718 = UNCERTAINTY_MEASURE_WITH_UNIT (LENGTH_MEASURE( 1.000000000000000082E-05 ), #75788, 'distance_accuracy_value', 'NONE');
#38719 = AXIS2_PLACEMENT_3D ( 'NONE', #119045, #110291, #129936 ) ;
#38720 = LINE ( 'NONE', #83680, #17721 ) ;
#38721 = DIRECTION ( 'NONE',  ( -0.000000000000000000, -0.000000000000000000, 1.000000000000000000 ) ) ;
#38722 = FACE_OUTER_BOUND ( 'NONE', #43552, .T. ) ;
#38723 = CARTESIAN_POINT ( 'NONE',  ( 64.97502705046288440, -5.819803920172572198, 5.819803920172572198 ) ) ;
#38724 = AXIS2_PLACEMENT_3D ( 'NONE', #59813, #82985, #71397 ) ;
#38725 = FACE_OUTER_BOUND ( 'NONE', #75362, .T. ) ;
#38726 = EDGE_LOOP ( 'NONE', ( #138055, #111813, #137569, #98409 ) ) ;
#38727 = ORIENTED_EDGE ( 'NONE', *, *, #74764, .T. ) ;
#38728 =( BOUNDED_CURVE ( )  B_SPLINE_CURVE ( 2, ( #21312, #65570, #109739, #10409, #54669, #132241, #121323, #32933, #19866, #140241, #85130, #8943, #30026 ),
 .UNSPECIFIED., .F., .T. ) 
 B_SPLINE_CURVE_WITH_KNOTS ( ( 3, 2, 2, 2, 2, 2, 3 ),
 ( 0.8333333333333333703, 0.8361111111111111382, 0.8388888888888889062, 0.8416666666666666741, 0.8444444444444444420, 0.8472222222222222099, 0.8499999999999999778 ),
 .UNSPECIFIED. ) 
 CURVE ( )  GEOMETRIC_REPRESENTATION_ITEM ( )  RATIONAL_B_SPLINE_CURVE ( ( 1.000000000000000000, 0.9659258262890683122, 1.000000000000000000, 0.9659258262890683122, 1.000000000000000000, 0.9659258262890683122, 1.000000000000000000, 0.9659258262890683122, 1.000000000000000000, 0.9659258262890683122, 1.000000000000000000, 0.9659258262890683122, 1.000000000000000000 ) ) 
 REPRESENTATION_ITEM ( '' )  );
#38729 = CARTESIAN_POINT ( 'NONE',  ( 66.33333333333332860, -6.884901960086287964, 3.974999999999998312 ) ) ;
#38730 = CARTESIAN_POINT ( 'NONE',  ( 2.510786437626908008, -27.52281430457053446, 5.000000000000000000 ) ) ;
#38731 = DIRECTION ( 'NONE',  ( -0.000000000000000000, -0.000000000000000000, -1.000000000000000000 ) ) ;
#38732 =( GEOMETRIC_REPRESENTATION_CONTEXT ( 3 ) GLOBAL_UNCERTAINTY_ASSIGNED_CONTEXT ( ( #94307 ) ) GLOBAL_UNIT_ASSIGNED_CONTEXT ( ( #16617, #117343, #106455 ) ) REPRESENTATION_CONTEXT ( 'NONE', 'WORKASPACE' ) );
#38733 = VERTEX_POINT ( 'NONE', #92011 ) ;
#38734 = ADVANCED_FACE ( 'NONE', ( #67439 ), #23921, .T. ) ;
#38735 = CARTESIAN_POINT ( 'NONE',  ( 127.2530914712157113, -1.701477371937629046, -6.349999999999998757 ) ) ;
#38736 = DIRECTION ( 'NONE',  ( -0.000000000000000000, -0.3543493200069152693, 0.9351131265310292928 ) ) ;
#38737 = CARTESIAN_POINT ( 'NONE',  ( 55.41709685856477563, 3.054999999999998828, 5.291415217122922066 ) ) ;
#38738 = VECTOR ( 'NONE', #11578, 1000.000000000000000 ) ;
#38739 = CYLINDRICAL_SURFACE ( 'NONE', #143195, 9.500000000000001776 ) ;
#38740 = EDGE_LOOP ( 'NONE', ( #123792, #23276, #105000, #60656 ) ) ;
#38741 = VERTEX_POINT ( 'NONE', #123246 ) ;
#38742 = CARTESIAN_POINT ( 'NONE',  ( -12.48921356237309155, -27.52281430457064104, 5.000000000000000000 ) ) ;
#38743 = CARTESIAN_POINT ( 'NONE',  ( 19.41972383043609440, 4.584330080086930965E-16, 0.000000000000000000 ) ) ;
#38744 = DIRECTION ( 'NONE',  ( -0.000000000000000000, -0.3543493200069152693, 0.9351131265310292928 ) ) ;
#38745 = CARTESIAN_POINT ( 'NONE',  ( 7.139999999999985469, -39.93000000000000682, -12.10072711459627293 ) ) ;
#38746 = CARTESIAN_POINT ( 'NONE',  ( 11.99999999999992717, -3.412538124160723108, 4.000000000000000000 ) ) ;
#38748 = ORIENTED_EDGE ( 'NONE', *, *, #91721, .T. ) ;
#38747 = LINE ( 'NONE', #82973, #77683 ) ;
#38749 = CARTESIAN_POINT ( 'NONE',  ( -31.49999999999977973, 3.431123077392151277, 4.000000000000000000 ) ) ;
#38750 = LINE ( 'NONE', #59120, #66233 ) ;
#38751 = LINE ( 'NONE', #117696, #81811 ) ;
#38752 = EDGE_CURVE ( 'NONE', #125982, #56501, #113091, .T. ) ;
#38753 = LINE ( 'NONE', #6075, #13687 ) ;
#38754 = ORIENTED_EDGE ( 'NONE', *, *, #86746, .F. ) ;
#38755 = ADVANCED_FACE ( 'NONE', ( #34091 ), #13009, .T. ) ;
#38756 = ORIENTED_EDGE ( 'NONE', *, *, #137173, .T. ) ;
#38757 = VECTOR ( 'NONE', #39340, 1000.000000000000000 ) ;
#38758 = CARTESIAN_POINT ( 'NONE',  ( 5.994519915287488843, 28.92564299267942118, 4.000000000000000000 ) ) ;
#38759 = EDGE_CURVE ( 'NONE', #35892, #9606, #134110, .T. ) ;
#38760 = LINE ( 'NONE', #125046, #105 ) ;
#38761 = CARTESIAN_POINT ( 'NONE',  ( 28.99806943317882002, -22.22500000000000142, 4.500000000000000888 ) ) ;
#38762 = DIRECTION ( 'NONE',  ( 0.7071067811865486830, -0.7071067811865464625, -0.000000000000000000 ) ) ;
#38763 = DIRECTION ( 'NONE',  ( 0.3543493200069162685, -0.000000000000000000, -0.9351131265310288487 ) ) ;
#38764 = ORIENTED_EDGE ( 'NONE', *, *, #46011, .T. ) ;
#38765 = ORIENTED_EDGE ( 'NONE', *, *, #86765, .T. ) ;
#38766 = PLANE ( 'NONE',  #51552 ) ;
#38767 = DIRECTION ( 'NONE',  ( -0.6830127018922180770, -0.6830127018922204085, -0.2588190451025213501 ) ) ;
#38768 = ORIENTED_EDGE ( 'NONE', *, *, #75462, .F. ) ;
#38769 = EDGE_CURVE ( 'NONE', #16744, #91733, #56592, .T. ) ;
#38770 = EDGE_CURVE ( 'NONE', #131909, #143522, #62202, .T. ) ;
#38771 = ORIENTED_EDGE ( 'NONE', *, *, #142510, .T. ) ;
#38772 = VECTOR ( 'NONE', #58387, 1000.000000000000000 ) ;
#38773 = CARTESIAN_POINT ( 'NONE',  ( 34.47516574401890210, 13.49051761211548772, 4.998110765256834398 ) ) ;
#38774 = ORIENTED_EDGE ( 'NONE', *, *, #43223, .F. ) ;
#38775 = CARTESIAN_POINT ( 'NONE',  ( 61.03752705046289151, -9.735942053221456900E-16, 7.949999999999998401 ) ) ;
#38776 = CARTESIAN_POINT ( 'NONE',  ( 27.99999999999999645, -57.14999999999999147, -49.92499999999968452 ) ) ;
#38777 =( GEOMETRIC_REPRESENTATION_CONTEXT ( 3 ) GLOBAL_UNCERTAINTY_ASSIGNED_CONTEXT ( ( #127284 ) ) GLOBAL_UNIT_ASSIGNED_CONTEXT ( ( #7776, #41865, #109958 ) ) REPRESENTATION_CONTEXT ( 'NONE', 'WORKASPACE' ) );
#38778 = AXIS2_PLACEMENT_3D ( 'NONE', #12727, #122940, #35956 ) ;
#38779 = EDGE_CURVE ( 'NONE', #130625, #130905, #101458, .T. ) ;
#38780 = FACE_BOUND ( 'NONE', #140312, .T. ) ;
#38781 = ADVANCED_FACE ( 'NONE', ( #80454 ), #78300, .F. ) ;
#38782 = FILL_AREA_STYLE ('',( #138094 ) ) ;
#38783 = DIRECTION ( 'NONE',  ( 0.000000000000000000, -0.000000000000000000, 1.000000000000000000 ) ) ;
#38785 = EDGE_LOOP ( 'NONE', ( #127120, #68430, #93871, #8344 ) ) ;
#38784 = DIRECTION ( 'NONE',  ( -1.000000000000000000, -0.000000000000000000, -0.000000000000000000 ) ) ;
#38786 = VECTOR ( 'NONE', #129711, 1000.000000000000227 ) ;
#38787 = FACE_OUTER_BOUND ( 'NONE', #132131, .T. ) ;
#38789 = EDGE_CURVE ( 'NONE', #51436, #77362, #12307, .T. ) ;
#38788 = APPLICATION_PROTOCOL_DEFINITION ( 'draft international standard', 'automotive_design', 1998, #69885 ) ;
#38790 = VERTEX_POINT ( 'NONE', #112354 ) ;
#38791 = CIRCLE ( 'NONE', #61889, 2.055000000000001048 ) ;
#38792 = ORIENTED_EDGE ( 'NONE', *, *, #36954, .T. ) ;
#38793 = CARTESIAN_POINT ( 'NONE',  ( 91.78709685856478018, 3.054999999999997495, 5.291415217122919401 ) ) ;
#38794 = ORIENTED_EDGE ( 'NONE', *, *, #36970, .T. ) ;
#38795 = CARTESIAN_POINT ( 'NONE',  ( 2.999999999999983569, -3.412538124160724884, 4.000000000000000000 ) ) ;
#38796 = AXIS2_PLACEMENT_3D ( 'NONE', #56280, #13409, #22849 ) ;
#38797 = CARTESIAN_POINT ( 'NONE',  ( -23.55512991947090029, -0.7407075233842665973, 4.307968247156982677 ) ) ;
#38798 = EDGE_CURVE ( 'NONE', #42222, #75919, #2107, .T. ) ;
#38799 = LINE ( 'NONE', #138108, #68804 ) ;
#38800 = DIRECTION ( 'NONE',  ( 1.000000000000000000, 0.000000000000000000, 0.000000000000000000 ) ) ;
#38801 = ORIENTED_EDGE ( 'NONE', *, *, #93418, .T. ) ;
#38802 = CARTESIAN_POINT ( 'NONE',  ( -2.999999999999975131, -18.41253812416056945, 4.000000000000000000 ) ) ;
#38803 = DIRECTION ( 'NONE',  ( -0.6830127018922180770, -0.6830127018922204085, -0.2588190451025213501 ) ) ;
#38804 = CARTESIAN_POINT ( 'NONE',  ( 17.99451991528748351, 28.92564299267950645, 4.000000000000000000 ) ) ;
#38806 = DIRECTION ( 'NONE',  ( -1.000000000000000000, -0.000000000000000000, 0.000000000000000000 ) ) ;
#38805 = DIRECTION ( 'NONE',  ( -1.000000000000000000, -1.224606353822377258E-16, -0.000000000000000000 ) ) ;
#38807 = DIRECTION ( 'NONE',  ( -0.000000000000000000, 0.000000000000000000, 1.000000000000000000 ) ) ;
#38808 = CARTESIAN_POINT ( 'NONE',  ( -26.99999999999980105, -13.44781430457069504, 5.000000000000000000 ) ) ;
#38809 = ADVANCED_FACE ( 'NONE', ( #89175 ), #1409, .T. ) ;
#38810 = CARTESIAN_POINT ( 'NONE',  ( -13.49999999999990408, -12.66682484999667402, -0.6294897503864261834 ) ) ;
#38811 = ORIENTED_EDGE ( 'NONE', *, *, #118482, .T. ) ;
#38812 = LINE ( 'NONE', #16305, #75009 ) ;
#38813 = DIRECTION ( 'NONE',  ( 0.7071067811865486830, -0.7071067811865464625, -0.000000000000000000 ) ) ;
#38814 = EDGE_LOOP ( 'NONE', ( #102851, #85486, #42264, #128974 ) ) ;
#38815 = ORIENTED_EDGE ( 'NONE', *, *, #127916, .T. ) ;
#38816 = ORIENTED_EDGE ( 'NONE', *, *, #29720, .F. ) ;
#38817 = ADVANCED_FACE ( 'NONE', ( #133401 ), #122486, .T. ) ;
#38818 = CARTESIAN_POINT ( 'NONE',  ( 41.56293019189810423, 1.637169565754157174, 6.110000000000002984 ) ) ;
#38820 = EDGE_CURVE ( 'NONE', #135923, #57800, #58005, .T. ) ;
#38819 = AXIS2_PLACEMENT_3D ( 'NONE', #109053, #99600, #143126 ) ;
#38821 = ORIENTED_EDGE ( 'NONE', *, *, #30562, .T. ) ;
#38822 = EDGE_CURVE ( 'NONE', #139365, #119425, #79041, .T. ) ;
#38823 = AXIS2_PLACEMENT_3D ( 'NONE', #72422, #60833, #15112 ) ;
#38824 = CARTESIAN_POINT ( 'NONE',  ( 20.02497294953710849, -4.461849672132299993, -4.461849672132299105 ) ) ;
#38825 = CARTESIAN_POINT ( 'NONE',  ( -16.96380654081093553, 5.480407308985125070, -29.16618357164760766 ) ) ;
#38826 = ORIENTED_EDGE ( 'NONE', *, *, #12955, .T. ) ;
#38827 = PLANE ( 'NONE',  #128125 ) ;
#38828 = ORIENTED_EDGE ( 'NONE', *, *, #16119, .F. ) ;
#38829 = PLANE ( 'NONE',  #16375 ) ;
#38830 = CARTESIAN_POINT ( 'NONE',  ( 10.32500000000000107, -9.500000000000001776, 0.000000000000000000 ) ) ;
#38832 = ORIENTED_EDGE ( 'NONE', *, *, #10608, .F. ) ;
#38831 = DIRECTION ( 'NONE',  ( -0.7071067811865487940, 0.7071067811865463515, -0.000000000000000000 ) ) ;
#38833 = VERTEX_POINT ( 'NONE', #36913 ) ;
#38834 = CARTESIAN_POINT ( 'NONE',  ( -66.29974487139159578, -27.71228299555252406, 4.000000000000000000 ) ) ;
#38835 = DIRECTION ( 'NONE',  ( -0.7071067811865487940, 0.7071067811865463515, -0.000000000000000000 ) ) ;
#38836 = ORIENTED_EDGE ( 'NONE', *, *, #6318, .F. ) ;
#38837 = DIRECTION ( 'NONE',  ( -0.6830127018922180770, -0.6830127018922204085, -0.2588190451025213501 ) ) ;
#38838 = ORIENTED_EDGE ( 'NONE', *, *, #15403, .T. ) ;
#38839 = PRODUCT_DEFINITION_SHAPE ( 'NONE', 'NONE',  #14658 ) ;
#38840 = EDGE_LOOP ( 'NONE', ( #41253, #102957, #141948, #98545 ) ) ;
#38841 = ORIENTED_EDGE ( 'NONE', *, *, #90040, .T. ) ;
#38842 = ORIENTED_EDGE ( 'NONE', *, *, #89506, .F. ) ;
#38843 = CARTESIAN_POINT ( 'NONE',  ( 34.49999999999975842, 21.43112307739196609, 4.000000000000000000 ) ) ;
#38844 = CARTESIAN_POINT ( 'NONE',  ( -35.20003122016815666, 8.259292476615634371, 16.85664084051849443 ) ) ;
#38845 = VECTOR ( 'NONE', #99767, 1000.000000000000000 ) ;
#38846 = LINE ( 'NONE', #72237, #16956 ) ;
#38847 = CARTESIAN_POINT ( 'NONE',  ( -23.99999999999982236, 8.587461875839151659, 4.000000000000000000 ) ) ;
#38848 = ORIENTED_EDGE ( 'NONE', *, *, #1737, .T. ) ;
#38849 = CARTESIAN_POINT ( 'NONE',  ( 67.20833333333332860, -3.974999999999999201, -6.884901960086287964 ) ) ;
#38850 = ORIENTED_EDGE ( 'NONE', *, *, #124322, .T. ) ;
#38851 = LINE ( 'NONE', #104813, #28573 ) ;
#38852 = CARTESIAN_POINT ( 'NONE',  ( 27.68706980810188867, -2.126176841940956130, 7.934999999999991616 ) ) ;
#38853 = CARTESIAN_POINT ( 'NONE',  ( -26.29289321881326913, -3.740707523384244837, 5.000000000000000000 ) ) ;
#38854 = DIRECTION ( 'NONE',  ( 0.7071067811865486830, -0.7071067811865464625, -0.000000000000000000 ) ) ;
#38855 = TOROIDAL_SURFACE ( 'NONE', #57400, 3.500000000000000000, 0.5000000000000000000 ) ;
#38856 = CARTESIAN_POINT ( 'NONE',  ( -34.75757056450616744, 22.27000000000000668, -10.47732366696226869 ) ) ;
#38857 = ORIENTED_EDGE ( 'NONE', *, *, #60481, .F. ) ;
#38858 = ORIENTED_EDGE ( 'NONE', *, *, #25258, .T. ) ;
#38859 = EDGE_CURVE ( 'NONE', #123360, #6090, #2854, .T. ) ;
#38860 = ORIENTED_EDGE ( 'NONE', *, *, #26350, .T. ) ;
#38861 = PLANE ( 'NONE',  #138988 ) ;
#38862 = LINE ( 'NONE', #3348, #102097 ) ;
#38863 = UNCERTAINTY_MEASURE_WITH_UNIT (LENGTH_MEASURE( 1.000000000000000082E-05 ), #142435, 'distance_accuracy_value', 'NONE');
#38864 = CARTESIAN_POINT ( 'NONE',  ( 4.499999999999979572, 1.087461875839227154, 4.000000000000000000 ) ) ;
#38865 = LINE ( 'NONE', #113544, #52027 ) ;
#38866 = CARTESIAN_POINT ( 'NONE',  ( 3.100164867289006754, -48.63026969829200397, -38.45492102172624271 ) ) ;
#38867 = CARTESIAN_POINT ( 'NONE',  ( 78.95376352523145158, -6.109999999999999432, -3.741295971395163529E-16 ) ) ;
#38868 = CARTESIAN_POINT ( 'NONE',  ( 73.72502705046288440, 5.819803920172573974, -5.819803920172573086 ) ) ;
#38870 = AXIS2_PLACEMENT_3D ( 'NONE', #126274, #1597, #67646 ) ;
#38869 = CARTESIAN_POINT ( 'NONE',  ( 28.49999999999980815, 14.14708470758593606, -0.5283514160167208651 ) ) ;
#38871 = CYLINDRICAL_SURFACE ( 'NONE', #69679, 2.500000000000000000 ) ;
#38872 = LINE ( 'NONE', #128731, #116155 ) ;
#38873 = CARTESIAN_POINT ( 'NONE',  ( -32.99999999999977263, 18.08204922493370148, 0.9627537363045626240 ) ) ;
#38874 = ORIENTED_EDGE ( 'NONE', *, *, #18474, .F. ) ;
#38875 = CARTESIAN_POINT ( 'NONE',  ( 13.17183060077637968, -20.24070752338407431, 4.000000000000000000 ) ) ;
#38876 = ORIENTED_EDGE ( 'NONE', *, *, #5505, .F. ) ;
#38877 = AXIS2_PLACEMENT_3D ( 'NONE', #130141, #21369, #19917 ) ;
#38878 = LINE ( 'NONE', #84543, #48418 ) ;
#38880 = VERTEX_POINT ( 'NONE', #57285 ) ;
#38879 = CARTESIAN_POINT ( 'NONE',  ( -10.49999999999992895, -4.796895815301030375, -3.611700055028705503 ) ) ;
#38881 = ADVANCED_FACE ( 'NONE', ( #66706 ), #14459, .F. ) ;
#38882 = CARTESIAN_POINT ( 'NONE',  ( 0.000000000000000000, 0.000000000000000000, 5.000000000000000000 ) ) ;
#38883 = PLANE ( 'NONE',  #77341 ) ;
#38884 = EDGE_LOOP ( 'NONE', ( #17859, #83326, #99033, #115561 ) ) ;
#38885 = EDGE_CURVE ( 'NONE', #91730, #121313, #126090, .T. ) ;
#38886 = ORIENTED_EDGE ( 'NONE', *, *, #80969, .T. ) ;
#38887 = CARTESIAN_POINT ( 'NONE',  ( 120.6833603837968667, -2.130196079835385170, 7.949999999995403854 ) ) ;
#38888 = EDGE_LOOP ( 'NONE', ( #140523, #113618, #54446, #63117 ) ) ;
#38889 = VECTOR ( 'NONE', #140103, 999.9999999999998863 ) ;
#38890 = VECTOR ( 'NONE', #84290, 1000.000000000000000 ) ;
#38891 = LINE ( 'NONE', #59251, #70485 ) ;
#38892 = CARTESIAN_POINT ( 'NONE',  ( 90.05836038379621300, -7.949999999999997513, -2.130196079827425759 ) ) ;
#38893 = CARTESIAN_POINT ( 'NONE',  ( -28.49999999999979394, 22.08746187583901843, 4.000000000000000000 ) ) ;
#38894 = CYLINDRICAL_SURFACE ( 'NONE', #138668, 5.999999999999998224 ) ;
#38895 = EDGE_LOOP ( 'NONE', ( #98486, #64528, #130320, #116670 ) ) ;
#38896 = EDGE_CURVE ( 'NONE', #56720, #32623, #137685, .T. ) ;
#38897 = FACE_OUTER_BOUND ( 'NONE', #71047, .T. ) ;
#38898 = CARTESIAN_POINT ( 'NONE',  ( 0.4892135623730947680, -27.52281430457055578, 5.000000000000000000 ) ) ;
#38899 = CARTESIAN_POINT ( 'NONE',  ( 27.56249999999999645, 4.461849672132300881, 4.461849672132299105 ) ) ;
#38900 = DIRECTION ( 'NONE',  ( 0.000000000000000000, -1.000000000000000000, 0.000000000000000000 ) ) ;
#38901 = LINE ( 'NONE', #83124, #116195 ) ;
#38902 = ORIENTED_EDGE ( 'NONE', *, *, #26113, .F. ) ;
#38903 = EDGE_CURVE ( 'NONE', #127446, #19682, #39809, .T. ) ;
#38904 = LINE ( 'NONE', #72297, #127767 ) ;
#38905 = VERTEX_POINT ( 'NONE', #105027 ) ;
#38906 = CARTESIAN_POINT ( 'NONE',  ( 87.79209685856477563, -5.291415217122921177, 3.054999999999999272 ) ) ;
#38907 = DIRECTION ( 'NONE',  ( -0.6830127018922180770, -0.6830127018922204085, -0.2588190451025213501 ) ) ;
#38908 = DIRECTION ( 'NONE',  ( 0.7071067811865487940, 0.7071067811865463515, -0.000000000000000000 ) ) ;
#38909 = CARTESIAN_POINT ( 'NONE',  ( -10.17183060077639389, -11.24070752338416845, 4.000000000000000000 ) ) ;
#38910 = VERTEX_POINT ( 'NONE', #105716 ) ;
#38911 = EDGE_CURVE ( 'NONE', #16679, #24719, #38359, .T. ) ;
#38912 = EDGE_CURVE ( 'NONE', #70384, #114250, #92716, .T. ) ;
#38913 = LINE ( 'NONE', #4795, #72077 ) ;
#38914 = VECTOR ( 'NONE', #121191, 1000.000000000000227 ) ;
#38915 = DIRECTION ( 'NONE',  ( -0.7071067811865487940, 0.7071067811865463515, 0.000000000000000000 ) ) ;
#38916 = LINE ( 'NONE', #106271, #2212 ) ;
#38917 = FACE_OUTER_BOUND ( 'NONE', #3881, .T. ) ;
#38919 = VERTEX_POINT ( 'NONE', #50652 ) ;
#38918 = DIRECTION ( 'NONE',  ( 0.7071067811865487940, -0.7071067811865463515, 0.000000000000000000 ) ) ;
#38921 = VECTOR ( 'NONE', #99391, 999.9999999999998863 ) ;
#38920 = CARTESIAN_POINT ( 'NONE',  ( -20.66652290003515446, 8.920938975803856863, 4.000000000000000000 ) ) ;
#38922 = LINE ( 'NONE', #28772, #19839 ) ;
#38923 = CARTESIAN_POINT ( 'NONE',  ( 1.703100290951983453, -4.351279483125353842, 4.685986356884224158 ) ) ;
#38924 = CARTESIAN_POINT ( 'NONE',  ( 58.89583333333332149, -2.130196079827427091, 7.949999999999998401 ) ) ;
#38925 = ORIENTED_EDGE ( 'NONE', *, *, #76754, .T. ) ;
#38926 = ORIENTED_EDGE ( 'NONE', *, *, #825, .F. ) ;
#38927 = CARTESIAN_POINT ( 'NONE',  ( 74.66709685856476142, -3.055000000000000160, -5.291415217122921177 ) ) ;
#38928 = VERTEX_POINT ( 'NONE', #9061 ) ;
#38929 = DIRECTION ( 'NONE',  ( 0.7071067811865487940, -0.7071067811865463515, 0.000000000000000000 ) ) ;
#38930 = EDGE_CURVE ( 'NONE', #130643, #118381, #27449, .T. ) ;
#38931 = CARTESIAN_POINT ( 'NONE',  ( 17.51078643762690845, -27.52281430457043143, 5.000000000000000000 ) ) ;
#38932 = CARTESIAN_POINT ( 'NONE',  ( 45.18398860626900415, 28.73617430169818832, 5.000000000000000000 ) ) ;
#38933 = CARTESIAN_POINT ( 'NONE',  ( -21.48921356237309155, -27.52281430457070499, 5.000000000000000000 ) ) ;
#38934 = ORIENTED_EDGE ( 'NONE', *, *, #46934, .F. ) ;
#38935 = VECTOR ( 'NONE', #87321, 1000.000000000000114 ) ;
#38936 = DIRECTION ( 'NONE',  ( 0.7071067811865487940, 0.7071067811865463515, 0.000000000000000000 ) ) ;
#38937 = CARTESIAN_POINT ( 'NONE',  ( -5.953411863704523022, 14.25929247661556332, 18.84478104361329187 ) ) ;
#38939 = EDGE_CURVE ( 'NONE', #101265, #139589, #84034, .T. ) ;
#38938 = VECTOR ( 'NONE', #40322, 1000.000000000000000 ) ;
#38940 = EDGE_CURVE ( 'NONE', #63172, #2777, #60127, .T. ) ;
#38941 = ORIENTED_EDGE ( 'NONE', *, *, #40711, .F. ) ;
#38942 = CARTESIAN_POINT ( 'NONE',  ( 2.999999999999987121, 7.552185695429095347, 5.000000000000000000 ) ) ;
#38943 = CARTESIAN_POINT ( 'NONE',  ( 34.05836038379622721, -7.949999999999996625, -2.130196079827426203 ) ) ;
#38944 = DIRECTION ( 'NONE',  ( 0.7071067811865487940, 0.7071067811865463515, 0.000000000000000000 ) ) ;
#38945 = EDGE_CURVE ( 'NONE', #116931, #26300, #49260, .T. ) ;
#38946 = EDGE_LOOP ( 'NONE', ( #10667, #135995, #6751, #171 ) ) ;
#38947 = ORIENTED_EDGE ( 'NONE', *, *, #3543, .T. ) ;
#38948 = EDGE_CURVE ( 'NONE', #39146, #118497, #42491, .T. ) ;
#38949 = EDGE_CURVE ( 'NONE', #62934, #10446, #28194, .T. ) ;
#38950 = LINE ( 'NONE', #73040, #80183 ) ;
#38951 = DIRECTION ( 'NONE',  ( -0.6830127018922181881, 0.6830127018922202975, -0.2588190451025214056 ) ) ;
#38952 = LINE ( 'NONE', #83922, #90497 ) ;
#38953 = DIRECTION ( 'NONE',  ( -0.7071067811865487940, 0.7071067811865463515, -0.000000000000000000 ) ) ;
#38954 = CARTESIAN_POINT ( 'NONE',  ( 52.87086038379622011, 6.884901960086289741, -3.974999999999993427 ) ) ;
#38955 = CARTESIAN_POINT ( 'NONE',  ( -34.92500000000001137, 21.72500000000000142, 5.000000000000000000 ) ) ;
#38956 = VERTEX_POINT ( 'NONE', #139107 ) ;
#38957 = ORIENTED_EDGE ( 'NONE', *, *, #66263, .F. ) ;
#38958 = COLOUR_RGB ( '', 0.08235294, 0.09019608, 0.10196078) ;
#38959 = ORIENTED_EDGE ( 'NONE', *, *, #85649, .F. ) ;
#38960 = EDGE_CURVE ( 'NONE', #5368, #42711, #48514, .T. ) ;
#38961 = ORIENTED_EDGE ( 'NONE', *, *, #38770, .T. ) ;
#38962 = EDGE_CURVE ( 'NONE', #29861, #86656, #17305, .T. ) ;
#38963 =( LENGTH_UNIT ( ) NAMED_UNIT ( * ) SI_UNIT ( .MILLI., .METRE. ) );
#38964 = EDGE_LOOP ( 'NONE', ( #66867, #37299, #90035, #61409 ) ) ;
#38965 = LINE ( 'NONE', #51287, #61152 ) ;
#38966 = LINE ( 'NONE', #7002, #115066 ) ;
#38967 = DIRECTION ( 'NONE',  ( 0.000000000000000000, -1.000000000000000000, 0.000000000000000000 ) ) ;
#38968 = AXIS2_PLACEMENT_3D ( 'NONE', #43269, #76622, #32385 ) ;
#38969 = VECTOR ( 'NONE', #37972, 1000.000000000000227 ) ;
#38970 = DIRECTION ( 'NONE',  ( -0.7071067811865486830, -0.7071067811865464625, 0.000000000000000000 ) ) ;
#38971 = VERTEX_POINT ( 'NONE', #94843 ) ;
#38972 = CARTESIAN_POINT ( 'NONE',  ( -11.99999999999991473, -1.447814304570815169, 5.000000000000000000 ) ) ;
#38973 = DIRECTION ( 'NONE',  ( -1.000000000000000000, 0.000000000000000000, 0.000000000000000000 ) ) ;
#38974 = VECTOR ( 'NONE', #74089, 1000.000000000000000 ) ;
#38975 = EDGE_LOOP ( 'NONE', ( #70511, #131105, #37866, #4709 ) ) ;
#38976 = DIRECTION ( 'NONE',  ( -0.6830127018922180770, -0.6830127018922204085, -0.2588190451025213501 ) ) ;
#38977 = EDGE_LOOP ( 'NONE', ( #1030, #70106, #7218, #61350, #124759 ) ) ;
#38978 = VERTEX_POINT ( 'NONE', #136950 ) ;
#38979 = DIRECTION ( 'NONE',  ( -1.000000000000000000, 0.000000000000000000, 0.000000000000000000 ) ) ;
#38980 = EDGE_LOOP ( 'NONE', ( #4825, #2540, #19496, #97958 ) ) ;
#38981 = ORIENTED_EDGE ( 'NONE', *, *, #130232, .F. ) ;
#38982 = CARTESIAN_POINT ( 'NONE',  ( 76.70876352523144703, -7.482591942790329030E-16, 6.110000000000001208 ) ) ;
#38983 = VECTOR ( 'NONE', #88404, 1000.000000000000000 ) ;
#38984 = ORIENTED_EDGE ( 'NONE', *, *, #112952, .F. ) ;
#38985 = VECTOR ( 'NONE', #94233, 999.9999999999998863 ) ;
#38986 = EDGE_CURVE ( 'NONE', #121050, #109497, #4956, .T. ) ;
#38987 = PLANE ( 'NONE',  #32710 ) ;
#38988 = EDGE_CURVE ( 'NONE', #98192, #112966, #128231, .T. ) ;
#38989 = CARTESIAN_POINT ( 'NONE',  ( -18.29974487139159223, -27.71228299555219010, 4.000000000000000000 ) ) ;
#38990 = CARTESIAN_POINT ( 'NONE',  ( 105.4379301918981042, -6.110000000000001208, 1.637169565754158951 ) ) ;
#38991 = CARTESIAN_POINT ( 'NONE',  ( -5.816011393731002066, 28.73617430169783304, 5.000000000000000000 ) ) ;
#38992 = FACE_OUTER_BOUND ( 'NONE', #5025, .T. ) ;
#38993 = DIRECTION ( 'NONE',  ( 0.000000000000000000, 1.000000000000000000, 0.000000000000000000 ) ) ;
#38994 = CARTESIAN_POINT ( 'NONE',  ( -12.77004279457784186, 21.73644205237998150, 5.000000000000000888 ) ) ;
#38995 = AXIS2_PLACEMENT_3D ( 'NONE', #109639, #108176, #8159 ) ;
#38996 = EDGE_CURVE ( 'NONE', #43627, #121003, #70320, .T. ) ;
#38997 = CARTESIAN_POINT ( 'NONE',  ( -30.70710678118632586, -18.74070752338408852, 5.000000000000000000 ) ) ;
#38998 =( BOUNDED_CURVE ( )  B_SPLINE_CURVE ( 3, ( #99538, #2355, #46670, #88712 ),
 .UNSPECIFIED., .F., .F. ) 
 B_SPLINE_CURVE_WITH_KNOTS ( ( 4, 4 ),
 ( 4.350170835173024386, 4.500739107949268458 ),
 .UNSPECIFIED. ) 
 CURVE ( )  GEOMETRIC_REPRESENTATION_ITEM ( )  RATIONAL_B_SPLINE_CURVE ( ( 1.000000000000000000, 0.9981116584018941973, 0.9981116584018941973, 1.000000000000000000 ) ) 
 REPRESENTATION_ITEM ( '' )  );
#38999 = LINE ( 'NONE', #27381, #28201 ) ;
#39000 = LINE ( 'NONE', #112979, #6570 ) ;
#39001 = EDGE_LOOP ( 'NONE', ( #130031, #108586, #103360, #37049, #63800 ) ) ;
#39002 = VECTOR ( 'NONE', #29591, 1000.000000000000227 ) ;
#39003 = FACE_OUTER_BOUND ( 'NONE', #124386, .T. ) ;
#39004 = CARTESIAN_POINT ( 'NONE',  ( -7.940000000000007496, -39.92999999999999261, -10.00000000000000178 ) ) ;
#39005 = ORIENTED_EDGE ( 'NONE', *, *, #37304, .F. ) ;
#39006 = ORIENTED_EDGE ( 'NONE', *, *, #116514, .F. ) ;
#39007 = VECTOR ( 'NONE', #71711, 1000.000000000000000 ) ;
#39008 = CARTESIAN_POINT ( 'NONE',  ( 8.031592354503320763, 3.061616997868380183E-16, -2.500000000000001332 ) ) ;
#39009 = ORIENTED_EDGE ( 'NONE', *, *, #103869, .F. ) ;
#39010 = AXIS2_PLACEMENT_3D ( 'NONE', #109089, #110502, #43860 ) ;
#39011 = FACE_OUTER_BOUND ( 'NONE', #118016, .T. ) ;
#39012 = CARTESIAN_POINT ( 'NONE',  ( 114.0208333333333144, 7.949999999999998401, 2.130196079827431532 ) ) ;
#39013 = VECTOR ( 'NONE', #91943, 1000.000000000000227 ) ;
#39014 = DIRECTION ( 'NONE',  ( 0.000000000000000000, -1.000000000000000000, 0.000000000000000000 ) ) ;
#39015 = DIRECTION ( 'NONE',  ( -0.000000000000000000, 0.000000000000000000, 1.000000000000000000 ) ) ;
#39016 = ORIENTED_EDGE ( 'NONE', *, *, #22193, .T. ) ;
#39017 = VERTEX_POINT ( 'NONE', #117311 ) ;
#39018 = CARTESIAN_POINT ( 'NONE',  ( 0.5620698081018861147, -7.934999999999991616, -2.126176841940955242 ) ) ;
#39019 = CARTESIAN_POINT ( 'NONE',  ( -15.00548008471250228, 28.92564299267927552, 4.000000000000000000 ) ) ;
#39020 = CARTESIAN_POINT ( 'NONE',  ( 152.4000000000000057, -16.48000000000005016, 33.92499999999998295 ) ) ;
#39021 = CARTESIAN_POINT ( 'NONE',  ( -45.48921356237309510, -27.52281430457087197, 5.000000000000000000 ) ) ;
#39022 = ORIENTED_EDGE ( 'NONE', *, *, #114951, .F. ) ;
#39023 = VERTEX_POINT ( 'NONE', #81901 ) ;
#39024 = EDGE_LOOP ( 'NONE', ( #74966, #132758, #72584, #41298 ) ) ;
#39025 = DIRECTION ( 'NONE',  ( 0.000000000000000000, -1.000000000000000000, 0.000000000000000000 ) ) ;
#39026 = CYLINDRICAL_SURFACE ( 'NONE', #92765, 7.950000000000000178 ) ;
#39028 = VECTOR ( 'NONE', #53242, 1000.000000000000000 ) ;
#39027 = PLANE ( 'NONE',  #35833 ) ;
#39029 =( LENGTH_UNIT ( ) NAMED_UNIT ( * ) SI_UNIT ( .MILLI., .METRE. ) );
#39030 = FACE_OUTER_BOUND ( 'NONE', #12901, .T. ) ;
#39031 = VECTOR ( 'NONE', #33558, 999.9999999999998863 ) ;
#39032 = LINE ( 'NONE', #37624, #48052 ) ;
#39033 = CARTESIAN_POINT ( 'NONE',  ( 14.39532882439692862, 4.202752102959690472E-16, 0.000000000000000000 ) ) ;
#39034 = PLANE ( 'NONE',  #2617 ) ;
#39035 = FACE_OUTER_BOUND ( 'NONE', #76707, .T. ) ;
#39036 = VERTEX_POINT ( 'NONE', #15146 ) ;
#39037 = CARTESIAN_POINT ( 'NONE',  ( 2.994519915287485734, 28.92564299267940342, 4.000000000000000000 ) ) ;
#39038 = PLANE ( 'NONE',  #5391 ) ;
#39039 = VERTEX_POINT ( 'NONE', #59427 ) ;
#39040 = EDGE_CURVE ( 'NONE', #98192, #121495, #77748, .T. ) ;
#39041 = LINE ( 'NONE', #82551, #94659 ) ;
#39043 = ORIENTED_EDGE ( 'NONE', *, *, #118824, .T. ) ;
#39042 = CARTESIAN_POINT ( 'NONE',  ( 10.83999999999999986, 9.521314400968980422E-16, 0.000000000000000000 ) ) ;
#39044 = EDGE_CURVE ( 'NONE', #49517, #23600, #130920, .T. ) ;
#39045 = EDGE_CURVE ( 'NONE', #90465, #31526, #1755, .T. ) ;
#39046 = DIRECTION ( 'NONE',  ( -1.000000000000000000, 0.000000000000000000, -0.000000000000000000 ) ) ;
#39047 = CARTESIAN_POINT ( 'NONE',  ( 34.92499999999998295, -1.545334305399975072, 14.00746825007384899 ) ) ;
#39048 = VERTEX_POINT ( 'NONE', #101108 ) ;
#39049 = CARTESIAN_POINT ( 'NONE',  ( -2.999999999999978240, 2.966399257802228906, 5.000000000000000000 ) ) ;
#39050 = UNCERTAINTY_MEASURE_WITH_UNIT (LENGTH_MEASURE( 1.000000000000000082E-05 ), #19662, 'distance_accuracy_value', 'NONE');
#39051 = ORIENTED_EDGE ( 'NONE', *, *, #15205, .F. ) ;
#39052 = EDGE_CURVE ( 'NONE', #45045, #16291, #131621, .T. ) ;
#39053 = EDGE_CURVE ( 'NONE', #16596, #118999, #100419, .T. ) ;
#39054 = DIRECTION ( 'NONE',  ( 0.000000000000000000, -1.000000000000000000, 0.000000000000000000 ) ) ;
#39055 = DIRECTION ( 'NONE',  ( 0.7071067811865486830, -0.7071067811865464625, -0.000000000000000000 ) ) ;
#39056 = CARTESIAN_POINT ( 'NONE',  ( 117.7666937171295416, -7.949999999999999289, 2.130196079827424427 ) ) ;
#39057 = CARTESIAN_POINT ( 'NONE',  ( 29.99999999999979394, 10.93112307739207623, 4.000000000000000000 ) ) ;
#39058 = CARTESIAN_POINT ( 'NONE',  ( 12.00548008471251293, 28.92564299267929684, 4.000000000000000000 ) ) ;
#39059 = EDGE_CURVE ( 'NONE', #30546, #65367, #88112, .T. ) ;
#39060 = DIRECTION ( 'NONE',  ( 1.000000000000000000, 0.000000000000000000, 0.000000000000000000 ) ) ;
#39061 = CARTESIAN_POINT ( 'NONE',  ( -5.345055162546144878, 5.259292476615662792, 12.77922209995892722 ) ) ;
#39062 = LINE ( 'NONE', #50649, #18181 ) ;
#39063 = CARTESIAN_POINT ( 'NONE',  ( 32.49956980810188867, -3.967499999999998028, -6.871911579029511330 ) ) ;
#39064 = CARTESIAN_POINT ( 'NONE',  ( 9.020403141435219041, 7.934999999999988951, -2.126176841940961904 ) ) ;
#39065 = DIRECTION ( 'NONE',  ( 0.3543493200069162685, -0.000000000000000000, -0.9351131265310288487 ) ) ;
#39066 = LINE ( 'NONE', #128232, #7306 ) ;
#39067 = CARTESIAN_POINT ( 'NONE',  ( -25.49999999999982947, -4.216083040037277740, -7.486842126848599399 ) ) ;
#39068 = ORIENTED_EDGE ( 'NONE', *, *, #128054, .T. ) ;
#39069 = ORIENTED_EDGE ( 'NONE', *, *, #101494, .F. ) ;
#39071 = ADVANCED_FACE ( 'NONE', ( #31592 ), #78662, .F. ) ;
#39070 = CARTESIAN_POINT ( 'NONE',  ( 84.70833333333332860, -3.974999999999999201, -6.884901960086287964 ) ) ;
#39073 = ORIENTED_EDGE ( 'NONE', *, *, #110008, .T. ) ;
#39072 = CYLINDRICAL_SURFACE ( 'NONE', #130034, 0.5000000000000004441 ) ;
#39074 = ORIENTED_EDGE ( 'NONE', *, *, #99601, .F. ) ;
#39075 = CARTESIAN_POINT ( 'NONE',  ( 11.28242261357426202, -21.73023691814493930, 5.000000000000000888 ) ) ;
#39076 = CARTESIAN_POINT ( 'NONE',  ( -10.41009064519825955, 9.759292476615618384, 11.28811694763776430 ) ) ;
#39077 = CARTESIAN_POINT ( 'NONE',  ( 30.70419371712955581, -6.884901960086285300, -3.975000000000000089 ) ) ;
#39078 = ORIENTED_EDGE ( 'NONE', *, *, #46480, .F. ) ;
#39080 = EDGE_CURVE ( 'NONE', #55993, #108448, #85120, .T. ) ;
#39079 = CIRCLE ( 'NONE', #64632, 2.500000000000000888 ) ;
#39081 = AXIS2_PLACEMENT_3D ( 'NONE', #16348, #94639, #72247 ) ;
#39083 = DIRECTION ( 'NONE',  ( -0.7071067811865487940, 0.7071067811865463515, 0.000000000000000000 ) ) ;
#39082 =( GEOMETRIC_REPRESENTATION_CONTEXT ( 3 ) GLOBAL_UNCERTAINTY_ASSIGNED_CONTEXT ( ( #107151 ) ) GLOBAL_UNIT_ASSIGNED_CONTEXT ( ( #51634, #127765, #140075 ) ) REPRESENTATION_CONTEXT ( 'NONE', 'WORKASPACE' ) );
#39084 = DIRECTION ( 'NONE',  ( -1.504632769052527134E-30, -3.469446951953615372E-15, -1.000000000000000000 ) ) ;
#39085 = VECTOR ( 'NONE', #62342, 1000.000000000000227 ) ;
#39086 = LINE ( 'NONE', #139852, #55655 ) ;
#39087 = DIRECTION ( 'NONE',  ( 0.7071067811865487940, 0.7071067811865463515, 0.000000000000000000 ) ) ;
#39088 = DIRECTION ( 'NONE',  ( -0.000000000000000000, 0.000000000000000000, 1.000000000000000000 ) ) ;
#39089 = CARTESIAN_POINT ( 'NONE',  ( -24.30132219248945447, 6.014229859109025966, 4.331046227559734341 ) ) ;
#39090 = ADVANCED_FACE ( 'NONE', ( #120714 ), #110539, .T. ) ;
#39092 = DIRECTION ( 'NONE',  ( -0.7071067811865487940, 0.7071067811865463515, -0.000000000000000000 ) ) ;
#39091 = VECTOR ( 'NONE', #78238, 1000.000000000000000 ) ;
#39093 = DIRECTION ( 'NONE',  ( -0.000000000000000000, 0.3543493200069153248, 0.9351131265310292928 ) ) ;
#39094 = CARTESIAN_POINT ( 'NONE',  ( 5.816011393731002066, 28.73617430169783304, 5.000000000000000000 ) ) ;
#39095 = VECTOR ( 'NONE', #56905, 1000.000000000000000 ) ;
#39096 = CARTESIAN_POINT ( 'NONE',  ( -30.18398860626900060, 28.73617430169808173, 5.000000000000000000 ) ) ;
#39097 = DIRECTION ( 'NONE',  ( 0.3543493200069162685, -0.000000000000000000, -0.9351131265310288487 ) ) ;
#39098 = ORIENTED_EDGE ( 'NONE', *, *, #41306, .F. ) ;
#39099 = VERTEX_POINT ( 'NONE', #33750 ) ;
#39100 = CARTESIAN_POINT ( 'NONE',  ( 99.02126352523144703, -4.472830434245839371, -4.472830434245840259 ) ) ;
#39101 = ORIENTED_EDGE ( 'NONE', *, *, #25375, .T. ) ;
#39102 = EDGE_CURVE ( 'NONE', #62405, #68775, #122138, .T. ) ;
#39103 = CARTESIAN_POINT ( 'NONE',  ( -29.03689333454773447, -22.22500000000000142, 7.231223724525455587 ) ) ;
#39104 = VECTOR ( 'NONE', #12290, 1000.000000000000000 ) ;
#39105 = CARTESIAN_POINT ( 'NONE',  ( 4.828169399223495084, -8.240707523384200428, 4.000000000000000000 ) ) ;
#39106 = ORIENTED_EDGE ( 'NONE', *, *, #10481, .F. ) ;
#39107 = DIRECTION ( 'NONE',  ( -0.3543493200069162685, -0.000000000000000000, -0.9351131265310288487 ) ) ;
#39108 = FACE_OUTER_BOUND ( 'NONE', #31622, .T. ) ;
#39109 = ADVANCED_FACE ( 'NONE', ( #10519 ), #11213, .F. ) ;
#39110 = VECTOR ( 'NONE', #130201, 1000.000000000000227 ) ;
#39111 = CARTESIAN_POINT ( 'NONE',  ( 104.0370968585647802, -3.054999999999998828, -5.291415217122919401 ) ) ;
#39112 = ORIENTED_EDGE ( 'NONE', *, *, #81065, .F. ) ;
#39113 = EDGE_CURVE ( 'NONE', #143241, #50481, #67825, .T. ) ;
#39114 = DIRECTION ( 'NONE',  ( 0.5735764363510448272, -0.8191520442889927978, 1.003171929053526103E-16 ) ) ;
#39115 = VERTEX_POINT ( 'NONE', #11953 ) ;
#39116 = DIRECTION ( 'NONE',  ( 0.7071067811865487940, 0.7071067811865463515, -0.000000000000000000 ) ) ;
#39117 = VECTOR ( 'NONE', #62435, 999.9999999999998863 ) ;
#39118 = DIRECTION ( 'NONE',  ( -0.7071067811865487940, 0.7071067811865463515, -0.000000000000000000 ) ) ;
#39119 = CARTESIAN_POINT ( 'NONE',  ( 30.18398860626900060, 28.73617430169808173, 5.000000000000000000 ) ) ;
#39120 = PRESENTATION_LAYER_ASSIGNMENT (  '', '', ( #80836 ) ) ;
#39121 = LINE ( 'NONE', #24848, #32357 ) ;
#39123 = EDGE_CURVE ( 'NONE', #102268, #65177, #27760, .T. ) ;
#39122 = VECTOR ( 'NONE', #63678, 1000.000000000000000 ) ;
#39124 = VECTOR ( 'NONE', #100563, 1000.000000000000000 ) ;
#39125 = EDGE_LOOP ( 'NONE', ( #27981, #44466, #51984, #60633 ) ) ;
#39126 = ORIENTED_EDGE ( 'NONE', *, *, #73769, .T. ) ;
#39127 = VERTEX_POINT ( 'NONE', #45351 ) ;
#39128 = DIRECTION ( 'NONE',  ( -0.6830127018922180770, -0.6830127018922204085, -0.2588190451025213501 ) ) ;
#39129 = LINE ( 'NONE', #40562, #73140 ) ;
#39130 = CARTESIAN_POINT ( 'NONE',  ( 8.087903141435219823, 6.871911579029515771, 3.967499999999989146 ) ) ;
#39131 = VECTOR ( 'NONE', #91329, 1000.000000000000114 ) ;
#39132 = AXIS2_PLACEMENT_3D ( 'NONE', #134596, #2607, #48271 ) ;
#39133 = DIRECTION ( 'NONE',  ( 0.7071067811865487940, -0.7071067811865463515, 0.000000000000000000 ) ) ;
#39134 = CARTESIAN_POINT ( 'NONE',  ( -31.99806943317879515, -22.22500000000000142, 4.500000000000000888 ) ) ;
#39135 = ORIENTED_EDGE ( 'NONE', *, *, #31383, .F. ) ;
#39136 = ORIENTED_EDGE ( 'NONE', *, *, #25430, .F. ) ;
#39137 = EDGE_CURVE ( 'NONE', #125282, #129157, #98277, .T. ) ;
#39138 = DIRECTION ( 'NONE',  ( -0.7071067811865486830, 0.7071067811865464625, 0.000000000000000000 ) ) ;
#39139 = ORIENTED_EDGE ( 'NONE', *, *, #99401, .F. ) ;
#39140 = ORIENTED_EDGE ( 'NONE', *, *, #29284, .T. ) ;
#39141 = VECTOR ( 'NONE', #128704, 1000.000000000000000 ) ;
#39142 = EDGE_CURVE ( 'NONE', #93894, #102448, #54780, .T. ) ;
#39143 = CARTESIAN_POINT ( 'NONE',  ( 114.6829301918981088, -1.637169565754158951, -6.109999999999998543 ) ) ;
#39144 = CARTESIAN_POINT ( 'NONE',  ( 31.82816939922330235, -5.240707523384235955, 4.000000000000000000 ) ) ;
#39145 = FACE_OUTER_BOUND ( 'NONE', #44644, .T. ) ;
#39146 = VERTEX_POINT ( 'NONE', #114133 ) ;
#39147 = LINE ( 'NONE', #83364, #127019 ) ;
#39148 = DIRECTION ( 'NONE',  ( 0.000000000000000000, 0.000000000000000000, 1.000000000000000000 ) ) ;
#39149 = LINE ( 'NONE', #72537, #62921 ) ;
#39150 = ORIENTED_EDGE ( 'NONE', *, *, #5477, .F. ) ;
#39151 = LINE ( 'NONE', #38438, #141406 ) ;
#39152 = FACE_BOUND ( 'NONE', #55958, .T. ) ;
#39153 = ORIENTED_EDGE ( 'NONE', *, *, #1179, .F. ) ;
#39154 = LINE ( 'NONE', #47914, #52704 ) ;
#39155 = CARTESIAN_POINT ( 'NONE',  ( -25.49999999999981526, 0.4497235411627213963, -5.599840258123600201 ) ) ;
#39156 = CARTESIAN_POINT ( 'NONE',  ( 6.299744871391586898, -27.71228299555210484, 4.000000000000000000 ) ) ;
#39157 = EDGE_CURVE ( 'NONE', #12547, #94195, #103623, .T. ) ;
#39158 = VERTEX_POINT ( 'NONE', #14817 ) ;
#39159 = LINE ( 'NONE', #52164, #85232 ) ;
#39160 = VERTEX_POINT ( 'NONE', #137331 ) ;
#39161 = ORIENTED_EDGE ( 'NONE', *, *, #31476, .T. ) ;
#39162 = ORIENTED_EDGE ( 'NONE', *, *, #57506, .T. ) ;
#39163 = EDGE_CURVE ( 'NONE', #4422, #137066, #78202, .T. ) ;
#39164 = CARTESIAN_POINT ( 'NONE',  ( 29.37043019189811233, -3.055000000000001492, 5.291415217122917625 ) ) ;
#39165 = EDGE_LOOP ( 'NONE', ( #64537, #56195, #59287, #46430 ) ) ;
#39166 = FACE_OUTER_BOUND ( 'NONE', #87001, .T. ) ;
#39167 = CARTESIAN_POINT ( 'NONE',  ( -11.99999999999990230, -16.44781430457067373, 5.000000000000000000 ) ) ;
#39168 = DIRECTION ( 'NONE',  ( -1.000000000000000000, -1.224606353822377258E-16, -0.000000000000000000 ) ) ;
#39169 = LINE ( 'NONE', #127608, #96839 ) ;
#39170 = EDGE_CURVE ( 'NONE', #93730, #16801, #35178, .T. ) ;
#39171 = DIRECTION ( 'NONE',  ( 0.3543493200069162685, -0.000000000000000000, -0.9351131265310288487 ) ) ;
#39172 = ADVANCED_FACE ( 'NONE', ( #24963 ), #135210, .F. ) ;
#39173 = FACE_OUTER_BOUND ( 'NONE', #28200, .T. ) ;
#39174 = FACE_OUTER_BOUND ( 'NONE', #70132, .T. ) ;
#39175 = CARTESIAN_POINT ( 'NONE',  ( 24.04658813629530201, 14.25929247661557042, 18.84478104361322082 ) ) ;
#39176 = ORIENTED_EDGE ( 'NONE', *, *, #115171, .F. ) ;
#39177 = ORIENTED_EDGE ( 'NONE', *, *, #5362, .F. ) ;
#39178 = STYLED_ITEM ( 'NONE', ( #79101 ), #975 ) ;
#39179 = ORIENTED_EDGE ( 'NONE', *, *, #85632, .T. ) ;
#39180 = VERTEX_POINT ( 'NONE', #59087 ) ;
#39181 = CARTESIAN_POINT ( 'NONE',  ( -28.17183060077627133, 18.75929247661552424, 4.000000000000000000 ) ) ;
#39182 = VECTOR ( 'NONE', #62710, 1000.000000000000000 ) ;
#39183 = MECHANICAL_DESIGN_GEOMETRIC_PRESENTATION_REPRESENTATION (  '', ( #67022 ), #78611 ) ;
#39184 = VERTEX_POINT ( 'NONE', #27115 ) ;
#39185 = CIRCLE ( 'NONE', #55437, 0.5000000000000004441 ) ;
#39187 = EDGE_LOOP ( 'NONE', ( #132546, #123905, #47896, #84495 ) ) ;
#39186 = VECTOR ( 'NONE', #90503, 1000.000000000000000 ) ;
#39188 = LINE ( 'NONE', #105145, #37558 ) ;
#39189 = CARTESIAN_POINT ( 'NONE',  ( 4.499999999999972466, -4.533600742197694267, 5.000000000000000000 ) ) ;
#39190 = EDGE_CURVE ( 'NONE', #35605, #68587, #103941, .T. ) ;
#39191 = CARTESIAN_POINT ( 'NONE',  ( 8.999999999999944933, 2.966399257802236011, 5.000000000000000000 ) ) ;
#39192 = ORIENTED_EDGE ( 'NONE', *, *, #45285, .F. ) ;
#39193 = PLANE ( 'NONE',  #11673 ) ;
#39194 = ORIENTED_EDGE ( 'NONE', *, *, #109442, .F. ) ;
#39195 =( BOUNDED_CURVE ( )  B_SPLINE_CURVE ( 3, ( #117876, #41077, #50533, #104904 ),
 .UNSPECIFIED., .F., .T. ) 
 B_SPLINE_CURVE_WITH_KNOTS ( ( 4, 4 ),
 ( 0.9743798061614656891, 1.027697802963069451 ),
 .UNSPECIFIED. ) 
 CURVE ( )  GEOMETRIC_REPRESENTATION_ITEM ( )  RATIONAL_B_SPLINE_CURVE ( ( 1.000000000000000000, 0.9997631132982454094, 0.9997631132982454094, 1.000000000000000000 ) ) 
 REPRESENTATION_ITEM ( '' )  );
#39196 = DIRECTION ( 'NONE',  ( 0.7071067811865487940, -0.7071067811865463515, 0.000000000000000000 ) ) ;
#39197 = CARTESIAN_POINT ( 'NONE',  ( 1.233736474768552860, 5.808823158059036373, 5.808823158059032821 ) ) ;
#39198 = ORIENTED_EDGE ( 'NONE', *, *, #106994, .T. ) ;
#39200 = CARTESIAN_POINT ( 'NONE',  ( 29.99999999999978684, 4.965500833774356693, -4.007596771432726079 ) ) ;
#39199 = CARTESIAN_POINT ( 'NONE',  ( 105.2037635252314516, 6.109999999999999432, 1.122388791418549108E-15 ) ) ;
#39201 = FILL_AREA_STYLE ('',( #117437 ) ) ;
#39202 =( NAMED_UNIT ( * ) SI_UNIT ( $, .STERADIAN. ) SOLID_ANGLE_UNIT ( ) );
#39203 = ORIENTED_EDGE ( 'NONE', *, *, #76752, .F. ) ;
#39204 = ORIENTED_EDGE ( 'NONE', *, *, #98383, .T. ) ;
#39205 = CARTESIAN_POINT ( 'NONE',  ( 34.92499999999998295, 22.22500000000000142, 4.000000000000000000 ) ) ;
#39206 = ORIENTED_EDGE ( 'NONE', *, *, #60664, .T. ) ;
#39207 = AXIS2_PLACEMENT_3D ( 'NONE', #4766, #114968, #59247 ) ;
#39208 = PRESENTATION_STYLE_ASSIGNMENT (( #38495 ) ) ;
#39209 = DIRECTION ( 'NONE',  ( -0.7071067811865486830, -0.7071067811865464625, -0.000000000000000000 ) ) ;
#39210 = CARTESIAN_POINT ( 'NONE',  ( 52.60764783923754351, -49.05583548141699168, -39.86617647058817937 ) ) ;
#39211 = DIRECTION ( 'NONE',  ( -0.000000000000000000, -0.3543493200069152693, 0.9351131265310292928 ) ) ;
#39212 = CARTESIAN_POINT ( 'NONE',  ( -25.17183060077628909, 3.759292476615678336, 4.000000000000000000 ) ) ;
#39213 = ORIENTED_EDGE ( 'NONE', *, *, #6615, .F. ) ;
#39214 = CARTESIAN_POINT ( 'NONE',  ( 6.640000000000043201, -9.638965590364918103E-15, -39.50000000000000000 ) ) ;
#39215 = VECTOR ( 'NONE', #45186, 1000.000000000000000 ) ;
#39216 = FACE_OUTER_BOUND ( 'NONE', #18031, .T. ) ;
#39217 = PLANE ( 'NONE',  #107008 ) ;
#39218 = EDGE_CURVE ( 'NONE', #141554, #100356, #57433, .T. ) ;
#39219 = ORIENTED_EDGE ( 'NONE', *, *, #24998, .T. ) ;
#39220 = DIRECTION ( 'NONE',  ( -0.7071067811865486830, 0.7071067811865464625, 0.000000000000000000 ) ) ;
#39221 = VECTOR ( 'NONE', #138622, 1000.000000000000000 ) ;
#39223 = EDGE_CURVE ( 'NONE', #70988, #41423, #59775, .T. ) ;
#39222 = CARTESIAN_POINT ( 'NONE',  ( 14.99999999999989519, 17.96639925780207747, 5.000000000000000000 ) ) ;
#39224 = ORIENTED_EDGE ( 'NONE', *, *, #1291, .F. ) ;
#39225 = VECTOR ( 'NONE', #96422, 1000.000000000000000 ) ;
#39227 = ORIENTED_EDGE ( 'NONE', *, *, #60740, .F. ) ;
#39226 = FACE_OUTER_BOUND ( 'NONE', #116181, .T. ) ;
#39228 = EDGE_CURVE ( 'NONE', #94937, #106661, #72284, .T. ) ;
#39229 = EDGE_CURVE ( 'NONE', #29394, #50127, #60502, .T. ) ;
#39230 = VERTEX_POINT ( 'NONE', #13368 ) ;
#39231 = CARTESIAN_POINT ( 'NONE',  ( -2.132336019816571060, 13.66774714948344283, -24.42935889323532805 ) ) ;
#39232 = AXIS2_PLACEMENT_3D ( 'NONE', #20860, #107856, #75281 ) ;
#39233 = DIRECTION ( 'NONE',  ( 0.7071067811865487940, 0.7071067811865463515, 0.000000000000000000 ) ) ;
#39234 = ORIENTED_EDGE ( 'NONE', *, *, #95227, .F. ) ;
#39235 = CARTESIAN_POINT ( 'NONE',  ( 81.29974487139159578, -27.71228299555262709, 4.000000000000000000 ) ) ;
#39236 = CIRCLE ( 'NONE', #120207, 2.500000000000000444 ) ;
#39237 = EDGE_CURVE ( 'NONE', #16172, #28113, #90235, .T. ) ;
#39238 = EDGE_CURVE ( 'NONE', #58071, #44292, #57645, .T. ) ;
#39239 = DIRECTION ( 'NONE',  ( -0.3543493200069162685, -0.000000000000000000, -0.9351131265310288487 ) ) ;
#39240 = PLANE ( 'NONE',  #113274 ) ;
#39241 = EDGE_CURVE ( 'NONE', #134483, #23024, #125745, .T. ) ;
#39242 = ORIENTED_EDGE ( 'NONE', *, *, #120943, .F. ) ;
#39243 = CARTESIAN_POINT ( 'NONE',  ( 34.92499999999998295, -11.99387692260791205, 4.000000000000000000 ) ) ;
#39244 = DIRECTION ( 'NONE',  ( -0.7071067811865487940, 0.7071067811865463515, -0.000000000000000000 ) ) ;
#39245 = ADVANCED_FACE ( 'NONE', ( #26421 ), #113407, .F. ) ;
#39246 = DIRECTION ( 'NONE',  ( -0.7071067811865487940, 0.7071067811865463515, -0.000000000000000000 ) ) ;
#39247 = CARTESIAN_POINT ( 'NONE',  ( 2.041666666666666963, 3.047499999999993214, -5.278424836066146320 ) ) ;
#39248 = DIRECTION ( 'NONE',  ( -0.7071067811865487940, 0.7071067811865463515, 0.000000000000000000 ) ) ;
#39249 = MECHANICAL_DESIGN_GEOMETRIC_PRESENTATION_REPRESENTATION (  '', ( #64698 ), #29902 ) ;
#39250 = PLANE ( 'NONE',  #79130 ) ;
#39251 = DIRECTION ( 'NONE',  ( 0.5735764363510444941, 0.8191520442889929088, 0.000000000000000000 ) ) ;
#39252 = ADVANCED_FACE ( 'NONE', ( #114813 ), #85071, .F. ) ;
#39253 = DIRECTION ( 'NONE',  ( 0.000000000000000000, -1.301042606982605074E-16, 1.000000000000000000 ) ) ;
#39254 = FILL_AREA_STYLE_COLOUR ( '', #87127 ) ;
#39255 = ORIENTED_EDGE ( 'NONE', *, *, #29296, .T. ) ;
#39256 = ORIENTED_EDGE ( 'NONE', *, *, #113630, .T. ) ;
#39257 = VERTEX_POINT ( 'NONE', #30720 ) ;
#39259 = ADVANCED_FACE ( 'NONE', ( #27837 ), #95228, .T. ) ;
#39258 = CARTESIAN_POINT ( 'NONE',  ( 109.3541666666666714, -2.130196079827425315, -7.950000000000001066 ) ) ;
#39260 = VERTEX_POINT ( 'NONE', #16968 ) ;
#39261 = ORIENTED_EDGE ( 'NONE', *, *, #75495, .F. ) ;
#39262 = VERTEX_POINT ( 'NONE', #129276 ) ;
#39263 = PLANE ( 'NONE',  #77974 ) ;
#39264 = DIRECTION ( 'NONE',  ( -0.000000000000000000, 0.000000000000000000, 1.000000000000000000 ) ) ;
#39265 = VERTEX_POINT ( 'NONE', #61923 ) ;
#39266 = LINE ( 'NONE', #129104, #2225 ) ;
#39267 = EDGE_CURVE ( 'NONE', #25758, #118900, #138758, .T. ) ;
#39268 = CYLINDRICAL_SURFACE ( 'NONE', #65020, 5.999999999999998224 ) ;
#39269 = CARTESIAN_POINT ( 'NONE',  ( 23.87852683662838871, -20.24070752338407075, 7.412974875817736731 ) ) ;
#39270 = PLANE ( 'NONE',  #141386 ) ;
#39271 = CARTESIAN_POINT ( 'NONE',  ( 116.3754301918981042, -5.291415217122920289, -3.055000000000001492 ) ) ;
#39272 = ORIENTED_EDGE ( 'NONE', *, *, #11729, .F. ) ;
#39273 = CARTESIAN_POINT ( 'NONE',  ( -30.51665438641024153, 22.22500000000000142, 4.500000000000000888 ) ) ;
#39274 = DIRECTION ( 'NONE',  ( -0.3543493200069162685, -0.000000000000000000, -0.9351131265310288487 ) ) ;
#39275 = DIRECTION ( 'NONE',  ( -0.6830127018922181881, 0.6830127018922202975, -0.2588190451025214056 ) ) ;
#39276 = FACE_OUTER_BOUND ( 'NONE', #127576, .T. ) ;
#39277 = EDGE_CURVE ( 'NONE', #117931, #59073, #98974, .T. ) ;
#39278 = FACE_OUTER_BOUND ( 'NONE', #47442, .T. ) ;
#39279 = CARTESIAN_POINT ( 'NONE',  ( -5.510786437626906675, -27.52281430457051314, 5.000000000000000000 ) ) ;
#39280 = CARTESIAN_POINT ( 'NONE',  ( 39.30836038379621300, 7.949999999999997513, 2.130196079827431088 ) ) ;
#39281 = LINE ( 'NONE', #15334, #25957 ) ;
#39282 = DIRECTION ( 'NONE',  ( 0.7071067811865487940, -0.7071067811865463515, 0.000000000000000000 ) ) ;
#39283 = ORIENTED_EDGE ( 'NONE', *, *, #119335, .F. ) ;
#39284 = ORIENTED_EDGE ( 'NONE', *, *, #38489, .T. ) ;
#39285 = CARTESIAN_POINT ( 'NONE',  ( 32.06249999999999289, -5.819803920172572198, -5.819803920172573086 ) ) ;
#39286 = ORIENTED_EDGE ( 'NONE', *, *, #101187, .T. ) ;
#39287 = DIRECTION ( 'NONE',  ( -0.7071067811865487940, 0.7071067811865463515, 0.000000000000000000 ) ) ;
#39288 = DIRECTION ( 'NONE',  ( 0.7071067811865487940, 0.7071067811865463515, 0.000000000000000000 ) ) ;
#39289 = LINE ( 'NONE', #42155, #31752 ) ;
#39290 = DIRECTION ( 'NONE',  ( 0.7071067811865487940, 0.7071067811865463515, 0.000000000000000000 ) ) ;
#39291 = FACE_OUTER_BOUND ( 'NONE', #20761, .T. ) ;
#39292 = CARTESIAN_POINT ( 'NONE',  ( -28.82816939922333432, -20.24070752338407431, 4.000000000000000000 ) ) ;
#39293 = EDGE_CURVE ( 'NONE', #100848, #133006, #94505, .T. ) ;
#39294 = CARTESIAN_POINT ( 'NONE',  ( 29.60459685856477563, 1.637169565754164946, -6.109999999999999432 ) ) ;
#39295 = ORIENTED_EDGE ( 'NONE', *, *, #92167, .T. ) ;
#39296 = EDGE_CURVE ( 'NONE', #35756, #104393, #139500, .T. ) ;
#39297 = LINE ( 'NONE', #140044, #3961 ) ;
#39299 = ORIENTED_EDGE ( 'NONE', *, *, #5644, .F. ) ;
#39298 = AXIS2_PLACEMENT_3D ( 'NONE', #62869, #83921, #16448 ) ;
#39300 = DIRECTION ( 'NONE',  ( -0.7071067811865486830, -0.7071067811865464625, 0.000000000000000000 ) ) ;
#39301 = AXIS2_PLACEMENT_3D ( 'NONE', #104401, #115979, #85494 ) ;
#39302 = AXIS2_PLACEMENT_3D ( 'NONE', #9191, #120846, #141929 ) ;
#39303 = VECTOR ( 'NONE', #35676, 1000.000000000000000 ) ;
#39304 = CARTESIAN_POINT ( 'NONE',  ( 5.999999999999967137, -7.447814304570758104, 5.000000000000000000 ) ) ;
#39306 = EDGE_CURVE ( 'NONE', #130956, #28809, #127891, .T. ) ;
#39305 = DIRECTION ( 'NONE',  ( -1.000000000000000000, -1.224606353822377258E-16, -0.000000000000000000 ) ) ;
#39307 = VECTOR ( 'NONE', #127978, 1000.000000000000000 ) ;
#39308 = CARTESIAN_POINT ( 'NONE',  ( 63.85416666666665719, -2.130196079827425759, -7.950000000000000178 ) ) ;
#39309 = ORIENTED_EDGE ( 'NONE', *, *, #138029, .T. ) ;
#39310 = CARTESIAN_POINT ( 'NONE',  ( 50.75043019189810423, 3.055000000000002824, -5.291415217122919401 ) ) ;
#39311 = ORIENTED_EDGE ( 'NONE', *, *, #83559, .F. ) ;
#39312 = LINE ( 'NONE', #37892, #14640 ) ;
#39313 = LINE ( 'NONE', #40047, #36928 ) ;
#39314 = CARTESIAN_POINT ( 'NONE',  ( -25.49999999999982592, 16.77039438581777375, 0.4657186855308330098 ) ) ;
#39315 = CARTESIAN_POINT ( 'NONE',  ( 29.67183060077626422, 17.25929247661553489, 4.000000000000000000 ) ) ;
#39316 = VECTOR ( 'NONE', #23910, 1000.000000000000000 ) ;
#39317 = AXIS2_PLACEMENT_3D ( 'NONE', #128543, #94462, #29210 ) ;
#39318 = CARTESIAN_POINT ( 'NONE',  ( 52.84959685856479439, 6.109999999999996767, 1.637169565754163836 ) ) ;
#39319 = ORIENTED_EDGE ( 'NONE', *, *, #129266, .F. ) ;
#39320 = CARTESIAN_POINT ( 'NONE',  ( 5.999999999999956479, -6.108550654416955439, -3.114665004254954184 ) ) ;
#39321 = EDGE_CURVE ( 'NONE', #19893, #77966, #87056, .T. ) ;
#39322 = DIRECTION ( 'NONE',  ( 0.7071067811865486830, -0.7071067811865464625, -0.000000000000000000 ) ) ;
#39323 = ORIENTED_EDGE ( 'NONE', *, *, #127314, .F. ) ;
#39324 = VERTEX_POINT ( 'NONE', #138036 ) ;
#39325 = VECTOR ( 'NONE', #112365, 1000.000000000000000 ) ;
#39326 = VECTOR ( 'NONE', #129637, 1000.000000000000000 ) ;
#39327 = DIRECTION ( 'NONE',  ( -0.000000000000000000, -0.3543493200069152693, 0.9351131265310292928 ) ) ;
#39328 = ORIENTED_EDGE ( 'NONE', *, *, #102135, .F. ) ;
#39329 = VECTOR ( 'NONE', #62461, 1000.000000000000000 ) ;
#39330 = FACE_OUTER_BOUND ( 'NONE', #42060, .T. ) ;
#39331 = EDGE_CURVE ( 'NONE', #28081, #4087, #85781, .T. ) ;
#39332 = ORIENTED_EDGE ( 'NONE', *, *, #70450, .T. ) ;
#39333 = CARTESIAN_POINT ( 'NONE',  ( 27.22000000000000242, 2.055000000000001492, 0.000000000000000000 ) ) ;
#39334 = AXIS2_PLACEMENT_3D ( 'NONE', #3241, #25719, #14839 ) ;
#39335 = CONICAL_SURFACE ( 'NONE', #127262, 2.500000000000000888, 0.9599310885968822538 ) ;
#39337 = CIRCLE ( 'NONE', #120300, 2.055000000000001048 ) ;
#39336 = CARTESIAN_POINT ( 'NONE',  ( -38.99451991528749062, 28.92564299267965211, 4.000000000000000000 ) ) ;
#39338 = ADVANCED_FACE ( 'NONE', ( #96620 ), #95945, .F. ) ;
#39339 = FACE_BOUND ( 'NONE', #109824, .T. ) ;
#39340 = DIRECTION ( 'NONE',  ( -0.7071067811865486830, -0.7071067811865464625, 0.000000000000000000 ) ) ;
#39341 = VECTOR ( 'NONE', #89959, 1000.000000000000000 ) ;
#39342 = CARTESIAN_POINT ( 'NONE',  ( 22.00193056682082826, -22.22500000000000142, 4.500000000000000888 ) ) ;
#39343 = CARTESIAN_POINT ( 'NONE',  ( -11.22995720542198406, 21.73644205237998150, 5.000000000000000888 ) ) ;
#39344 = ORIENTED_EDGE ( 'NONE', *, *, #75603, .T. ) ;
#39345 = DIRECTION ( 'NONE',  ( 0.000000000000000000, -1.000000000000000000, 0.000000000000000000 ) ) ;
#39347 = ORIENTED_EDGE ( 'NONE', *, *, #83180, .F. ) ;
#39346 = CARTESIAN_POINT ( 'NONE',  ( 24.29974487139158867, -27.71228299555223273, 4.000000000000000000 ) ) ;
#39348 = VECTOR ( 'NONE', #96803, 1000.000000000000000 ) ;
#39349 = ORIENTED_EDGE ( 'NONE', *, *, #64136, .F. ) ;
#39350 = DIRECTION ( 'NONE',  ( 0.7071067811865487940, 0.7071067811865463515, 0.000000000000000000 ) ) ;
#39351 = ORIENTED_EDGE ( 'NONE', *, *, #98881, .F. ) ;
#39352 = ORIENTED_EDGE ( 'NONE', *, *, #65546, .T. ) ;
#39353 = CARTESIAN_POINT ( 'NONE',  ( 67.87043019189812298, -3.055000000000001492, 5.291415217122917625 ) ) ;
#39354 = VERTEX_POINT ( 'NONE', #61241 ) ;
#39355 = LINE ( 'NONE', #103839, #122817 ) ;
#39356 = FACE_OUTER_BOUND ( 'NONE', #41834, .T. ) ;
#39357 = ORIENTED_EDGE ( 'NONE', *, *, #21754, .T. ) ;
#39358 = SURFACE_STYLE_FILL_AREA ( #140098 ) ;
#39359 = AXIS2_PLACEMENT_3D ( 'NONE', #131145, #20935, #52151 ) ;
#39360 = EDGE_CURVE ( 'NONE', #30958, #83476, #6748, .T. ) ;
#39361 = ADVANCED_FACE ( 'NONE', ( #38722 ), #84392, .F. ) ;
#39362 = FACE_OUTER_BOUND ( 'NONE', #76789, .T. ) ;
#39363 = LINE ( 'NONE', #37199, #82949 ) ;
#39364 = CARTESIAN_POINT ( 'NONE',  ( 12.29974487139158512, -27.71228299555214747, 4.000000000000000000 ) ) ;
#39365 = CARTESIAN_POINT ( 'NONE',  ( 16.33333333333333570, 5.278424836066143655, -3.047499999999997655 ) ) ;
#39366 = ORIENTED_EDGE ( 'NONE', *, *, #140215, .F. ) ;
#39367 = VECTOR ( 'NONE', #42237, 1000.000000000000000 ) ;
#39368 = ORIENTED_EDGE ( 'NONE', *, *, #80045, .F. ) ;
#39369 = CARTESIAN_POINT ( 'NONE',  ( 69.48921356237309510, -27.52281430457103895, 5.000000000000000000 ) ) ;
#39370 = CARTESIAN_POINT ( 'NONE',  ( -21.09843580608223945, 11.25929247661560595, 10.79108189686402142 ) ) ;
#39371 = ORIENTED_EDGE ( 'NONE', *, *, #91007, .T. ) ;
#39372 = ORIENTED_EDGE ( 'NONE', *, *, #107742, .F. ) ;
#39373 = EDGE_LOOP ( 'NONE', ( #84443, #39434, #104605, #140066, #6969 ) ) ;
#39374 = DIRECTION ( 'NONE',  ( -0.000000000000000000, -0.3543493200069152693, 0.9351131265310292928 ) ) ;
#39375 = CARTESIAN_POINT ( 'NONE',  ( 26.99999999999981881, -22.06887692260759692, 4.000000000000000000 ) ) ;
#39376 = EDGE_CURVE ( 'NONE', #128706, #20835, #126010, .T. ) ;
#39377 = PLANE ( 'NONE',  #57835 ) ;
#39378 = ORIENTED_EDGE ( 'NONE', *, *, #45562, .F. ) ;
#39379 = DIRECTION ( 'NONE',  ( -1.000000000000000000, -8.828454896530885185E-16, 0.000000000000000000 ) ) ;
#39380 = CARTESIAN_POINT ( 'NONE',  ( 2.671830600776456510, 5.259292476615662792, 4.000000000000000000 ) ) ;
#39381 = CARTESIAN_POINT ( 'NONE',  ( 11.73373647476855197, 5.808823158059036373, 5.808823158059032821 ) ) ;
#39382 = CARTESIAN_POINT ( 'NONE',  ( 25.97159235450331849, 2.500000000000001332, 0.000000000000000000 ) ) ;
#39383 = ORIENTED_EDGE ( 'NONE', *, *, #132864, .F. ) ;
#39384 = CYLINDRICAL_SURFACE ( 'NONE', #59127, 2.500000000000000000 ) ;
#39385 = LINE ( 'NONE', #83614, #120585 ) ;
#39387 = ORIENTED_EDGE ( 'NONE', *, *, #121168, .T. ) ;
#39386 = CARTESIAN_POINT ( 'NONE',  ( -30.48921356237309510, -27.52281430457076894, 5.000000000000000000 ) ) ;
#39388 = DIRECTION ( 'NONE',  ( -0.7071067811865486830, 0.7071067811865464625, 0.000000000000000000 ) ) ;
#39389 = VERTEX_POINT ( 'NONE', #121963 ) ;
#39390 = DIRECTION ( 'NONE',  ( -1.000000000000000000, -1.224606353822377258E-16, -0.000000000000000000 ) ) ;
#39391 = CARTESIAN_POINT ( 'NONE',  ( 18.18398860626898994, 28.73617430169800002, 5.000000000000000000 ) ) ;
#39392 = CARTESIAN_POINT ( 'NONE',  ( 0.000000000000000000, 0.000000000000000000, 5.000000000000000000 ) ) ;
#39393 = VERTEX_POINT ( 'NONE', #88665 ) ;
#39394 = VECTOR ( 'NONE', #15094, 999.9999999999998863 ) ;
#39395 = CARTESIAN_POINT ( 'NONE',  ( 41.99451991528749062, 28.92564299267967343, 4.000000000000000000 ) ) ;
#39396 = CARTESIAN_POINT ( 'NONE',  ( 3.183988606268992161, 28.73617430169789699, 5.000000000000000000 ) ) ;
#39397 = CARTESIAN_POINT ( 'NONE',  ( 24.48921356237309510, -27.52281430457072631, 5.000000000000000000 ) ) ;
#39398 = EDGE_LOOP ( 'NONE', ( #72486, #1143, #33046, #57116 ) ) ;
#39399 = VECTOR ( 'NONE', #118135, 1000.000000000000000 ) ;
#39400 = VECTOR ( 'NONE', #15995, 1000.000000000000227 ) ;
#39401 = AXIS2_PLACEMENT_3D ( 'NONE', #1373, #66675, #34761 ) ;
#39402 = CARTESIAN_POINT ( 'NONE',  ( 12.35051985313232237, 4.584330080086930965E-16, 0.000000000000000000 ) ) ;
#39403 = PLANE ( 'NONE',  #26161 ) ;
#39404 = LINE ( 'NONE', #83637, #7567 ) ;
#39405 = MECHANICAL_DESIGN_GEOMETRIC_PRESENTATION_REPRESENTATION (  '', ( #90396 ), #76455 ) ;
#39406 = PLANE ( 'NONE',  #42545 ) ;
#39407 = CARTESIAN_POINT ( 'NONE',  ( 103.0375270504628986, -9.735942053221456900E-16, 7.949999999999998401 ) ) ;
#39408 = EDGE_LOOP ( 'NONE', ( #114195, #123152, #106312, #49457 ) ) ;
#39409 = VERTEX_POINT ( 'NONE', #895 ) ;
#39410 = DIRECTION ( 'NONE',  ( -1.000000000000000000, -1.224606353822377258E-16, -0.000000000000000000 ) ) ;
#39411 = VECTOR ( 'NONE', #93973, 1000.000000000000000 ) ;
#39412 = DIRECTION ( 'NONE',  ( -1.000000000000000000, -0.000000000000000000, -0.000000000000000000 ) ) ;
#39413 = CARTESIAN_POINT ( 'NONE',  ( 6.395403141435219929, 2.126176841940962348, 7.934999999999989839 ) ) ;
#39414 = CARTESIAN_POINT ( 'NONE',  ( 48.48921356237309510, -27.52281430457089328, 5.000000000000000000 ) ) ;
#39415 = ADVANCED_FACE ( 'NONE', ( #42312 ), #66899, .F. ) ;
#39416 = DIRECTION ( 'NONE',  ( -0.7071067811865487940, 0.7071067811865463515, -0.000000000000000000 ) ) ;
#39417 = CARTESIAN_POINT ( 'NONE',  ( 4.171830600776446296, 18.75929247661552779, 4.000000000000000000 ) ) ;
#39418 = CARTESIAN_POINT ( 'NONE',  ( 17.81601139373099940, 28.73617430169775133, 5.000000000000000000 ) ) ;
#39419 = ADVANCED_FACE ( 'NONE', ( #54606 ), #89359, .T. ) ;
#39420 = ORIENTED_EDGE ( 'NONE', *, *, #27117, .F. ) ;
#39421 = FACE_OUTER_BOUND ( 'NONE', #24060, .T. ) ;
#39422 = EDGE_CURVE ( 'NONE', #123534, #43910, #64757, .T. ) ;
#39423 = DIRECTION ( 'NONE',  ( -0.7071067811865486830, -0.7071067811865464625, 0.000000000000000000 ) ) ;
#39424 = CARTESIAN_POINT ( 'NONE',  ( 17.99451991528748351, 28.92564299267950645, 4.000000000000000000 ) ) ;
#39425 = VECTOR ( 'NONE', #49230, 999.9999999999998863 ) ;
#39426 = DIRECTION ( 'NONE',  ( 0.6830127018922180770, -0.6830127018922204085, -0.2588190451025213501 ) ) ;
#39427 = EDGE_CURVE ( 'NONE', #9541, #123638, #99060, .T. ) ;
#39428 = CARTESIAN_POINT ( 'NONE',  ( 42.64126352523145158, 4.472830434245837594, 4.472830434245841147 ) ) ;
#39429 = SHAPE_REPRESENTATION ( '1.8 Handle Rod', ( #127880 ), #114185 ) ;
#39430 = CARTESIAN_POINT ( 'NONE',  ( 184.1499999999998636, -50.24077216217758490, -35.40405119785167898 ) ) ;
#39431 = AXIS2_PLACEMENT_3D ( 'NONE', #20713, #99706, #98300 ) ;
#39432 = VERTEX_POINT ( 'NONE', #23374 ) ;
#39433 = DIRECTION ( 'NONE',  ( 0.7071067811865487940, 0.7071067811865463515, 0.000000000000000000 ) ) ;
#39434 = ORIENTED_EDGE ( 'NONE', *, *, #131201, .F. ) ;
#39435 = EDGE_CURVE ( 'NONE', #22872, #36502, #87222, .T. ) ;
#39436 = VECTOR ( 'NONE', #58384, 1000.000000000000000 ) ;
#39437 = ORIENTED_EDGE ( 'NONE', *, *, #119407, .T. ) ;
#39438 = DIRECTION ( 'NONE',  ( 0.7071067811865487940, 0.7071067811865463515, 0.000000000000000000 ) ) ;
#39439 = AXIS2_PLACEMENT_3D ( 'NONE', #92730, #137699, #81915 ) ;
#39440 = CARTESIAN_POINT ( 'NONE',  ( -21.00548008471250938, 28.92564299267923644, 4.000000000000000000 ) ) ;
#39441 = CARTESIAN_POINT ( 'NONE',  ( -22.49999999999984723, 15.05218569542901541, 5.000000000000000000 ) ) ;
#39442 = ADVANCED_FACE ( 'NONE', ( #21245 ), #132172, .T. ) ;
#39443 = FACE_OUTER_BOUND ( 'NONE', #21409, .T. ) ;
#39444 = EDGE_CURVE ( 'NONE', #124629, #43828, #9630, .T. ) ;
#39445 = CARTESIAN_POINT ( 'NONE',  ( -34.49999999999975131, -16.53574439159933718, 4.994342998332169437 ) ) ;
#39446 = SURFACE_SIDE_STYLE ('',( #5340 ) ) ;
#39447 = AXIS2_PLACEMENT_3D ( 'NONE', #39594, #62772, #106957 ) ;
#39448 = VERTEX_POINT ( 'NONE', #21952 ) ;
#39449 = LINE ( 'NONE', #18344, #46726 ) ;
#39450 = LINE ( 'NONE', #106071, #139485 ) ;
#39451 = DIRECTION ( 'NONE',  ( 0.3543493200069163240, 0.000000000000000000, 0.9351131265310288487 ) ) ;
#39452 = CARTESIAN_POINT ( 'NONE',  ( -5.475998614145474619, 22.03583458319438293, 4.979811245910087614 ) ) ;
#39453 = EDGE_CURVE ( 'NONE', #136490, #5707, #31419, .T. ) ;
#39454 = CARTESIAN_POINT ( 'NONE',  ( 15.18079593298623564, 4.202752102959690472E-16, 0.000000000000000000 ) ) ;
#39455 = CARTESIAN_POINT ( 'NONE',  ( 63.51669371712956291, 7.950000000000001066, -2.130196079827421318 ) ) ;
#39456 = CARTESIAN_POINT ( 'NONE',  ( -7.499999999999945821, -17.91344420646042934, 1.358650452708445311 ) ) ;
#39457 = AXIS2_PLACEMENT_3D ( 'NONE', #54673, #1658, #34333 ) ;
#39458 = ORIENTED_EDGE ( 'NONE', *, *, #25342, .T. ) ;
#39459 = ORIENTED_EDGE ( 'NONE', *, *, #50219, .T. ) ;
#39460 = CARTESIAN_POINT ( 'NONE',  ( 62.25000000000000000, -9.735942053221458872E-16, 7.950000000000000178 ) ) ;
#39461 = CARTESIAN_POINT ( 'NONE',  ( -5.671830600776434750, -9.740707523384186217, 4.000000000000000000 ) ) ;
#39462 = FACE_OUTER_BOUND ( 'NONE', #17740, .T. ) ;
#39463 = AXIS2_PLACEMENT_3D ( 'NONE', #1585, #132887, #64745 ) ;
#39464 = EDGE_LOOP ( 'NONE', ( #110288, #97886, #106115, #6390 ) ) ;
#39465 = PLANE ( 'NONE',  #23643 ) ;
#39466 = CARTESIAN_POINT ( 'NONE',  ( 0.9891197134605101970, -22.02621442084247505, 4.990779571109222879 ) ) ;
#39467 = CARTESIAN_POINT ( 'NONE',  ( 59.20876352523143993, -7.482591942790329030E-16, 6.110000000000001208 ) ) ;
#39468 = EDGE_CURVE ( 'NONE', #62841, #82772, #143074, .T. ) ;
#39469 = DIRECTION ( 'NONE',  ( -1.000000000000000000, -0.000000000000000000, -0.000000000000000000 ) ) ;
#39470 = ORIENTED_EDGE ( 'NONE', *, *, #77714, .T. ) ;
#39471 = ORIENTED_EDGE ( 'NONE', *, *, #12952, .F. ) ;
#39472 = VECTOR ( 'NONE', #131188, 1000.000000000000000 ) ;
#39473 = CARTESIAN_POINT ( 'NONE',  ( 0.000000000000000000, 0.000000000000000000, 5.000000000000000000 ) ) ;
#39474 = CARTESIAN_POINT ( 'NONE',  ( -25.49999999999982236, 1.466399257802255329, 5.000000000000000000 ) ) ;
#39475 = PLANE ( 'NONE',  #7273 ) ;
#39476 = CARTESIAN_POINT ( 'NONE',  ( 34.92500000000001137, 22.27000000000000668, -40.00000000000000000 ) ) ;
#39477 = DIRECTION ( 'NONE',  ( 0.7071067811865487940, 0.7071067811865463515, 0.000000000000000000 ) ) ;
#39479 = ORIENTED_EDGE ( 'NONE', *, *, #22329, .T. ) ;
#39478 = CARTESIAN_POINT ( 'NONE',  ( -17.01299345042646749, -0.9444868035190714384, -36.07450300634584295 ) ) ;
#39480 = CARTESIAN_POINT ( 'NONE',  ( 16.49999999999988276, -15.29013452822853303, 0.3645803511610747893 ) ) ;
#39481 = DIRECTION ( 'NONE',  ( -0.6830127018922180770, -0.6830127018922204085, -0.2588190451025213501 ) ) ;
#39482 = LINE ( 'NONE', #49660, #28604 ) ;
#39483 = CIRCLE ( 'NONE', #58030, 3.378199999999997871 ) ;
#39484 = CARTESIAN_POINT ( 'NONE',  ( -32.99999999999977263, -0.2811185226894649669, -5.995736974527443586 ) ) ;
#39485 = VECTOR ( 'NONE', #71858, 1000.000000000000227 ) ;
#39486 = ORIENTED_EDGE ( 'NONE', *, *, #10470, .T. ) ;
#39487 = ORIENTED_EDGE ( 'NONE', *, *, #77044, .T. ) ;
#39488 = FACE_OUTER_BOUND ( 'NONE', #71182, .T. ) ;
#39489 = CARTESIAN_POINT ( 'NONE',  ( 54.18398860626899705, 28.73617430169825226, 5.000000000000000000 ) ) ;
#39490 = LINE ( 'NONE', #28616, #135893 ) ;
#39491 = ADVANCED_FACE ( 'NONE', ( #110369 ), #75640, .F. ) ;
#39492 = CARTESIAN_POINT ( 'NONE',  ( 29.29298673570674438, -21.74070752338405654, 4.999753212805219782 ) ) ;
#39493 = PLANE ( 'NONE',  #135851 ) ;
#39494 = ORIENTED_EDGE ( 'NONE', *, *, #25417, .F. ) ;
#39495 = ORIENTED_EDGE ( 'NONE', *, *, #19793, .F. ) ;
#39496 = CARTESIAN_POINT ( 'NONE',  ( -8.999999999999937828, 2.966399257802232459, 5.000000000000000000 ) ) ;
#39498 = AXIS2_PLACEMENT_3D ( 'NONE', #89264, #47760, #32024 ) ;
#39497 = SURFACE_STYLE_USAGE ( .BOTH. , #6801 ) ;
#39499 = ORIENTED_EDGE ( 'NONE', *, *, #47686, .F. ) ;
#39500 = VECTOR ( 'NONE', #128310, 1000.000000000000114 ) ;
#39502 = ORIENTED_EDGE ( 'NONE', *, *, #65172, .T. ) ;
#39501 = CIRCLE ( 'NONE', #111276, 3.999999999999996447 ) ;
#39503 = EDGE_CURVE ( 'NONE', #113128, #115214, #8874, .T. ) ;
#39504 = CARTESIAN_POINT ( 'NONE',  ( 0.000000000000000000, 0.000000000000000000, 5.000000000000000000 ) ) ;
#39505 = VERTEX_POINT ( 'NONE', #86521 ) ;
#39506 = PLANE ( 'NONE',  #17848 ) ;
#39507 = DIRECTION ( 'NONE',  ( -0.6830127018922181881, 0.6830127018922202975, -0.2588190451025214056 ) ) ;
#39508 = AXIS2_PLACEMENT_3D ( 'NONE', #658, #44950, #89129 ) ;
#39509 = AXIS2_PLACEMENT_3D ( 'NONE', #29416, #132350, #99665 ) ;
#39510 = AXIS2_PLACEMENT_3D ( 'NONE', #41893, #98412, #8490 ) ;
#39511 = VECTOR ( 'NONE', #111496, 1000.000000000000000 ) ;
#39512 = PRESENTATION_LAYER_ASSIGNMENT (  '', '', ( #9438 ) ) ;
#39513 = EDGE_CURVE ( 'NONE', #138950, #131861, #87927, .T. ) ;
#39514 = FACE_BOUND ( 'NONE', #22741, .T. ) ;
#39515 = CARTESIAN_POINT ( 'NONE',  ( 110.0375270504628986, -9.735942053221456900E-16, 7.949999999999998401 ) ) ;
#39516 = ADVANCED_FACE ( 'NONE', ( #55319 ), #98101, .F. ) ;
#39517 = CARTESIAN_POINT ( 'NONE',  ( 30.48921356237309510, -27.52281430457076894, 5.000000000000000000 ) ) ;
#39518 = AXIS2_PLACEMENT_3D ( 'NONE', #36243, #45711, #123969 ) ;
#39520 = EDGE_LOOP ( 'NONE', ( #16817, #114596, #100515, #131491, #63965, #102052, #37163, #17945, #118788, #69591, #57437, #39857, #123204, #79300, #140216, #130887, #107822, #43226, #134048, #91395, #3964, #135300, #70008, #118662, #109119, #67990, #84114, #129438, #40287, #41830, #128402, #46327, #76254, #96716, #106671, #60283, #70495, #112274, #83080, #97884, #32263, #109024, #15943, #70674, #12079, #57448, #101541, #125506, #23258, #35447, #127873, #96328, #33409, #61096, #13433, #50280, #2381, #31998, #8970, #137266, #131930, #15536, #107820, #34408, #75955, #128409, #8342 ) ) ;
#39519 = DIRECTION ( 'NONE',  ( 1.000000000000000000, 0.000000000000000000, 0.000000000000000000 ) ) ;
#39521 = CARTESIAN_POINT ( 'NONE',  ( 24.18398860626899705, 28.73617430169804265, 5.000000000000000000 ) ) ;
#39522 = VERTEX_POINT ( 'NONE', #78492 ) ;
#39523 = ORIENTED_EDGE ( 'NONE', *, *, #41354, .T. ) ;
#39524 = CARTESIAN_POINT ( 'NONE',  ( 90.62043019189810877, 3.055000000000001936, -5.291415217122916737 ) ) ;
#39525 = ORIENTED_EDGE ( 'NONE', *, *, #132217, .F. ) ;
#39526 = CARTESIAN_POINT ( 'NONE',  ( 127.0000000000000000, 0.000000000000000000, 0.000000000000000000 ) ) ;
#39527 = VECTOR ( 'NONE', #130346, 1000.000000000000000 ) ;
#39528 = CARTESIAN_POINT ( 'NONE',  ( 45.48921356237309510, -27.52281430457087197, 5.000000000000000000 ) ) ;
#39529 = DIRECTION ( 'NONE',  ( 1.000000000000000000, 0.000000000000000000, 0.000000000000000000 ) ) ;
#39530 = VECTOR ( 'NONE', #65186, 1000.000000000000000 ) ;
#39531 = CARTESIAN_POINT ( 'NONE',  ( 45.29974487139158867, -27.71228299555237840, 4.000000000000000000 ) ) ;
#39532 = ORIENTED_EDGE ( 'NONE', *, *, #87318, .T. ) ;
#39533 = LINE ( 'NONE', #93177, #138640 ) ;
#39534 = VECTOR ( 'NONE', #53042, 1000.000000000000000 ) ;
#39535 = ADVANCED_FACE ( 'NONE', ( #164 ), #44461, .F. ) ;
#39536 = DIRECTION ( 'NONE',  ( -0.7071067811865486830, -0.7071067811865464625, 0.000000000000000000 ) ) ;
#39537 = VECTOR ( 'NONE', #46624, 1000.000000000000000 ) ;
#39538 = CARTESIAN_POINT ( 'NONE',  ( -8.994519915287490619, 28.92564299267944250, 4.000000000000000000 ) ) ;
#39539 = CARTESIAN_POINT ( 'NONE',  ( 180.6620941962882227, -49.11927476322659203, -40.22110306067541075 ) ) ;
#39540 = FACE_OUTER_BOUND ( 'NONE', #26104, .T. ) ;
#39541 = ORIENTED_EDGE ( 'NONE', *, *, #130567, .F. ) ;
#39542 = VECTOR ( 'NONE', #72966, 1000.000000000000000 ) ;
#39543 = LINE ( 'NONE', #62011, #58896 ) ;
#39544 = CARTESIAN_POINT ( 'NONE',  ( 3.710381658649933634, 4.584330080086930965E-16, 0.000000000000000000 ) ) ;
#39545 = ORIENTED_EDGE ( 'NONE', *, *, #112721, .F. ) ;
#39546 = EDGE_CURVE ( 'NONE', #27314, #71394, #100243, .T. ) ;
#39547 = ORIENTED_EDGE ( 'NONE', *, *, #37425, .T. ) ;
#39548 = CIRCLE ( 'NONE', #127590, 5.968999999999998529 ) ;
#39549 = EDGE_CURVE ( 'NONE', #16517, #19682, #135046, .T. ) ;
#39550 = ORIENTED_EDGE ( 'NONE', *, *, #91855, .F. ) ;
#39551 = CARTESIAN_POINT ( 'NONE',  ( 40.54209685856477563, 5.291415217122923842, -3.054999999999996163 ) ) ;
#39552 = ORIENTED_EDGE ( 'NONE', *, *, #14145, .T. ) ;
#39553 = AXIS2_PLACEMENT_3D ( 'NONE', #40327, #142479, #128730 ) ;
#39554 = CARTESIAN_POINT ( 'NONE',  ( 14.33747294953710494, 6.094999999999989981, -1.119633336120465690E-15 ) ) ;
#39555 = CARTESIAN_POINT ( 'NONE',  ( -17.51947408101518633, 4.682391862010510053, -29.48234182121950653 ) ) ;
#39556 = ORIENTED_EDGE ( 'NONE', *, *, #119091, .F. ) ;
#39557 = CARTESIAN_POINT ( 'NONE',  ( -32.99999999999976552, -0.4125381241607533611, 4.000000000000000000 ) ) ;
#39558 = ORIENTED_EDGE ( 'NONE', *, *, #81225, .T. ) ;
#39559 = DIRECTION ( 'NONE',  ( -0.7071067811865487940, 0.7071067811865463515, -0.000000000000000000 ) ) ;
#39560 = AXIS2_PLACEMENT_3D ( 'NONE', #1424, #101475, #36931 ) ;
#39561 = FACE_OUTER_BOUND ( 'NONE', #116664, .T. ) ;
#39563 = ORIENTED_EDGE ( 'NONE', *, *, #74083, .F. ) ;
#39562 = PLANE ( 'NONE',  #81863 ) ;
#39564 = ORIENTED_EDGE ( 'NONE', *, *, #114012, .F. ) ;
#39565 = EDGE_CURVE ( 'NONE', #16785, #55534, #69057, .T. ) ;
#39566 = LINE ( 'NONE', #83796, #123315 ) ;
#39567 = LINE ( 'NONE', #126536, #4379 ) ;
#39568 = EDGE_LOOP ( 'NONE', ( #140537, #114922, #111367, #128076 ) ) ;
#39569 = DIRECTION ( 'NONE',  ( 0.7071067811865487940, 0.7071067811865463515, 0.000000000000000000 ) ) ;
#39570 = ORIENTED_EDGE ( 'NONE', *, *, #118922, .F. ) ;
#39571 = ORIENTED_EDGE ( 'NONE', *, *, #53589, .T. ) ;
#39572 = ORIENTED_EDGE ( 'NONE', *, *, #64232, .T. ) ;
#39573 = ORIENTED_EDGE ( 'NONE', *, *, #448, .F. ) ;
#39574 = DIRECTION ( 'NONE',  ( -1.000000000000000000, 0.000000000000000000, 0.000000000000000000 ) ) ;
#39575 = VECTOR ( 'NONE', #20815, 1000.000000000000000 ) ;
#39576 = PLANE ( 'NONE',  #139513 ) ;
#39577 = PLANE ( 'NONE',  #26281 ) ;
#39578 = CARTESIAN_POINT ( 'NONE',  ( -7.140000000000001457, -39.92999999999999261, 18.93259187797432475 ) ) ;
#39579 = ORIENTED_EDGE ( 'NONE', *, *, #103395, .F. ) ;
#39580 = CARTESIAN_POINT ( 'NONE',  ( -11.20710678118646442, -20.24070752338407431, 5.000000000000000000 ) ) ;
#39581 = ORIENTED_EDGE ( 'NONE', *, *, #89660, .F. ) ;
#39582 = AXIS2_PLACEMENT_3D ( 'NONE', #118391, #130739, #53131 ) ;
#39583 = VECTOR ( 'NONE', #21737, 999.9999999999998863 ) ;
#39584 = CARTESIAN_POINT ( 'NONE',  ( -32.99451991528749062, 28.92564299267960948, 4.000000000000000000 ) ) ;
#39585 = CARTESIAN_POINT ( 'NONE',  ( 27.83290314143522437, -3.967499999999994476, 6.871911579029513106 ) ) ;
#39586 = DIRECTION ( 'NONE',  ( -0.7071067811865486830, 0.7071067811865464625, 0.000000000000000000 ) ) ;
#39587 = ADVANCED_FACE ( 'NONE', ( #57473 ), #126808, .T. ) ;
#39588 = LINE ( 'NONE', #106953, #55340 ) ;
#39589 = DIRECTION ( 'NONE',  ( 0.000000000000000000, -1.000000000000000000, 0.000000000000000000 ) ) ;
#39590 = ORIENTED_EDGE ( 'NONE', *, *, #132201, .F. ) ;
#39591 = EDGE_CURVE ( 'NONE', #18615, #57817, #4414, .T. ) ;
#39592 = VERTEX_POINT ( 'NONE', #59617 ) ;
#39593 = VERTEX_POINT ( 'NONE', #113237 ) ;
#39594 = CARTESIAN_POINT ( 'NONE',  ( -63.48921356237309510, -27.52281430457099631, 5.000000000000000000 ) ) ;
#39595 = FACE_OUTER_BOUND ( 'NONE', #134069, .T. ) ;
#39596 = DIRECTION ( 'NONE',  ( -0.7071067811865486830, -0.7071067811865464625, -0.000000000000000000 ) ) ;
#39597 = LINE ( 'NONE', #130169, #31240 ) ;
#39598 = AXIS2_PLACEMENT_3D ( 'NONE', #24572, #67397, #1368 ) ;
#39599 = CARTESIAN_POINT ( 'NONE',  ( 0.3339215173231541711, -51.89584459748878942, -39.24672819827818415 ) ) ;
#39600 = EDGE_CURVE ( 'NONE', #88422, #26808, #56781, .T. ) ;
#39602 = ADVANCED_FACE ( 'NONE', ( #100940 ), #79958, .F. ) ;
#39601 = CARTESIAN_POINT ( 'NONE',  ( 77.05793019189810877, 6.110000000000001208, -1.637169565754156286 ) ) ;
#39603 = CARTESIAN_POINT ( 'NONE',  ( 81.49999999999998579, 0.000000000000000000, -7.950000000000000178 ) ) ;
#39604 = AXIS2_PLACEMENT_3D ( 'NONE', #50409, #72199, #27930 ) ;
#39605 = VECTOR ( 'NONE', #12191, 1000.000000000000000 ) ;
#39606 = DIRECTION ( 'NONE',  ( -0.3543493200069162685, -0.000000000000000000, -0.9351131265310288487 ) ) ;
#39607 = CARTESIAN_POINT ( 'NONE',  ( -24.48921356237309510, -27.52281430457072631, 5.000000000000000000 ) ) ;
#39608 = DIRECTION ( 'NONE',  ( -0.7071067811865486830, -0.7071067811865464625, 0.000000000000000000 ) ) ;
#39609 = SPHERICAL_SURFACE ( 'NONE', #99723, 0.5000000000000000000 ) ;
#39610 = VERTEX_POINT ( 'NONE', #136422 ) ;
#39611 = AXIS2_PLACEMENT_3D ( 'NONE', #31366, #140810, #129964 ) ;
#39612 = VECTOR ( 'NONE', #119274, 1000.000000000000000 ) ;
#39613 = VECTOR ( 'NONE', #5126, 1000.000000000000114 ) ;
#39615 = CARTESIAN_POINT ( 'NONE',  ( 33.18398860626899705, 28.73617430169810305, 5.000000000000000000 ) ) ;
#39614 = CONICAL_SURFACE ( 'NONE', #141418, 2.055000000000000604, 0.9599310885968764806 ) ;
#39616 = ORIENTED_EDGE ( 'NONE', *, *, #33959, .F. ) ;
#39617 = AXIS2_PLACEMENT_3D ( 'NONE', #26522, #114912, #25070 ) ;
#39618 = DIRECTION ( 'NONE',  ( -0.000000000000000000, -0.3543493200069152693, 0.9351131265310292928 ) ) ;
#39620 = ORIENTED_EDGE ( 'NONE', *, *, #74954, .F. ) ;
#39619 = CARTESIAN_POINT ( 'NONE',  ( 51.48921356237309510, -27.52281430457091460, 5.000000000000000000 ) ) ;
#39621 = EDGE_CURVE ( 'NONE', #106357, #59504, #135728, .T. ) ;
#39622 = EDGE_CURVE ( 'NONE', #70428, #62641, #105989, .T. ) ;
#39623 = DIRECTION ( 'NONE',  ( -0.6830127018922181881, 0.6830127018922202975, -0.2588190451025214056 ) ) ;
#39624 = DIRECTION ( 'NONE',  ( -0.7071067811865486830, 0.7071067811865464625, 0.000000000000000000 ) ) ;
#39625 = EDGE_LOOP ( 'NONE', ( #100922, #117835, #40707, #112912 ) ) ;
#39626 = EDGE_LOOP ( 'NONE', ( #103296, #63483, #18204, #35650 ) ) ;
#39627 = CARTESIAN_POINT ( 'NONE',  ( -11.70025512860841133, -27.71228299555198049, 4.000000000000000000 ) ) ;
#39628 = CYLINDRICAL_SURFACE ( 'NONE', #12040, 1.000000000000000888 ) ;
#39629 = VECTOR ( 'NONE', #132558, 1000.000000000000000 ) ;
#39630 = CARTESIAN_POINT ( 'NONE',  ( 176.2838169021916599, 7.919999999999943086, 19.12499999999998224 ) ) ;
#39631 = ADVANCED_FACE ( 'NONE', ( #124129 ), #112538, .F. ) ;
#39632 = CARTESIAN_POINT ( 'NONE',  ( 97.20419371712955581, -6.884901960086285300, -3.975000000000000089 ) ) ;
#39633 = CARTESIAN_POINT ( 'NONE',  ( 26.99999999999981171, 7.931123077392104648, 4.000000000000000000 ) ) ;
#39634 = LINE ( 'NONE', #95406, #136271 ) ;
#39635 = ORIENTED_EDGE ( 'NONE', *, *, #20559, .T. ) ;
#39636 = VECTOR ( 'NONE', #14170, 1000.000000000000000 ) ;
#39637 = PLANE ( 'NONE',  #23811 ) ;
#39638 = DIRECTION ( 'NONE',  ( -0.000000000000000000, -0.3543493200069152138, 0.9351131265310292928 ) ) ;
#39639 = CARTESIAN_POINT ( 'NONE',  ( 21.29166666666666785, -3.047499999999994547, 5.278424836066145431 ) ) ;
#39640 = PRESENTATION_LAYER_ASSIGNMENT (  '', '', ( #58180 ) ) ;
#39641 = ADVANCED_FACE ( 'NONE', ( #36413 ), #13914, .F. ) ;
#39642 = CARTESIAN_POINT ( 'NONE',  ( 28.49999999999980815, -16.53360074219757081, 5.000000000000000000 ) ) ;
#39643 = ORIENTED_EDGE ( 'NONE', *, *, #56085, .T. ) ;
#39644 = VECTOR ( 'NONE', #24161, 1000.000000000000227 ) ;
#39645 = CARTESIAN_POINT ( 'NONE',  ( 46.89169371712956291, 2.130196079827421762, 7.950000000000000178 ) ) ;
#39646 = VERTEX_POINT ( 'NONE', #12500 ) ;
#39647 = VECTOR ( 'NONE', #86548, 1000.000000000000000 ) ;
#39648 = CARTESIAN_POINT ( 'NONE',  ( 84.58376352523144703, -6.110000000000001208, -3.741295971395164515E-16 ) ) ;
#39649 = AXIS2_PLACEMENT_3D ( 'NONE', #29687, #118106, #18814 ) ;
#39650 = CARTESIAN_POINT ( 'NONE',  ( -31.17183060077626067, -8.240707523384200428, 4.000000000000000000 ) ) ;
#39651 = EDGE_CURVE ( 'NONE', #48429, #112121, #114661, .T. ) ;
#39652 = CARTESIAN_POINT ( 'NONE',  ( 122.6835989386367771, -57.15000000000008384, -34.92499999999998295 ) ) ;
#39653 = PLANE ( 'NONE',  #38589 ) ;
#39654 = VERTEX_POINT ( 'NONE', #58214 ) ;
#39655 = AXIS2_PLACEMENT_3D ( 'NONE', #58183, #105199, #13881 ) ;
#39656 = PLANE ( 'NONE',  #74275 ) ;
#39657 = DIRECTION ( 'NONE',  ( -0.7071067811865486830, -0.7071067811865464625, 0.000000000000000000 ) ) ;
#39660 = ADVANCED_FACE ( 'NONE', ( #80643 ), #102405, .F. ) ;
#39659 = EDGE_LOOP ( 'NONE', ( #38334, #130997, #125077, #82892 ) ) ;
#39658 = LINE ( 'NONE', #139693, #119245 ) ;
#39661 = DIRECTION ( 'NONE',  ( -0.7071067811865487940, 0.7071067811865463515, 0.000000000000000000 ) ) ;
#39662 = DIRECTION ( 'NONE',  ( -0.000000000000000000, -0.3543493200069152693, 0.9351131265310292928 ) ) ;
#39663 = CARTESIAN_POINT ( 'NONE',  ( 59.04166666666665719, -3.975000000000002753, 6.884901960086286188 ) ) ;
#39664 = VERTEX_POINT ( 'NONE', #25516 ) ;
#39665 = EDGE_CURVE ( 'NONE', #54723, #128366, #101655, .T. ) ;
#39666 = ORIENTED_EDGE ( 'NONE', *, *, #87568, .T. ) ;
#39667 = CARTESIAN_POINT ( 'NONE',  ( 69.85459685856476142, -1.637169565754161615, 6.110000000000000320 ) ) ;
#39668 = EDGE_LOOP ( 'NONE', ( #68454, #84822, #51662, #3007 ) ) ;
#39669 = CARTESIAN_POINT ( 'NONE',  ( 0.000000000000000000, -21.72500000000000142, 4.500000000000000888 ) ) ;
#39670 = CONICAL_SURFACE ( 'NONE', #129883, 2.500000000000000888, 0.9599310885968822538 ) ;
#39671 = LINE ( 'NONE', #73027, #96594 ) ;
#39672 = DIRECTION ( 'NONE',  ( 0.7071067811865487940, 0.7071067811865463515, 0.000000000000000000 ) ) ;
#39673 = VERTEX_POINT ( 'NONE', #58935 ) ;
#39674 = VECTOR ( 'NONE', #33198, 1000.000000000000000 ) ;
#39675 = LINE ( 'NONE', #131666, #127929 ) ;
#39676 = CARTESIAN_POINT ( 'NONE',  ( 14.74000000000000021, -2.055000000000000160, 2.789133085058098087E-16 ) ) ;
#39677 = EDGE_LOOP ( 'NONE', ( #13093, #66036, #18850 ) ) ;
#39678 = EDGE_CURVE ( 'NONE', #103755, #5851, #47346, .T. ) ;
#39679 = DIRECTION ( 'NONE',  ( -0.000000000000000000, 0.3543493200069153248, 0.9351131265310292928 ) ) ;
#39680 = AXIS2_PLACEMENT_3D ( 'NONE', #22291, #34644, #14835 ) ;
#39681 = DIRECTION ( 'NONE',  ( 0.7071067811865487940, 0.7071067811865463515, -0.000000000000000000 ) ) ;
#39682 = CARTESIAN_POINT ( 'NONE',  ( -33.70710678118631165, 2.259292476615694323, 5.000000000000000000 ) ) ;
#39683 = VECTOR ( 'NONE', #11169, 999.9999999999998863 ) ;
#39684 = ORIENTED_EDGE ( 'NONE', *, *, #28723, .F. ) ;
#39685 = ORIENTED_EDGE ( 'NONE', *, *, #72810, .T. ) ;
#39686 = ADVANCED_FACE ( 'NONE', ( #37116 ), #81371, .F. ) ;
#39687 = DIRECTION ( 'NONE',  ( -0.7071067811865486830, -0.7071067811865464625, 0.000000000000000000 ) ) ;
#39688 = DIRECTION ( 'NONE',  ( 0.6830127018922180770, -0.6830127018922204085, -0.2588190451025213501 ) ) ;
#39689 = DIRECTION ( 'NONE',  ( 0.3543493200069162685, -0.000000000000000000, -0.9351131265310288487 ) ) ;
#39690 = CARTESIAN_POINT ( 'NONE',  ( -2.483345613589531542, 22.22500000000000142, 4.500000000000000888 ) ) ;
#39691 = VECTOR ( 'NONE', #89883, 1000.000000000000000 ) ;
#39692 = PLANE ( 'NONE',  #37262 ) ;
#39693 = ORIENTED_EDGE ( 'NONE', *, *, #17255, .T. ) ;
#39694 = VERTEX_POINT ( 'NONE', #84230 ) ;
#39695 = ORIENTED_EDGE ( 'NONE', *, *, #77882, .F. ) ;
#39696 = ORIENTED_EDGE ( 'NONE', *, *, #81767, .T. ) ;
#39697 = ADVANCED_FACE ( 'NONE', ( #140025 ), #16794, .F. ) ;
#39698 = AXIS2_PLACEMENT_3D ( 'NONE', #4018, #50455, #93229 ) ;
#39699 = DIRECTION ( 'NONE',  ( 0.7071067811865487940, 0.7071067811865463515, 0.000000000000000000 ) ) ;
#39700 = VECTOR ( 'NONE', #103857, 1000.000000000000000 ) ;
#39701 = VECTOR ( 'NONE', #63425, 1000.000000000000000 ) ;
#39702 = VERTEX_POINT ( 'NONE', #61072 ) ;
#39703 = LINE ( 'NONE', #50555, #6523 ) ;
#39704 = FACE_OUTER_BOUND ( 'NONE', #105960, .T. ) ;
#39705 = EDGE_CURVE ( 'NONE', #140963, #98610, #50152, .T. ) ;
#39706 = CARTESIAN_POINT ( 'NONE',  ( 26.40000000000000568, -18.48000000000005372, 33.92499999999998295 ) ) ;
#39707 = DIRECTION ( 'NONE',  ( -0.7071067811865487940, 0.7071067811865463515, 0.000000000000000000 ) ) ;
#39708 = AXIS2_PLACEMENT_3D ( 'NONE', #129061, #56565, #45667 ) ;
#39709 = VECTOR ( 'NONE', #68696, 1000.000000000000000 ) ;
#39710 = AXIS2_PLACEMENT_3D ( 'NONE', #107150, #41921, #21589 ) ;
#39711 = CIRCLE ( 'NONE', #221, 2.500000000000000444 ) ;
#39712 = FACE_OUTER_BOUND ( 'NONE', #3253, .T. ) ;
#39713 = ORIENTED_EDGE ( 'NONE', *, *, #105470, .F. ) ;
#39714 = VECTOR ( 'NONE', #101039, 1000.000000000000000 ) ;
#39715 = LINE ( 'NONE', #83943, #137392 ) ;
#39716 = CARTESIAN_POINT ( 'NONE',  ( 25.39999999999999858, -2.600000000000012523, -20.40202195861969159 ) ) ;
#39717 = VERTEX_POINT ( 'NONE', #129119 ) ;
#39718 = EDGE_CURVE ( 'NONE', #87654, #84329, #29101, .T. ) ;
#39719 = FACE_OUTER_BOUND ( 'NONE', #25927, .T. ) ;
#39720 = ORIENTED_EDGE ( 'NONE', *, *, #68388, .F. ) ;
#39722 = ADVANCED_FACE ( 'NONE', ( #8034 ), #16037, .F. ) ;
#39721 = CARTESIAN_POINT ( 'NONE',  ( -9.411614905948246346, 22.22500000000000142, 4.777194822843814137 ) ) ;
#39723 = ORIENTED_EDGE ( 'NONE', *, *, #92350, .F. ) ;
#39724 = EDGE_LOOP ( 'NONE', ( #75385, #8118, #57232, #88248 ) ) ;
#39725 = VECTOR ( 'NONE', #138058, 1000.000000000000000 ) ;
#39726 = CARTESIAN_POINT ( 'NONE',  ( 68.83376352523143282, 6.110000000000001208, 1.122388791418549305E-15 ) ) ;
#39727 = ORIENTED_EDGE ( 'NONE', *, *, #74348, .F. ) ;
#39728 = CARTESIAN_POINT ( 'NONE',  ( -17.20666063542140378, 21.75929247661549937, 4.998822639870711626 ) ) ;
#39729 = CARTESIAN_POINT ( 'NONE',  ( 104.7087635252314328, -7.482591942790329030E-16, 6.110000000000001208 ) ) ;
#39730 = CARTESIAN_POINT ( 'NONE',  ( -71.99451991528749772, 28.92564299267988304, 4.000000000000000000 ) ) ;
#39731 = ADVANCED_FACE ( 'NONE', ( #62458 ), #74038, .T. ) ;
#39732 = VECTOR ( 'NONE', #101010, 1000.000000000000000 ) ;
#39733 = FACE_OUTER_BOUND ( 'NONE', #76554, .T. ) ;
#39734 = PLANE ( 'NONE',  #53349 ) ;
#39735 = DIRECTION ( 'NONE',  ( 1.000000000000000000, 0.000000000000000000, 0.000000000000000000 ) ) ;
#39736 = FACE_OUTER_BOUND ( 'NONE', #134461, .T. ) ;
#39737 = ADVANCED_FACE ( 'NONE', ( #115350 ), #5883, .F. ) ;
#39738 = AXIS2_PLACEMENT_3D ( 'NONE', #92077, #125448, #137029 ) ;
#39739 = DIRECTION ( 'NONE',  ( 0.7071067811865487940, 0.7071067811865463515, -0.000000000000000000 ) ) ;
#39740 = VERTEX_POINT ( 'NONE', #128426 ) ;
#39741 = VECTOR ( 'NONE', #10042, 1000.000000000000000 ) ;
#39742 = CARTESIAN_POINT ( 'NONE',  ( 33.18398860626899705, 28.73617430169810305, 5.000000000000000000 ) ) ;
#39743 = LINE ( 'NONE', #49190, #91482 ) ;
#39744 = ORIENTED_EDGE ( 'NONE', *, *, #115611, .T. ) ;
#39745 = AXIS2_PLACEMENT_3D ( 'NONE', #18275, #62551, #106725 ) ;
#39746 = ORIENTED_EDGE ( 'NONE', *, *, #73880, .T. ) ;
#39747 = CARTESIAN_POINT ( 'NONE',  ( 114.5583603837962272, -7.949999999999996625, -2.130196079827426203 ) ) ;
#39748 = ADVANCED_FACE ( 'NONE', ( #18183 ), #73339, .F. ) ;
#39749 = ORIENTED_EDGE ( 'NONE', *, *, #4315, .T. ) ;
#39750 = AXIS2_PLACEMENT_3D ( 'NONE', #52085, #118755, #19450 ) ;
#39751 = DIRECTION ( 'NONE',  ( 0.7071067811865487940, 0.7071067811865463515, -0.000000000000000000 ) ) ;
#39752 = CARTESIAN_POINT ( 'NONE',  ( -28.96836484077790885, 2.259292476615697876, 13.77329220150630462 ) ) ;
#39753 = VECTOR ( 'NONE', #136221, 1000.000000000000000 ) ;
#39754 = CARTESIAN_POINT ( 'NONE',  ( -25.39999999999996305, 0.000000000000000000, 0.000000000000000000 ) ) ;
#39755 = DIRECTION ( 'NONE',  ( -0.7071067811865487940, 0.7071067811865463515, 0.000000000000000000 ) ) ;
#39756 = ORIENTED_EDGE ( 'NONE', *, *, #86468, .T. ) ;
#39757 = ORIENTED_EDGE ( 'NONE', *, *, #26455, .F. ) ;
#39758 = EDGE_CURVE ( 'NONE', #46491, #20610, #41394, .T. ) ;
#39759 = CARTESIAN_POINT ( 'NONE',  ( 0.1245698081018860176, -6.871911579029512218, 3.967499999999996252 ) ) ;
#39760 = LINE ( 'NONE', #39019, #49002 ) ;
#39761 = CYLINDRICAL_SURFACE ( 'NONE', #103723, 0.5000000000000004441 ) ;
#39762 = CARTESIAN_POINT ( 'NONE',  ( 32.67183060077624646, 20.25929247661551003, 4.000000000000000000 ) ) ;
#39763 = VERTEX_POINT ( 'NONE', #26950 ) ;
#39764 = EDGE_CURVE ( 'NONE', #129163, #119037, #105917, .T. ) ;
#39765 = EDGE_LOOP ( 'NONE', ( #123810, #98735, #16989, #28083 ) ) ;
#39766 = VECTOR ( 'NONE', #80492, 1000.000000000000000 ) ;
#39767 = ORIENTED_EDGE ( 'NONE', *, *, #24609, .F. ) ;
#39768 = DIRECTION ( 'NONE',  ( -0.000000000000000000, 1.000000000000000000, -0.000000000000000000 ) ) ;
#39769 = PLANE ( 'NONE',  #64967 ) ;
#39770 = CARTESIAN_POINT ( 'NONE',  ( -1.499999999999987566, -8.947814304570737676, 5.000000000000000000 ) ) ;
#39771 = AXIS2_PLACEMENT_3D ( 'NONE', #25480, #11017, #33556 ) ;
#39772 = DIRECTION ( 'NONE',  ( 0.7071067811865487940, -0.7071067811865463515, 0.000000000000000000 ) ) ;
#39773 = CARTESIAN_POINT ( 'NONE',  ( -36.48921356237310221, -27.52281430457080802, 5.000000000000000000 ) ) ;
#39774 = ADVANCED_FACE ( 'NONE', ( #38554 ), #82781, .F. ) ;
#39775 = EDGE_CURVE ( 'NONE', #118193, #99040, #118955, .T. ) ;
#39776 = CARTESIAN_POINT ( 'NONE',  ( -34.49999999999976552, -9.462702396501047275, -9.474982329943436810 ) ) ;
#39777 = DIRECTION ( 'NONE',  ( -0.6830127018922180770, -0.6830127018922204085, -0.2588190451025213501 ) ) ;
#39778 = LINE ( 'NONE', #40488, #72233 ) ;
#39780 = AXIS2_PLACEMENT_3D ( 'NONE', #115794, #27377, #74501 ) ;
#39779 = CARTESIAN_POINT ( 'NONE',  ( 33.48921356237309510, -27.52281430457078670, 5.000000000000000000 ) ) ;
#39781 = ORIENTED_EDGE ( 'NONE', *, *, #75441, .T. ) ;
#39782 = LINE ( 'NONE', #71678, #55666 ) ;
#39783 = VECTOR ( 'NONE', #31367, 1000.000000000000000 ) ;
#39785 = EDGE_CURVE ( 'NONE', #94195, #8957, #10189, .T. ) ;
#39784 = DIRECTION ( 'NONE',  ( 0.7071067811865487940, 0.7071067811865463515, 0.000000000000000000 ) ) ;
#39786 = EDGE_LOOP ( 'NONE', ( #112421, #141220, #63614 ) ) ;
#39787 = LINE ( 'NONE', #95555, #11237 ) ;
#39789 = ORIENTED_EDGE ( 'NONE', *, *, #70095, .T. ) ;
#39788 = CARTESIAN_POINT ( 'NONE',  ( 55.64345981607718983, -48.97294124528584547, -39.12804664298375457 ) ) ;
#39790 = EDGE_CURVE ( 'NONE', #12370, #34226, #44286, .T. ) ;
#39791 = ADVANCED_FACE ( 'NONE', ( #64586 ), #119642, .F. ) ;
#39792 = PLANE ( 'NONE',  #42281 ) ;
#39793 = LINE ( 'NONE', #50637, #71600 ) ;
#39795 = ORIENTED_EDGE ( 'NONE', *, *, #131111, .F. ) ;
#39794 = CONICAL_SURFACE ( 'NONE', #88320, 2.055000000000001048, 0.9599310885968758145 ) ;
#39796 = CARTESIAN_POINT ( 'NONE',  ( 149.2199999999997999, -3.180000000000061444, 31.92499999999998295 ) ) ;
#39797 = VERTEX_POINT ( 'NONE', #66733 ) ;
#39798 = LINE ( 'NONE', #38346, #91559 ) ;
#39799 = CARTESIAN_POINT ( 'NONE',  ( 126.3708603837962130, 6.884901960086289741, -3.974999999999993427 ) ) ;
#39800 = EDGE_CURVE ( 'NONE', #100733, #61244, #62198, .T. ) ;
#39801 = DIRECTION ( 'NONE',  ( 1.000000000000000000, 0.000000000000000000, 0.000000000000000000 ) ) ;
#39802 = ADVANCED_FACE ( 'NONE', ( #121095 ), #66238, .T. ) ;
#39803 = DIRECTION ( 'NONE',  ( 0.7071067811865486830, -0.7071067811865464625, -0.000000000000000000 ) ) ;
#39804 = DIRECTION ( 'NONE',  ( 0.3543493200069162685, -0.000000000000000000, -0.9351131265310288487 ) ) ;
#39805 = FACE_OUTER_BOUND ( 'NONE', #53376, .T. ) ;
#39806 = DIRECTION ( 'NONE',  ( 0.000000000000000000, -1.000000000000000000, 0.000000000000000000 ) ) ;
#39807 = CARTESIAN_POINT ( 'NONE',  ( 28.41623647476855652, -7.934999999999990727, 4.858786175617117713E-16 ) ) ;
#39808 = CARTESIAN_POINT ( 'NONE',  ( 12.37456980810188512, 6.871911579029510442, -3.967499999999998916 ) ) ;
#39809 = LINE ( 'NONE', #16575, #13518 ) ;
#39811 = EDGE_CURVE ( 'NONE', #128354, #132699, #33426, .T. ) ;
#39810 = VECTOR ( 'NONE', #48865, 1000.000000000000000 ) ;
#39812 = VECTOR ( 'NONE', #89289, 1000.000000000000114 ) ;
#39813 = CARTESIAN_POINT ( 'NONE',  ( -24.29974487139158867, -27.71228299555223273, 4.000000000000000000 ) ) ;
#39814 = CARTESIAN_POINT ( 'NONE',  ( -5.994519915287488843, 28.92564299267942118, 4.000000000000000000 ) ) ;
#39815 = ORIENTED_EDGE ( 'NONE', *, *, #87487, .T. ) ;
#39816 = ORIENTED_EDGE ( 'NONE', *, *, #95832, .F. ) ;
#39817 = VECTOR ( 'NONE', #57048, 999.9999999999998863 ) ;
#39818 = CARTESIAN_POINT ( 'NONE',  ( 78.29166666666665719, 3.975000000000003642, -6.884901960086285300 ) ) ;
#39819 = VECTOR ( 'NONE', #132787, 1000.000000000000000 ) ;
#39820 = DIRECTION ( 'NONE',  ( -0.7071067811865486830, -0.7071067811865464625, -0.000000000000000000 ) ) ;
#39821 = VERTEX_POINT ( 'NONE', #42144 ) ;
#39822 = PLANE ( 'NONE',  #24864 ) ;
#39823 = LINE ( 'NONE', #39076, #41791 ) ;
#39824 = AXIS2_PLACEMENT_3D ( 'NONE', #81728, #136779, #125924 ) ;
#39825 = EDGE_CURVE ( 'NONE', #113508, #48675, #109514, .T. ) ;
#39826 = MECHANICAL_DESIGN_GEOMETRIC_PRESENTATION_REPRESENTATION (  '', ( #90725 ), #14333 ) ;
#39827 = FACE_OUTER_BOUND ( 'NONE', #81750, .T. ) ;
#39828 = ORIENTED_EDGE ( 'NONE', *, *, #69861, .T. ) ;
#39829 = CARTESIAN_POINT ( 'NONE',  ( -9.489213562373095101, -27.52281430457062328, 5.000000000000000000 ) ) ;
#39830 = DIRECTION ( 'NONE',  ( 0.000000000000000000, 1.000000000000000000, -3.469446951953614189E-15 ) ) ;
#39831 = CARTESIAN_POINT ( 'NONE',  ( 29.58838509405148542, 22.22500000000000142, 4.777194822843815913 ) ) ;
#39832 = CARTESIAN_POINT ( 'NONE',  ( 21.76000000000000156, 2.055000000000001492, 0.000000000000000000 ) ) ;
#39833 = DIRECTION ( 'NONE',  ( 1.000000000000000000, 0.000000000000000000, 0.000000000000000000 ) ) ;
#39834 = DIRECTION ( 'NONE',  ( -0.000000000000000000, 0.000000000000000000, 1.000000000000000000 ) ) ;
#39835 = EDGE_CURVE ( 'NONE', #139444, #42123, #88498, .T. ) ;
#39836 = DIRECTION ( 'NONE',  ( -0.6830127018922181881, 0.6830127018922202975, -0.2588190451025214056 ) ) ;
#39837 = PLANE ( 'NONE',  #111792 ) ;
#39838 = PLANE ( 'NONE',  #107888 ) ;
#39839 = DIRECTION ( 'NONE',  ( 0.000000000000000000, -1.000000000000000000, 0.000000000000000000 ) ) ;
#39840 = CARTESIAN_POINT ( 'NONE',  ( 60.76962477604072177, -44.19516442796815170, 34.92499999999998295 ) ) ;
#39841 = EDGE_CURVE ( 'NONE', #118711, #125243, #142169, .T. ) ;
#39842 = ORIENTED_EDGE ( 'NONE', *, *, #74287, .F. ) ;
#39843 = ORIENTED_EDGE ( 'NONE', *, *, #94807, .T. ) ;
#39844 = CARTESIAN_POINT ( 'NONE',  ( 98.14626352523144703, -4.472830434245840259, 4.472830434245839371 ) ) ;
#39845 = ORIENTED_EDGE ( 'NONE', *, *, #107708, .F. ) ;
#39846 = DIRECTION ( 'NONE',  ( -0.7071067811865486830, 0.7071067811865464625, 0.000000000000000000 ) ) ;
#39847 = ORIENTED_EDGE ( 'NONE', *, *, #7110, .T. ) ;
#39848 = EDGE_CURVE ( 'NONE', #8196, #42180, #729, .T. ) ;
#39849 = CARTESIAN_POINT ( 'NONE',  ( 29.20710678118634007, 9.759292476615620160, 5.000000000000000000 ) ) ;
#39850 = PLANE ( 'NONE',  #95143 ) ;
#39851 = VECTOR ( 'NONE', #87482, 999.9999999999998863 ) ;
#39852 = CIRCLE ( 'NONE', #55997, 2.552699999999994418 ) ;
#39853 = CARTESIAN_POINT ( 'NONE',  ( 90.76626352523146579, 4.472830434245839371, -4.472830434245838482 ) ) ;
#39854 = ORIENTED_EDGE ( 'NONE', *, *, #23546, .F. ) ;
#39855 = VECTOR ( 'NONE', #120263, 1000.000000000000227 ) ;
#39856 = CARTESIAN_POINT ( 'NONE',  ( -22.82816939922336630, 18.75929247661553845, 4.000000000000000000 ) ) ;
#39857 = ORIENTED_EDGE ( 'NONE', *, *, #2876, .F. ) ;
#39858 = CARTESIAN_POINT ( 'NONE',  ( 23.55512991947088963, -0.7407075233842735917, 4.307968247157003994 ) ) ;
#39859 = LINE ( 'NONE', #29640, #35656 ) ;
#39860 = VECTOR ( 'NONE', #14660, 1000.000000000000000 ) ;
#39861 = DIRECTION ( 'NONE',  ( -0.000000000000000000, -0.3543493200069152693, 0.9351131265310292928 ) ) ;
#39862 = ORIENTED_EDGE ( 'NONE', *, *, #140064, .F. ) ;
#39863 = VERTEX_POINT ( 'NONE', #55148 ) ;
#39864 = ORIENTED_EDGE ( 'NONE', *, *, #58949, .T. ) ;
#39865 = CARTESIAN_POINT ( 'NONE',  ( -12.48921356237309155, -27.52281430457064104, 5.000000000000000000 ) ) ;
#39866 = CARTESIAN_POINT ( 'NONE',  ( -29.99999999999978684, 8.966399257802176948, 5.000000000000000000 ) ) ;
#39867 = CARTESIAN_POINT ( 'NONE',  ( 6.046236474768552860, -7.934999999999990727, 4.858786175617117713E-16 ) ) ;
#39868 = AXIS2_PLACEMENT_3D ( 'NONE', #42212, #74111, #73408 ) ;
#39869 = CARTESIAN_POINT ( 'NONE',  ( 8.111591955682463606, 4.202752102959690472E-16, 0.000000000000000000 ) ) ;
#39870 = ORIENTED_EDGE ( 'NONE', *, *, #1166, .T. ) ;
#39871 = ORIENTED_EDGE ( 'NONE', *, *, #56991, .T. ) ;
#39872 = LINE ( 'NONE', #50022, #27082 ) ;
#39874 = EDGE_CURVE ( 'NONE', #140745, #108674, #131999, .T. ) ;
#39873 = VERTEX_POINT ( 'NONE', #87054 ) ;
#39875 = VERTEX_POINT ( 'NONE', #99326 ) ;
#39876 = AXIS2_PLACEMENT_3D ( 'NONE', #70188, #34664, #91212 ) ;
#39877 = VECTOR ( 'NONE', #113034, 1000.000000000000000 ) ;
#39878 = CARTESIAN_POINT ( 'NONE',  ( 110.3079301918981088, -6.109999999999998543, 1.637169565754158507 ) ) ;
#39879 = CARTESIAN_POINT ( 'NONE',  ( -3.489213562373097322, -27.52281430457057709, 5.000000000000000000 ) ) ;
#39880 = CARTESIAN_POINT ( 'NONE',  ( -30.70612307739174796, 22.22500000000000142, 4.000000000000000000 ) ) ;
#39881 = ORIENTED_EDGE ( 'NONE', *, *, #129354, .F. ) ;
#39882 = LINE ( 'NONE', #139902, #43733 ) ;
#39883 = FACE_OUTER_BOUND ( 'NONE', #138925, .T. ) ;
#39884 = VECTOR ( 'NONE', #72606, 1000.000000000000000 ) ;
#39885 = DIRECTION ( 'NONE',  ( -0.7071067811865486830, -0.7071067811865464625, -0.000000000000000000 ) ) ;
#39886 =( BOUNDED_CURVE ( )  B_SPLINE_CURVE ( 3, ( #63665, #141180, #140471, #62952 ),
 .UNSPECIFIED., .F., .T. ) 
 B_SPLINE_CURVE_WITH_KNOTS ( ( 4, 4 ),
 ( 2.001653308786179419, 3.503810798801449522 ),
 .UNSPECIFIED. ) 
 CURVE ( )  GEOMETRIC_REPRESENTATION_ITEM ( )  RATIONAL_B_SPLINE_CURVE ( ( 1.000000000000000000, 0.8206354192515267210, 0.8206354192515267210, 1.000000000000000000 ) ) 
 REPRESENTATION_ITEM ( '' )  );
#39887 = CARTESIAN_POINT ( 'NONE',  ( 25.49999999999982236, 3.073033219394647464, -6.593910359670911880 ) ) ;
#39888 = ORIENTED_EDGE ( 'NONE', *, *, #95403, .F. ) ;
#39889 = EDGE_CURVE ( 'NONE', #82163, #114199, #63889, .T. ) ;
#39890 = DIRECTION ( 'NONE',  ( 0.6830127018922180770, -0.6830127018922204085, -0.2588190451025213501 ) ) ;
#39891 = ORIENTED_EDGE ( 'NONE', *, *, #20453, .F. ) ;
#39892 = CARTESIAN_POINT ( 'NONE',  ( 25.40000000000000568, 1.328209827113943309, -7.833578357555276206 ) ) ;
#39893 = EDGE_CURVE ( 'NONE', #12168, #132912, #86355, .T. ) ;
#39894 = DIRECTION ( 'NONE',  ( -0.000000000000000000, 0.3543493200069153248, 0.9351131265310292928 ) ) ;
#39895 = ORIENTED_EDGE ( 'NONE', *, *, #20664, .F. ) ;
#39896 = DIRECTION ( 'NONE',  ( -0.7071067811865486830, -0.7071067811865464625, 0.000000000000000000 ) ) ;
#39897 = ORIENTED_EDGE ( 'NONE', *, *, #138664, .F. ) ;
#39898 = EDGE_LOOP ( 'NONE', ( #2600, #25369, #130385, #52918 ) ) ;
#39899 = ORIENTED_EDGE ( 'NONE', *, *, #14896, .F. ) ;
#39900 = ADVANCED_FACE ( 'NONE', ( #130574 ), #98627, .F. ) ;
#39901 = EDGE_CURVE ( 'NONE', #88238, #69036, #61057, .T. ) ;
#39902 = CARTESIAN_POINT ( 'NONE',  ( 24.09999999999999787, 9.521314400968980422E-16, 0.000000000000000000 ) ) ;
#39903 = LINE ( 'NONE', #125464, #85356 ) ;
#39904 = DIRECTION ( 'NONE',  ( 0.7071067811865487940, 0.7071067811865463515, 0.000000000000000000 ) ) ;
#39905 =( NAMED_UNIT ( * ) PLANE_ANGLE_UNIT ( ) SI_UNIT ( $, .RADIAN. ) );
#39906 = FACE_OUTER_BOUND ( 'NONE', #22540, .T. ) ;
#39907 = EDGE_CURVE ( 'NONE', #93479, #74127, #76039, .T. ) ;
#39908 = DIRECTION ( 'NONE',  ( 0.7071067811865487940, -0.7071067811865463515, 0.000000000000000000 ) ) ;
#39909 = VECTOR ( 'NONE', #8507, 1000.000000000000000 ) ;
#39910 = AXIS2_PLACEMENT_3D ( 'NONE', #56894, #44601, #109807 ) ;
#39911 = VECTOR ( 'NONE', #99172, 1000.000000000000000 ) ;
#39912 = DIRECTION ( 'NONE',  ( -0.7071067811865487940, 0.7071067811865463515, -0.000000000000000000 ) ) ;
#39913 = VECTOR ( 'NONE', #47451, 1000.000000000000000 ) ;
#39914 = EDGE_CURVE ( 'NONE', #10965, #95953, #13034, .T. ) ;
#39915 = AXIS2_PLACEMENT_3D ( 'NONE', #44161, #98521, #22357 ) ;
#39916 = CARTESIAN_POINT ( 'NONE',  ( 62.99451991528749772, 28.92564299267982264, 4.000000000000000000 ) ) ;
#39917 = LINE ( 'NONE', #51487, #85322 ) ;
#39918 = FACE_OUTER_BOUND ( 'NONE', #40499, .T. ) ;
#39919 = ORIENTED_EDGE ( 'NONE', *, *, #59219, .F. ) ;
#39920 = VERTEX_POINT ( 'NONE', #91361 ) ;
#39921 = VECTOR ( 'NONE', #52985, 1000.000000000000227 ) ;
#39922 = ORIENTED_EDGE ( 'NONE', *, *, #136413, .F. ) ;
#39923 = VECTOR ( 'NONE', #93803, 999.9999999999998863 ) ;
#39924 = ORIENTED_EDGE ( 'NONE', *, *, #123082, .F. ) ;
#39925 = PRESENTATION_LAYER_ASSIGNMENT (  '', '', ( #134819 ) ) ;
#39926 = CARTESIAN_POINT ( 'NONE',  ( -1.152691986415045111, 0.6678635374937111902, 3.830955253485991197 ) ) ;
#39927 = ADVANCED_FACE ( 'NONE', ( #70346 ), #5952, .T. ) ;
#39928 = ORIENTED_EDGE ( 'NONE', *, *, #9473, .T. ) ;
#39929 = EDGE_LOOP ( 'NONE', ( #94900, #135109, #20254, #11540 ) ) ;
#39930 = CARTESIAN_POINT ( 'NONE',  ( 25.34840764549667469, 2.499999999999998224, 3.061616997868380183E-16 ) ) ;
#39931 = CARTESIAN_POINT ( 'NONE',  ( 27.29974487139158512, -27.71228299555225405, 4.000000000000000000 ) ) ;
#39932 = PLANE ( 'NONE',  #111171 ) ;
#39933 = ORIENTED_EDGE ( 'NONE', *, *, #124525, .T. ) ;
#39934 = PLANE ( 'NONE',  #120428 ) ;
#39935 = EDGE_CURVE ( 'NONE', #115217, #131076, #100783, .T. ) ;
#39936 = EDGE_CURVE ( 'NONE', #25329, #903, #134874, .T. ) ;
#39937 = ORIENTED_EDGE ( 'NONE', *, *, #18143, .T. ) ;
#39938 = CARTESIAN_POINT ( 'NONE',  ( -29.99999999999979039, 8.587461875839160541, 4.000000000000000000 ) ) ;
#39939 = FACE_OUTER_BOUND ( 'NONE', #122108, .T. ) ;
#39940 = CARTESIAN_POINT ( 'NONE',  ( 8.671236474768553748, 0.000000000000000000, 7.934999999999990727 ) ) ;
#39941 = ORIENTED_EDGE ( 'NONE', *, *, #135904, .F. ) ;
#39942 = CARTESIAN_POINT ( 'NONE',  ( 105.0579301918981230, 6.110000000000001208, -1.637169565754156286 ) ) ;
#39943 = CARTESIAN_POINT ( 'NONE',  ( 25.39999999999999858, -14.29000000000013593, -12.70000000000045404 ) ) ;
#39944 = LINE ( 'NONE', #128362, #41967 ) ;
#39945 = VERTEX_POINT ( 'NONE', #34827 ) ;
#39946 = EDGE_CURVE ( 'NONE', #130142, #27289, #124673, .T. ) ;
#39947 = ORIENTED_EDGE ( 'NONE', *, *, #1846, .T. ) ;
#39948 = DIRECTION ( 'NONE',  ( 0.7071067811865487940, -0.7071067811865463515, 0.000000000000000000 ) ) ;
#39949 = ORIENTED_EDGE ( 'NONE', *, *, #123821, .T. ) ;
#39950 = DIRECTION ( 'NONE',  ( 0.3543493200069164351, 2.781805975412904658E-17, -0.9351131265310288487 ) ) ;
#39951 = CARTESIAN_POINT ( 'NONE',  ( 45.48921356237309510, -27.52281430457087197, 5.000000000000000000 ) ) ;
#39952 = DIRECTION ( 'NONE',  ( -0.7071067811865486830, 0.7071067811865464625, 0.000000000000000000 ) ) ;
#39953 = CARTESIAN_POINT ( 'NONE',  ( 183.8160784826766587, -51.89584459748878942, -39.24672819827820547 ) ) ;
#39954 = VERTEX_POINT ( 'NONE', #89893 ) ;
#39955 = VECTOR ( 'NONE', #69688, 1000.000000000000000 ) ;
#39956 = EDGE_CURVE ( 'NONE', #105156, #138063, #23188, .T. ) ;
#39957 = EDGE_CURVE ( 'NONE', #65885, #29858, #3666, .T. ) ;
#39958 = CARTESIAN_POINT ( 'NONE',  ( -20.81601139373100295, 28.73617430169773002, 5.000000000000000000 ) ) ;
#39959 = AXIS2_PLACEMENT_3D ( 'NONE', #95515, #139778, #50601 ) ;
#39960 = CARTESIAN_POINT ( 'NONE',  ( 45.18398860626900415, 28.73617430169818832, 5.000000000000000000 ) ) ;
#39961 = DIRECTION ( 'NONE',  ( 0.3543493200069163240, -0.000000000000000000, -0.9351131265310288487 ) ) ;
#39962 = ORIENTED_EDGE ( 'NONE', *, *, #140418, .F. ) ;
#39963 = DIRECTION ( 'NONE',  ( -0.7071067811865487940, 0.7071067811865463515, -0.000000000000000000 ) ) ;
#39964 = AXIS2_PLACEMENT_3D ( 'NONE', #25354, #113800, #135571 ) ;
#39966 = EDGE_CURVE ( 'NONE', #41713, #114574, #14486, .T. ) ;
#39965 = DIRECTION ( 'NONE',  ( -0.7071067811865487940, 0.7071067811865463515, 0.000000000000000000 ) ) ;
#39967 = ORIENTED_EDGE ( 'NONE', *, *, #107470, .F. ) ;
#39969 = ORIENTED_EDGE ( 'NONE', *, *, #4762, .T. ) ;
#39968 = LINE ( 'NONE', #29055, #71790 ) ;
#39970 = ADVANCED_FACE ( 'NONE', ( #23947 ), #68205, .F. ) ;
#39971 = EDGE_LOOP ( 'NONE', ( #42779, #102472, #102848, #12287, #121317, #79871 ) ) ;
#39972 = CARTESIAN_POINT ( 'NONE',  ( -5.731388644227705775, 12.99752701236087660, -24.93595787201127578 ) ) ;
#39973 = EDGE_LOOP ( 'NONE', ( #87124, #89081, #58825, #13653 ) ) ;
#39974 = DIRECTION ( 'NONE',  ( 0.000000000000000000, -1.000000000000000000, 0.000000000000000000 ) ) ;
#39975 = CARTESIAN_POINT ( 'NONE',  ( -44.99451991528749772, 28.92564299267969474, 4.000000000000000000 ) ) ;
#39976 = LINE ( 'NONE', #84195, #22904 ) ;
#39977 = EDGE_CURVE ( 'NONE', #36972, #140889, #102232, .T. ) ;
#39978 = DIRECTION ( 'NONE',  ( -0.6830127018922180770, -0.6830127018922204085, -0.2588190451025213501 ) ) ;
#39979 = CARTESIAN_POINT ( 'NONE',  ( 12.19999999999999574, 12.19802518668052649, 4.711086268963014412 ) ) ;
#39980 = DIRECTION ( 'NONE',  ( -0.6830127018922180770, -0.6830127018922204085, -0.2588190451025213501 ) ) ;
#39981 = VECTOR ( 'NONE', #8238, 1000.000000000000000 ) ;
#39982 = DIRECTION ( 'NONE',  ( -0.7071067811865486830, -0.7071067811865464625, 0.000000000000000000 ) ) ;
#39983 = CARTESIAN_POINT ( 'NONE',  ( -13.82816939922343735, -5.240707523384227073, 4.000000000000000000 ) ) ;
#39984 = CARTESIAN_POINT ( 'NONE',  ( -23.18753812416036908, -22.22500000000000142, 4.000000000000000000 ) ) ;
#39985 = AXIS2_PLACEMENT_3D ( 'NONE', #46971, #140347, #118587 ) ;
#39986 = CARTESIAN_POINT ( 'NONE',  ( 21.05633424050521540, 8.797022467481218300, 4.404357971607193889 ) ) ;
#39987 = EDGE_CURVE ( 'NONE', #28420, #41423, #92032, .T. ) ;
#39988 = CARTESIAN_POINT ( 'NONE',  ( -19.49999999999986500, -16.53360074219757081, 5.000000000000000000 ) ) ;
#39989 = LINE ( 'NONE', #5861, #131114 ) ;
#39990 = ORIENTED_EDGE ( 'NONE', *, *, #77589, .F. ) ;
#39991 = ORIENTED_EDGE ( 'NONE', *, *, #19378, .F. ) ;
#39992 = EDGE_LOOP ( 'NONE', ( #23707, #105995, #97748, #106026, #30442 ) ) ;
#39993 = CARTESIAN_POINT ( 'NONE',  ( 107.8958333333333144, -2.130196079827427091, 7.949999999999999289 ) ) ;
#39994 = ORIENTED_EDGE ( 'NONE', *, *, #126790, .F. ) ;
#39995 = VERTEX_POINT ( 'NONE', #1436 ) ;
#39996 = VERTEX_POINT ( 'NONE', #112380 ) ;
#39997 = DIRECTION ( 'NONE',  ( 1.000000000000000000, 0.000000000000000000, 0.000000000000000000 ) ) ;
#39998 = LINE ( 'NONE', #27643, #25410 ) ;
#39999 = VECTOR ( 'NONE', #131673, 1000.000000000000227 ) ;
#40000 = EDGE_LOOP ( 'NONE', ( #52181, #78757, #62103, #2431 ) ) ;
#40001 = CARTESIAN_POINT ( 'NONE',  ( 21.29974487139158512, -27.71228299555221142, 4.000000000000000000 ) ) ;
#40002 = DIRECTION ( 'NONE',  ( 0.3543493200069162685, -0.000000000000000000, -0.9351131265310288487 ) ) ;
#40003 = LINE ( 'NONE', #29092, #11623 ) ;
#40004 = CARTESIAN_POINT ( 'NONE',  ( 33.48921356237309510, -27.52281430457078670, 5.000000000000000000 ) ) ;
#40005 = CARTESIAN_POINT ( 'NONE',  ( 107.7712635252314186, 4.472830434245839371, 4.472830434245842035 ) ) ;
#40006 = ORIENTED_EDGE ( 'NONE', *, *, #79132, .T. ) ;
#40007 = CARTESIAN_POINT ( 'NONE',  ( -30.79333936457826226, 21.75929247661549581, 4.998822639870701856 ) ) ;
#40008 =( LENGTH_UNIT ( ) NAMED_UNIT ( * ) SI_UNIT ( .MILLI., .METRE. ) );
#40010 = VECTOR ( 'NONE', #13913, 1000.000000000000000 ) ;
#40009 = CARTESIAN_POINT ( 'NONE',  ( -25.49999999999982236, 8.900465351122130997, -2.516491619111453915 ) ) ;
#40011 = CARTESIAN_POINT ( 'NONE',  ( 30.18398860626900060, 28.73617430169808173, 5.000000000000000000 ) ) ;
#40012 = CARTESIAN_POINT ( 'NONE',  ( -51.18398860626899705, 28.73617430169823095, 5.000000000000000000 ) ) ;
#40013 = DIRECTION ( 'NONE',  ( 0.7071067811865487940, 0.7071067811865463515, 0.000000000000000000 ) ) ;
#40014 = DIRECTION ( 'NONE',  ( -0.6830127018922181881, 0.6830127018922202975, -0.2588190451025214056 ) ) ;
#40015 = CARTESIAN_POINT ( 'NONE',  ( 35.95419371712956291, 6.884901960086283523, 3.975000000000002753 ) ) ;
#40016 = CARTESIAN_POINT ( 'NONE',  ( -19.49999999999985789, 19.08746187583904330, 4.000000000000000000 ) ) ;
#40017 = ADVANCED_FACE ( 'NONE', ( #57311 ), #36941, .F. ) ;
#40018 = DIRECTION ( 'NONE',  ( 0.7071067811865487940, 0.7071067811865463515, -0.000000000000000000 ) ) ;
#40019 = VERTEX_POINT ( 'NONE', #2883 ) ;
#40020 = ORIENTED_EDGE ( 'NONE', *, *, #141728, .F. ) ;
#40021 = CARTESIAN_POINT ( 'NONE',  ( 126.2920968585647614, -5.291415217122921177, 3.054999999999999272 ) ) ;
#40022 = ORIENTED_EDGE ( 'NONE', *, *, #66125, .T. ) ;
#40023 = CARTESIAN_POINT ( 'NONE',  ( -23.54739889332687497, 7.099584588756134629, 5.000000000000000000 ) ) ;
#40024 = DIRECTION ( 'NONE',  ( -0.7071067811865487940, 0.7071067811865463515, -0.000000000000000000 ) ) ;
#40025 = VECTOR ( 'NONE', #4544, 1000.000000000000114 ) ;
#40026 = AXIS2_PLACEMENT_3D ( 'NONE', #22320, #123839, #99924 ) ;
#40027 = DIRECTION ( 'NONE',  ( 0.7071067811865486830, -0.7071067811865464625, -0.000000000000000000 ) ) ;
#40028 = DIRECTION ( 'NONE',  ( -0.6830127018922181881, 0.6830127018922202975, -0.2588190451025214056 ) ) ;
#40029 = VECTOR ( 'NONE', #72042, 999.9999999999998863 ) ;
#40030 = DIRECTION ( 'NONE',  ( 0.7071067811865487940, -0.7071067811865463515, 0.000000000000000000 ) ) ;
#40032 = AXIS2_PLACEMENT_3D ( 'NONE', #18430, #140261, #40946 ) ;
#40031 = LINE ( 'NONE', #53746, #11717 ) ;
#40033 = CARTESIAN_POINT ( 'NONE',  ( 124.3079301918981230, -6.109999999999998543, 1.637169565754158063 ) ) ;
#40034 = ORIENTED_EDGE ( 'NONE', *, *, #100272, .F. ) ;
#40035 = DIRECTION ( 'NONE',  ( -0.7071067811865486830, -0.7071067811865464625, 0.000000000000000000 ) ) ;
#40036 = ORIENTED_EDGE ( 'NONE', *, *, #71154, .T. ) ;
#40037 = STYLED_ITEM ( 'NONE', ( #51677 ), #131194 ) ;
#40038 = VECTOR ( 'NONE', #11398, 1000.000000000000000 ) ;
#40039 = LINE ( 'NONE', #28422, #114609 ) ;
#40040 = FILL_AREA_STYLE ('',( #95080 ) ) ;
#40041 = FILL_AREA_STYLE ('',( #74062 ) ) ;
#40042 = DIRECTION ( 'NONE',  ( -0.3543493200069162685, -0.000000000000000000, -0.9351131265310288487 ) ) ;
#40043 = ORIENTED_EDGE ( 'NONE', *, *, #29111, .F. ) ;
#40044 = CARTESIAN_POINT ( 'NONE',  ( 45.06293019189811844, 1.637169565754157174, 6.110000000000002984 ) ) ;
#40045 = ORIENTED_EDGE ( 'NONE', *, *, #115392, .F. ) ;
#40046 = DIRECTION ( 'NONE',  ( 0.7071067811865486830, -0.7071067811865464625, -0.000000000000000000 ) ) ;
#40047 = CARTESIAN_POINT ( 'NONE',  ( 38.99451991528749062, 28.92564299267965211, 4.000000000000000000 ) ) ;
#40048 = DIRECTION ( 'NONE',  ( 0.7071067811865486830, -0.7071067811865464625, -0.000000000000000000 ) ) ;
#40049 = LINE ( 'NONE', #74814, #30160 ) ;
#40050 = AXIS2_PLACEMENT_3D ( 'NONE', #1037, #35875, #135184 ) ;
#40051 = CARTESIAN_POINT ( 'NONE',  ( 49.05793019189810877, 6.110000000000000320, -1.637169565754156064 ) ) ;
#40052 = EDGE_LOOP ( 'NONE', ( #134540, #105259, #97671, #72977, #73560, #2168, #64447 ) ) ;
#40053 = LINE ( 'NONE', #78187, #25705 ) ;
#40054 = CARTESIAN_POINT ( 'NONE',  ( 29.29289321881325137, 8.259292476615643253, 5.000000000000000000 ) ) ;
#40055 = ORIENTED_EDGE ( 'NONE', *, *, #44696, .T. ) ;
#40056 = EDGE_LOOP ( 'NONE', ( #41120, #72898, #110243, #13329, #29155 ) ) ;
#40057 = EDGE_LOOP ( 'NONE', ( #63715, #123263, #50351, #105434 ) ) ;
#40058 = AXIS2_PLACEMENT_3D ( 'NONE', #60054, #134777, #137611 ) ;
#40059 = PRODUCT_DEFINITION_SHAPE ( 'NONE', 'NONE',  #143560 ) ;
#40060 = DIRECTION ( 'NONE',  ( 0.000000000000000000, 1.000000000000000000, 0.000000000000000000 ) ) ;
#40061 = ORIENTED_EDGE ( 'NONE', *, *, #77316, .T. ) ;
#40062 = VECTOR ( 'NONE', #62754, 1000.000000000000000 ) ;
#40063 = CARTESIAN_POINT ( 'NONE',  ( 45.28752705046289151, 0.000000000000000000, -7.949999999999998401 ) ) ;
#40064 = VECTOR ( 'NONE', #75152, 1000.000000000000227 ) ;
#40065 = CARTESIAN_POINT ( 'NONE',  ( 150.3000000000000114, 0.000000000000000000, 6.349999999999997868 ) ) ;
#40066 = EDGE_CURVE ( 'NONE', #64057, #38139, #111665, .T. ) ;
#40067 = FACE_BOUND ( 'NONE', #45462, .T. ) ;
#40068 = LINE ( 'NONE', #21843, #80486 ) ;
#40069 = EDGE_CURVE ( 'NONE', #117114, #25784, #101485, .T. ) ;
#40070 = EDGE_CURVE ( 'NONE', #88880, #10438, #113070, .T. ) ;
#40071 = PLANE ( 'NONE',  #12030 ) ;
#40072 = ORIENTED_EDGE ( 'NONE', *, *, #110419, .F. ) ;
#40073 = DIRECTION ( 'NONE',  ( 0.3543493200069162685, -0.000000000000000000, -0.9351131265310288487 ) ) ;
#40075 = EDGE_LOOP ( 'NONE', ( #53009, #122620, #31245, #59809 ) ) ;
#40074 = DIRECTION ( 'NONE',  ( -0.7071067811865486830, -0.7071067811865464625, 0.000000000000000000 ) ) ;
#40076 = VERTEX_POINT ( 'NONE', #47179 ) ;
#40077 = LINE ( 'NONE', #51646, #125909 ) ;
#40078 = ORIENTED_EDGE ( 'NONE', *, *, #122793, .F. ) ;
#40080 = EDGE_CURVE ( 'NONE', #97623, #62679, #29619, .T. ) ;
#40079 = VECTOR ( 'NONE', #66693, 1000.000000000000000 ) ;
#40081 = ADVANCED_FACE ( 'NONE', ( #116644 ), #39838, .F. ) ;
#40082 = CARTESIAN_POINT ( 'NONE',  ( 52.26626352523145158, 4.472830434245838482, -4.472830434245837594 ) ) ;
#40083 = ORIENTED_EDGE ( 'NONE', *, *, #82077, .F. ) ;
#40084 = CARTESIAN_POINT ( 'NONE',  ( -15.18398860626900237, 28.73617430169797871, 5.000000000000000000 ) ) ;
#40085 = LINE ( 'NONE', #84300, #77373 ) ;
#40086 = EDGE_CURVE ( 'NONE', #98841, #25963, #61587, .T. ) ;
#40087 = CIRCLE ( 'NONE', #128033, 5.968999999999998529 ) ;
#40088 = ORIENTED_EDGE ( 'NONE', *, *, #70375, .F. ) ;
#40089 = DIRECTION ( 'NONE',  ( -0.7071067811865486830, -0.7071067811865464625, -0.000000000000000000 ) ) ;
#40090 = AXIS2_PLACEMENT_3D ( 'NONE', #30727, #19108, #63373 ) ;
#40091 = ADVANCED_FACE ( 'NONE', ( #62287 ), #126114, .F. ) ;
#40092 = CARTESIAN_POINT ( 'NONE',  ( 34.68749999999999289, -5.819803920172573974, 5.819803920172573086 ) ) ;
#40093 = DIRECTION ( 'NONE',  ( -0.7071067811865486830, -0.7071067811865464625, 0.000000000000000000 ) ) ;
#40094 = CARTESIAN_POINT ( 'NONE',  ( -21.85181644961842196, 17.25929247661554555, 8.802941693769151144 ) ) ;
#40095 = DIRECTION ( 'NONE',  ( 0.7071067811865487940, 0.7071067811865463515, -0.000000000000000000 ) ) ;
#40096 = DIRECTION ( 'NONE',  ( 0.7071067811865487940, -0.7071067811865463515, 0.000000000000000000 ) ) ;
#40097 = ORIENTED_EDGE ( 'NONE', *, *, #46901, .F. ) ;
#40098 = EDGE_CURVE ( 'NONE', #13272, #11616, #8133, .T. ) ;
#40099 = AXIS2_PLACEMENT_3D ( 'NONE', #136823, #101340, #1976 ) ;
#40100 = ORIENTED_EDGE ( 'NONE', *, *, #57618, .F. ) ;
#40101 = CARTESIAN_POINT ( 'NONE',  ( 30.48921356237309510, -27.52281430457076894, 5.000000000000000000 ) ) ;
#40102 = DIRECTION ( 'NONE',  ( 0.7071067811865487940, -0.7071067811865463515, 0.000000000000000000 ) ) ;
#40103 = EDGE_LOOP ( 'NONE', ( #121982, #36053, #135204 ) ) ;
#40104 = EDGE_LOOP ( 'NONE', ( #26142, #19809, #69313, #135112 ) ) ;
#40105 = VERTEX_POINT ( 'NONE', #73863 ) ;
#40106 = PLANE ( 'NONE',  #65202 ) ;
#40107 = CARTESIAN_POINT ( 'NONE',  ( -8.816011393731004731, 28.73617430169781173, 5.000000000000000000 ) ) ;
#40108 = PRESENTATION_LAYER_ASSIGNMENT (  '', '', ( #100206 ) ) ;
#40109 = ORIENTED_EDGE ( 'NONE', *, *, #42439, .T. ) ;
#40110 = PLANE ( 'NONE',  #90252 ) ;
#40111 = EDGE_CURVE ( 'NONE', #74550, #45124, #115180, .T. ) ;
#40112 = CARTESIAN_POINT ( 'NONE',  ( 13.48373647476855375, -5.808823158059035485, -5.808823158059033709 ) ) ;
#40113 = CARTESIAN_POINT ( 'NONE',  ( -23.99451991528749062, 28.92564299267954908, 4.000000000000000000 ) ) ;
#40114 = ORIENTED_EDGE ( 'NONE', *, *, #55288, .T. ) ;
#40115 = LINE ( 'NONE', #6685, #3474 ) ;
#40116 = DIRECTION ( 'NONE',  ( -0.7071067811865487940, 0.7071067811865463515, 0.000000000000000000 ) ) ;
#40117 = EDGE_CURVE ( 'NONE', #105516, #39821, #38383, .T. ) ;
#40118 = CARTESIAN_POINT ( 'NONE',  ( -60.29974487139158867, -27.71228299555248142, 4.000000000000000000 ) ) ;
#40119 = VECTOR ( 'NONE', #34774, 1000.000000000000000 ) ;
#40121 = ORIENTED_EDGE ( 'NONE', *, *, #3601, .T. ) ;
#40120 = CARTESIAN_POINT ( 'NONE',  ( 15.49238828748955576, 4.584330080086930965E-16, 0.000000000000000000 ) ) ;
#40122 = DIRECTION ( 'NONE',  ( 1.000000000000000000, 1.224606353822377258E-16, 0.000000000000000000 ) ) ;
#40123 = EDGE_LOOP ( 'NONE', ( #129687, #137070, #6464, #33376 ) ) ;
#40124 = DIRECTION ( 'NONE',  ( -0.3543493200069162685, -0.000000000000000000, -0.9351131265310288487 ) ) ;
#40125 = LINE ( 'NONE', #29203, #65476 ) ;
#40126 = CARTESIAN_POINT ( 'NONE',  ( 45.48921356237309510, -27.52281430457087197, 5.000000000000000000 ) ) ;
#40128 = EDGE_LOOP ( 'NONE', ( #129967, #12179, #141069, #142947 ) ) ;
#40127 = VECTOR ( 'NONE', #63097, 1000.000000000000000 ) ;
#40129 = EDGE_CURVE ( 'NONE', #100921, #27961, #6540, .T. ) ;
#40130 = ADVANCED_FACE ( 'NONE', ( #4987 ), #118036, .F. ) ;
#40131 = FACE_OUTER_BOUND ( 'NONE', #118526, .T. ) ;
#40132 = LINE ( 'NONE', #69914, #118206 ) ;
#40133 = PLANE ( 'NONE',  #132421 ) ;
#40134 = VECTOR ( 'NONE', #40732, 1000.000000000000000 ) ;
#40135 = ORIENTED_EDGE ( 'NONE', *, *, #97128, .T. ) ;
#40136 = COLOUR_RGB ( '', 0.66274510, 0.83137255, 0.94901961) ;
#40137 = FACE_OUTER_BOUND ( 'NONE', #11439, .T. ) ;
#40138 = DIRECTION ( 'NONE',  ( -0.000000000000000000, 0.3543493200069153248, 0.9351131265310292928 ) ) ;
#40140 = ADVANCED_FACE ( 'NONE', ( #7128 ), #95602, .F. ) ;
#40139 = DIRECTION ( 'NONE',  ( -1.000000000000000000, -1.224606353822377258E-16, -0.000000000000000000 ) ) ;
#40141 = CARTESIAN_POINT ( 'NONE',  ( 2.816011393730999401, 28.73617430169785436, 5.000000000000000000 ) ) ;
#40142 = DIRECTION ( 'NONE',  ( -0.000000000000000000, 0.3543493200069153248, 0.9351131265310292928 ) ) ;
#40143 = VERTEX_POINT ( 'NONE', #27479 ) ;
#40144 = ORIENTED_EDGE ( 'NONE', *, *, #120067, .F. ) ;
#40145 = DIRECTION ( 'NONE',  ( 0.000000000000000000, 0.000000000000000000, -1.000000000000000000 ) ) ;
#40146 = DIRECTION ( 'NONE',  ( -0.000000000000000000, 0.3543493200069153248, 0.9351131265310292928 ) ) ;
#40147 = EDGE_CURVE ( 'NONE', #111848, #51277, #115901, .T. ) ;
#40149 = B_SPLINE_CURVE_WITH_KNOTS ( 'NONE', 3,
 ( #34232, #853, #45144, #24068, #11007, #57428, #68325, #13157, #88626, #55275, #44422, #2267, #89320, #122649, #101613, #99452, #47301, #24769, #78456, #113193, #91472, #23325, #25468, #138542, #26912, #71157, #39231, #116773, #124801, #82736, #39972, #69746, #49421, #113923, #5841, #14614, #16748, #60284, #115301, #27615, #92879, #61028, #127671, #4374, #47985, #136383 ),
 .UNSPECIFIED., .F., .F.,
 ( 4, 2, 2, 2, 2, 2, 2, 2, 2, 2, 2, 2, 2, 2, 2, 2, 2, 2, 2, 2, 2, 2, 4 ),
 ( 1.301042606982605321E-18, 0.003160655639991156486, 0.004740983459986731693, 0.006321311279982309503, 0.009481966919973470326, 0.01106229473996905160, 0.01264262255996463115, 0.01580327819995578503, 0.01738360601995135937, 0.01896393383994693718, 0.02212458947993808239, 0.02370491729993365326, 0.02528524511992922413, 0.02844590075992036934, 0.03002622857991594021, 0.03160655639991151455, 0.03476721203990266323, 0.03792786767989381191, 0.04108852331988496059, 0.04266885113988053840, 0.04424917895987611621, 0.04740983459986727183, 0.05057049023985842745 ),
 .UNSPECIFIED. ) ;
#40148 = CARTESIAN_POINT ( 'NONE',  ( 11.20790314143521904, -6.871911579029513106, -3.967499999999993587 ) ) ;
#40150 = LINE ( 'NONE', #104644, #27391 ) ;
#40151 = AXIS2_PLACEMENT_3D ( 'NONE', #90781, #59583, #14624 ) ;
#40152 = DIRECTION ( 'NONE',  ( -0.3543493200069162685, -0.000000000000000000, -0.9351131265310288487 ) ) ;
#40153 = DIRECTION ( 'NONE',  ( -0.000000000000000000, 0.000000000000000000, 1.000000000000000000 ) ) ;
#40154 = ORIENTED_EDGE ( 'NONE', *, *, #22805, .T. ) ;
#40155 = EDGE_CURVE ( 'NONE', #66046, #96996, #63016, .T. ) ;
#40156 = DIRECTION ( 'NONE',  ( -0.7071067811865487940, 0.7071067811865463515, -0.000000000000000000 ) ) ;
#40157 = CARTESIAN_POINT ( 'NONE',  ( -16.44665057663207719, 2.259292476615690770, 14.86850063742358330 ) ) ;
#40158 = CARTESIAN_POINT ( 'NONE',  ( 29.67183060077626422, 20.25929247661551358, 4.000000000000000000 ) ) ;
#40159 = LINE ( 'NONE', #7466, #124713 ) ;
#40160 = CARTESIAN_POINT ( 'NONE',  ( 43.37043019189810877, -3.055000000000001936, 5.291415217122918513 ) ) ;
#40161 = VECTOR ( 'NONE', #14206, 1000.000000000000000 ) ;
#40162 = DIRECTION ( 'NONE',  ( 0.3543493200069162685, -0.000000000000000000, -0.9351131265310288487 ) ) ;
#40163 = VERTEX_POINT ( 'NONE', #127525 ) ;
#40164 = DIRECTION ( 'NONE',  ( -0.000000000000000000, -0.3543493200069152693, 0.9351131265310292928 ) ) ;
#40165 = VECTOR ( 'NONE', #68472, 1000.000000000000000 ) ;
#40166 = ORIENTED_EDGE ( 'NONE', *, *, #123106, .T. ) ;
#40167 = VERTEX_POINT ( 'NONE', #137709 ) ;
#40168 = DIRECTION ( 'NONE',  ( 0.6830127018922180770, -0.6830127018922204085, -0.2588190451025213501 ) ) ;
#40169 = DIRECTION ( 'NONE',  ( 0.000000000000000000, 1.000000000000000000, 1.365923996832126925E-16 ) ) ;
#40171 = VECTOR ( 'NONE', #2445, 1000.000000000000000 ) ;
#40170 = DIRECTION ( 'NONE',  ( -0.6830127018922180770, -0.6830127018922204085, -0.2588190451025213501 ) ) ;
#40172 = CARTESIAN_POINT ( 'NONE',  ( -16.62823445044374893, -8.240707523384200428, 11.38925528200756432 ) ) ;
#40173 = EDGE_CURVE ( 'NONE', #81146, #8053, #107190, .T. ) ;
#40174 = CARTESIAN_POINT ( 'NONE',  ( -5.671830600776432973, 20.25929247661551003, 4.000000000000000000 ) ) ;
#40175 = CARTESIAN_POINT ( 'NONE',  ( 15.00548008471250228, 28.92564299267927552, 4.000000000000000000 ) ) ;
#40176 = ORIENTED_EDGE ( 'NONE', *, *, #139692, .F. ) ;
#40177 = LINE ( 'NONE', #95940, #69558 ) ;
#40178 = FACE_OUTER_BOUND ( 'NONE', #49801, .T. ) ;
#40179 = FACE_OUTER_BOUND ( 'NONE', #14521, .T. ) ;
#40180 = LINE ( 'NONE', #16209, #92488 ) ;
#40181 = CARTESIAN_POINT ( 'NONE',  ( -15.48921356237309510, -27.52281430457066236, 5.000000000000000000 ) ) ;
#40182 = CARTESIAN_POINT ( 'NONE',  ( -72.48921356237309510, -27.52281430457106026, 5.000000000000000000 ) ) ;
#40183 = VECTOR ( 'NONE', #125084, 1000.000000000000227 ) ;
#40184 = CARTESIAN_POINT ( 'NONE',  ( 66.87086038379622721, 6.884901960086289741, -3.974999999999993427 ) ) ;
#40185 = COLOUR_RGB ( '', 0.40784314, 0.44705882, 0.49803922) ;
#40186 = CARTESIAN_POINT ( 'NONE',  ( -0.3281693992235254487, -0.7407075233842788098, 4.000000000000000000 ) ) ;
#40187 = ORIENTED_EDGE ( 'NONE', *, *, #88567, .F. ) ;
#40188 = ORIENTED_EDGE ( 'NONE', *, *, #72703, .T. ) ;
#40189 = CARTESIAN_POINT ( 'NONE',  ( 52.18749999999999289, -5.819803920172573086, 5.819803920172572198 ) ) ;
#40190 = DIRECTION ( 'NONE',  ( -0.7071067811865486830, 0.7071067811865464625, 0.000000000000000000 ) ) ;
#40191 = CARTESIAN_POINT ( 'NONE',  ( 31.92500000000001492, 1.196650378695341299, -30.59010235425025215 ) ) ;
#40192 = AXIS2_PLACEMENT_3D ( 'NONE', #95595, #131095, #42682 ) ;
#40193 = ORIENTED_EDGE ( 'NONE', *, *, #94880, .F. ) ;
#40194 = EDGE_CURVE ( 'NONE', #101903, #105827, #72481, .T. ) ;
#40195 = DIRECTION ( 'NONE',  ( 0.7071067811865487940, -0.7071067811865463515, 0.000000000000000000 ) ) ;
#40196 = ADVANCED_FACE ( 'NONE', ( #84058 ), #128256, .F. ) ;
#40197 = CARTESIAN_POINT ( 'NONE',  ( 52.35459685856476852, -1.637169565754161615, 6.110000000000000320 ) ) ;
#40198 = EDGE_LOOP ( 'NONE', ( #26496, #39372, #16136 ) ) ;
#40199 = CARTESIAN_POINT ( 'NONE',  ( -32.99999999999976552, 10.93112307739207445, 4.000000000000000000 ) ) ;
#40200 = VERTEX_POINT ( 'NONE', #81927 ) ;
#40201 = EDGE_LOOP ( 'NONE', ( #98663, #83148, #72281, #65933 ) ) ;
#40202 = VECTOR ( 'NONE', #79931, 1000.000000000000000 ) ;
#40203 = CARTESIAN_POINT ( 'NONE',  ( -11.99999999999991296, -18.41253812416056945, 4.000000000000000000 ) ) ;
#40204 = PRESENTATION_STYLE_ASSIGNMENT (( #116296 ) ) ;
#40205 = FACE_OUTER_BOUND ( 'NONE', #10716, .T. ) ;
#40206 = PLANE ( 'NONE',  #11633 ) ;
#40207 = EDGE_CURVE ( 'NONE', #15118, #134245, #26782, .T. ) ;
#40208 = LINE ( 'NONE', #72854, #30295 ) ;
#40210 = ORIENTED_EDGE ( 'NONE', *, *, #41714, .T. ) ;
#40209 = CARTESIAN_POINT ( 'NONE',  ( 100.5583603837962272, -7.949999999999996625, -2.130196079827426203 ) ) ;
#40211 = DIRECTION ( 'NONE',  ( -0.5735764363510507113, 0.8191520442889885789, 1.003171929053520926E-16 ) ) ;
#40212 = CARTESIAN_POINT ( 'NONE',  ( 1.500000000000001332, 16.08746187583907172, 4.000000000000000000 ) ) ;
#40213 = AXIS2_PLACEMENT_3D ( 'NONE', #11983, #47536, #111294 ) ;
#40214 = CARTESIAN_POINT ( 'NONE',  ( -12.32816939922343913, 2.259292476615696099, 4.000000000000000000 ) ) ;
#40215 = CARTESIAN_POINT ( 'NONE',  ( -6.328169399223481761, -12.74070752338415424, 4.000000000000000000 ) ) ;
#40216 = ORIENTED_EDGE ( 'NONE', *, *, #56116, .T. ) ;
#40217 = ORIENTED_EDGE ( 'NONE', *, *, #86907, .F. ) ;
#40218 = VECTOR ( 'NONE', #94774, 1000.000000000000114 ) ;
#40219 = CARTESIAN_POINT ( 'NONE',  ( 77.20376352523145158, 6.109999999999998543, 1.122388791418548911E-15 ) ) ;
#40220 = DIRECTION ( 'NONE',  ( 0.7071067811865486830, -0.7071067811865464625, -0.000000000000000000 ) ) ;
#40221 = FACE_OUTER_BOUND ( 'NONE', #13039, .T. ) ;
#40222 = CARTESIAN_POINT ( 'NONE',  ( -34.75611968250420603, 1.705650698524048936, 4.955485411084896263 ) ) ;
#40223 = EDGE_LOOP ( 'NONE', ( #75058, #20506, #74758, #84885, #1184 ) ) ;
#40224 = ORIENTED_EDGE ( 'NONE', *, *, #94322, .F. ) ;
#40225 = CARTESIAN_POINT ( 'NONE',  ( 4.911592354503321545, 2.500000000000001332, 0.000000000000000000 ) ) ;
#40226 = DIRECTION ( 'NONE',  ( -0.3543493200069162685, -0.000000000000000000, -0.9351131265310288487 ) ) ;
#40227 = ORIENTED_EDGE ( 'NONE', *, *, #47212, .F. ) ;
#40228 = VECTOR ( 'NONE', #22379, 999.9999999999998863 ) ;
#40229 = EDGE_LOOP ( 'NONE', ( #91605, #130690, #60896, #52194, #13530, #36347 ) ) ;
#40230 = DIRECTION ( 'NONE',  ( -0.6830127018922180770, -0.6830127018922204085, -0.2588190451025213501 ) ) ;
#40231 = ORIENTED_EDGE ( 'NONE', *, *, #78503, .F. ) ;
#40232 = FACE_OUTER_BOUND ( 'NONE', #65219, .T. ) ;
#40233 = FACE_BOUND ( 'NONE', #114941, .T. ) ;
#40234 = CARTESIAN_POINT ( 'NONE',  ( 36.29974487139159578, -27.71228299555231445, 4.000000000000000000 ) ) ;
#40235 = ADVANCED_FACE ( 'NONE', ( #132564 ), #32510, .F. ) ;
#40236 = DIRECTION ( 'NONE',  ( -0.6830127018922180770, -0.6830127018922204085, -0.2588190451025213501 ) ) ;
#40237 = DIRECTION ( 'NONE',  ( -1.000000000000000000, -1.224606353822377258E-16, -0.000000000000000000 ) ) ;
#40239 = ORIENTED_EDGE ( 'NONE', *, *, #134408, .T. ) ;
#40238 = CARTESIAN_POINT ( 'NONE',  ( 23.11162361894744777, 9.759292476615614831, 17.35367589129207389 ) ) ;
#40240 = VECTOR ( 'NONE', #31314, 1000.000000000000000 ) ;
#40241 = ORIENTED_EDGE ( 'NONE', *, *, #27169, .F. ) ;
#40242 = ADVANCED_FACE ( 'NONE', ( #74594 ), #108581, .F. ) ;
#40243 = ADVANCED_FACE ( 'NONE', ( #140528 ), #9266, .F. ) ;
#40244 = CIRCLE ( 'NONE', #121224, 2.500000000000000888 ) ;
#40245 = VERTEX_POINT ( 'NONE', #10709 ) ;
#40246 = CARTESIAN_POINT ( 'NONE',  ( 84.05793019189810877, 6.110000000000000320, -1.637169565754156064 ) ) ;
#40247 = ORIENTED_EDGE ( 'NONE', *, *, #81922, .F. ) ;
#40248 = PLANE ( 'NONE',  #54547 ) ;
#40249 = EDGE_CURVE ( 'NONE', #4447, #59626, #77463, .T. ) ;
#40250 = PLANE ( 'NONE',  #69753 ) ;
#40251 = EDGE_CURVE ( 'NONE', #39324, #124216, #30352, .T. ) ;
#40252 = CARTESIAN_POINT ( 'NONE',  ( 60.18398860626900415, 28.73617430169829490, 5.000000000000000000 ) ) ;
#40253 = EDGE_CURVE ( 'NONE', #84947, #67897, #109342, .T. ) ;
#40254 = VECTOR ( 'NONE', #43649, 999.9999999999998863 ) ;
#40255 = PLANE ( 'NONE',  #35626 ) ;
#40256 = ORIENTED_EDGE ( 'NONE', *, *, #123629, .T. ) ;
#40257 = DIRECTION ( 'NONE',  ( 0.000000000000000000, 0.000000000000000000, 1.000000000000000000 ) ) ;
#40258 = EDGE_CURVE ( 'NONE', #12164, #126832, #21626, .T. ) ;
#40259 = CARTESIAN_POINT ( 'NONE',  ( 12.19999999999999574, -40.43000000000000682, -39.50000000000000000 ) ) ;
#40260 = AXIS2_PLACEMENT_3D ( 'NONE', #7433, #51696, #102 ) ;
#40261 = DIRECTION ( 'NONE',  ( 0.7071067811865487940, 0.7071067811865463515, 0.000000000000000000 ) ) ;
#40262 =( NAMED_UNIT ( * ) PLANE_ANGLE_UNIT ( ) SI_UNIT ( $, .RADIAN. ) );
#40263 = LINE ( 'NONE', #6835, #115711 ) ;
#40264 = DIRECTION ( 'NONE',  ( 0.7071067811865487940, 0.7071067811865463515, -0.000000000000000000 ) ) ;
#40265 = ORIENTED_EDGE ( 'NONE', *, *, #25360, .F. ) ;
#40266 = CARTESIAN_POINT ( 'NONE',  ( 123.3083603837962130, 7.949999999999996625, 2.130196079827431088 ) ) ;
#40267 = LINE ( 'NONE', #29341, #48910 ) ;
#40268 = VECTOR ( 'NONE', #86481, 999.9999999999998863 ) ;
#40269 = EDGE_CURVE ( 'NONE', #52145, #3412, #120176, .T. ) ;
#40270 = EDGE_LOOP ( 'NONE', ( #139526, #121172, #25907 ) ) ;
#40271 = VERTEX_POINT ( 'NONE', #96284 ) ;
#40272 = EDGE_CURVE ( 'NONE', #79754, #25103, #94246, .T. ) ;
#40273 = ORIENTED_EDGE ( 'NONE', *, *, #109213, .F. ) ;
#40274 = CARTESIAN_POINT ( 'NONE',  ( 37.62543019189811133, 5.291415217122919401, 3.055000000000002824 ) ) ;
#40275 = ORIENTED_EDGE ( 'NONE', *, *, #62158, .F. ) ;
#40276 = EDGE_CURVE ( 'NONE', #87099, #11206, #65882, .T. ) ;
#40277 = AXIS2_PLACEMENT_3D ( 'NONE', #70243, #81817, #70927 ) ;
#40278 = CIRCLE ( 'NONE', #7835, 4.000000000000000000 ) ;
#40279 = CARTESIAN_POINT ( 'NONE',  ( 18.42080628287044064, 3.047499999999997655, 5.278424836066143655 ) ) ;
#40280 = CARTESIAN_POINT ( 'NONE',  ( -16.45742106731621490, 0.9613713492673534589, -33.49048331797056477 ) ) ;
#40281 = ORIENTED_EDGE ( 'NONE', *, *, #118790, .F. ) ;
#40282 = DIRECTION ( 'NONE',  ( -0.000000000000000000, 0.3543493200069153248, 0.9351131265310292928 ) ) ;
#40283 = VERTEX_POINT ( 'NONE', #10023 ) ;
#40284 = VECTOR ( 'NONE', #115680, 1000.000000000000000 ) ;
#40285 = CARTESIAN_POINT ( 'NONE',  ( -0.3281693992235289459, -15.74070752338412760, 4.000000000000000000 ) ) ;
#40287 = ORIENTED_EDGE ( 'NONE', *, *, #120905, .F. ) ;
#40286 = DIRECTION ( 'NONE',  ( -0.7071067811865487940, 0.7071067811865463515, 0.000000000000000000 ) ) ;
#40288 = ORIENTED_EDGE ( 'NONE', *, *, #130390, .F. ) ;
#40289 = SHAPE_REPRESENTATION ( '1.0 Base', ( #127880 ), #141741 ) ;
#40290 = CARTESIAN_POINT ( 'NONE',  ( -1.499999999999994449, -12.08601207473289740, -10.46905243149094389 ) ) ;
#40291 = VERTEX_POINT ( 'NONE', #141243 ) ;
#40292 = LINE ( 'NONE', #126538, #1774 ) ;
#40293 = ORIENTED_EDGE ( 'NONE', *, *, #19415, .F. ) ;
#40294 = ORIENTED_EDGE ( 'NONE', *, *, #92590, .F. ) ;
#40295 = ORIENTED_EDGE ( 'NONE', *, *, #61919, .T. ) ;
#40296 = VERTEX_POINT ( 'NONE', #131101 ) ;
#40297 = EDGE_CURVE ( 'NONE', #18088, #40635, #143394, .T. ) ;
#40298 = LINE ( 'NONE', #117783, #132814 ) ;
#40299 = VECTOR ( 'NONE', #11158, 999.9999999999998863 ) ;
#40300 = CARTESIAN_POINT ( 'NONE',  ( 5.816011393731002066, 28.73617430169783304, 5.000000000000000000 ) ) ;
#40301 = LINE ( 'NONE', #137452, #97982 ) ;
#40302 = LINE ( 'NONE', #84509, #39141 ) ;
#40303 = VERTEX_POINT ( 'NONE', #41957 ) ;
#40304 = CARTESIAN_POINT ( 'NONE',  ( 26.29289321881328334, -18.74070752338408852, 5.000000000000000000 ) ) ;
#40305 = ORIENTED_EDGE ( 'NONE', *, *, #13266, .F. ) ;
#40306 = FACE_OUTER_BOUND ( 'NONE', #31900, .T. ) ;
#40307 = ADVANCED_FACE ( 'NONE', ( #7865 ), #131818, .T. ) ;
#40308 = CARTESIAN_POINT ( 'NONE',  ( 54.18398860626899705, 28.73617430169825226, 5.000000000000000000 ) ) ;
#40309 = LINE ( 'NONE', #45140, #27681 ) ;
#40311 = ORIENTED_EDGE ( 'NONE', *, *, #15119, .T. ) ;
#40310 = AXIS2_PLACEMENT_3D ( 'NONE', #41492, #89127, #52369 ) ;
#40312 = LINE ( 'NONE', #77230, #22892 ) ;
#40313 = DIRECTION ( 'NONE',  ( -0.3543493200069162685, -0.000000000000000000, -0.9351131265310288487 ) ) ;
#40314 = ORIENTED_EDGE ( 'NONE', *, *, #72074, .F. ) ;
#40315 = ORIENTED_EDGE ( 'NONE', *, *, #142272, .F. ) ;
#40316 = ADVANCED_FACE ( 'NONE', ( #119472 ), #20165, .F. ) ;
#40317 = ORIENTED_EDGE ( 'NONE', *, *, #56130, .T. ) ;
#40318 = DIRECTION ( 'NONE',  ( -0.000000000000000000, 0.000000000000000000, 1.000000000000000000 ) ) ;
#40319 = CARTESIAN_POINT ( 'NONE',  ( -29.24139925780183091, 21.72500000000000853, 5.000000000000000000 ) ) ;
#40320 = PLANE ( 'NONE',  #141862 ) ;
#40321 = CARTESIAN_POINT ( 'NONE',  ( 12.71757738642558522, -21.73023691814493574, 5.000000000000000888 ) ) ;
#40322 = DIRECTION ( 'NONE',  ( 0.7071067811865487940, 0.7071067811865463515, -0.000000000000000000 ) ) ;
#40323 = CARTESIAN_POINT ( 'NONE',  ( 74.28709685856478018, 3.054999999999997939, 5.291415217122920289 ) ) ;
#40324 = VECTOR ( 'NONE', #78744, 999.9999999999998863 ) ;
#40325 = PLANE ( 'NONE',  #122826 ) ;
#40326 = CARTESIAN_POINT ( 'NONE',  ( 8.999999999999937828, 15.45873954670186201, -0.03131636524296085855 ) ) ;
#40327 = CARTESIAN_POINT ( 'NONE',  ( -0.1839886062690032631, 28.73617430169787568, 5.000000000000000000 ) ) ;
#40328 = EDGE_CURVE ( 'NONE', #136372, #110693, #59513, .T. ) ;
#40329 = CARTESIAN_POINT ( 'NONE',  ( 32.99451991528749062, 28.92564299267960948, 4.000000000000000000 ) ) ;
#40330 = DIRECTION ( 'NONE',  ( -0.7071067811865487940, 0.7071067811865463515, -0.000000000000000000 ) ) ;
#40331 = ORIENTED_EDGE ( 'NONE', *, *, #60372, .T. ) ;
#40332 = DIRECTION ( 'NONE',  ( -1.369518533665900312E-16, 1.000000000000000000, -0.000000000000000000 ) ) ;
#40333 = ORIENTED_EDGE ( 'NONE', *, *, #56706, .T. ) ;
#40334 = CYLINDRICAL_SURFACE ( 'NONE', #92378, 0.5000000000000004441 ) ;
#40336 = ORIENTED_EDGE ( 'NONE', *, *, #121689, .F. ) ;
#40335 = FACE_OUTER_BOUND ( 'NONE', #6702, .T. ) ;
#40337 = EDGE_CURVE ( 'NONE', #27137, #74390, #31787, .T. ) ;
#40338 = DIRECTION ( 'NONE',  ( 0.000000000000000000, -1.000000000000000000, 0.000000000000000000 ) ) ;
#40339 = CARTESIAN_POINT ( 'NONE',  ( -4.033400323430202050, 6.759292476615643253, 12.28218704918521453 ) ) ;
#40340 = ORIENTED_EDGE ( 'NONE', *, *, #19739, .F. ) ;
#40341 = ORIENTED_EDGE ( 'NONE', *, *, #7527, .T. ) ;
#40342 = CARTESIAN_POINT ( 'NONE',  ( -3.183988606268992161, 28.73617430169789699, 5.000000000000000000 ) ) ;
#40343 = DIRECTION ( 'NONE',  ( -0.6830127018922180770, -0.6830127018922204085, -0.2588190451025213501 ) ) ;
#40344 = AXIS2_PLACEMENT_3D ( 'NONE', #77867, #35096, #11861 ) ;
#40345 = CARTESIAN_POINT ( 'NONE',  ( 8.994519915287490619, 28.92564299267944250, 4.000000000000000000 ) ) ;
#40346 = CARTESIAN_POINT ( 'NONE',  ( 94.14169371712957002, -2.130196079827424871, -7.949999999999999289 ) ) ;
#40347 = PLANE ( 'NONE',  #138964 ) ;
#40348 = VECTOR ( 'NONE', #87217, 999.9999999999998863 ) ;
#40349 = DIRECTION ( 'NONE',  ( -0.6830127018922181881, 0.6830127018922202975, -0.2588190451025214056 ) ) ;
#40350 = ORIENTED_EDGE ( 'NONE', *, *, #80178, .T. ) ;
#40352 = EDGE_CURVE ( 'NONE', #116152, #112560, #120925, .T. ) ;
#40351 = CARTESIAN_POINT ( 'NONE',  ( 7.499999999999961808, 19.08746187583905396, 4.000000000000000000 ) ) ;
#40353 = FACE_OUTER_BOUND ( 'NONE', #5670, .T. ) ;
#40354 = CARTESIAN_POINT ( 'NONE',  ( 35.00000000000000000, 0.000000000000000000, 6.094999999999989981 ) ) ;
#40355 = LINE ( 'NONE', #84564, #35200 ) ;
#40356 = VERTEX_POINT ( 'NONE', #36088 ) ;
#40357 = EDGE_CURVE ( 'NONE', #20616, #114574, #101320, .T. ) ;
#40358 = EDGE_CURVE ( 'NONE', #78905, #7428, #89044, .T. ) ;
#40359 = FACE_OUTER_BOUND ( 'NONE', #136343, .T. ) ;
#40360 = ORIENTED_EDGE ( 'NONE', *, *, #42969, .F. ) ;
#40361 = ADVANCED_FACE ( 'NONE', ( #2707 ), #123814, .F. ) ;
#40362 = VECTOR ( 'NONE', #47115, 1000.000000000000000 ) ;
#40363 = VECTOR ( 'NONE', #1617, 1000.000000000000114 ) ;
#40364 = CARTESIAN_POINT ( 'NONE',  ( 89.25043019189810423, 3.055000000000002824, -5.291415217122919401 ) ) ;
#40365 = CARTESIAN_POINT ( 'NONE',  ( 32.99451991528749062, 28.92564299267960948, 4.000000000000000000 ) ) ;
#40366 = CARTESIAN_POINT ( 'NONE',  ( -32.20710678118631165, -11.24070752338416668, 5.000000000000000000 ) ) ;
#40367 = PLANE ( 'NONE',  #121967 ) ;
#40368 = ORIENTED_EDGE ( 'NONE', *, *, #107641, .T. ) ;
#40369 = PLANE ( 'NONE',  #69802 ) ;
#40370 = DIRECTION ( 'NONE',  ( 0.7071067811865487940, -0.7071067811865463515, 0.000000000000000000 ) ) ;
#40371 = VECTOR ( 'NONE', #137088, 999.9999999999998863 ) ;
#40372 = LINE ( 'NONE', #4797, #115631 ) ;
#40373 = EDGE_CURVE ( 'NONE', #133213, #96656, #1955, .T. ) ;
#40375 = ORIENTED_EDGE ( 'NONE', *, *, #92265, .F. ) ;
#40374 = CARTESIAN_POINT ( 'NONE',  ( -7.641757024588559766, 15.75929247661555088, 19.34181609438701344 ) ) ;
#40376 = CARTESIAN_POINT ( 'NONE',  ( 12.54166666666666785, 3.047499999999993214, -5.278424836066146320 ) ) ;
#40377 = CARTESIAN_POINT ( 'NONE',  ( -66.48921356237309510, -27.52281430457101763, 5.000000000000000000 ) ) ;
#40378 = CARTESIAN_POINT ( 'NONE',  ( 1.624181887823187953, -3.508773871178531234, 5.449882146574780428 ) ) ;
#40379 = AXIS2_PLACEMENT_3D ( 'NONE', #62389, #117428, #20989 ) ;
#40380 = ORIENTED_EDGE ( 'NONE', *, *, #52177, .F. ) ;
#40381 = VERTEX_POINT ( 'NONE', #123091 ) ;
#40382 = CARTESIAN_POINT ( 'NONE',  ( 73.35459685856476142, -1.637169565754161615, 6.110000000000000320 ) ) ;
#40383 = VECTOR ( 'NONE', #108873, 1000.000000000000000 ) ;
#40384 = VERTEX_POINT ( 'NONE', #112215 ) ;
#40385 = DIRECTION ( 'NONE',  ( 0.7071067811865487940, 0.7071067811865463515, -0.000000000000000000 ) ) ;
#40386 = FACE_OUTER_BOUND ( 'NONE', #66846, .T. ) ;
#40387 = CARTESIAN_POINT ( 'NONE',  ( 3.183988606268992161, 28.73617430169789699, 5.000000000000000000 ) ) ;
#40388 = VERTEX_POINT ( 'NONE', #23010 ) ;
#40389 = DIRECTION ( 'NONE',  ( -0.7071067811865487940, 0.7071067811865463515, -0.000000000000000000 ) ) ;
#40390 = LINE ( 'NONE', #104157, #18877 ) ;
#40391 = AXIS2_PLACEMENT_3D ( 'NONE', #140951, #143107, #41645 ) ;
#40392 = ORIENTED_EDGE ( 'NONE', *, *, #40593, .F. ) ;
#40393 = CARTESIAN_POINT ( 'NONE',  ( 19.73159235450332005, 3.061616997868380183E-16, -2.500000000000001332 ) ) ;
#40394 = LINE ( 'NONE', #17191, #110367 ) ;
#40395 = LINE ( 'NONE', #84601, #84079 ) ;
#40396 = ORIENTED_EDGE ( 'NONE', *, *, #109906, .F. ) ;
#40398 = ADVANCED_FACE ( 'NONE', ( #33941 ), #12860, .F. ) ;
#40397 = ORIENTED_EDGE ( 'NONE', *, *, #116056, .T. ) ;
#40399 = LINE ( 'NONE', #138264, #126492 ) ;
#40400 = CARTESIAN_POINT ( 'NONE',  ( 25.40000000000000568, -5.651140751524227568, -5.186583730001445680 ) ) ;
#40401 = DIRECTION ( 'NONE',  ( 0.000000000000000000, 0.000000000000000000, 1.000000000000000000 ) ) ;
#40402 = CARTESIAN_POINT ( 'NONE',  ( 181.1499999999998067, -47.62213595499955687, -36.92499999999996163 ) ) ;
#40403 = CARTESIAN_POINT ( 'NONE',  ( 27.18398860626900060, 28.73617430169806042, 5.000000000000000000 ) ) ;
#40404 = VERTEX_POINT ( 'NONE', #69430 ) ;
#40405 = EDGE_CURVE ( 'NONE', #117002, #103562, #68035, .T. ) ;
#40406 = VERTEX_POINT ( 'NONE', #56446 ) ;
#40407 = VERTEX_POINT ( 'NONE', #1268 ) ;
#40408 = ADVANCED_FACE ( 'NONE', ( #11416 ), #68716, .T. ) ;
#40409 = ORIENTED_EDGE ( 'NONE', *, *, #108991, .T. ) ;
#40410 = EDGE_CURVE ( 'NONE', #33542, #67920, #90449, .T. ) ;
#40411 = CARTESIAN_POINT ( 'NONE',  ( 180.5530070941967438, -49.14999999999999147, 40.56450646617377487 ) ) ;
#40412 = EDGE_CURVE ( 'NONE', #106956, #75231, #112909, .T. ) ;
#40413 = VECTOR ( 'NONE', #65949, 1000.000000000000114 ) ;
#40414 = DIRECTION ( 'NONE',  ( 0.000000000000000000, 0.000000000000000000, -1.000000000000000000 ) ) ;
#40415 = DIRECTION ( 'NONE',  ( -1.000000000000000000, -0.000000000000000000, -0.000000000000000000 ) ) ;
#40416 = EDGE_LOOP ( 'NONE', ( #52883, #55444, #112631, #2233 ) ) ;
#40417 = CARTESIAN_POINT ( 'NONE',  ( 24.39999999999999858, -5.520864266206504263E-14, -33.92499999999998295 ) ) ;
#40418 = FACE_OUTER_BOUND ( 'NONE', #15559, .T. ) ;
#40419 = CARTESIAN_POINT ( 'NONE',  ( 14.08373646989360317, 0.000000000000000000, 2.500000000000000444 ) ) ;
#40420 = DIRECTION ( 'NONE',  ( 1.000000000000000000, 0.000000000000000000, 0.000000000000000000 ) ) ;
#40421 = CARTESIAN_POINT ( 'NONE',  ( 26.99999999999998579, -7.850927237173508821, -1.251176053402193178 ) ) ;
#40422 = ORIENTED_EDGE ( 'NONE', *, *, #177, .T. ) ;
#40423 = DIRECTION ( 'NONE',  ( -1.000000000000000000, -0.000000000000000000, -0.000000000000000000 ) ) ;
#40424 = CARTESIAN_POINT ( 'NONE',  ( 50.14583333333332149, 2.130196079827356037, -7.950000000000043698 ) ) ;
#40425 = EDGE_CURVE ( 'NONE', #81393, #119020, #133261, .T. ) ;
#40426 = EDGE_LOOP ( 'NONE', ( #127186, #69860, #65103, #68265 ) ) ;
#40427 = B_SPLINE_CURVE_WITH_KNOTS ( 'NONE', 3,
 ( #101247, #99823, #122266, #1884, #134620, #35317, #79557, #68649, #28712, #62060, #4731, #71490, #38856, #117109, #103367, #59220 ),
 .UNSPECIFIED., .F., .F.,
 ( 4, 2, 2, 2, 2, 2, 2, 4 ),
 ( 0.000000000000000000, 0.0005146009271697703615, 0.001029201854339540723, 0.002058403708679101395, 0.003087605563018661851, 0.004116807417358222740, 0.006175211126037349722, 0.008233614834716476705 ),
 .UNSPECIFIED. ) ;
#40428 = CARTESIAN_POINT ( 'NONE',  ( 48.18398860626899705, 28.73617430169820608, 5.000000000000000000 ) ) ;
#40429 = ORIENTED_EDGE ( 'NONE', *, *, #131724, .F. ) ;
#40430 = EDGE_CURVE ( 'NONE', #128814, #115328, #124501, .T. ) ;
#40431 = DIRECTION ( 'NONE',  ( -0.7071067811865486830, -0.7071067811865464625, -0.000000000000000000 ) ) ;
#40432 = EDGE_LOOP ( 'NONE', ( #117011, #92339, #69639, #7405 ) ) ;
#40433 = CARTESIAN_POINT ( 'NONE',  ( 72.33376352523143282, 6.110000000000001208, 1.122388791418549305E-15 ) ) ;
#40434 = CIRCLE ( 'NONE', #14934, 2.500000000000000888 ) ;
#40435 = ORIENTED_EDGE ( 'NONE', *, *, #122239, .F. ) ;
#40436 = ORIENTED_EDGE ( 'NONE', *, *, #81815, .T. ) ;
#40437 = ADVANCED_FACE ( 'NONE', ( #14308 ), #134695, .F. ) ;
#40438 = CARTESIAN_POINT ( 'NONE',  ( 8.816011393731004731, 28.73617430169781173, 5.000000000000000000 ) ) ;
#40439 = AXIS2_PLACEMENT_3D ( 'NONE', #2879, #102927, #36937 ) ;
#40440 = LINE ( 'NONE', #118684, #31154 ) ;
#40442 =( BOUNDED_CURVE ( )  B_SPLINE_CURVE ( 2, ( #110446, #79327, #122770, #69132, #56858, #121339, #90891, #23457, #67726, #135120, #113311, #77170, #35084 ),
 .UNSPECIFIED., .F., .T. ) 
 B_SPLINE_CURVE_WITH_KNOTS ( ( 3, 2, 2, 2, 2, 2, 3 ),
 ( 0.03333333333333336063, 0.03611111111111113547, 0.03888888888888892420, 0.04166666666666669905, 0.04444444444444448084, 0.04722222222222226262, 0.05000000000000004441 ),
 .UNSPECIFIED. ) 
 CURVE ( )  GEOMETRIC_REPRESENTATION_ITEM ( )  RATIONAL_B_SPLINE_CURVE ( ( 0.9999999999999996669, 0.9659258262890686453, 1.000000000000000000, 0.9659258262890683122, 1.000000000000000000, 0.9659258262890683122, 1.000000000000000000, 0.9659258262890683122, 1.000000000000000000, 0.9659258262890683122, 1.000000000000000000, 0.9659258262890677571, 1.000000000000000444 ) ) 
 REPRESENTATION_ITEM ( '' )  );
#40441 = CARTESIAN_POINT ( 'NONE',  ( 110.8337635252314470, 6.110000000000001208, 1.122388791418549305E-15 ) ) ;
#40443 = DIRECTION ( 'NONE',  ( 0.6830127018922180770, -0.6830127018922204085, -0.2588190451025213501 ) ) ;
#40444 = AXIS2_PLACEMENT_3D ( 'NONE', #118400, #16967, #85070 ) ;
#40445 = CARTESIAN_POINT ( 'NONE',  ( 33.29974487139158867, -27.71228299555229313, 4.000000000000000000 ) ) ;
#40446 = DIRECTION ( 'NONE',  ( 0.7071067811865486830, -0.7071067811865464625, -0.000000000000000000 ) ) ;
#40447 = EDGE_CURVE ( 'NONE', #1803, #130345, #78158, .T. ) ;
#40448 = LINE ( 'NONE', #4886, #142599 ) ;
#40449 = LINE ( 'NONE', #60795, #81765 ) ;
#40450 = LINE ( 'NONE', #42600, #37529 ) ;
#40451 = LINE ( 'NONE', #118693, #26587 ) ;
#40452 = ORIENTED_EDGE ( 'NONE', *, *, #113999, .F. ) ;
#40453 = DIRECTION ( 'NONE',  ( 0.7071067811865487940, -0.7071067811865463515, 0.000000000000000000 ) ) ;
#40454 = AXIS2_PLACEMENT_3D ( 'NONE', #17459, #81328, #126238 ) ;
#40455 = ORIENTED_EDGE ( 'NONE', *, *, #102274, .T. ) ;
#40456 = VERTEX_POINT ( 'NONE', #88260 ) ;
#40457 = EDGE_LOOP ( 'NONE', ( #32841, #85665, #125263, #41918 ) ) ;
#40458 = EDGE_CURVE ( 'NONE', #87786, #22970, #90386, .T. ) ;
#40459 = ORIENTED_EDGE ( 'NONE', *, *, #14401, .T. ) ;
#40460 = CARTESIAN_POINT ( 'NONE',  ( -5.758305415748097289, 0.7592924766157034266, 14.37146558664984042 ) ) ;
#40461 = CARTESIAN_POINT ( 'NONE',  ( 34.47516574401891631, -14.97193265888402713, 4.998110765256834398 ) ) ;
#40462 = CARTESIAN_POINT ( 'NONE',  ( 0.000000000000000000, 0.000000000000000000, 5.000000000000000000 ) ) ;
#40463 = CARTESIAN_POINT ( 'NONE',  ( 0.000000000000000000, 0.000000000000000000, 5.000000000000000000 ) ) ;
#40464 = ORIENTED_EDGE ( 'NONE', *, *, #34838, .F. ) ;
#40465 = CARTESIAN_POINT ( 'NONE',  ( 3.298144211979590068, -48.98056306480232536, 39.49745726092411502 ) ) ;
#40466 = ORIENTED_EDGE ( 'NONE', *, *, #60800, .T. ) ;
#40467 = EDGE_CURVE ( 'NONE', #65577, #135321, #140791, .T. ) ;
#40468 = CIRCLE ( 'NONE', #38190, 6.349999999999997868 ) ;
#40469 = AXIS2_PLACEMENT_3D ( 'NONE', #33974, #134735, #45585 ) ;
#40470 = CARTESIAN_POINT ( 'NONE',  ( 3.041236474768552966, 0.000000000000000000, 7.934999999999990727 ) ) ;
#40471 = VECTOR ( 'NONE', #16538, 1000.000000000000000 ) ;
#40472 = DIRECTION ( 'NONE',  ( -0.000000000000000000, 0.000000000000000000, 1.000000000000000000 ) ) ;
#40473 = VECTOR ( 'NONE', #68765, 1000.000000000000000 ) ;
#40474 = LINE ( 'NONE', #82533, #2722 ) ;
#40475 = ORIENTED_EDGE ( 'NONE', *, *, #142835, .T. ) ;
#40476 = ORIENTED_EDGE ( 'NONE', *, *, #80269, .T. ) ;
#40477 = EDGE_CURVE ( 'NONE', #104186, #4701, #68663, .T. ) ;
#40478 = ORIENTED_EDGE ( 'NONE', *, *, #43035, .T. ) ;
#40479 = CARTESIAN_POINT ( 'NONE',  ( 55.18164086290596515, -52.14999999999999147, -41.64500000000001023 ) ) ;
#40480 = CARTESIAN_POINT ( 'NONE',  ( -7.940000000000001279, -33.26999999999999602, -10.00000000000000178 ) ) ;
#40481 = DIRECTION ( 'NONE',  ( -0.7071067811865487940, 0.7071067811865463515, -0.000000000000000000 ) ) ;
#40482 = DIRECTION ( 'NONE',  ( -1.000000000000000000, -0.000000000000000000, -0.000000000000000000 ) ) ;
#40483 = CARTESIAN_POINT ( 'NONE',  ( 15.20840764549667767, 3.061616997868380183E-16, -2.500000000000001332 ) ) ;
#40484 = CARTESIAN_POINT ( 'NONE',  ( -10.49999999999993250, 1.030536316426501564, -5.498701923753775311 ) ) ;
#40485 = CARTESIAN_POINT ( 'NONE',  ( 21.44840764549667611, 0.000000000000000000, 2.500000000000001332 ) ) ;
#40486 = CARTESIAN_POINT ( 'NONE',  ( 27.12543019189810067, 5.291415217122919401, 3.055000000000002824 ) ) ;
#40487 = EDGE_CURVE ( 'NONE', #121873, #121929, #22949, .T. ) ;
#40488 = CARTESIAN_POINT ( 'NONE',  ( 34.92499999999998295, -22.22500000000000142, 4.500000000000000888 ) ) ;
#40489 = ORIENTED_EDGE ( 'NONE', *, *, #29440, .T. ) ;
#40490 = DIRECTION ( 'NONE',  ( 0.7071067811865487940, -0.7071067811865463515, -0.000000000000000000 ) ) ;
#40491 = CARTESIAN_POINT ( 'NONE',  ( 0.000000000000000000, 0.000000000000000000, 5.000000000000000000 ) ) ;
#40492 = VERTEX_POINT ( 'NONE', #88983 ) ;
#40493 = CARTESIAN_POINT ( 'NONE',  ( 26.29320749275909463, 20.25929247661551358, 20.83292124670808931 ) ) ;
#40495 = VERTEX_POINT ( 'NONE', #1210 ) ;
#40494 = PLANE ( 'NONE',  #74267 ) ;
#40496 = EDGE_CURVE ( 'NONE', #113523, #48370, #67973, .T. ) ;
#40497 = DIRECTION ( 'NONE',  ( 0.3543493200069162685, -0.000000000000000000, -0.9351131265310288487 ) ) ;
#40498 =( NAMED_UNIT ( * ) SI_UNIT ( $, .STERADIAN. ) SOLID_ANGLE_UNIT ( ) );
#40499 = EDGE_LOOP ( 'NONE', ( #88887, #10491, #53522, #82832, #96518 ) ) ;
#40500 = CARTESIAN_POINT ( 'NONE',  ( -19.49999999999986500, 9.127013188829483425, 4.802533355213530086 ) ) ;
#40501 = ORIENTED_EDGE ( 'NONE', *, *, #79326, .T. ) ;
#40502 = CARTESIAN_POINT ( 'NONE',  ( 92.82919371712955581, -3.975000000000001865, 6.884901960086284411 ) ) ;
#40503 = CARTESIAN_POINT ( 'NONE',  ( 121.7041937171295700, -6.884901960086285300, -3.975000000000000089 ) ) ;
#40504 = CARTESIAN_POINT ( 'NONE',  ( 48.93336038379622721, 2.130196079827431532, -7.949999999999996625 ) ) ;
#40505 = FACE_OUTER_BOUND ( 'NONE', #20722, .T. ) ;
#40506 = FACE_OUTER_BOUND ( 'NONE', #136075, .T. ) ;
#40507 = LINE ( 'NONE', #128227, #131653 ) ;
#40508 = CARTESIAN_POINT ( 'NONE',  ( 3.645833333333333037, -1.633150327867689988, 6.094999999999989981 ) ) ;
#40509 = CARTESIAN_POINT ( 'NONE',  ( 12.08290314143522082, 3.967499999999992699, -6.871911579029513994 ) ) ;
#40510 = LINE ( 'NONE', #84712, #14260 ) ;
#40511 = DIRECTION ( 'NONE',  ( 0.3543493200069162685, -0.000000000000000000, -0.9351131265310288487 ) ) ;
#40512 = ORIENTED_EDGE ( 'NONE', *, *, #96496, .F. ) ;
#40513 = VECTOR ( 'NONE', #67929, 1000.000000000000000 ) ;
#40514 = EDGE_LOOP ( 'NONE', ( #60014, #2495, #115432, #2681 ) ) ;
#40515 = CARTESIAN_POINT ( 'NONE',  ( 80.62500000000000000, -7.950000000000000178, -4.867971026610729436E-16 ) ) ;
#40516 = CARTESIAN_POINT ( 'NONE',  ( 0.000000000000000000, 0.000000000000000000, 5.000000000000000000 ) ) ;
#40517 = ORIENTED_EDGE ( 'NONE', *, *, #142641, .F. ) ;
#40518 = EDGE_CURVE ( 'NONE', #80227, #20476, #115022, .T. ) ;
#40519 = CARTESIAN_POINT ( 'NONE',  ( 91.80836038379622721, 7.949999999999996625, 2.130196079827431088 ) ) ;
#40520 = CARTESIAN_POINT ( 'NONE',  ( -15.18398860626900237, 28.73617430169797871, 5.000000000000000000 ) ) ;
#40521 = CARTESIAN_POINT ( 'NONE',  ( 28.00000000000002487, -52.14999999999999147, 62.92500000000006111 ) ) ;
#40522 = EDGE_LOOP ( 'NONE', ( #28338, #86332, #62396, #122385 ) ) ;
#40523 = CARTESIAN_POINT ( 'NONE',  ( -34.49999999999976552, 3.054329344830908344, 4.994342998332172101 ) ) ;
#40524 = DIRECTION ( 'NONE',  ( 0.6830127018922180770, -0.6830127018922204085, -0.2588190451025213501 ) ) ;
#40525 = CARTESIAN_POINT ( 'NONE',  ( 4.499999999999966249, 14.14708470758591652, -0.5283514160166653539 ) ) ;
#40526 = EDGE_CURVE ( 'NONE', #11525, #35337, #23704, .T. ) ;
#40527 = EDGE_CURVE ( 'NONE', #131428, #19769, #126629, .T. ) ;
#40528 = DIRECTION ( 'NONE',  ( -1.000000000000000000, 0.000000000000000000, 3.596245529072721644E-15 ) ) ;
#40530 = EDGE_LOOP ( 'NONE', ( #73890, #30744, #69994, #57560, #71655, #124050 ) ) ;
#40529 = DIRECTION ( 'NONE',  ( 1.000000000000000000, 0.000000000000000000, 0.000000000000000000 ) ) ;
#40531 = CARTESIAN_POINT ( 'NONE',  ( 30.70612307739174796, 22.22500000000000142, 4.000000000000000000 ) ) ;
#40532 = CARTESIAN_POINT ( 'NONE',  ( 30.32816939922332367, 17.25929247661554200, 4.000000000000000000 ) ) ;
#40533 = PLANE ( 'NONE',  #86351 ) ;
#40534 = DIRECTION ( 'NONE',  ( -0.000000000000000000, 0.3543493200069153248, 0.9351131265310292928 ) ) ;
#40535 = LINE ( 'NONE', #1088, #119291 ) ;
#40536 = CARTESIAN_POINT ( 'NONE',  ( 60.59549430336050335, -44.02090675802819675, 34.92500000000511307 ) ) ;
#40537 = VECTOR ( 'NONE', #92556, 1000.000000000000227 ) ;
#40538 = VERTEX_POINT ( 'NONE', #13513 ) ;
#40539 = EDGE_LOOP ( 'NONE', ( #81856, #23693, #60210, #12545 ) ) ;
#40540 = CARTESIAN_POINT ( 'NONE',  ( 106.3129301918981042, -1.637169565754159617, -6.110000000000001208 ) ) ;
#40541 = ORIENTED_EDGE ( 'NONE', *, *, #105201, .T. ) ;
#40542 = VECTOR ( 'NONE', #43370, 1000.000000000000000 ) ;
#40543 = CARTESIAN_POINT ( 'NONE',  ( 127.6984665281585762, -50.67230138428261910, 37.61253110040533443 ) ) ;
#40544 = CARTESIAN_POINT ( 'NONE',  ( 6.707106781186499944, -12.74070752338415247, 5.000000000000000000 ) ) ;
#40545 = VERTEX_POINT ( 'NONE', #69373 ) ;
#40546 = EDGE_CURVE ( 'NONE', #37549, #4136, #110674, .T. ) ;
#40547 = CARTESIAN_POINT ( 'NONE',  ( -30.48921356237309510, -27.52281430457076894, 5.000000000000000000 ) ) ;
#40548 = CARTESIAN_POINT ( 'NONE',  ( 50.99451991528749062, 28.92564299267973738, 4.000000000000000000 ) ) ;
#40549 = CARTESIAN_POINT ( 'NONE',  ( 95.87043019189810877, -3.055000000000001492, 5.291415217122917625 ) ) ;
#40550 = AXIS2_PLACEMENT_3D ( 'NONE', #55836, #25306, #22436 ) ;
#40551 = ORIENTED_EDGE ( 'NONE', *, *, #23521, .T. ) ;
#40552 = AXIS2_PLACEMENT_3D ( 'NONE', #27679, #17518, #38575 ) ;
#40553 = DIRECTION ( 'NONE',  ( 0.7071067811865486830, -0.7071067811865464625, -0.000000000000000000 ) ) ;
#40554 = ORIENTED_EDGE ( 'NONE', *, *, #114039, .T. ) ;
#40555 = DIRECTION ( 'NONE',  ( 0.7071067811865486830, -0.7071067811865464625, -0.000000000000000000 ) ) ;
#40556 = DIRECTION ( 'NONE',  ( 0.000000000000000000, 0.000000000000000000, -1.000000000000000000 ) ) ;
#40557 = PLANE ( 'NONE',  #113356 ) ;
#40558 = ORIENTED_EDGE ( 'NONE', *, *, #46698, .F. ) ;
#40559 = ORIENTED_EDGE ( 'NONE', *, *, #68787, .F. ) ;
#40560 = ORIENTED_EDGE ( 'NONE', *, *, #94197, .T. ) ;
#40561 = CARTESIAN_POINT ( 'NONE',  ( 23.67183060077631396, 14.25929247661558286, 4.000000000000000000 ) ) ;
#40562 = CARTESIAN_POINT ( 'NONE',  ( 53.99451991528749062, 28.92564299267975869, 4.000000000000000000 ) ) ;
#40563 = CARTESIAN_POINT ( 'NONE',  ( 6.921236474768553748, -9.717572351234235426E-16, -7.934999999999990727 ) ) ;
#40564 = CARTESIAN_POINT ( 'NONE',  ( 22.31250000000000000, -4.461849672132299993, -4.461849672132299105 ) ) ;
#40565 = VECTOR ( 'NONE', #101117, 1000.000000000000000 ) ;
#40567 = AXIS2_PLACEMENT_3D ( 'NONE', #122806, #280, #47446 ) ;
#40566 =( NAMED_UNIT ( * ) PLANE_ANGLE_UNIT ( ) SI_UNIT ( $, .RADIAN. ) );
#40569 = EDGE_CURVE ( 'NONE', #20459, #59056, #55633, .T. ) ;
#40568 = AXIS2_PLACEMENT_3D ( 'NONE', #109955, #23669, #67941 ) ;
#40570 = VERTEX_POINT ( 'NONE', #99835 ) ;
#40572 = ORIENTED_EDGE ( 'NONE', *, *, #13836, .T. ) ;
#40571 = VECTOR ( 'NONE', #78585, 1000.000000000000000 ) ;
#40573 = EDGE_CURVE ( 'NONE', #124115, #140149, #21717, .T. ) ;
#40574 = AXIS2_PLACEMENT_3D ( 'NONE', #106445, #94873, #37687 ) ;
#40575 = LINE ( 'NONE', #129688, #128905 ) ;
#40576 = ORIENTED_EDGE ( 'NONE', *, *, #44502, .T. ) ;
#40577 = VERTEX_POINT ( 'NONE', #99091 ) ;
#40578 = EDGE_CURVE ( 'NONE', #65015, #120961, #33882, .T. ) ;
#40579 = EDGE_CURVE ( 'NONE', #20435, #19025, #47237, .T. ) ;
#40580 = CARTESIAN_POINT ( 'NONE',  ( 35.99451991528749772, 28.92564299267963079, 4.000000000000000000 ) ) ;
#40581 = ORIENTED_EDGE ( 'NONE', *, *, #116947, .T. ) ;
#40582 = CARTESIAN_POINT ( 'NONE',  ( 5.687500000000000000, 4.461849672132297329, -4.461849672132302658 ) ) ;
#40583 = FACE_OUTER_BOUND ( 'NONE', #83846, .T. ) ;
#40584 = DIRECTION ( 'NONE',  ( 0.7071067811865487940, 0.7071067811865463515, 0.000000000000000000 ) ) ;
#40585 = FACE_OUTER_BOUND ( 'NONE', #22661, .T. ) ;
#40586 = VERTEX_POINT ( 'NONE', #89670 ) ;
#40587 = LINE ( 'NONE', #29674, #53334 ) ;
#40588 = CARTESIAN_POINT ( 'NONE',  ( 36.43750000000000000, 5.819803920172574863, -5.819803920172573086 ) ) ;
#40589 = EDGE_CURVE ( 'NONE', #63037, #99871, #135351, .T. ) ;
#40590 = VERTEX_POINT ( 'NONE', #124444 ) ;
#40591 = CARTESIAN_POINT ( 'NONE',  ( -32.99451991528749062, 28.92564299267960948, 4.000000000000000000 ) ) ;
#40592 = DIRECTION ( 'NONE',  ( -0.000000000000000000, 0.000000000000000000, 1.000000000000000000 ) ) ;
#40593 = EDGE_CURVE ( 'NONE', #112076, #113191, #111415, .T. ) ;
#40594 = EDGE_LOOP ( 'NONE', ( #134080, #51435, #83585, #26810 ) ) ;
#40595 = CARTESIAN_POINT ( 'NONE',  ( 24.29974487139158867, -27.71228299555223273, 4.000000000000000000 ) ) ;
#40596 = ORIENTED_EDGE ( 'NONE', *, *, #12360, .F. ) ;
#40597 = ORIENTED_EDGE ( 'NONE', *, *, #21542, .T. ) ;
#40598 = ORIENTED_EDGE ( 'NONE', *, *, #122242, .T. ) ;
#40599 = CARTESIAN_POINT ( 'NONE',  ( 28.20376352523144803, 6.109999999999998543, 1.122388791418548911E-15 ) ) ;
#40600 = EDGE_CURVE ( 'NONE', #56871, #25054, #132896, .T. ) ;
#40601 = CARTESIAN_POINT ( 'NONE',  ( 34.49999999999975842, 10.46425560840038571, 4.994342998332157890 ) ) ;
#40602 = LINE ( 'NONE', #96354, #132900 ) ;
#40603 = CARTESIAN_POINT ( 'NONE',  ( 0.000000000000000000, 0.000000000000000000, 5.000000000000000000 ) ) ;
#40604 = LINE ( 'NONE', #5784, #109923 ) ;
#40605 = PLANE ( 'NONE',  #71430 ) ;
#40607 = CARTESIAN_POINT ( 'NONE',  ( -17.24139925780192328, 21.72500000000000142, 5.000000000000000000 ) ) ;
#40606 = DIRECTION ( 'NONE',  ( 0.000000000000000000, -1.000000000000000000, 0.000000000000000000 ) ) ;
#40608 = EDGE_CURVE ( 'NONE', #14910, #69767, #44039, .T. ) ;
#40609 = PLANE ( 'NONE',  #74822 ) ;
#40610 = DIRECTION ( 'NONE',  ( 0.7071067811865487940, -0.7071067811865463515, 0.000000000000000000 ) ) ;
#40611 = DIRECTION ( 'NONE',  ( -0.7071067811865486830, 0.7071067811865464625, 0.000000000000000000 ) ) ;
#40612 = DIRECTION ( 'NONE',  ( 0.7071067811865487940, 0.7071067811865463515, 0.000000000000000000 ) ) ;
#40613 = ORIENTED_EDGE ( 'NONE', *, *, #8789, .F. ) ;
#40614 = ORIENTED_EDGE ( 'NONE', *, *, #65947, .T. ) ;
#40616 = ORIENTED_EDGE ( 'NONE', *, *, #53400, .F. ) ;
#40615 = ADVANCED_FACE ( 'NONE', ( #121574 ), #121260, .T. ) ;
#40617 = ORIENTED_EDGE ( 'NONE', *, *, #98817, .F. ) ;
#40618 = DIRECTION ( 'NONE',  ( 0.000000000000000000, -1.000000000000000000, 0.000000000000000000 ) ) ;
#40619 = ORIENTED_EDGE ( 'NONE', *, *, #72988, .F. ) ;
#40620 = ORIENTED_EDGE ( 'NONE', *, *, #12683, .F. ) ;
#40621 = CARTESIAN_POINT ( 'NONE',  ( -21.18398860626899349, 28.73617430169802134, 5.000000000000000000 ) ) ;
#40622 = DIRECTION ( 'NONE',  ( 1.000000000000000000, 0.000000000000000000, 0.000000000000000000 ) ) ;
#40623 = CARTESIAN_POINT ( 'NONE',  ( 10.49999999999992895, -4.533600742197696043, 5.000000000000000000 ) ) ;
#40624 = CARTESIAN_POINT ( 'NONE',  ( -10.49999999999991829, 1.087461875839235814, 4.000000000000000000 ) ) ;
#40625 = EDGE_CURVE ( 'NONE', #29676, #129956, #4031, .T. ) ;
#40626 = ORIENTED_EDGE ( 'NONE', *, *, #106814, .T. ) ;
#40627 = ADVANCED_FACE ( 'NONE', ( #71507 ), #27994, .F. ) ;
#40628 = CARTESIAN_POINT ( 'NONE',  ( 27.68840764549667455, 9.139736423841732040E-16, 0.000000000000000000 ) ) ;
#40629 = VERTEX_POINT ( 'NONE', #60670 ) ;
#40630 = CARTESIAN_POINT ( 'NONE',  ( 21.15294044719737698, 0.000000000000000000, 2.500000000000000444 ) ) ;
#40631 = EDGE_CURVE ( 'NONE', #11751, #101542, #6192, .T. ) ;
#40632 = AXIS2_PLACEMENT_3D ( 'NONE', #111290, #88144, #31616 ) ;
#40633 = DIRECTION ( 'NONE',  ( 0.7071067811865486830, -0.7071067811865464625, -0.000000000000000000 ) ) ;
#40634 = CARTESIAN_POINT ( 'NONE',  ( 8.233736474768550195, 5.808823158059036373, 5.808823158059032821 ) ) ;
#40635 = VERTEX_POINT ( 'NONE', #25845 ) ;
#40636 = CARTESIAN_POINT ( 'NONE',  ( 89.01626352523143737, -4.472830434245839371, 4.472830434245839371 ) ) ;
#40637 = AXIS2_PLACEMENT_3D ( 'NONE', #134520, #11990, #121474 ) ;
#40638 = LINE ( 'NONE', #118146, #123122 ) ;
#40639 = ORIENTED_EDGE ( 'NONE', *, *, #77275, .T. ) ;
#40640 = ORIENTED_EDGE ( 'NONE', *, *, #34196, .F. ) ;
#40641 = DIRECTION ( 'NONE',  ( -0.7071067811865487940, 0.7071067811865463515, -0.000000000000000000 ) ) ;
#40642 = ORIENTED_EDGE ( 'NONE', *, *, #132781, .T. ) ;
#40643 = CARTESIAN_POINT ( 'NONE',  ( 18.32816939922339472, -15.74070752338412760, 4.000000000000000000 ) ) ;
#40644 = LINE ( 'NONE', #107990, #11686 ) ;
#40645 = PLANE ( 'NONE',  #53983 ) ;
#40646 = LINE ( 'NONE', #74715, #26371 ) ;
#40647 = ORIENTED_EDGE ( 'NONE', *, *, #129751, .T. ) ;
#40648 = CARTESIAN_POINT ( 'NONE',  ( -5.994519915287488843, 28.92564299267942118, 4.000000000000000000 ) ) ;
#40649 = VECTOR ( 'NONE', #104108, 1000.000000000000000 ) ;
#40650 = CARTESIAN_POINT ( 'NONE',  ( -26.99451991528749417, 28.92564299267956685, 4.000000000000000000 ) ) ;
#40651 = PLANE ( 'NONE',  #5150 ) ;
#40652 = ORIENTED_EDGE ( 'NONE', *, *, #32883, .T. ) ;
#40653 = DIRECTION ( 'NONE',  ( -1.000000000000000000, -0.000000000000000000, -0.000000000000000000 ) ) ;
#40654 = CARTESIAN_POINT ( 'NONE',  ( 12.48921356237309155, -27.52281430457064104, 5.000000000000000000 ) ) ;
#40655 = ORIENTED_EDGE ( 'NONE', *, *, #93875, .T. ) ;
#40657 = ORIENTED_EDGE ( 'NONE', *, *, #69358, .T. ) ;
#40656 = DIRECTION ( 'NONE',  ( -0.6830127018922181881, 0.6830127018922202975, -0.2588190451025214056 ) ) ;
#40658 = ORIENTED_EDGE ( 'NONE', *, *, #100702, .T. ) ;
#40659 = CARTESIAN_POINT ( 'NONE',  ( 19.49999999999986500, -6.839392718269110105, -8.480912228396132235 ) ) ;
#40660 = CARTESIAN_POINT ( 'NONE',  ( -3.183988606268992161, 28.73617430169789699, 5.000000000000000000 ) ) ;
#40661 = ORIENTED_EDGE ( 'NONE', *, *, #80992, .T. ) ;
#40662 = PLANE ( 'NONE',  #51190 ) ;
#40663 = VECTOR ( 'NONE', #36939, 1000.000000000000000 ) ;
#40664 = DIRECTION ( 'NONE',  ( -0.000000000000000000, 0.3543493200069153248, 0.9351131265310292928 ) ) ;
#40665 = VECTOR ( 'NONE', #376, 1000.000000000000000 ) ;
#40666 = DIRECTION ( 'NONE',  ( 0.6830127018922180770, -0.6830127018922202975, -0.2588190451025213501 ) ) ;
#40667 = VECTOR ( 'NONE', #135660, 1000.000000000000000 ) ;
#40668 = CARTESIAN_POINT ( 'NONE',  ( -36.18398860626899705, 28.73617430169812437, 5.000000000000000000 ) ) ;
#40669 = CARTESIAN_POINT ( 'NONE',  ( 0.1600000000000005584, -7.937054096915820089, 0.2840606438466312111 ) ) ;
#40670 = LINE ( 'NONE', #98598, #16539 ) ;
#40671 = CARTESIAN_POINT ( 'NONE',  ( 14.86920357848291196, 2.500000000000000444, 3.061616997868383634E-16 ) ) ;
#40672 = FACE_OUTER_BOUND ( 'NONE', #74711, .T. ) ;
#40673 = CARTESIAN_POINT ( 'NONE',  ( 57.29974487139158157, -27.71228299555246011, 4.000000000000000000 ) ) ;
#40674 = DIRECTION ( 'NONE',  ( -0.3543493200069162685, -0.000000000000000000, -0.9351131265310288487 ) ) ;
#40675 = CARTESIAN_POINT ( 'NONE',  ( 28.17183060077628554, 21.75929247661550647, 4.000000000000000000 ) ) ;
#40676 = AXIS2_PLACEMENT_3D ( 'NONE', #4756, #93250, #105536 ) ;
#40677 = CARTESIAN_POINT ( 'NONE',  ( 75.18398860626899705, 28.73617430169839793, 5.000000000000000000 ) ) ;
#40678 = FILL_AREA_STYLE ('',( #39254 ) ) ;
#40679 = ORIENTED_EDGE ( 'NONE', *, *, #66742, .T. ) ;
#40680 = EDGE_LOOP ( 'NONE', ( #57257, #84799, #60979, #40823 ) ) ;
#40681 = ORIENTED_EDGE ( 'NONE', *, *, #121887, .F. ) ;
#40682 = CARTESIAN_POINT ( 'NONE',  ( 107.3124999999999858, 5.819803920172571310, 5.819803920172575751 ) ) ;
#40683 = ORIENTED_EDGE ( 'NONE', *, *, #36228, .F. ) ;
#40684 = EDGE_LOOP ( 'NONE', ( #135649, #11218, #17715, #108486 ) ) ;
#40685 = ORIENTED_EDGE ( 'NONE', *, *, #142523, .T. ) ;
#40686 = CARTESIAN_POINT ( 'NONE',  ( -48.29974487139158867, -27.71228299555239971, 4.000000000000000000 ) ) ;
#40687 = CARTESIAN_POINT ( 'NONE',  ( 45.48921356237309510, -27.52281430457087197, 5.000000000000000000 ) ) ;
#40688 = EDGE_LOOP ( 'NONE', ( #106787, #75165, #40336, #80229 ) ) ;
#40689 = LINE ( 'NONE', #94336, #50916 ) ;
#40690 = LINE ( 'NONE', #52263, #108841 ) ;
#40691 = DIRECTION ( 'NONE',  ( 0.7071067811865487940, -0.7071067811865463515, 0.000000000000000000 ) ) ;
#40692 = CARTESIAN_POINT ( 'NONE',  ( -34.49999999999976552, -1.535744391599501490, 4.994342998332164996 ) ) ;
#40693 = CARTESIAN_POINT ( 'NONE',  ( 106.1670968585647756, -3.055000000000000160, -5.291415217122921177 ) ) ;
#40694 = EDGE_CURVE ( 'NONE', #52896, #59390, #70120, .T. ) ;
#40695 = VERTEX_POINT ( 'NONE', #72263 ) ;
#40696 = CARTESIAN_POINT ( 'NONE',  ( 30.18398860626900060, 28.73617430169808173, 5.000000000000000000 ) ) ;
#40697 = CARTESIAN_POINT ( 'NONE',  ( 25.49999999999982592, 3.653845994658417418, -4.504631822206428993 ) ) ;
#40698 = EDGE_CURVE ( 'NONE', #77145, #104436, #72969, .T. ) ;
#40699 = CARTESIAN_POINT ( 'NONE',  ( -25.49999999999982592, 11.52377502935400599, -1.522421517564026772 ) ) ;
#40700 = CARTESIAN_POINT ( 'NONE',  ( 15.68879807097514956, -1.757674993583058898, 4.000000000000000000 ) ) ;
#40701 = CARTESIAN_POINT ( 'NONE',  ( 0.000000000000000000, 0.000000000000000000, 7.950000000000000178 ) ) ;
#40702 = DIRECTION ( 'NONE',  ( 0.7071067811865487940, 0.7071067811865463515, 0.000000000000000000 ) ) ;
#40703 = FILL_AREA_STYLE_COLOUR ( '', #33846 ) ;
#40704 = CARTESIAN_POINT ( 'NONE',  ( -26.99999999999981171, -7.068876922607739921, 4.000000000000000000 ) ) ;
#40705 = DIRECTION ( 'NONE',  ( -1.000000000000000000, -1.224606353822377258E-16, -0.000000000000000000 ) ) ;
#40706 = DIRECTION ( 'NONE',  ( -0.7071067811865486830, -0.7071067811865464625, -0.000000000000000000 ) ) ;
#40707 = ORIENTED_EDGE ( 'NONE', *, *, #15024, .F. ) ;
#40708 = ORIENTED_EDGE ( 'NONE', *, *, #92270, .F. ) ;
#40709 = CARTESIAN_POINT ( 'NONE',  ( 30.02083333333332860, 7.949999999999999289, 2.130196079827431532 ) ) ;
#40710 = EDGE_LOOP ( 'NONE', ( #3464, #23065, #132038, #83784 ) ) ;
#40711 = EDGE_CURVE ( 'NONE', #83776, #80177, #17118, .T. ) ;
#40712 = DIRECTION ( 'NONE',  ( 0.7071067811865486830, -0.7071067811865464625, -0.000000000000000000 ) ) ;
#40713 = CARTESIAN_POINT ( 'NONE',  ( -3.489213562373097322, -27.52281430457057709, 5.000000000000000000 ) ) ;
#40714 = FACE_OUTER_BOUND ( 'NONE', #114285, .T. ) ;
#40715 = CARTESIAN_POINT ( 'NONE',  ( -22.49999999999984723, 19.39370406404965408, 1.459788787078254657 ) ) ;
#40716 = ADVANCED_FACE ( 'NONE', ( #114282 ), #83838, .F. ) ;
#40717 = CARTESIAN_POINT ( 'NONE',  ( -9.183988606268997046, 28.73617430169793607, 5.000000000000000000 ) ) ;
#40718 = LINE ( 'NONE', #84924, #114 ) ;
#40719 = CARTESIAN_POINT ( 'NONE',  ( 123.8704301918981230, -3.055000000000001492, 5.291415217122917625 ) ) ;
#40720 = VERTEX_POINT ( 'NONE', #136737 ) ;
#40721 = DIRECTION ( 'NONE',  ( 0.7071067811865486830, -0.7071067811865464625, -0.000000000000000000 ) ) ;
#40722 = ORIENTED_EDGE ( 'NONE', *, *, #72378, .T. ) ;
#40723 = FACE_OUTER_BOUND ( 'NONE', #80793, .T. ) ;
#40724 = EDGE_CURVE ( 'NONE', #96207, #89805, #138187, .T. ) ;
#40725 = CARTESIAN_POINT ( 'NONE',  ( -13.80981832425542954, -18.74070752338408852, 7.910009926591540008 ) ) ;
#40727 =( BOUNDED_CURVE ( )  B_SPLINE_CURVE ( 3, ( #71052, #56091, #89390, #33613 ),
 .UNSPECIFIED., .F., .T. ) 
 B_SPLINE_CURVE_WITH_KNOTS ( ( 4, 4 ),
 ( 4.350170835173029715, 4.500739107949200069 ),
 .UNSPECIFIED. ) 
 CURVE ( )  GEOMETRIC_REPRESENTATION_ITEM ( )  RATIONAL_B_SPLINE_CURVE ( ( 1.000000000000000000, 0.9981116584018959736, 0.9981116584018959736, 1.000000000000000000 ) ) 
 REPRESENTATION_ITEM ( '' )  );
#40726 = SURFACE_SIDE_STYLE ('',( #62480 ) ) ;
#40728 = LINE ( 'NONE', #74064, #9345 ) ;
#40729 = VERTEX_POINT ( 'NONE', #4748 ) ;
#40730 = CARTESIAN_POINT ( 'NONE',  ( 41.70876352523143993, -7.482591942790329030E-16, 6.110000000000001208 ) ) ;
#40731 = EDGE_LOOP ( 'NONE', ( #103639, #99539, #10078, #75918 ) ) ;
#40732 = DIRECTION ( 'NONE',  ( 0.000000000000000000, -1.000000000000000000, 0.000000000000000000 ) ) ;
#40733 = DIRECTION ( 'NONE',  ( -0.7071067811865487940, 0.7071067811865463515, -0.000000000000000000 ) ) ;
#40734 = PLANE ( 'NONE',  #82562 ) ;
#40735 = EDGE_CURVE ( 'NONE', #113219, #108055, #126567, .T. ) ;
#40736 = CARTESIAN_POINT ( 'NONE',  ( -2.994519915287485734, 28.92564299267940342, 4.000000000000000000 ) ) ;
#40737 = VECTOR ( 'NONE', #38404, 1000.000000000000000 ) ;
#40738 = CARTESIAN_POINT ( 'NONE',  ( 34.76626352523145158, 4.472830434245839371, -4.472830434245838482 ) ) ;
#40739 = EDGE_LOOP ( 'NONE', ( #88976, #77739, #55258, #63137, #29187 ) ) ;
#40740 = AXIS2_PLACEMENT_3D ( 'NONE', #111875, #122003, #99534 ) ;
#40741 = EDGE_CURVE ( 'NONE', #57945, #30286, #58538, .T. ) ;
#40742 = DIRECTION ( 'NONE',  ( -0.6830127018922180770, -0.6830127018922204085, -0.2588190451025213501 ) ) ;
#40743 = EDGE_LOOP ( 'NONE', ( #46907, #89100, #4034, #77700 ) ) ;
#40744 = ORIENTED_EDGE ( 'NONE', *, *, #112172, .T. ) ;
#40745 = EDGE_LOOP ( 'NONE', ( #68473, #41778, #56653, #142968 ) ) ;
#40746 = EDGE_CURVE ( 'NONE', #93317, #73359, #115668, .T. ) ;
#40747 = ADVANCED_FACE ( 'NONE', ( #102706 ), #38871, .T. ) ;
#40748 = DIRECTION ( 'NONE',  ( 0.000000000000000000, -1.000000000000000000, 0.000000000000000000 ) ) ;
#40749 = DIRECTION ( 'NONE',  ( -0.7071067811865486830, -0.7071067811865464625, 0.000000000000000000 ) ) ;
#40750 = ORIENTED_EDGE ( 'NONE', *, *, #2153, .F. ) ;
#40751 = LINE ( 'NONE', #29841, #4234 ) ;
#40752 = AXIS2_PLACEMENT_3D ( 'NONE', #89520, #24955, #66361 ) ;
#40753 = LINE ( 'NONE', #8764, #29744 ) ;
#40754 = EDGE_CURVE ( 'NONE', #41681, #130550, #93245, .T. ) ;
#40755 = DIRECTION ( 'NONE',  ( -1.000000000000000000, -0.000000000000000000, -0.000000000000000000 ) ) ;
#40756 = FACE_BOUND ( 'NONE', #66190, .T. ) ;
#40757 = EDGE_CURVE ( 'NONE', #37138, #81345, #136030, .T. ) ;
#40758 = ORIENTED_EDGE ( 'NONE', *, *, #141487, .T. ) ;
#40759 = DIRECTION ( 'NONE',  ( 0.7071067811865487940, 0.7071067811865463515, -0.000000000000000000 ) ) ;
#40760 = CARTESIAN_POINT ( 'NONE',  ( -34.49999999999975842, 22.21934299833216997, 4.348028800457638177 ) ) ;
#40761 = DIRECTION ( 'NONE',  ( 0.6830127018922181881, 0.6830127018922202975, -0.2588190451025214056 ) ) ;
#40762 = ADVANCED_FACE ( 'NONE', ( #37455 ), #125893, .F. ) ;
#40763 = EDGE_LOOP ( 'NONE', ( #107780, #53815, #11996, #121834 ) ) ;
#40764 = LINE ( 'NONE', #84966, #64342 ) ;
#40765 = ORIENTED_EDGE ( 'NONE', *, *, #22329, .F. ) ;
#40766 = EDGE_LOOP ( 'NONE', ( #37367, #51210, #139036 ) ) ;
#40767 = FACE_OUTER_BOUND ( 'NONE', #76613, .T. ) ;
#40768 = VECTOR ( 'NONE', #68033, 1000.000000000000000 ) ;
#40769 = ORIENTED_EDGE ( 'NONE', *, *, #28023, .T. ) ;
#40770 = AXIS2_PLACEMENT_3D ( 'NONE', #8900, #187, #20526 ) ;
#40771 = CARTESIAN_POINT ( 'NONE',  ( 61.16209685856478728, -5.291415217122919401, 3.054999999999997939 ) ) ;
#40772 = ORIENTED_EDGE ( 'NONE', *, *, #84240, .F. ) ;
#40773 = EDGE_CURVE ( 'NONE', #70580, #101203, #104090, .T. ) ;
#40774 = LINE ( 'NONE', #6651, #108918 ) ;
#40775 = VECTOR ( 'NONE', #59452, 1000.000000000000000 ) ;
#40776 = CARTESIAN_POINT ( 'NONE',  ( -23.99451991528749062, 28.92564299267954908, 4.000000000000000000 ) ) ;
#40777 = ORIENTED_EDGE ( 'NONE', *, *, #53610, .T. ) ;
#40778 = PLANE ( 'NONE',  #49171 ) ;
#40779 = VECTOR ( 'NONE', #140675, 999.9999999999998863 ) ;
#40780 = EDGE_CURVE ( 'NONE', #96557, #137344, #85938, .T. ) ;
#40781 = DIRECTION ( 'NONE',  ( -0.6830127018922180770, -0.6830127018922204085, -0.2588190451025213501 ) ) ;
#40782 = DIRECTION ( 'NONE',  ( 4.681814790819592407E-17, 0.3543493200069153248, 0.9351131265310292928 ) ) ;
#40783 = CARTESIAN_POINT ( 'NONE',  ( 15.48921356237309510, -27.52281430457066236, 5.000000000000000000 ) ) ;
#40784 = CARTESIAN_POINT ( 'NONE',  ( 34.92499999999998295, -21.18334561358932433, 4.500000000000000888 ) ) ;
#40785 =( NAMED_UNIT ( * ) PLANE_ANGLE_UNIT ( ) SI_UNIT ( $, .RADIAN. ) );
#40786 = ORIENTED_EDGE ( 'NONE', *, *, #13155, .F. ) ;
#40787 = ORIENTED_EDGE ( 'NONE', *, *, #64059, .F. ) ;
#40788 = DIRECTION ( 'NONE',  ( 0.3543493200069162685, -0.000000000000000000, -0.9351131265310288487 ) ) ;
#40789 = CARTESIAN_POINT ( 'NONE',  ( 9.489213562373095101, -27.52281430457062328, 5.000000000000000000 ) ) ;
#40790 = VERTEX_POINT ( 'NONE', #18507 ) ;
#40791 = ORIENTED_EDGE ( 'NONE', *, *, #12515, .T. ) ;
#40792 = EDGE_LOOP ( 'NONE', ( #44125, #103540, #141093, #107394 ) ) ;
#40793 = CARTESIAN_POINT ( 'NONE',  ( 15.52000000000000135, 2.055000000000001492, 0.000000000000000000 ) ) ;
#40794 = LINE ( 'NONE', #19028, #71679 ) ;
#40795 = ORIENTED_EDGE ( 'NONE', *, *, #32094, .T. ) ;
#40796 = CARTESIAN_POINT ( 'NONE',  ( -19.17183060077633883, 12.75929247661559174, 4.000000000000000000 ) ) ;
#40797 = EDGE_CURVE ( 'NONE', #15438, #105436, #96085, .T. ) ;
#40798 = ADVANCED_FACE ( 'NONE', ( #97513 ), #8339, .F. ) ;
#40799 = CARTESIAN_POINT ( 'NONE',  ( 17.12956980810188767, -3.967499999999998028, -6.871911579029511330 ) ) ;
#40800 = CARTESIAN_POINT ( 'NONE',  ( 0.000000000000000000, 0.4000000000000001332, -2.015694669338588429 ) ) ;
#40801 = ORIENTED_EDGE ( 'NONE', *, *, #130583, .T. ) ;
#40802 = CARTESIAN_POINT ( 'NONE',  ( 123.7245968585647660, -1.637169565754161171, 6.109999999999998543 ) ) ;
#40803 = CARTESIAN_POINT ( 'NONE',  ( 57.48921356237308800, -27.52281430457095368, 5.000000000000000000 ) ) ;
#40804 = CARTESIAN_POINT ( 'NONE',  ( 50.99451991528749062, 28.92564299267973738, 4.000000000000000000 ) ) ;
#40806 = ORIENTED_EDGE ( 'NONE', *, *, #45502, .T. ) ;
#40805 = LINE ( 'NONE', #28510, #47216 ) ;
#40807 = CARTESIAN_POINT ( 'NONE',  ( 0.000000000000000000, 0.000000000000000000, 5.000000000000000000 ) ) ;
#40808 = ORIENTED_EDGE ( 'NONE', *, *, #69073, .F. ) ;
#40809 = DIRECTION ( 'NONE',  ( -0.7071067811865487940, 0.7071067811865463515, 0.000000000000000000 ) ) ;
#40810 = CARTESIAN_POINT ( 'NONE',  ( 0.2997448713915885632, -27.71228299555206220, 4.000000000000000000 ) ) ;
#40811 = CARTESIAN_POINT ( 'NONE',  ( -11.38161509397997051, -2.240707523384260824, 13.37739548510242038 ) ) ;
#40812 = ORIENTED_EDGE ( 'NONE', *, *, #2759, .T. ) ;
#40813 = CARTESIAN_POINT ( 'NONE',  ( 14.99999999999990763, -3.412538124160717778, 4.000000000000000000 ) ) ;
#40814 = CARTESIAN_POINT ( 'NONE',  ( 30.43680103220810551, -12.74070752338415602, 9.898150129686305476 ) ) ;
#40815 = DIRECTION ( 'NONE',  ( -0.7071067811865486830, -0.7071067811865464625, 0.000000000000000000 ) ) ;
#40816 = VECTOR ( 'NONE', #70657, 1000.000000000000000 ) ;
#40817 = ORIENTED_EDGE ( 'NONE', *, *, #107580, .F. ) ;
#40818 = PLANE ( 'NONE',  #108686 ) ;
#40819 = LINE ( 'NONE', #127093, #47027 ) ;
#40820 = DIRECTION ( 'NONE',  ( -0.7071067811865487940, 0.7071067811865463515, 0.000000000000000000 ) ) ;
#40821 = PLANE ( 'NONE',  #132886 ) ;
#40822 = FACE_OUTER_BOUND ( 'NONE', #57812, .T. ) ;
#40823 = ORIENTED_EDGE ( 'NONE', *, *, #87413, .T. ) ;
#40824 = ORIENTED_EDGE ( 'NONE', *, *, #30583, .T. ) ;
#40825 = CARTESIAN_POINT ( 'NONE',  ( 18.48921356237309510, -27.52281430457068367, 5.000000000000000000 ) ) ;
#40826 = DIRECTION ( 'NONE',  ( -0.7071067811865486830, -0.7071067811865464625, 0.000000000000000000 ) ) ;
#40827 = CARTESIAN_POINT ( 'NONE',  ( 10.18706980810188689, -2.126176841940956130, 7.934999999999991616 ) ) ;
#40828 = AXIS2_PLACEMENT_3D ( 'NONE', #12743, #123695, #34517 ) ;
#40829 = DIRECTION ( 'NONE',  ( -0.000000000000000000, 0.000000000000000000, 1.000000000000000000 ) ) ;
#40830 = DIRECTION ( 'NONE',  ( 0.7071067811865487940, 0.7071067811865463515, 0.000000000000000000 ) ) ;
#40831 = CARTESIAN_POINT ( 'NONE',  ( -0.4892135623730947680, -27.52281430457055578, 5.000000000000000000 ) ) ;
#40832 = VECTOR ( 'NONE', #1985, 1000.000000000000000 ) ;
#40833 = ORIENTED_EDGE ( 'NONE', *, *, #91310, .F. ) ;
#40834 = DIRECTION ( 'NONE',  ( -0.6830127018922181881, 0.6830127018922202975, -0.2588190451025214056 ) ) ;
#40835 = LINE ( 'NONE', #131417, #23602 ) ;
#40836 = DIRECTION ( 'NONE',  ( 0.7071067811865487940, 0.7071067811865463515, 0.000000000000000000 ) ) ;
#40837 = FACE_OUTER_BOUND ( 'NONE', #101665, .T. ) ;
#40838 = CARTESIAN_POINT ( 'NONE',  ( 38.55793019189810877, 6.110000000000001208, -1.637169565754156286 ) ) ;
#40839 = FACE_OUTER_BOUND ( 'NONE', #36405, .T. ) ;
#40840 = ORIENTED_EDGE ( 'NONE', *, *, #65609, .T. ) ;
#40841 = FACE_OUTER_BOUND ( 'NONE', #49764, .T. ) ;
#40842 = ORIENTED_EDGE ( 'NONE', *, *, #26102, .T. ) ;
#40843 = COLOUR_RGB ( '', 0.66274510, 0.83137255, 0.94901961) ;
#40844 = EDGE_LOOP ( 'NONE', ( #97049, #42340, #74450, #132582 ) ) ;
#40845 = LINE ( 'NONE', #73484, #8375 ) ;
#40846 = CARTESIAN_POINT ( 'NONE',  ( -11.99451991528749417, 28.92564299267946382, 4.000000000000000000 ) ) ;
#40847 = LINE ( 'NONE', #127881, #25230 ) ;
#40848 = DIRECTION ( 'NONE',  ( 0.7071067811865487940, 0.7071067811865463515, 0.000000000000000000 ) ) ;
#40849 = EDGE_CURVE ( 'NONE', #82150, #132831, #29408, .T. ) ;
#40850 = CARTESIAN_POINT ( 'NONE',  ( -34.92500000000001137, 22.22500000000000142, 4.000000000000000000 ) ) ;
#40851 = VECTOR ( 'NONE', #44112, 1000.000000000000000 ) ;
#40852 = CARTESIAN_POINT ( 'NONE',  ( 81.79166666666667140, 3.975000000000003642, -6.884901960086285300 ) ) ;
#40853 = CARTESIAN_POINT ( 'NONE',  ( 128.9683591370937847, -52.14999999999999147, 41.64499999999998181 ) ) ;
#40854 = EDGE_CURVE ( 'NONE', #84071, #116753, #95383, .T. ) ;
#40855 = EDGE_CURVE ( 'NONE', #131359, #133539, #115785, .T. ) ;
#40856 = ORIENTED_EDGE ( 'NONE', *, *, #134066, .T. ) ;
#40857 = CARTESIAN_POINT ( 'NONE',  ( 34.49999999999975842, -2.945670655169024155, 4.994342998332159667 ) ) ;
#40858 = CARTESIAN_POINT ( 'NONE',  ( 30.48921356237309510, -27.52281430457076894, 5.000000000000000000 ) ) ;
#40859 = DIRECTION ( 'NONE',  ( -0.6830127018922180770, -0.6830127018922204085, -0.2588190451025213501 ) ) ;
#40860 = CARTESIAN_POINT ( 'NONE',  ( -0.2997448713915885632, -27.71228299555206220, 4.000000000000000000 ) ) ;
#40861 = DIRECTION ( 'NONE',  ( -0.6830127018922180770, -0.6830127018922204085, -0.2588190451025213501 ) ) ;
#40862 = CIRCLE ( 'NONE', #15364, 3.000000000000002220 ) ;
#40863 = DIRECTION ( 'NONE',  ( 1.000000000000000000, 0.000000000000000000, 0.000000000000000000 ) ) ;
#40865 = EDGE_CURVE ( 'NONE', #65878, #8725, #17800, .T. ) ;
#40864 = CIRCLE ( 'NONE', #45555, 2.999999999999999112 ) ;
#40867 = EDGE_CURVE ( 'NONE', #131518, #77993, #106967, .T. ) ;
#40866 = CARTESIAN_POINT ( 'NONE',  ( 65.55836038379622721, -7.949999999999997513, -2.130196079827425759 ) ) ;
#40868 = VECTOR ( 'NONE', #115200, 1000.000000000000227 ) ;
#40869 = DIRECTION ( 'NONE',  ( 0.7071067811865486830, -0.7071067811865464625, -0.000000000000000000 ) ) ;
#40870 = ORIENTED_EDGE ( 'NONE', *, *, #124288, .T. ) ;
#40871 = ORIENTED_EDGE ( 'NONE', *, *, #108769, .F. ) ;
#40872 = CARTESIAN_POINT ( 'NONE',  ( 59.33333333333333570, -6.884901960086287964, 3.974999999999998312 ) ) ;
#40873 = DIRECTION ( 'NONE',  ( -0.7071067811865486830, -0.7071067811865464625, -0.000000000000000000 ) ) ;
#40874 = ADVANCED_FACE ( 'NONE', ( #20669 ), #131594, .F. ) ;
#40875 = LINE ( 'NONE', #29267, #4483 ) ;
#40877 = LINE ( 'NONE', #129286, #34448 ) ;
#40876 = AXIS2_PLACEMENT_3D ( 'NONE', #10685, #75285, #120897 ) ;
#40878 = ORIENTED_EDGE ( 'NONE', *, *, #35279, .F. ) ;
#40879 = DIRECTION ( 'NONE',  ( 0.6830127018922180770, -0.6830127018922204085, -0.2588190451025214056 ) ) ;
#40880 = EDGE_CURVE ( 'NONE', #8478, #139534, #140324, .T. ) ;
#40881 = CARTESIAN_POINT ( 'NONE',  ( 45.50043019189810423, -3.055000000000002380, 5.291415217122920289 ) ) ;
#40882 = ORIENTED_EDGE ( 'NONE', *, *, #48127, .T. ) ;
#40883 = DIRECTION ( 'NONE',  ( -0.7071067811865486830, -0.7071067811865464625, 0.000000000000000000 ) ) ;
#40884 = ORIENTED_EDGE ( 'NONE', *, *, #46310, .T. ) ;
#40885 = ORIENTED_EDGE ( 'NONE', *, *, #138887, .F. ) ;
#40886 = CARTESIAN_POINT ( 'NONE',  ( 23.29289321881330110, -12.74070752338415247, 5.000000000000000000 ) ) ;
#40887 = ADVANCED_FACE ( 'NONE', ( #130176 ), #6903, .F. ) ;
#40888 = CARTESIAN_POINT ( 'NONE',  ( 25.39999999999999858, -30.18000000000009564, 15.92499999999935945 ) ) ;
#40889 = DIRECTION ( 'NONE',  ( -0.7071067811865487940, 0.7071067811865463515, 0.000000000000000000 ) ) ;
#40890 =( NAMED_UNIT ( * ) PLANE_ANGLE_UNIT ( ) SI_UNIT ( $, .RADIAN. ) );
#40891 = VERTEX_POINT ( 'NONE', #85210 ) ;
#40892 = DIRECTION ( 'NONE',  ( 1.000000000000000000, 1.224606353822377258E-16, 0.000000000000000000 ) ) ;
#40894 = VERTEX_POINT ( 'NONE', #9035 ) ;
#40893 = DIRECTION ( 'NONE',  ( -0.7071067811865487940, 0.7071067811865463515, 0.000000000000000000 ) ) ;
#40895 = LINE ( 'NONE', #129308, #16089 ) ;
#40896 = DIRECTION ( 'NONE',  ( 0.7071067811865487940, 0.7071067811865463515, 0.000000000000000000 ) ) ;
#40897 = CARTESIAN_POINT ( 'NONE',  ( 1.554198602559970332, -0.4000000000000004108, 2.412907414356850744 ) ) ;
#40898 = EDGE_CURVE ( 'NONE', #101043, #129287, #76518, .T. ) ;
#40899 = LINE ( 'NONE', #74243, #9005 ) ;
#40900 = VERTEX_POINT ( 'NONE', #96766 ) ;
#40901 = ORIENTED_EDGE ( 'NONE', *, *, #79213, .F. ) ;
#40902 = PLANE ( 'NONE',  #50051 ) ;
#40903 = CARTESIAN_POINT ( 'NONE',  ( 66.26626352523145158, 4.472830434245839371, -4.472830434245838482 ) ) ;
#40904 = CARTESIAN_POINT ( 'NONE',  ( 22.58990935480154150, 9.759292476615614831, 11.28811694763784068 ) ) ;
#40905 = EDGE_CURVE ( 'NONE', #117114, #17080, #62072, .T. ) ;
#40906 = PLANE ( 'NONE',  #73263 ) ;
#40907 = LINE ( 'NONE', #52478, #6133 ) ;
#40908 = ORIENTED_EDGE ( 'NONE', *, *, #19568, .T. ) ;
#40909 = VERTEX_POINT ( 'NONE', #31570 ) ;
#40910 = VECTOR ( 'NONE', #121104, 1000.000000000000000 ) ;
#40911 = LINE ( 'NONE', #127934, #49179 ) ;
#40912 = PRESENTATION_STYLE_ASSIGNMENT (( #51802 ) ) ;
#40913 = ORIENTED_EDGE ( 'NONE', *, *, #103899, .F. ) ;
#40914 = EDGE_CURVE ( 'NONE', #75083, #59733, #30868, .T. ) ;
#40915 = ORIENTED_EDGE ( 'NONE', *, *, #35708, .T. ) ;
#40916 = LINE ( 'NONE', #127939, #37453 ) ;
#40918 = EDGE_CURVE ( 'NONE', #53085, #83276, #119956, .T. ) ;
#40917 = ORIENTED_EDGE ( 'NONE', *, *, #140432, .F. ) ;
#40919 = FACE_OUTER_BOUND ( 'NONE', #135445, .T. ) ;
#40920 = LINE ( 'NONE', #9696, #45641 ) ;
#40921 = VECTOR ( 'NONE', #134286, 999.9999999999998863 ) ;
#40922 = EDGE_CURVE ( 'NONE', #96698, #98296, #75793, .T. ) ;
#40923 = PLANE ( 'NONE',  #83626 ) ;
#40924 = VECTOR ( 'NONE', #128305, 1000.000000000000000 ) ;
#40925 = FACE_BOUND ( 'NONE', #51450, .T. ) ;
#40926 = CARTESIAN_POINT ( 'NONE',  ( -28.17183060077627843, -17.24070752338410273, 4.000000000000000000 ) ) ;
#40927 = FACE_OUTER_BOUND ( 'NONE', #38118, .T. ) ;
#40928 = CARTESIAN_POINT ( 'NONE',  ( -34.92500000000001137, -4.199905483972744769, 4.759050581649340472 ) ) ;
#40930 = EDGE_LOOP ( 'NONE', ( #8631, #124414, #79194, #1276 ) ) ;
#40929 = LINE ( 'NONE', #50379, #129196 ) ;
#40931 = LINE ( 'NONE', #8255, #120412 ) ;
#40932 = CONTEXT_DEPENDENT_SHAPE_REPRESENTATION ( #3143, #104800 ) ;
#40934 = ORIENTED_EDGE ( 'NONE', *, *, #124207, .T. ) ;
#40933 = VECTOR ( 'NONE', #93724, 1000.000000000000000 ) ;
#40935 = ORIENTED_EDGE ( 'NONE', *, *, #80975, .F. ) ;
#40936 = CARTESIAN_POINT ( 'NONE',  ( 83.62043019189812298, 3.055000000000001936, -5.291415217122916737 ) ) ;
#40937 = VERTEX_POINT ( 'NONE', #109108 ) ;
#40938 = VECTOR ( 'NONE', #96853, 1000.000000000000000 ) ;
#40939 = ADVANCED_FACE ( 'NONE', ( #54067 ), #89508, .F. ) ;
#40940 = CARTESIAN_POINT ( 'NONE',  ( 3.679462845988301645, -22.22500000000000142, -9.628674082947240365 ) ) ;
#40941 = DIRECTION ( 'NONE',  ( -1.000000000000000000, -1.224606353822377258E-16, -0.000000000000000000 ) ) ;
#40942 = DIRECTION ( 'NONE',  ( 0.7071067811865487940, 0.7071067811865463515, 0.000000000000000000 ) ) ;
#40943 = DIRECTION ( 'NONE',  ( 1.000000000000000000, 0.000000000000000000, 0.000000000000000000 ) ) ;
#40944 = LINE ( 'NONE', #8271, #140371 ) ;
#40945 = CARTESIAN_POINT ( 'NONE',  ( 16.49999999999988276, 16.18958161055404332, -11.56426086740807513 ) ) ;
#40946 = DIRECTION ( 'NONE',  ( 0.000000000000000000, -1.000000000000000000, 0.000000000000000000 ) ) ;
#40947 = CARTESIAN_POINT ( 'NONE',  ( -32.99999999999976552, -6.412538124160687580, 4.000000000000000000 ) ) ;
#40948 = SURFACE_STYLE_FILL_AREA ( #32217 ) ;
#40949 = ORIENTED_EDGE ( 'NONE', *, *, #30590, .F. ) ;
#40950 = CARTESIAN_POINT ( 'NONE',  ( -3.489213562373097322, -27.52281430457057709, 5.000000000000000000 ) ) ;
#40951 = CARTESIAN_POINT ( 'NONE',  ( -3.489213562373097322, -27.52281430457057709, 5.000000000000000000 ) ) ;
#40952 = EDGE_LOOP ( 'NONE', ( #125751, #127803, #77501, #32013 ) ) ;
#40954 = ORIENTED_EDGE ( 'NONE', *, *, #142945, .T. ) ;
#40953 = AXIS2_PLACEMENT_3D ( 'NONE', #64990, #103283, #33790 ) ;
#40955 = ORIENTED_EDGE ( 'NONE', *, *, #122748, .F. ) ;
#40956 = CARTESIAN_POINT ( 'NONE',  ( 31.79209685856476852, -5.291415217122921177, 3.054999999999999272 ) ) ;
#40957 = VERTEX_POINT ( 'NONE', #112683 ) ;
#40958 = CARTESIAN_POINT ( 'NONE',  ( 46.50000000000000000, 0.000000000000000000, -7.950000000000000178 ) ) ;
#40959 = CIRCLE ( 'NONE', #119568, 2.500000000000000888 ) ;
#40961 = CIRCLE ( 'NONE', #68822, 2.500000000000000888 ) ;
#40960 = CONICAL_SURFACE ( 'NONE', #142781, 2.055000000000001048, 0.9599310885968758145 ) ;
#40962 = EDGE_CURVE ( 'NONE', #143327, #49398, #34415, .T. ) ;
#40963 = STYLED_ITEM ( 'NONE', ( #99134 ), #109467 ) ;
#40964 = CARTESIAN_POINT ( 'NONE',  ( 23.81663961620377279, -1.633150327867691987, -6.094999999999989093 ) ) ;
#40965 = CARTESIAN_POINT ( 'NONE',  ( -3.933891695358868734, 12.14980826004766712, -25.57915494108756249 ) ) ;
#40966 = VERTEX_POINT ( 'NONE', #78640 ) ;
#40967 = CARTESIAN_POINT ( 'NONE',  ( 10.37159235450332062, 2.500000000000001776, 0.000000000000000000 ) ) ;
#40968 = VECTOR ( 'NONE', #113615, 1000.000000000000000 ) ;
#40969 = ORIENTED_EDGE ( 'NONE', *, *, #51057, .F. ) ;
#40970 = FACE_OUTER_BOUND ( 'NONE', #35521, .T. ) ;
#40971 = CARTESIAN_POINT ( 'NONE',  ( 54.18398860626899705, 28.73617430169825226, 5.000000000000000000 ) ) ;
#40973 = ORIENTED_EDGE ( 'NONE', *, *, #13956, .F. ) ;
#40972 = PLANE ( 'NONE',  #104990 ) ;
#40974 = ORIENTED_EDGE ( 'NONE', *, *, #4358, .F. ) ;
#40975 = EDGE_CURVE ( 'NONE', #140166, #96665, #23533, .T. ) ;
#40976 = CARTESIAN_POINT ( 'NONE',  ( 12.69999999999999574, -22.26999999999999247, -39.50000000000000000 ) ) ;
#40977 = LINE ( 'NONE', #75756, #107267 ) ;
#40978 = EDGE_LOOP ( 'NONE', ( #61615, #20072, #116683, #80024 ) ) ;
#40979 = ADVANCED_FACE ( 'NONE', ( #56915 ), #101088, .F. ) ;
#40980 = CARTESIAN_POINT ( 'NONE',  ( -31.82816939922331656, -20.24070752338406720, 4.000000000000000000 ) ) ;
#40981 = ORIENTED_EDGE ( 'NONE', *, *, #17739, .T. ) ;
#40982 = VERTEX_POINT ( 'NONE', #46778 ) ;
#40983 = ORIENTED_EDGE ( 'NONE', *, *, #65517, .F. ) ;
#40984 = CARTESIAN_POINT ( 'NONE',  ( -30.48921356237309510, -27.52281430457076894, 5.000000000000000000 ) ) ;
#40985 = CARTESIAN_POINT ( 'NONE',  ( 20.20710678118641113, 12.75929247661558286, 5.000000000000000000 ) ) ;
#40986 = DIRECTION ( 'NONE',  ( 0.7071067811865487940, 0.7071067811865463515, 0.000000000000000000 ) ) ;
#40987 = LINE ( 'NONE', #106204, #28559 ) ;
#40988 = LINE ( 'NONE', #21380, #18193 ) ;
#40989 = EDGE_CURVE ( 'NONE', #45628, #123770, #90215, .T. ) ;
#40990 = ORIENTED_EDGE ( 'NONE', *, *, #23006, .T. ) ;
#40991 = LINE ( 'NONE', #139624, #122963 ) ;
#40992 = VERTEX_POINT ( 'NONE', #66351 ) ;
#40993 = AXIS2_PLACEMENT_3D ( 'NONE', #48636, #92837, #7228 ) ;
#40994 = LINE ( 'NONE', #85191, #19347 ) ;
#40995 = CARTESIAN_POINT ( 'NONE',  ( 29.14540314143522437, -2.126176841940958351, -7.934999999999989839 ) ) ;
#40996 = VERTEX_POINT ( 'NONE', #24257 ) ;
#40997 = DIRECTION ( 'NONE',  ( -0.6830127018922181881, 0.6830127018922202975, -0.2588190451025214056 ) ) ;
#40998 = CARTESIAN_POINT ( 'NONE',  ( -57.18398860626899705, 28.73617430169827358, 5.000000000000000000 ) ) ;
#40999 = VERTEX_POINT ( 'NONE', #68504 ) ;
#41000 = ORIENTED_EDGE ( 'NONE', *, *, #86875, .T. ) ;
#41001 = LINE ( 'NONE', #17109, #2343 ) ;
#41002 = CARTESIAN_POINT ( 'NONE',  ( 11.53839644629422345, -9.740707523384180888, 17.74957260769613399 ) ) ;
#41003 = CARTESIAN_POINT ( 'NONE',  ( -32.99451991528749062, 28.92564299267960948, 4.000000000000000000 ) ) ;
#41004 = CARTESIAN_POINT ( 'NONE',  ( -34.92500000000001137, 21.72500000000000142, 5.000000000000000000 ) ) ;
#41005 =( NAMED_UNIT ( * ) PLANE_ANGLE_UNIT ( ) SI_UNIT ( $, .RADIAN. ) );
#41006 = CARTESIAN_POINT ( 'NONE',  ( 65.24543019189810877, -5.291415217122919401, -3.055000000000000604 ) ) ;
#41007 = FACE_OUTER_BOUND ( 'NONE', #67992, .T. ) ;
#41008 = DIRECTION ( 'NONE',  ( 1.000000000000000000, -0.000000000000000000, 0.000000000000000000 ) ) ;
#41009 = CARTESIAN_POINT ( 'NONE',  ( -2.994519915287485734, 28.92564299267940342, 4.000000000000000000 ) ) ;
#41010 = LINE ( 'NONE', #30121, #4971 ) ;
#41011 = VERTEX_POINT ( 'NONE', #90960 ) ;
#41012 = CARTESIAN_POINT ( 'NONE',  ( -25.49999999999981171, 4.087461875839202285, 4.000000000000000000 ) ) ;
#41013 = CIRCLE ( 'NONE', #34101, 2.500000000000000444 ) ;
#41014 = ORIENTED_EDGE ( 'NONE', *, *, #75742, .F. ) ;
#41015 = CARTESIAN_POINT ( 'NONE',  ( -13.17183060077637968, 9.759292476615618384, 4.000000000000000000 ) ) ;
#41016 = CARTESIAN_POINT ( 'NONE',  ( 51.18398860626899705, 28.73617430169823095, 5.000000000000000000 ) ) ;
#41017 = VERTEX_POINT ( 'NONE', #135190 ) ;
#41018 = CARTESIAN_POINT ( 'NONE',  ( -21.87485380690753090, -14.24070752338414181, 9.401115078912708256 ) ) ;
#41020 = ORIENTED_EDGE ( 'NONE', *, *, #25978, .T. ) ;
#41019 = LINE ( 'NONE', #72273, #111283 ) ;
#41021 = CARTESIAN_POINT ( 'NONE',  ( 1.499999999999984013, -7.912538124160671593, 4.000000000000000000 ) ) ;
#41022 = DIRECTION ( 'NONE',  ( 0.7071067811865486830, -0.7071067811865464625, -0.000000000000000000 ) ) ;
#41023 = ADVANCED_FACE ( 'NONE', ( #13351 ), #35880, .F. ) ;
#41024 = EDGE_CURVE ( 'NONE', #130004, #70502, #121414, .T. ) ;
#41025 = ORIENTED_EDGE ( 'NONE', *, *, #38288, .F. ) ;
#41026 = VERTEX_POINT ( 'NONE', #110519 ) ;
#41027 = CARTESIAN_POINT ( 'NONE',  ( 33.29974487139158867, -27.71228299555229313, 4.000000000000000000 ) ) ;
#41028 = DIRECTION ( 'NONE',  ( -1.000000000000000000, -1.224606353822377258E-16, -0.000000000000000000 ) ) ;
#41029 = EDGE_CURVE ( 'NONE', #128763, #91210, #51067, .T. ) ;
#41031 = ADVANCED_FACE ( 'NONE', ( #104659 ), #93083, .T. ) ;
#41030 = CARTESIAN_POINT ( 'NONE',  ( 92.53752705046289861, -9.735942053221456900E-16, 7.949999999999998401 ) ) ;
#41032 = CARTESIAN_POINT ( 'NONE',  ( 24.41159235450331977, 3.061616997868380183E-16, -2.500000000000001332 ) ) ;
#41033 = LINE ( 'NONE', #10522, #80830 ) ;
#41035 = EDGE_CURVE ( 'NONE', #125641, #99168, #113384, .T. ) ;
#41034 = VERTEX_POINT ( 'NONE', #114797 ) ;
#41036 = AXIS2_PLACEMENT_3D ( 'NONE', #47398, #92250, #136481 ) ;
#41037 = CARTESIAN_POINT ( 'NONE',  ( 19.17183060077633172, -20.24070752338407786, 4.000000000000000000 ) ) ;
#41038 = ADVANCED_FACE ( 'NONE', ( #47487 ), #15477, .T. ) ;
#41039 = CARTESIAN_POINT ( 'NONE',  ( 0.000000000000000000, 0.000000000000000000, 5.000000000000000000 ) ) ;
#41040 = CARTESIAN_POINT ( 'NONE',  ( -34.42500000000001137, 1.541399257802000822, 5.000000000000000000 ) ) ;
#41041 = CARTESIAN_POINT ( 'NONE',  ( -23.99999999999983302, 12.83542986846995149, -1.025386466790314310 ) ) ;
#41042 = EDGE_CURVE ( 'NONE', #55488, #97116, #81523, .T. ) ;
#41043 = ORIENTED_EDGE ( 'NONE', *, *, #85819, .T. ) ;
#41044 = LINE ( 'NONE', #118594, #32890 ) ;
#41046 = ORIENTED_EDGE ( 'NONE', *, *, #83690, .F. ) ;
#41045 = ADVANCED_FACE ( 'NONE', ( #16949 ), #92338, .F. ) ;
#41047 = CARTESIAN_POINT ( 'NONE',  ( 73.50043019189811844, -3.055000000000002380, 5.291415217122920289 ) ) ;
#41048 = FACE_OUTER_BOUND ( 'NONE', #112889, .T. ) ;
#41049 = DIRECTION ( 'NONE',  ( -0.000000000000000000, 0.000000000000000000, 1.000000000000000000 ) ) ;
#41050 = ORIENTED_EDGE ( 'NONE', *, *, #37149, .F. ) ;
#41051 = CARTESIAN_POINT ( 'NONE',  ( 22.49999999999985434, -11.56887692260769285, 4.000000000000000000 ) ) ;
#41052 = EDGE_CURVE ( 'NONE', #48427, #50477, #1880, .T. ) ;
#41053 = PLANE ( 'NONE',  #97416 ) ;
#41054 = CARTESIAN_POINT ( 'NONE',  ( 118.2041937171295700, -6.884901960086285300, -3.975000000000000089 ) ) ;
#41056 = VERTEX_POINT ( 'NONE', #25670 ) ;
#41055 = CARTESIAN_POINT ( 'NONE',  ( 5.816011393731002066, 28.73617430169783304, 5.000000000000000000 ) ) ;
#41057 = CARTESIAN_POINT ( 'NONE',  ( 21.18398860626899349, 28.73617430169802134, 5.000000000000000000 ) ) ;
#41058 = DIRECTION ( 'NONE',  ( -0.6830127018922180770, -0.6830127018922204085, -0.2588190451025213501 ) ) ;
#41059 = CARTESIAN_POINT ( 'NONE',  ( 27.70612307739175861, 22.22500000000000142, 4.000000000000000000 ) ) ;
#41060 = EDGE_CURVE ( 'NONE', #47726, #59437, #48875, .T. ) ;
#41061 = CARTESIAN_POINT ( 'NONE',  ( 59.91666666666665719, -6.884901960086287076, -3.975000000000000977 ) ) ;
#41062 = VECTOR ( 'NONE', #95999, 1000.000000000000000 ) ;
#41063 = ORIENTED_EDGE ( 'NONE', *, *, #55929, .F. ) ;
#41064 = ORIENTED_EDGE ( 'NONE', *, *, #79559, .F. ) ;
#41065 = AXIS2_PLACEMENT_3D ( 'NONE', #14672, #37130, #58953 ) ;
#41066 = CARTESIAN_POINT ( 'NONE',  ( 77.14626352523143282, -4.472830434245840259, 4.472830434245839371 ) ) ;
#41067 = VERTEX_POINT ( 'NONE', #38009 ) ;
#41068 = DIRECTION ( 'NONE',  ( -1.000000000000000000, -0.000000000000000000, -0.000000000000000000 ) ) ;
#41069 = CARTESIAN_POINT ( 'NONE',  ( 25.19159235450331735, 9.902892378096218942E-16, 0.000000000000000000 ) ) ;
#41071 = VECTOR ( 'NONE', #14316, 1000.000000000000227 ) ;
#41070 = CARTESIAN_POINT ( 'NONE',  ( -6.707106781186491062, 8.259292476615636147, 5.000000000000000000 ) ) ;
#41072 = CARTESIAN_POINT ( 'NONE',  ( 21.48921356237309155, -27.52281430457070499, 5.000000000000000000 ) ) ;
#41073 = VERTEX_POINT ( 'NONE', #24943 ) ;
#41074 = PLANE ( 'NONE',  #139432 ) ;
#41075 = SURFACE_SIDE_STYLE ('',( #140385 ) ) ;
#41076 = ORIENTED_EDGE ( 'NONE', *, *, #89242, .F. ) ;
#41077 = CARTESIAN_POINT ( 'NONE',  ( -24.89279686680829329, 1.949462372756119333, 4.672399651904018292 ) ) ;
#41078 = ADVANCED_FACE ( 'NONE', ( #136566 ), #102548, .T. ) ;
#41079 = PLANE ( 'NONE',  #59505 ) ;
#41080 = DIRECTION ( 'NONE',  ( 0.000000000000000000, 0.000000000000000000, 1.000000000000000000 ) ) ;
#41081 = ADVANCED_FACE ( 'NONE', ( #103227 ), #82234, .F. ) ;
#41082 = EDGE_LOOP ( 'NONE', ( #36749, #96949 ) ) ;
#41083 = ORIENTED_EDGE ( 'NONE', *, *, #50672, .T. ) ;
#41084 = FACE_OUTER_BOUND ( 'NONE', #31150, .T. ) ;
#41085 = DIRECTION ( 'NONE',  ( -0.000000000000000000, 0.3543493200069153248, 0.9351131265310292928 ) ) ;
#41086 = DIRECTION ( 'NONE',  ( -0.000000000000000000, -0.3543493200069152693, 0.9351131265310292928 ) ) ;
#41087 = FILL_AREA_STYLE ('',( #129507 ) ) ;
#41088 = VECTOR ( 'NONE', #92434, 999.9999999999998863 ) ;
#41089 = DIRECTION ( 'NONE',  ( 0.7071067811865486830, -0.7071067811865464625, -0.000000000000000000 ) ) ;
#41090 = EDGE_CURVE ( 'NONE', #111985, #109319, #16753, .T. ) ;
#41091 = LINE ( 'NONE', #85289, #102152 ) ;
#41092 = SURFACE_STYLE_USAGE ( .BOTH. , #139728 ) ;
#41093 = ORIENTED_EDGE ( 'NONE', *, *, #138994, .F. ) ;
#41094 =( GEOMETRIC_REPRESENTATION_CONTEXT ( 3 ) GLOBAL_UNCERTAINTY_ASSIGNED_CONTEXT ( ( #47827 ) ) GLOBAL_UNIT_ASSIGNED_CONTEXT ( ( #12277, #113011, #132682 ) ) REPRESENTATION_CONTEXT ( 'NONE', 'WORKASPACE' ) );
#41095 = VERTEX_POINT ( 'NONE', #30697 ) ;
#41096 = EDGE_LOOP ( 'NONE', ( #122406, #53713, #6296, #13693 ) ) ;
#41097 = EDGE_CURVE ( 'NONE', #142771, #103184, #129990, .T. ) ;
#41098 = ORIENTED_EDGE ( 'NONE', *, *, #34369, .T. ) ;
#41099 = VECTOR ( 'NONE', #33093, 1000.000000000000000 ) ;
#41100 = CARTESIAN_POINT ( 'NONE',  ( 181.0498351327038620, -48.63026969829178370, 38.45492102172562454 ) ) ;
#41101 =( BOUNDED_CURVE ( )  B_SPLINE_CURVE ( 3, ( #135360, #34598, #45504, #36045 ),
 .UNSPECIFIED., .F., .F. ) 
 B_SPLINE_CURVE_WITH_KNOTS ( ( 4, 4 ),
 ( 5.143245962375971203, 6.645403452391246191 ),
 .UNSPECIFIED. ) 
 CURVE ( )  GEOMETRIC_REPRESENTATION_ITEM ( )  RATIONAL_B_SPLINE_CURVE ( ( 1.000000000000000000, 0.8206354192515254997, 0.8206354192515254997, 1.000000000000000000 ) ) 
 REPRESENTATION_ITEM ( '' )  );
#41102 = DIRECTION ( 'NONE',  ( -1.000000000000000000, 0.000000000000000000, 0.000000000000000000 ) ) ;
#41103 = FACE_OUTER_BOUND ( 'NONE', #51713, .T. ) ;
#41104 = ORIENTED_EDGE ( 'NONE', *, *, #139354, .T. ) ;
#41105 = FACE_OUTER_BOUND ( 'NONE', #99305, .T. ) ;
#41106 = CARTESIAN_POINT ( 'NONE',  ( -23.99999999999982592, -6.412538124160692909, 4.000000000000000000 ) ) ;
#41107 = EDGE_CURVE ( 'NONE', #30424, #135054, #84376, .T. ) ;
#41108 = FACE_OUTER_BOUND ( 'NONE', #107747, .T. ) ;
#41109 = LINE ( 'NONE', #104932, #73951 ) ;
#41110 = CARTESIAN_POINT ( 'NONE',  ( -2.700255128608413990, -27.71228299555204089, 4.000000000000000000 ) ) ;
#41111 = ORIENTED_EDGE ( 'NONE', *, *, #77957, .F. ) ;
#41112 = DIRECTION ( 'NONE',  ( -0.000000000000000000, 0.3543493200069153248, 0.9351131265310292928 ) ) ;
#41113 = DIRECTION ( 'NONE',  ( 0.6830127018922181881, 0.6830127018922202975, -0.2588190451025214056 ) ) ;
#41114 = ORIENTED_EDGE ( 'NONE', *, *, #55260, .T. ) ;
#41116 = EDGE_CURVE ( 'NONE', #31939, #69693, #53117, .T. ) ;
#41115 = DIRECTION ( 'NONE',  ( -1.000000000000000000, 0.000000000000000000, 0.000000000000000000 ) ) ;
#41117 = ORIENTED_EDGE ( 'NONE', *, *, #12785, .F. ) ;
#41118 = EDGE_CURVE ( 'NONE', #71286, #135278, #6725, .T. ) ;
#41119 = LINE ( 'NONE', #139750, #99178 ) ;
#41120 = ORIENTED_EDGE ( 'NONE', *, *, #35547, .F. ) ;
#41121 = CARTESIAN_POINT ( 'NONE',  ( 62.27126352523142572, 4.472830434245838482, 4.472830434245842035 ) ) ;
#41122 = VERTEX_POINT ( 'NONE', #64025 ) ;
#41123 = ORIENTED_EDGE ( 'NONE', *, *, #19505, .F. ) ;
#41124 = EDGE_CURVE ( 'NONE', #51392, #13028, #8854, .T. ) ;
#41125 = DIRECTION ( 'NONE',  ( 0.7071067811865487940, 0.7071067811865463515, -0.000000000000000000 ) ) ;
#41126 = VECTOR ( 'NONE', #15219, 1000.000000000000000 ) ;
#41127 = CARTESIAN_POINT ( 'NONE',  ( 95.95876352523144703, 0.000000000000000000, -6.110000000000001208 ) ) ;
#41128 = DIRECTION ( 'NONE',  ( 0.7071067811865487940, 0.7071067811865463515, -0.000000000000000000 ) ) ;
#41129 = CARTESIAN_POINT ( 'NONE',  ( -34.92500000000001137, 12.00612307739180551, 4.000000000000000000 ) ) ;
#41130 = CARTESIAN_POINT ( 'NONE',  ( 15.06011071044010485, -9.740707523384184441, 10.89222023123377348 ) ) ;
#41131 = CARTESIAN_POINT ( 'NONE',  ( 11.99999999999992006, -13.44781430457068794, 5.000000000000000000 ) ) ;
#41132 = EDGE_CURVE ( 'NONE', #25784, #31384, #97320, .T. ) ;
#41133 = CARTESIAN_POINT ( 'NONE',  ( 5.999999999999967137, -1.447814304570820276, 5.000000000000000000 ) ) ;
#41134 = CARTESIAN_POINT ( 'NONE',  ( -2.999999999999975131, -2.904428200921311376, -6.989807076074934677 ) ) ;
#41135 = EDGE_LOOP ( 'NONE', ( #35672, #84672, #131329, #34697, #65340, #120451 ) ) ;
#41136 = VECTOR ( 'NONE', #69968, 1000.000000000000000 ) ;
#41137 = ADVANCED_FACE ( 'NONE', ( #63343 ), #51731, .F. ) ;
#41138 = DIRECTION ( 'NONE',  ( -0.7071067811865486830, 0.7071067811865464625, 0.000000000000000000 ) ) ;
#41139 = ORIENTED_EDGE ( 'NONE', *, *, #43373, .T. ) ;
#41140 = VERTEX_POINT ( 'NONE', #53885 ) ;
#41141 = EDGE_LOOP ( 'NONE', ( #135453, #91871, #68673 ) ) ;
#41142 = ORIENTED_EDGE ( 'NONE', *, *, #139290, .T. ) ;
#41143 = PRESENTATION_LAYER_ASSIGNMENT (  '', '', ( #103629 ) ) ;
#41144 = CARTESIAN_POINT ( 'NONE',  ( -12.20000000000000284, -39.92999999999999261, -39.50000000000000000 ) ) ;
#41145 = CARTESIAN_POINT ( 'NONE',  ( 5.994519915287488843, 28.92564299267942118, 4.000000000000000000 ) ) ;
#41146 = AXIS2_PLACEMENT_3D ( 'NONE', #110601, #42552, #75183 ) ;
#41147 = CYLINDRICAL_SURFACE ( 'NONE', #104222, 2.500000000000000000 ) ;
#41148 = EDGE_CURVE ( 'NONE', #7978, #65537, #141588, .T. ) ;
#41149 = VERTEX_POINT ( 'NONE', #85756 ) ;
#41150 = CARTESIAN_POINT ( 'NONE',  ( 0.000000000000000000, -47.62213595499959951, 36.92500000000000426 ) ) ;
#41151 = VERTEX_POINT ( 'NONE', #29238 ) ;
#41152 = CARTESIAN_POINT ( 'NONE',  ( 4.791236474768552966, -9.717572351234235426E-16, -7.934999999999990727 ) ) ;
#41153 = LINE ( 'NONE', #117961, #42400 ) ;
#41154 = FACE_OUTER_BOUND ( 'NONE', #7269, .T. ) ;
#41155 = FACE_OUTER_BOUND ( 'NONE', #10580, .T. ) ;
#41156 = EDGE_LOOP ( 'NONE', ( #98891, #80349, #5287, #41342 ) ) ;
#41157 = ORIENTED_EDGE ( 'NONE', *, *, #124615, .F. ) ;
#41158 = ORIENTED_EDGE ( 'NONE', *, *, #107384, .F. ) ;
#41159 = CARTESIAN_POINT ( 'NONE',  ( 5.380000000000000782, 9.521314400968980422E-16, 0.000000000000000000 ) ) ;
#41160 = CARTESIAN_POINT ( 'NONE',  ( -25.17694361456247876, -22.22500000000000142, 1.306097034074463314 ) ) ;
#41161 = DIRECTION ( 'NONE',  ( -0.000000000000000000, -1.000000000000000000, -0.000000000000000000 ) ) ;
#41162 = FACE_OUTER_BOUND ( 'NONE', #2515, .T. ) ;
#41163 = CARTESIAN_POINT ( 'NONE',  ( 1.179999999999999272, 10.00000000000000178, 6.750000000000000888 ) ) ;
#41164 = DIRECTION ( 'NONE',  ( -0.000000000000000000, 0.000000000000000000, 1.000000000000000000 ) ) ;
#41165 = CARTESIAN_POINT ( 'NONE',  ( -34.49999999999975131, -20.53675388469233809, 2.352720554255813390 ) ) ;
#41166 = CARTESIAN_POINT ( 'NONE',  ( 30.91709685856476497, 3.054999999999998828, 5.291415217122922066 ) ) ;
#41167 = FACE_OUTER_BOUND ( 'NONE', #26135, .T. ) ;
#41168 = DIRECTION ( 'NONE',  ( 0.000000000000000000, -1.000000000000000000, 0.000000000000000000 ) ) ;
#41169 = ORIENTED_EDGE ( 'NONE', *, *, #45934, .F. ) ;
#41170 = CARTESIAN_POINT ( 'NONE',  ( 111.7875270504628986, 0.000000000000000000, -7.949999999999998401 ) ) ;
#41171 = ADVANCED_FACE ( 'NONE', ( #117646 ), #42291, .F. ) ;
#41172 = FACE_OUTER_BOUND ( 'NONE', #113495, .T. ) ;
#41173 = ORIENTED_EDGE ( 'NONE', *, *, #49133, .F. ) ;
#41174 = CARTESIAN_POINT ( 'NONE',  ( 7.499999999999947597, -13.91253812416061386, 4.000000000000000000 ) ) ;
#41176 = ORIENTED_EDGE ( 'NONE', *, *, #68274, .T. ) ;
#41175 = CARTESIAN_POINT ( 'NONE',  ( 53.94409967708044462, -48.16486758952232350, -37.61253110040615866 ) ) ;
#41177 = CARTESIAN_POINT ( 'NONE',  ( 0.4892135623730947680, -27.52281430457055578, 5.000000000000000000 ) ) ;
#41179 = AXIS2_PLACEMENT_3D ( 'NONE', #71439, #60593, #64660 ) ;
#41178 = FACE_OUTER_BOUND ( 'NONE', #506, .T. ) ;
#41180 = VERTEX_POINT ( 'NONE', #83663 ) ;
#41181 = DIRECTION ( 'NONE',  ( -0.6830127018922181881, 0.6830127018922202975, -0.2588190451025214056 ) ) ;
#41182 = VERTEX_POINT ( 'NONE', #51010 ) ;
#41183 = CARTESIAN_POINT ( 'NONE',  ( -12.49289321881345494, -22.06289321881344634, -40.00000000000000000 ) ) ;
#41185 = EDGE_CURVE ( 'NONE', #126336, #66418, #129257, .T. ) ;
#41184 = CARTESIAN_POINT ( 'NONE',  ( 119.8083603837962272, 7.949999999999997513, 2.130196079827431088 ) ) ;
#41186 = DIRECTION ( 'NONE',  ( -0.000000000000000000, 0.3543493200069153248, 0.9351131265310292928 ) ) ;
#41187 = DIRECTION ( 'NONE',  ( -0.000000000000000000, 0.3543493200069153248, 0.9351131265310292928 ) ) ;
#41188 = ADVANCED_FACE ( 'NONE', ( #62603 ), #106788, .T. ) ;
#41189 = DIRECTION ( 'NONE',  ( -0.6830127018922181881, 0.6830127018922202975, -0.2588190451025214056 ) ) ;
#41190 = EDGE_CURVE ( 'NONE', #62041, #62992, #17632, .T. ) ;
#41191 = CARTESIAN_POINT ( 'NONE',  ( 26.99999999999980815, -0.8619312979531723595, -5.102805207349763172 ) ) ;
#41192 = CARTESIAN_POINT ( 'NONE',  ( 0.2916666666666667407, -3.047499999999994547, 5.278424836066145431 ) ) ;
#41193 = CARTESIAN_POINT ( 'NONE',  ( 18.35373647476854941, -5.808823158059035485, -5.808823158059033709 ) ) ;
#41194 = DIRECTION ( 'NONE',  ( -0.7071067811865486830, -0.7071067811865464625, 0.000000000000000000 ) ) ;
#41196 = EDGE_CURVE ( 'NONE', #58969, #63466, #61903, .T. ) ;
#41195 = CARTESIAN_POINT ( 'NONE',  ( 8.207106781186489286, -17.24070752338410273, 5.000000000000000000 ) ) ;
#41197 = ORIENTED_EDGE ( 'NONE', *, *, #131826, .T. ) ;
#41198 = VERTEX_POINT ( 'NONE', #52413 ) ;
#41199 = CYLINDRICAL_SURFACE ( 'NONE', #65174, 3.000000000000000000 ) ;
#41200 = ORIENTED_EDGE ( 'NONE', *, *, #76972, .T. ) ;
#41201 = PRODUCT_DEFINITION_SHAPE ( 'NONE', 'NONE',  #143568 ) ;
#41202 = ADVANCED_FACE ( 'NONE', ( #40841 ), #107514, .T. ) ;
#41203 = LINE ( 'NONE', #20872, #75798 ) ;
#41204 = LINE ( 'NONE', #130383, #115622 ) ;
#41205 = CARTESIAN_POINT ( 'NONE',  ( -7.828169399223474656, -14.24070752338414181, 4.000000000000000000 ) ) ;
#41206 = CARTESIAN_POINT ( 'NONE',  ( 34.49999999999976552, 21.05432934483073026, 4.994342998332161443 ) ) ;
#41207 = ORIENTED_EDGE ( 'NONE', *, *, #110362, .T. ) ;
#41208 = LINE ( 'NONE', #107179, #51041 ) ;
#41209 = EDGE_CURVE ( 'NONE', #46033, #142592, #77067, .T. ) ;
#41211 = VECTOR ( 'NONE', #76625, 1000.000000000000000 ) ;
#41210 = CARTESIAN_POINT ( 'NONE',  ( 5.380000000000000782, 2.055000000000001492, 2.516649172247811554E-16 ) ) ;
#41212 = CARTESIAN_POINT ( 'NONE',  ( -35.99451991528749772, 28.92564299267963079, 4.000000000000000000 ) ) ;
#41213 = EDGE_CURVE ( 'NONE', #16399, #60444, #56760, .T. ) ;
#41214 = CARTESIAN_POINT ( 'NONE',  ( 0.8183591370940056509, -52.14999999999999147, 41.64499999999997470 ) ) ;
#41216 = EDGE_LOOP ( 'NONE', ( #43434, #124541, #49751, #41922 ) ) ;
#41215 = FACE_OUTER_BOUND ( 'NONE', #95258, .T. ) ;
#41217 = CARTESIAN_POINT ( 'NONE',  ( 40.08333333333332860, 6.884901960086290629, -3.974999999999994316 ) ) ;
#41218 = DIRECTION ( 'NONE',  ( -0.000000000000000000, -0.3543493200069152693, 0.9351131265310292928 ) ) ;
#41219 = DIRECTION ( 'NONE',  ( 0.3543493200069162685, -0.000000000000000000, -0.9351131265310288487 ) ) ;
#41220 = DIRECTION ( 'NONE',  ( -0.000000000000000000, 0.000000000000000000, 1.000000000000000000 ) ) ;
#41221 = EDGE_CURVE ( 'NONE', #91203, #78911, #55298, .T. ) ;
#41222 = LINE ( 'NONE', #30353, #58510 ) ;
#41223 = ORIENTED_EDGE ( 'NONE', *, *, #80035, .T. ) ;
#41224 = VERTEX_POINT ( 'NONE', #1576 ) ;
#41225 = ORIENTED_EDGE ( 'NONE', *, *, #115191, .F. ) ;
#41226 = CARTESIAN_POINT ( 'NONE',  ( 103.5420968585647756, 5.291415217122923842, -3.054999999999996163 ) ) ;
#41227 = COLOUR_RGB ( '', 0.40784314, 0.44705882, 0.49803922) ;
#41228 = ORIENTED_EDGE ( 'NONE', *, *, #71155, .F. ) ;
#41229 = CARTESIAN_POINT ( 'NONE',  ( 125.9828883629226510, -46.44928942427174690, 35.85226645762418229 ) ) ;
#41230 = LINE ( 'NONE', #7876, #73256 ) ;
#41231 = ORIENTED_EDGE ( 'NONE', *, *, #103860, .T. ) ;
#41232 = CARTESIAN_POINT ( 'NONE',  ( -1.320800000000306618, -4.493284886149243553E-13, 3.775643966265820328 ) ) ;
#41233 = DIRECTION ( 'NONE',  ( 0.6830127018922180770, -0.6830127018922204085, -0.2588190451025213501 ) ) ;
#41234 = CARTESIAN_POINT ( 'NONE',  ( 94.26626352523143737, 4.472830434245839371, -4.472830434245838482 ) ) ;
#41235 = ORIENTED_EDGE ( 'NONE', *, *, #123722, .F. ) ;
#41236 = DIRECTION ( 'NONE',  ( 0.7071067811865487940, 0.7071067811865463515, 0.000000000000000000 ) ) ;
#41238 = EDGE_CURVE ( 'NONE', #19313, #26139, #134279, .T. ) ;
#41237 = CARTESIAN_POINT ( 'NONE',  ( 30.27825451568554271, 8.259292476615634371, 11.78515199841157468 ) ) ;
#41239 = CARTESIAN_POINT ( 'NONE',  ( 26.75159235450331963, 2.500000000000001776, 0.000000000000000000 ) ) ;
#41240 = DIRECTION ( 'NONE',  ( 0.7071067811865486830, -0.7071067811865464625, -0.000000000000000000 ) ) ;
#41241 = ORIENTED_EDGE ( 'NONE', *, *, #15823, .F. ) ;
#41242 = EDGE_LOOP ( 'NONE', ( #99543, #54554, #110117, #129007 ) ) ;
#41243 = VECTOR ( 'NONE', #61300, 1000.000000000000000 ) ;
#41244 = ORIENTED_EDGE ( 'NONE', *, *, #16502, .F. ) ;
#41245 = DIRECTION ( 'NONE',  ( -0.000000000000000000, -0.3543493200069152693, 0.9351131265310292928 ) ) ;
#41246 = CARTESIAN_POINT ( 'NONE',  ( -3.489213562373097322, -27.52281430457057709, 5.000000000000000000 ) ) ;
#41247 = CARTESIAN_POINT ( 'NONE',  ( 6.192069808101886785, -7.934999999999990727, -2.126176841940955242 ) ) ;
#41248 = AXIS2_PLACEMENT_3D ( 'NONE', #141129, #56861, #133669 ) ;
#41249 = CIRCLE ( 'NONE', #122260, 2.500000000000000888 ) ;
#41250 = CARTESIAN_POINT ( 'NONE',  ( 7.553349423367771820, 2.259292476615690770, 14.86850063742352646 ) ) ;
#41251 = EDGE_CURVE ( 'NONE', #56450, #37411, #66881, .T. ) ;
#41252 = VERTEX_POINT ( 'NONE', #13175 ) ;
#41253 = ORIENTED_EDGE ( 'NONE', *, *, #104747, .T. ) ;
#41254 = DIRECTION ( 'NONE',  ( -0.6830127018922180770, -0.6830127018922204085, -0.2588190451025213501 ) ) ;
#41256 = VERTEX_POINT ( 'NONE', #87198 ) ;
#41255 = EDGE_CURVE ( 'NONE', #3251, #130838, #76330, .T. ) ;
#41257 = VERTEX_POINT ( 'NONE', #10332 ) ;
#41258 = CARTESIAN_POINT ( 'NONE',  ( 18.66666666666666785, -5.278424836066145431, -3.047499999999993658 ) ) ;
#41259 = LINE ( 'NONE', #7906, #17060 ) ;
#41260 = ORIENTED_EDGE ( 'NONE', *, *, #52527, .F. ) ;
#41261 = DIRECTION ( 'NONE',  ( 0.7071067811865487940, 0.7071067811865463515, -0.000000000000000000 ) ) ;
#41262 = CARTESIAN_POINT ( 'NONE',  ( -25.39999999999996305, 3.061616997868383141E-16, -2.500000000000000000 ) ) ;
#41263 = ADVANCED_FACE ( 'NONE', ( #872 ), #110347, .F. ) ;
#41264 = CARTESIAN_POINT ( 'NONE',  ( 12.08840764549667668, 9.139736423841732040E-16, 0.000000000000000000 ) ) ;
#41265 = DIRECTION ( 'NONE',  ( 0.6830127018922180770, -0.6830127018922204085, -0.2588190451025213501 ) ) ;
#41266 = VECTOR ( 'NONE', #68180, 1000.000000000000000 ) ;
#41267 = CARTESIAN_POINT ( 'NONE',  ( 26.48831394071551415, 6.759292476615649470, 16.35960578974463431 ) ) ;
#41268 = EDGE_LOOP ( 'NONE', ( #69084, #65418, #67895, #72279 ) ) ;
#41269 = VECTOR ( 'NONE', #27428, 999.9999999999998863 ) ;
#41270 = CARTESIAN_POINT ( 'NONE',  ( 34.92499999999998295, 7.711264365774191276, -0.4997969837368084201 ) ) ;
#41271 = AXIS2_PLACEMENT_3D ( 'NONE', #68110, #112291, #132642 ) ;
#41272 = DIRECTION ( 'NONE',  ( -0.6830127018922180770, 0.6830127018922202975, -0.2588190451025213501 ) ) ;
#41273 = ORIENTED_EDGE ( 'NONE', *, *, #106620, .T. ) ;
#41274 = CARTESIAN_POINT ( 'NONE',  ( 25.40000000000000568, 0.1175040200531159013, -7.944505609933036006 ) ) ;
#41276 = EDGE_CURVE ( 'NONE', #23205, #66308, #42997, .T. ) ;
#41275 = CARTESIAN_POINT ( 'NONE',  ( 24.87999999999999901, 9.521314400968980422E-16, 0.000000000000000000 ) ) ;
#41277 = LINE ( 'NONE', #64470, #93174 ) ;
#41278 = ORIENTED_EDGE ( 'NONE', *, *, #73378, .F. ) ;
#41279 = CARTESIAN_POINT ( 'NONE',  ( 20.20710678118640047, 9.759292476615618384, 5.000000000000000000 ) ) ;
#41280 = ORIENTED_EDGE ( 'NONE', *, *, #123665, .T. ) ;
#41281 = ORIENTED_EDGE ( 'NONE', *, *, #32972, .F. ) ;
#41282 =( BOUNDED_CURVE ( )  B_SPLINE_CURVE ( 2, ( #6451, #20209, #65921, #64455, #33304, #107923, #110086, #43424, #19520, #31134, #44146, #75351, #142733 ),
 .UNSPECIFIED., .F., .T. ) 
 B_SPLINE_CURVE_WITH_KNOTS ( ( 3, 2, 2, 2, 2, 2, 3 ),
 ( 0.6666666666666666297, 0.6694444444444443976, 0.6722222222222222765, 0.6750000000000000444, 0.6777777777777779233, 0.6805555555555556912, 0.6833333333333334592 ),
 .UNSPECIFIED. ) 
 CURVE ( )  GEOMETRIC_REPRESENTATION_ITEM ( )  RATIONAL_B_SPLINE_CURVE ( ( 1.000000000000000000, 0.9659258262890683122, 1.000000000000000000, 0.9659258262890683122, 1.000000000000000000, 0.9659258262890683122, 1.000000000000000000, 0.9659258262890683122, 1.000000000000000000, 0.9659258262890683122, 1.000000000000000000, 0.9659258262890669799, 1.000000000000001332 ) ) 
 REPRESENTATION_ITEM ( '' )  );
#41283 = ORIENTED_EDGE ( 'NONE', *, *, #102660, .T. ) ;
#41284 = CARTESIAN_POINT ( 'NONE',  ( 28.64126352523144092, 4.472830434245835818, 4.472830434245840259 ) ) ;
#41285 = PLANE ( 'NONE',  #108512 ) ;
#41286 = CARTESIAN_POINT ( 'NONE',  ( -31.22850677138645636, 20.25929247661551003, 7.808871592221697355 ) ) ;
#41287 = CARTESIAN_POINT ( 'NONE',  ( -34.45011844616454511, -2.997695858406015379, 5.000000000000000888 ) ) ;
#41288 = DIRECTION ( 'NONE',  ( -0.3543493200069162685, -0.000000000000000000, -0.9351131265310288487 ) ) ;
#41289 = LINE ( 'NONE', #17400, #8849 ) ;
#41291 = PLANE ( 'NONE',  #137550 ) ;
#41290 = CARTESIAN_POINT ( 'NONE',  ( 33.48921356237309510, -27.52281430457078670, 5.000000000000000000 ) ) ;
#41292 = AXIS2_PLACEMENT_3D ( 'NONE', #110807, #99971, #89795 ) ;
#41293 = DIRECTION ( 'NONE',  ( -0.000000000000000000, -0.3543493200069152693, 0.9351131265310292928 ) ) ;
#41294 = CARTESIAN_POINT ( 'NONE',  ( -26.99999999999980815, -8.151047557385094677, -8.977947279169736561 ) ) ;
#41295 = ADVANCED_FACE ( 'NONE', ( #88644 ), #90879, .T. ) ;
#41296 = CARTESIAN_POINT ( 'NONE',  ( 45.48921356237309510, -27.52281430457087197, 5.000000000000000000 ) ) ;
#41297 = DIRECTION ( 'NONE',  ( 0.7071067811865487940, 0.7071067811865463515, 0.000000000000000000 ) ) ;
#41298 = ORIENTED_EDGE ( 'NONE', *, *, #54480, .T. ) ;
#41299 = ORIENTED_EDGE ( 'NONE', *, *, #95204, .F. ) ;
#41300 = ORIENTED_EDGE ( 'NONE', *, *, #102929, .T. ) ;
#41301 = ORIENTED_EDGE ( 'NONE', *, *, #139423, .F. ) ;
#41302 = CARTESIAN_POINT ( 'NONE',  ( 54.18398860626899705, 28.73617430169825226, 5.000000000000000000 ) ) ;
#41303 = VERTEX_POINT ( 'NONE', #104919 ) ;
#41304 = ORIENTED_EDGE ( 'NONE', *, *, #118506, .F. ) ;
#41305 = DIRECTION ( 'NONE',  ( -0.6830127018922180770, -0.6830127018922204085, -0.2588190451025213501 ) ) ;
#41306 = EDGE_CURVE ( 'NONE', #45356, #11807, #104173, .T. ) ;
#41307 = ADVANCED_FACE ( 'NONE', ( #114370 ), #60010, .F. ) ;
#41308 = CARTESIAN_POINT ( 'NONE',  ( 0.000000000000000000, 0.000000000000000000, 5.000000000000000000 ) ) ;
#41309 = VERTEX_POINT ( 'NONE', #115046 ) ;
#41310 = CARTESIAN_POINT ( 'NONE',  ( 33.79289321881321939, -17.24070752338410628, 5.000000000000000000 ) ) ;
#41311 = ORIENTED_EDGE ( 'NONE', *, *, #25164, .T. ) ;
#41312 = CARTESIAN_POINT ( 'NONE',  ( 19.10840764549667270, 9.139736423841732040E-16, 0.000000000000000000 ) ) ;
#41313 = CARTESIAN_POINT ( 'NONE',  ( 0.000000000000000000, 0.000000000000000000, 5.000000000000000000 ) ) ;
#41314 = CARTESIAN_POINT ( 'NONE',  ( 13.19206980810188412, -7.934999999999991616, -2.126176841940955242 ) ) ;
#41315 = ORIENTED_EDGE ( 'NONE', *, *, #143287, .F. ) ;
#41316 = CARTESIAN_POINT ( 'NONE',  ( 92.95376352523145158, -6.109999999999999432, -3.741295971395163529E-16 ) ) ;
#41317 = FILL_AREA_STYLE_COLOUR ( '', #131604 ) ;
#41318 = DIRECTION ( 'NONE',  ( 0.7071067811865486830, -0.7071067811865464625, -0.000000000000000000 ) ) ;
#41319 = CARTESIAN_POINT ( 'NONE',  ( -51.48921356237309510, -27.52281430457091460, 5.000000000000000000 ) ) ;
#41320 = ORIENTED_EDGE ( 'NONE', *, *, #103177, .T. ) ;
#41321 = ORIENTED_EDGE ( 'NONE', *, *, #138688, .F. ) ;
#41322 = LINE ( 'NONE', #86984, #45049 ) ;
#41323 = ORIENTED_EDGE ( 'NONE', *, *, #74006, .T. ) ;
#41324 = LINE ( 'NONE', #85536, #41653 ) ;
#41325 = DIRECTION ( 'NONE',  ( -0.3543493200069162685, -0.000000000000000000, -0.9351131265310288487 ) ) ;
#41326 = DIRECTION ( 'NONE',  ( 0.7071067811865487940, -0.7071067811865463515, 0.000000000000000000 ) ) ;
#41327 = DIRECTION ( 'NONE',  ( 0.7071067811865487940, 0.7071067811865463515, 0.000000000000000000 ) ) ;
#41328 = EDGE_CURVE ( 'NONE', #133807, #42382, #27341, .T. ) ;
#41329 = ORIENTED_EDGE ( 'NONE', *, *, #41368, .T. ) ;
#41330 = DIRECTION ( 'NONE',  ( 0.6830127018922181881, 0.6830127018922202975, -0.2588190451025214056 ) ) ;
#41331 =( NAMED_UNIT ( * ) PLANE_ANGLE_UNIT ( ) SI_UNIT ( $, .RADIAN. ) );
#41332 = DIRECTION ( 'NONE',  ( -0.000000000000000000, -0.3543493200069152693, 0.9351131265310292928 ) ) ;
#41333 = ORIENTED_EDGE ( 'NONE', *, *, #2451, .F. ) ;
#41334 = LINE ( 'NONE', #64529, #23503 ) ;
#41335 = VECTOR ( 'NONE', #70907, 1000.000000000000000 ) ;
#41336 = CIRCLE ( 'NONE', #41441, 3.999999999999989786 ) ;
#41337 = CARTESIAN_POINT ( 'NONE',  ( 4.600000000000001421, -2.055000000000000160, 0.000000000000000000 ) ) ;
#41338 = ORIENTED_EDGE ( 'NONE', *, *, #64941, .F. ) ;
#41339 = AXIS2_PLACEMENT_3D ( 'NONE', #100481, #80875, #112071 ) ;
#41341 = ORIENTED_EDGE ( 'NONE', *, *, #8085, .F. ) ;
#41340 = CARTESIAN_POINT ( 'NONE',  ( 12.69999999999999574, -22.33999999999998565, 0.000000000000000000 ) ) ;
#41342 = ORIENTED_EDGE ( 'NONE', *, *, #14873, .F. ) ;
#41343 = AXIS2_PLACEMENT_3D ( 'NONE', #128883, #96935, #75254 ) ;
#41344 = DIRECTION ( 'NONE',  ( 0.7071067811865487940, 0.7071067811865463515, 0.000000000000000000 ) ) ;
#41345 = DIRECTION ( 'NONE',  ( -0.6830127018922180770, -0.6830127018922204085, -0.2588190451025213501 ) ) ;
#41346 = PRESENTATION_LAYER_ASSIGNMENT (  '', '', ( #29753 ) ) ;
#41347 = ORIENTED_EDGE ( 'NONE', *, *, #39190, .T. ) ;
#41348 = CARTESIAN_POINT ( 'NONE',  ( -25.82816939922335209, 12.75929247661558996, 4.000000000000000000 ) ) ;
#41349 = VECTOR ( 'NONE', #82921, 1000.000000000000000 ) ;
#41350 = CARTESIAN_POINT ( 'NONE',  ( -6.299744871391586898, -27.71228299555210484, 4.000000000000000000 ) ) ;
#41351 = EDGE_CURVE ( 'NONE', #122401, #6499, #5586, .T. ) ;
#41352 = DIRECTION ( 'NONE',  ( 0.7071067811865486830, -0.7071067811865464625, -0.000000000000000000 ) ) ;
#41353 = CARTESIAN_POINT ( 'NONE',  ( -23.20710678118638626, 12.75929247661559529, 5.000000000000000000 ) ) ;
#41354 = EDGE_CURVE ( 'NONE', #43329, #116175, #70894, .T. ) ;
#41355 = CARTESIAN_POINT ( 'NONE',  ( 0.1600000000000024458, -7.674647425206645224, -2.043597544210264072 ) ) ;
#41356 = LINE ( 'NONE', #63159, #137021 ) ;
#41357 = CARTESIAN_POINT ( 'NONE',  ( 47.95833333333332860, 3.974999999999997424, 6.884901960086288852 ) ) ;
#41358 = LINE ( 'NONE', #118186, #83615 ) ;
#41359 = DIRECTION ( 'NONE',  ( 0.7071067811865487940, 0.7071067811865463515, 0.000000000000000000 ) ) ;
#41361 = CIRCLE ( 'NONE', #1891, 2.055000000000001048 ) ;
#41360 = FACE_OUTER_BOUND ( 'NONE', #52598, .T. ) ;
#41362 = DIRECTION ( 'NONE',  ( 0.000000000000000000, -1.000000000000000000, 0.000000000000000000 ) ) ;
#41363 = COLOUR_RGB ( '', 0.72549020, 0.75294118, 0.79215686) ;
#41364 = CARTESIAN_POINT ( 'NONE',  ( -7.499999999999940492, -14.94781430457067906, 5.000000000000000000 ) ) ;
#41366 = EDGE_CURVE ( 'NONE', #9952, #85558, #81053, .T. ) ;
#41365 = SURFACE_SIDE_STYLE ('',( #83467 ) ) ;
#41368 = EDGE_CURVE ( 'NONE', #17308, #86287, #15041, .T. ) ;
#41367 = ORIENTED_EDGE ( 'NONE', *, *, #19686, .T. ) ;
#41369 = EDGE_LOOP ( 'NONE', ( #22495, #10116, #79319, #128449 ) ) ;
#41370 = VERTEX_POINT ( 'NONE', #25944 ) ;
#41371 = CARTESIAN_POINT ( 'NONE',  ( 113.2916666666666714, 3.975000000000003642, -6.884901960086285300 ) ) ;
#41372 = AXIS2_PLACEMENT_3D ( 'NONE', #108384, #88115, #132364 ) ;
#41373 = ORIENTED_EDGE ( 'NONE', *, *, #69555, .T. ) ;
#41374 = EDGE_LOOP ( 'NONE', ( #132619, #870, #67578, #22200 ) ) ;
#41375 = VERTEX_POINT ( 'NONE', #138272 ) ;
#41376 = CARTESIAN_POINT ( 'NONE',  ( 26.99999999999981171, -7.068876922607739921, 4.000000000000000000 ) ) ;
#41377 = DIRECTION ( 'NONE',  ( -0.000000000000000000, 0.000000000000000000, 1.000000000000000000 ) ) ;
#41378 = ORIENTED_EDGE ( 'NONE', *, *, #98797, .F. ) ;
#41379 = AXIS2_PLACEMENT_3D ( 'NONE', #100251, #56791, #173 ) ;
#41380 = DIRECTION ( 'NONE',  ( -0.000000000000000000, -0.3543493200069152693, 0.9351131265310292928 ) ) ;
#41381 = AXIS2_PLACEMENT_3D ( 'NONE', #129446, #107688, #83847 ) ;
#41382 = DIRECTION ( 'NONE',  ( -0.000000000000000000, 0.3543493200069153248, 0.9351131265310292928 ) ) ;
#41383 = VECTOR ( 'NONE', #32285, 1000.000000000000000 ) ;
#41384 = ADVANCED_FACE ( 'NONE', ( #116516 ), #83925, .F. ) ;
#41385 = CARTESIAN_POINT ( 'NONE',  ( -22.49999999999984013, -14.70932175296478839, -11.46312253303831774 ) ) ;
#41386 = LINE ( 'NONE', #9442, #51271 ) ;
#41387 = CARTESIAN_POINT ( 'NONE',  ( 103.1045968585647756, 1.637169565754164946, -6.109999999999999432 ) ) ;
#41388 = ORIENTED_EDGE ( 'NONE', *, *, #120840, .F. ) ;
#41389 = ADVANCED_FACE ( 'NONE', ( #93334 ), #39692, .F. ) ;
#41390 = CARTESIAN_POINT ( 'NONE',  ( 0.9194859777227279984, 12.57226318162868672, -26.75049658419982634 ) ) ;
#41391 = FILL_AREA_STYLE ('',( #42140 ) ) ;
#41392 = CARTESIAN_POINT ( 'NONE',  ( 24.34427593291135139, 5.931737808750704666, 4.000000000000000000 ) ) ;
#41393 = PLANE ( 'NONE',  #134901 ) ;
#41394 = LINE ( 'NONE', #85602, #135662 ) ;
#41395 =( GEOMETRIC_REPRESENTATION_CONTEXT ( 3 ) GLOBAL_UNCERTAINTY_ASSIGNED_CONTEXT ( ( #2664 ) ) GLOBAL_UNIT_ASSIGNED_CONTEXT ( ( #86950, #99966, #68791 ) ) REPRESENTATION_CONTEXT ( 'NONE', 'WORKASPACE' ) );
#41396 = CARTESIAN_POINT ( 'NONE',  ( 26.11162361894743000, 9.759292476615625489, 17.35367589129206678 ) ) ;
#41397 = EDGE_CURVE ( 'NONE', #140087, #55935, #82469, .T. ) ;
#41398 = DIRECTION ( 'NONE',  ( 0.6830127018922180770, -0.6830127018922204085, -0.2588190451025213501 ) ) ;
#41399 = ORIENTED_EDGE ( 'NONE', *, *, #57734, .F. ) ;
#41400 = ORIENTED_EDGE ( 'NONE', *, *, #43, .T. ) ;
#41401 = CARTESIAN_POINT ( 'NONE',  ( 127.0212635252314328, -4.472830434245839371, -4.472830434245840259 ) ) ;
#41402 = ORIENTED_EDGE ( 'NONE', *, *, #119297, .T. ) ;
#41403 = DIRECTION ( 'NONE',  ( 0.000000000000000000, 1.000000000000000000, 0.000000000000000000 ) ) ;
#41404 = CARTESIAN_POINT ( 'NONE',  ( -7.171830600776425868, 0.7592924766157104211, 4.000000000000000000 ) ) ;
#41405 = EDGE_CURVE ( 'NONE', #51683, #22300, #4113, .T. ) ;
#41406 = VECTOR ( 'NONE', #143148, 1000.000000000000000 ) ;
#41407 = DIRECTION ( 'NONE',  ( 0.000000000000000000, -1.000000000000000000, 0.000000000000000000 ) ) ;
#41408 = DIRECTION ( 'NONE',  ( -0.000000000000000000, -0.3543493200069152693, 0.9351131265310292928 ) ) ;
#41409 = CARTESIAN_POINT ( 'NONE',  ( -51.18398860626899705, 28.73617430169823095, 5.000000000000000000 ) ) ;
#41410 = CARTESIAN_POINT ( 'NONE',  ( 26.40000000000000568, -18.48000000000005372, -33.92499999999998295 ) ) ;
#41411 = CARTESIAN_POINT ( 'NONE',  ( 120.3704301918981230, -3.055000000000001492, 5.291415217122917625 ) ) ;
#41412 = B_SPLINE_CURVE_WITH_KNOTS ( 'NONE', 3,
 ( #113547, #36708, #57077, #92506, #36034, #103379, #134630, #24414, #136733, #78099, #78809, #70117, #13509, #22947, #14250, #58534, #112156, #102703, #12807, #67211, #57790, #111410, #101976, #2642, #1208, #80954, #133896, #45490, #89667, #34587, #46941, #123023, #23701, #125152 ),
 .UNSPECIFIED., .F., .F.,
 ( 4, 2, 2, 2, 2, 2, 2, 2, 2, 2, 2, 2, 2, 2, 2, 2, 4 ),
 ( 0.000000000000000000, 0.0008672315150799628312, 0.001734463030159925662, 0.002601694545239888277, 0.003468926060319849156, 0.004336157575399808735, 0.005203389090479769614, 0.006070620605559729627, 0.006937852120639688772, 0.007805083635719650519, 0.008672315150799608796, 0.009539546665879569676, 0.01040677818095952882, 0.01127400969603948970, 0.01214124121111944711, 0.01300847272619940452, 0.01387570424127936193 ),
 .UNSPECIFIED. ) ;
#41413 = VERTEX_POINT ( 'NONE', #94036 ) ;
#41414 = CARTESIAN_POINT ( 'NONE',  ( 4.499999999999970690, -10.91253812416064939, 4.000000000000000000 ) ) ;
#41415 = ORIENTED_EDGE ( 'NONE', *, *, #65702, .F. ) ;
#41416 = EDGE_CURVE ( 'NONE', #89832, #114032, #17202, .T. ) ;
#41417 = CARTESIAN_POINT ( 'NONE',  ( 71.24586038379622721, 3.974999999999996980, 6.884901960086287964 ) ) ;
#41418 = LINE ( 'NONE', #85626, #110267 ) ;
#41419 = DIRECTION ( 'NONE',  ( -1.000000000000000000, -1.224606353822377258E-16, -0.000000000000000000 ) ) ;
#41420 = CARTESIAN_POINT ( 'NONE',  ( 24.18398860626899705, 28.73617430169804265, 5.000000000000000000 ) ) ;
#41421 = ORIENTED_EDGE ( 'NONE', *, *, #48825, .F. ) ;
#41422 = CARTESIAN_POINT ( 'NONE',  ( 50.31293019189810423, -1.637169565754159617, -6.110000000000001208 ) ) ;
#41423 = VERTEX_POINT ( 'NONE', #83178 ) ;
#41424 = CARTESIAN_POINT ( 'NONE',  ( -24.32816939922335209, -21.74070752338406365, 4.000000000000000000 ) ) ;
#41425 = DIRECTION ( 'NONE',  ( -0.6830127018922180770, -0.6830127018922204085, -0.2588190451025213501 ) ) ;
#41426 = CARTESIAN_POINT ( 'NONE',  ( 11.22995720542198406, 21.73644205237998150, 5.000000000000000888 ) ) ;
#41427 = EDGE_CURVE ( 'NONE', #81813, #22881, #125980, .T. ) ;
#41428 = CARTESIAN_POINT ( 'NONE',  ( 12.60486233187513960, 21.75929247661549937, 21.32995629748183930 ) ) ;
#41429 = EDGE_CURVE ( 'NONE', #45858, #69422, #127602, .T. ) ;
#41430 = CARTESIAN_POINT ( 'NONE',  ( 41.62043019189810877, 3.055000000000001936, -5.291415217122916737 ) ) ;
#41431 = ORIENTED_EDGE ( 'NONE', *, *, #133427, .T. ) ;
#41432 = CARTESIAN_POINT ( 'NONE',  ( 34.45011844616451668, -4.483719188362457864, 5.000000000000000888 ) ) ;
#41433 = ORIENTED_EDGE ( 'NONE', *, *, #1868, .F. ) ;
#41434 = EDGE_LOOP ( 'NONE', ( #102970, #17259, #52186, #85557 ) ) ;
#41435 = ORIENTED_EDGE ( 'NONE', *, *, #82813, .T. ) ;
#41436 = FACE_OUTER_BOUND ( 'NONE', #55734, .T. ) ;
#41437 = EDGE_LOOP ( 'NONE', ( #139457, #19023, #79542, #67284 ) ) ;
#41438 = DIRECTION ( 'NONE',  ( -0.7071067811865487940, 0.7071067811865463515, 0.000000000000000000 ) ) ;
#41439 = CARTESIAN_POINT ( 'NONE',  ( 17.99451991528748351, 28.92564299267950645, 4.000000000000000000 ) ) ;
#41440 = VECTOR ( 'NONE', #101189, 1000.000000000000227 ) ;
#41441 = AXIS2_PLACEMENT_3D ( 'NONE', #121562, #31019, #486 ) ;
#41442 = VECTOR ( 'NONE', #64981, 999.9999999999998863 ) ;
#41443 = CARTESIAN_POINT ( 'NONE',  ( 174.7500000000000000, 7.919999999999947526, 19.12499999999998224 ) ) ;
#41444 = FACE_BOUND ( 'NONE', #55498, .T. ) ;
#41445 = ORIENTED_EDGE ( 'NONE', *, *, #85138, .F. ) ;
#41446 = CARTESIAN_POINT ( 'NONE',  ( 45.48921356237309510, -27.52281430457087197, 5.000000000000000000 ) ) ;
#41447 = DIRECTION ( 'NONE',  ( 1.301042606982605074E-16, -1.000000000000000000, 0.000000000000000000 ) ) ;
#41448 = LINE ( 'NONE', #85661, #6862 ) ;
#41449 = EDGE_LOOP ( 'NONE', ( #79711, #109469, #68492, #83430 ) ) ;
#41450 = ORIENTED_EDGE ( 'NONE', *, *, #85034, .F. ) ;
#41451 = VERTEX_POINT ( 'NONE', #62149 ) ;
#41452 = VECTOR ( 'NONE', #82058, 1000.000000000000000 ) ;
#41453 = CARTESIAN_POINT ( 'NONE',  ( 14.99999999999989519, -19.22509904557634997, 1.855685503482213505 ) ) ;
#41454 = VERTEX_POINT ( 'NONE', #136834 ) ;
#41455 = CARTESIAN_POINT ( 'NONE',  ( 54.45376352523144448, -6.109999999999998543, -3.741295971395162543E-16 ) ) ;
#41456 = ORIENTED_EDGE ( 'NONE', *, *, #95541, .T. ) ;
#41457 = FACE_OUTER_BOUND ( 'NONE', #106166, .T. ) ;
#41458 = DIRECTION ( 'NONE',  ( -0.000000000000000000, 0.3543493200069153248, 0.9351131265310292928 ) ) ;
#41459 = ORIENTED_EDGE ( 'NONE', *, *, #3919, .T. ) ;
#41460 = ADVANCED_FACE ( 'NONE', ( #50544 ), #26648, .T. ) ;
#41461 = DIRECTION ( 'NONE',  ( -0.6830127018922181881, 0.6830127018922202975, -0.2588190451025214056 ) ) ;
#41462 = CARTESIAN_POINT ( 'NONE',  ( -2.999999999999974243, 13.55218569542903317, 5.000000000000000000 ) ) ;
#41463 = AXIS2_PLACEMENT_3D ( 'NONE', #65287, #52922, #109473 ) ;
#41464 = VECTOR ( 'NONE', #16364, 999.9999999999998863 ) ;
#41465 = AXIS2_PLACEMENT_3D ( 'NONE', #98792, #141612, #74210 ) ;
#41466 = DIRECTION ( 'NONE',  ( 0.6830127018922181881, 0.6830127018922202975, -0.2588190451025214056 ) ) ;
#41467 =( NAMED_UNIT ( * ) PLANE_ANGLE_UNIT ( ) SI_UNIT ( $, .RADIAN. ) );
#41468 = DIRECTION ( 'NONE',  ( -0.000000000000000000, 1.000000000000000000, -0.000000000000000000 ) ) ;
#41469 = CARTESIAN_POINT ( 'NONE',  ( 6.852250093007166143, 4.584330080086930965E-16, 0.000000000000000000 ) ) ;
#41470 = CARTESIAN_POINT ( 'NONE',  ( -41.99451991528749062, 28.92564299267967343, 4.000000000000000000 ) ) ;
#41471 = VERTEX_POINT ( 'NONE', #36807 ) ;
#41472 = ORIENTED_EDGE ( 'NONE', *, *, #119947, .F. ) ;
#41473 = AXIS2_PLACEMENT_3D ( 'NONE', #28048, #73017, #116478 ) ;
#41474 = CARTESIAN_POINT ( 'NONE',  ( 5.999999999999960032, -10.44781430457072524, 5.000000000000000000 ) ) ;
#41475 = CARTESIAN_POINT ( 'NONE',  ( 0.000000000000000000, 0.000000000000000000, 5.000000000000000000 ) ) ;
#41476 = ORIENTED_EDGE ( 'NONE', *, *, #20375, .T. ) ;
#41477 = VECTOR ( 'NONE', #67064, 1000.000000000000000 ) ;
#41478 = ORIENTED_EDGE ( 'NONE', *, *, #11456, .T. ) ;
#41479 = VECTOR ( 'NONE', #65827, 1000.000000000000000 ) ;
#41480 = ORIENTED_EDGE ( 'NONE', *, *, #75480, .T. ) ;
#41481 = DIRECTION ( 'NONE',  ( -0.7071067811865486830, -0.7071067811865464625, 0.000000000000000000 ) ) ;
#41482 = CARTESIAN_POINT ( 'NONE',  ( 13.49999999999990585, -10.91253812416064228, 4.000000000000000000 ) ) ;
#41483 = EDGE_CURVE ( 'NONE', #124821, #105469, #122216, .T. ) ;
#41484 = EDGE_CURVE ( 'NONE', #118697, #110885, #142563, .T. ) ;
#41485 = DIRECTION ( 'NONE',  ( 0.7071067811865487940, 0.7071067811865463515, 0.000000000000000000 ) ) ;
#41486 = ORIENTED_EDGE ( 'NONE', *, *, #44385, .F. ) ;
#41487 = VECTOR ( 'NONE', #114984, 1000.000000000000000 ) ;
#41488 = CARTESIAN_POINT ( 'NONE',  ( -21.00548008471250938, 28.92564299267923644, 4.000000000000000000 ) ) ;
#41489 = VECTOR ( 'NONE', #42242, 1000.000000000000000 ) ;
#41490 = CARTESIAN_POINT ( 'NONE',  ( -21.60769999999999058, 3.130000000000008331, -2.396719511207313368E-16 ) ) ;
#41491 = CARTESIAN_POINT ( 'NONE',  ( 21.94206980810188057, 7.934999999999993392, 2.126176841940951689 ) ) ;
#41492 = CARTESIAN_POINT ( 'NONE',  ( 11.51078643762690490, -27.52281430457047406, 5.000000000000000000 ) ) ;
#41493 = ORIENTED_EDGE ( 'NONE', *, *, #92965, .F. ) ;
#41494 = CARTESIAN_POINT ( 'NONE',  ( 115.5579301918981088, 6.110000000000001208, -1.637169565754156286 ) ) ;
#41495 = EDGE_CURVE ( 'NONE', #133266, #110313, #109198, .T. ) ;
#41496 = FACE_OUTER_BOUND ( 'NONE', #123018, .T. ) ;
#41497 = CARTESIAN_POINT ( 'NONE',  ( -20.99999999999984368, -3.412538124160719555, 4.000000000000000000 ) ) ;
#41499 = ORIENTED_EDGE ( 'NONE', *, *, #32051, .F. ) ;
#41498 = DIRECTION ( 'NONE',  ( -0.000000000000000000, 0.3543493200069153248, 0.9351131265310292928 ) ) ;
#41500 = CARTESIAN_POINT ( 'NONE',  ( -13.49999999999989875, -10.91253812416064406, 4.000000000000000000 ) ) ;
#41501 = VERTEX_POINT ( 'NONE', #29485 ) ;
#41502 = DIRECTION ( 'NONE',  ( -0.000000000000000000, 0.000000000000000000, 1.000000000000000000 ) ) ;
#41503 = CARTESIAN_POINT ( 'NONE',  ( -8.999999999999932498, 11.96639925780213964, 5.000000000000000000 ) ) ;
#41504 = CARTESIAN_POINT ( 'NONE',  ( -23.99999999999983302, -13.06887692260768041, 4.000000000000000000 ) ) ;
#41505 = ADVANCED_FACE ( 'NONE', ( #129510 ), #4811, .T. ) ;
#41506 = ORIENTED_EDGE ( 'NONE', *, *, #59762, .T. ) ;
#41507 = CARTESIAN_POINT ( 'NONE',  ( -12.32816939922343735, -9.740707523384180888, 4.000000000000000000 ) ) ;
#41508 = CARTESIAN_POINT ( 'NONE',  ( -19.93618820135885983, -3.270000000000009788, -35.72555304890778416 ) ) ;
#41509 = VERTEX_POINT ( 'NONE', #75184 ) ;
#41510 = EDGE_CURVE ( 'NONE', #142252, #42684, #109049, .T. ) ;
#41511 = CARTESIAN_POINT ( 'NONE',  ( 8.811592354503320124, 9.902892378096218942E-16, 0.000000000000000000 ) ) ;
#41512 = CARTESIAN_POINT ( 'NONE',  ( 0.000000000000000000, 0.000000000000000000, 0.000000000000000000 ) ) ;
#41513 = LINE ( 'NONE', #129234, #88900 ) ;
#41514 = CARTESIAN_POINT ( 'NONE',  ( 6.489213562373093325, -27.52281430457059841, 5.000000000000000000 ) ) ;
#41515 = ORIENTED_EDGE ( 'NONE', *, *, #76028, .F. ) ;
#41516 = ORIENTED_EDGE ( 'NONE', *, *, #51281, .T. ) ;
#41517 = LINE ( 'NONE', #64717, #81971 ) ;
#41518 = DIRECTION ( 'NONE',  ( -0.3543493200069162685, -0.000000000000000000, -0.9351131265310288487 ) ) ;
#41519 = CARTESIAN_POINT ( 'NONE',  ( 12.52040314143522082, 7.934999999999989839, -2.126176841940961904 ) ) ;
#41520 = CARTESIAN_POINT ( 'NONE',  ( 34.42499999999998295, 0.000000000000000000, 4.500000000000000888 ) ) ;
#41521 = DIRECTION ( 'NONE',  ( 0.7071067811865487940, 0.7071067811865463515, 0.000000000000000000 ) ) ;
#41522 = ORIENTED_EDGE ( 'NONE', *, *, #62387, .F. ) ;
#41523 = EDGE_CURVE ( 'NONE', #76506, #109556, #119340, .T. ) ;
#41524 = LINE ( 'NONE', #76323, #106890 ) ;
#41525 = DIRECTION ( 'NONE',  ( -1.000000000000000000, -0.000000000000000000, -0.000000000000000000 ) ) ;
#41526 = CARTESIAN_POINT ( 'NONE',  ( 37.39126352523143737, -4.472830434245839371, -4.472830434245839371 ) ) ;
#41527 = DIRECTION ( 'NONE',  ( -0.000000000000000000, 0.000000000000000000, 1.000000000000000000 ) ) ;
#41528 = EDGE_CURVE ( 'NONE', #50567, #142230, #65012, .T. ) ;
#41529 = ADVANCED_FACE ( 'NONE', ( #87467 ), #131682, .T. ) ;
#41530 = VERTEX_POINT ( 'NONE', #52674 ) ;
#41531 = CARTESIAN_POINT ( 'NONE',  ( -18.70701326429291456, -21.74070752338405654, 4.999753212805221558 ) ) ;
#41532 = ORIENTED_EDGE ( 'NONE', *, *, #39102, .F. ) ;
#41533 = EDGE_LOOP ( 'NONE', ( #53570, #127514, #136826, #51770 ) ) ;
#41534 = AXIS2_PLACEMENT_3D ( 'NONE', #123303, #135595, #102961 ) ;
#41535 = DIRECTION ( 'NONE',  ( -0.000000000000000000, -0.3543493200069152693, 0.9351131265310292928 ) ) ;
#41536 = CARTESIAN_POINT ( 'NONE',  ( 30.18398860626900060, 28.73617430169808173, 5.000000000000000000 ) ) ;
#41537 = VECTOR ( 'NONE', #83650, 1000.000000000000000 ) ;
#41538 = AXIS2_PLACEMENT_3D ( 'NONE', #87871, #140802, #85710 ) ;
#41539 = EDGE_CURVE ( 'NONE', #22717, #3810, #30954, .T. ) ;
#41540 = EDGE_LOOP ( 'NONE', ( #81100, #68954, #19157 ) ) ;
#41541 =( BOUNDED_CURVE ( )  B_SPLINE_CURVE ( 3, ( #18983, #17543, #72714, #63251 ),
 .UNSPECIFIED., .F., .T. ) 
 B_SPLINE_CURVE_WITH_KNOTS ( ( 4, 4 ),
 ( 5.255487504216517003, 5.308805501018120765 ),
 .UNSPECIFIED. ) 
 CURVE ( )  GEOMETRIC_REPRESENTATION_ITEM ( )  RATIONAL_B_SPLINE_CURVE ( ( 1.000000000000000000, 0.9997631132982454094, 0.9997631132982454094, 1.000000000000000000 ) ) 
 REPRESENTATION_ITEM ( '' )  );
#41542 = CARTESIAN_POINT ( 'NONE',  ( 0.000000000000000000, -39.92999999999999261, -40.00000000000000000 ) ) ;
#41543 = DIRECTION ( 'NONE',  ( 0.3543493200069162685, -0.000000000000000000, -0.9351131265310288487 ) ) ;
#41544 = AXIS2_PLACEMENT_3D ( 'NONE', #58475, #14182, #35973 ) ;
#41545 = DIRECTION ( 'NONE',  ( 1.000000000000000000, 0.000000000000000000, 0.000000000000000000 ) ) ;
#41546 = ADVANCED_FACE ( 'NONE', ( #107058 ), #41812, .F. ) ;
#41547 = CARTESIAN_POINT ( 'NONE',  ( 82.22916666666665719, 7.950000000000001954, -2.130196079827421762 ) ) ;
#41548 = DIRECTION ( 'NONE',  ( -0.7071067811865486830, -0.7071067811865464625, -0.000000000000000000 ) ) ;
#41549 = ORIENTED_EDGE ( 'NONE', *, *, #44124, .F. ) ;
#41550 = EDGE_CURVE ( 'NONE', #7390, #50436, #96858, .T. ) ;
#41551 = LINE ( 'NONE', #142329, #111318 ) ;
#41552 = CARTESIAN_POINT ( 'NONE',  ( 17.07999999999999829, 9.521314400968980422E-16, 0.000000000000000000 ) ) ;
#41553 = CARTESIAN_POINT ( 'NONE',  ( 13.18000000000000149, -2.055000000000000160, 2.789133085058098087E-16 ) ) ;
#41554 = AXIS2_PLACEMENT_3D ( 'NONE', #142824, #97895, #142133 ) ;
#41555 =( NAMED_UNIT ( * ) SI_UNIT ( $, .STERADIAN. ) SOLID_ANGLE_UNIT ( ) );
#41556 = CARTESIAN_POINT ( 'NONE',  ( 33.32816939922329880, -6.740707523384202204, 4.000000000000000000 ) ) ;
#41557 = DIRECTION ( 'NONE',  ( -0.6830127018922181881, 0.6830127018922202975, -0.2588190451025214056 ) ) ;
#41558 = DIRECTION ( 'NONE',  ( -0.000000000000000000, -0.3543493200069152693, 0.9351131265310292928 ) ) ;
#41559 = CARTESIAN_POINT ( 'NONE',  ( 58.99586038379622721, -3.974999999999998312, -6.884901960086286188 ) ) ;
#41560 = EDGE_CURVE ( 'NONE', #53824, #139011, #106311, .T. ) ;
#41561 = DIRECTION ( 'NONE',  ( -0.6830127018922180770, -0.6830127018922204085, -0.2588190451025213501 ) ) ;
#41562 = CIRCLE ( 'NONE', #23017, 2.500000000000000444 ) ;
#41563 = VERTEX_POINT ( 'NONE', #140405 ) ;
#41564 = ORIENTED_EDGE ( 'NONE', *, *, #7229, .F. ) ;
#41565 = CARTESIAN_POINT ( 'NONE',  ( 54.22916666666666430, 7.950000000000001954, -2.130196079827421762 ) ) ;
#41566 = EDGE_CURVE ( 'NONE', #133878, #99698, #41091, .T. ) ;
#41567 = DIRECTION ( 'NONE',  ( 1.000000000000000000, 0.000000000000000000, 0.000000000000000000 ) ) ;
#41568 = PLANE ( 'NONE',  #46300 ) ;
#41569 = VECTOR ( 'NONE', #16383, 999.9999999999998863 ) ;
#41570 = CARTESIAN_POINT ( 'NONE',  ( -30.18398860626900060, 28.73617430169808173, 5.000000000000000000 ) ) ;
#41571 = ORIENTED_EDGE ( 'NONE', *, *, #95191, .T. ) ;
#41572 = ADVANCED_FACE ( 'NONE', ( #130266 ), #139727, .F. ) ;
#41573 = DIRECTION ( 'NONE',  ( 0.6830127018922180770, -0.6830127018922204085, -0.2588190451025213501 ) ) ;
#41574 = AXIS2_PLACEMENT_3D ( 'NONE', #17841, #29449, #104133 ) ;
#41575 = CARTESIAN_POINT ( 'NONE',  ( 46.95876352523143993, 0.000000000000000000, -6.110000000000001208 ) ) ;
#41576 = EDGE_LOOP ( 'NONE', ( #77682, #3301, #3043, #22730 ) ) ;
#41577 = CARTESIAN_POINT ( 'NONE',  ( 5.999999999999960032, -22.06887692260759692, 4.000000000000000000 ) ) ;
#41578 = ORIENTED_EDGE ( 'NONE', *, *, #134582, .F. ) ;
#41579 = EDGE_LOOP ( 'NONE', ( #52313, #120015, #3754, #121730 ) ) ;
#41580 = FACE_OUTER_BOUND ( 'NONE', #86540, .T. ) ;
#41581 = VECTOR ( 'NONE', #71232, 1000.000000000000227 ) ;
#41582 = VECTOR ( 'NONE', #24793, 1000.000000000000000 ) ;
#41583 = CARTESIAN_POINT ( 'NONE',  ( 80.87086038379622721, 6.884901960086289741, -3.974999999999993427 ) ) ;
#41584 = CARTESIAN_POINT ( 'NONE',  ( 20.29289321881331531, -18.74070752338408852, 5.000000000000000000 ) ) ;
#41585 = AXIS2_PLACEMENT_3D ( 'NONE', #43510, #44248, #132703 ) ;
#41586 = DIRECTION ( 'NONE',  ( 0.7071067811865486830, -0.7071067811865464625, -0.000000000000000000 ) ) ;
#41587 = ORIENTED_EDGE ( 'NONE', *, *, #119827, .F. ) ;
#41588 = CARTESIAN_POINT ( 'NONE',  ( -23.28242261357416254, -21.73023691814493219, 5.000000000000000888 ) ) ;
#41589 = FACE_OUTER_BOUND ( 'NONE', #114670, .T. ) ;
#41591 = VERTEX_POINT ( 'NONE', #128810 ) ;
#41590 = FACE_OUTER_BOUND ( 'NONE', #76637, .T. ) ;
#41592 = CARTESIAN_POINT ( 'NONE',  ( 83.56293019189811844, 1.637169565754157174, 6.110000000000002984 ) ) ;
#41593 = DIRECTION ( 'NONE',  ( -0.7071067811865486830, -0.7071067811865464625, -0.000000000000000000 ) ) ;
#41594 = LINE ( 'NONE', #86553, #38479 ) ;
#41595 = DIRECTION ( 'NONE',  ( -0.5735764363510501562, 0.8191520442889890230, 1.003171929053521419E-16 ) ) ;
#41596 = AXIS2_PLACEMENT_3D ( 'NONE', #37302, #138045, #26429 ) ;
#41597 = ADVANCED_FACE ( 'NONE', ( #74458 ), #64277, .F. ) ;
#41598 = LINE ( 'NONE', #18388, #50980 ) ;
#41599 = CARTESIAN_POINT ( 'NONE',  ( -25.95484226663317173, -21.74070752338405299, 21.72585301388578571 ) ) ;
#41600 = EDGE_CURVE ( 'NONE', #73177, #66788, #415, .T. ) ;
#41601 = EDGE_CURVE ( 'NONE', #36869, #103933, #67891, .T. ) ;
#41602 = ORIENTED_EDGE ( 'NONE', *, *, #114354, .F. ) ;
#41603 = B_SPLINE_CURVE_WITH_KNOTS ( 'NONE', 3,
 ( #109733, #110422, #11096, #98845 ),
 .UNSPECIFIED., .F., .F.,
 ( 4, 4 ),
 ( 0.003615568590623272072, 0.004164643302645765210 ),
 .UNSPECIFIED. ) ;
#41604 = SURFACE_SIDE_STYLE ('',( #73540 ) ) ;
#41605 = CARTESIAN_POINT ( 'NONE',  ( 69.76626352523143737, 4.472830434245839371, -4.472830434245838482 ) ) ;
#41606 = PLANE ( 'NONE',  #134386 ) ;
#41607 = CARTESIAN_POINT ( 'NONE',  ( -5.999999999999952927, 10.55218569542906160, 5.000000000000000000 ) ) ;
#41608 = CARTESIAN_POINT ( 'NONE',  ( 9.793339364578407924, 21.75929247661549937, 4.998822639870711626 ) ) ;
#41609 = ORIENTED_EDGE ( 'NONE', *, *, #56656, .T. ) ;
#41610 = ORIENTED_EDGE ( 'NONE', *, *, #113801, .T. ) ;
#41611 = VECTOR ( 'NONE', #123236, 1000.000000000000000 ) ;
#41612 = CARTESIAN_POINT ( 'NONE',  ( 0.000000000000000000, 0.000000000000000000, 0.000000000000000000 ) ) ;
#41614 = ADVANCED_FACE ( 'NONE', ( #11281 ), #68581, .F. ) ;
#41613 = CARTESIAN_POINT ( 'NONE',  ( -24.48921356237309510, -27.52281430457072631, 5.000000000000000000 ) ) ;
#41615 = VERTEX_POINT ( 'NONE', #123681 ) ;
#41616 = ORIENTED_EDGE ( 'NONE', *, *, #10192, .F. ) ;
#41617 = CARTESIAN_POINT ( 'NONE',  ( 6.083148067729274189, 21.75929247661549937, 7.311836541448064608 ) ) ;
#41618 = EDGE_LOOP ( 'NONE', ( #92859, #46641, #30674, #24561 ) ) ;
#41619 = CARTESIAN_POINT ( 'NONE',  ( -34.49999999999975842, -10.53574439159939757, 4.994342998332166772 ) ) ;
#41620 = CARTESIAN_POINT ( 'NONE',  ( -78.18398860626899705, 28.73617430169841924, 5.000000000000000000 ) ) ;
#41621 = DIRECTION ( 'NONE',  ( -0.7071067811865486830, 0.7071067811865464625, 0.000000000000000000 ) ) ;
#41622 = FACE_BOUND ( 'NONE', #74905, .T. ) ;
#41623 = FACE_OUTER_BOUND ( 'NONE', #41369, .T. ) ;
#41624 = DIRECTION ( 'NONE',  ( -0.7071067811865486830, -0.7071067811865464625, 0.000000000000000000 ) ) ;
#41625 = FACE_OUTER_BOUND ( 'NONE', #109939, .T. ) ;
#41627 = VERTEX_POINT ( 'NONE', #35957 ) ;
#41626 = DIRECTION ( 'NONE',  ( 0.6830127018922181881, 0.6830127018922202975, -0.2588190451025214056 ) ) ;
#41628 = CARTESIAN_POINT ( 'NONE',  ( 63.48921356237309510, -27.52281430457099631, 5.000000000000000000 ) ) ;
#41629 = ITEM_DEFINED_TRANSFORMATION ( 'NONE', 'NONE', #116470,  #127880 ) ;
#41630 = EDGE_LOOP ( 'NONE', ( #82070, #121218, #133405, #118126 ) ) ;
#41631 = VERTEX_POINT ( 'NONE', #133818 ) ;
#41632 = CARTESIAN_POINT ( 'NONE',  ( 81.43293019189810877, 1.637169565754156508, 6.110000000000000320 ) ) ;
#41633 = ORIENTED_EDGE ( 'NONE', *, *, #13608, .F. ) ;
#41634 = DIRECTION ( 'NONE',  ( -0.7071067811865486830, 0.7071067811865464625, 0.000000000000000000 ) ) ;
#41635 = EDGE_CURVE ( 'NONE', #104944, #118169, #78023, .T. ) ;
#41636 = EDGE_CURVE ( 'NONE', #122865, #28687, #10577, .T. ) ;
#41637 = ORIENTED_EDGE ( 'NONE', *, *, #60574, .F. ) ;
#41638 = DIRECTION ( 'NONE',  ( 0.000000000000000000, -1.000000000000000000, 0.000000000000000000 ) ) ;
#41639 = DIRECTION ( 'NONE',  ( -0.3543493200069163795, -9.265275131829747941E-33, -0.9351131265310288487 ) ) ;
#41640 = EDGE_CURVE ( 'NONE', #57451, #141054, #112074, .T. ) ;
#41641 = CARTESIAN_POINT ( 'NONE',  ( -29.54016161050242317, 18.75929247661552779, 8.305906642995418920 ) ) ;
#41642 = VECTOR ( 'NONE', #25089, 1000.000000000000227 ) ;
#41643 = CARTESIAN_POINT ( 'NONE',  ( -34.92500000000001137, 22.22500000000000142, 4.000000000000000000 ) ) ;
#41644 = DIRECTION ( 'NONE',  ( -0.6830127018922181881, 0.6830127018922202975, -0.2588190451025214056 ) ) ;
#41645 = DIRECTION ( 'NONE',  ( 0.000000000000000000, -1.000000000000000000, 0.000000000000000000 ) ) ;
#41646 = LINE ( 'NONE', #96706, #102515 ) ;
#41647 = LINE ( 'NONE', #109034, #62481 ) ;
#41649 = ORIENTED_EDGE ( 'NONE', *, *, #137433, .F. ) ;
#41648 = VECTOR ( 'NONE', #132208, 1000.000000000000000 ) ;
#41650 = CONICAL_SURFACE ( 'NONE', #141189, 2.500000000000000444, 0.9599310885968830309 ) ;
#41651 = CIRCLE ( 'NONE', #46251, 2.055000000000000604 ) ;
#41652 = FACE_OUTER_BOUND ( 'NONE', #116198, .T. ) ;
#41653 = VECTOR ( 'NONE', #120285, 1000.000000000000000 ) ;
#41654 = VERTEX_POINT ( 'NONE', #35245 ) ;
#41655 = CARTESIAN_POINT ( 'NONE',  ( 122.7250270504628844, 5.819803920172573974, -5.819803920172573086 ) ) ;
#41656 = DIRECTION ( 'NONE',  ( 0.7071067811865487940, 0.7071067811865463515, 0.000000000000000000 ) ) ;
#41658 = ADVANCED_FACE ( 'NONE', ( #56301 ), #115977, .T. ) ;
#41657 = VECTOR ( 'NONE', #4501, 1000.000000000000000 ) ;
#41659 = VERTEX_POINT ( 'NONE', #44717 ) ;
#41660 = VERTEX_POINT ( 'NONE', #133127 ) ;
#41661 = ADVANCED_FACE ( 'NONE', ( #109915 ), #2555, .T. ) ;
#41662 = EDGE_LOOP ( 'NONE', ( #24320, #38319, #135181, #9593 ) ) ;
#41663 = CARTESIAN_POINT ( 'NONE',  ( 36.02126352523143282, -4.472830434245838482, -4.472830434245840259 ) ) ;
#41664 = ORIENTED_EDGE ( 'NONE', *, *, #118311, .F. ) ;
#41665 = VECTOR ( 'NONE', #31594, 1000.000000000000227 ) ;
#41666 = DIRECTION ( 'NONE',  ( -0.000000000000000000, 0.000000000000000000, 1.000000000000000000 ) ) ;
#41667 = ADVANCED_FACE ( 'NONE', ( #34501 ), #56998, .F. ) ;
#41668 = EDGE_CURVE ( 'NONE', #56202, #54748, #91050, .T. ) ;
#41669 = CARTESIAN_POINT ( 'NONE',  ( 28.77497294953710849, 4.461849672132300881, 4.461849672132299105 ) ) ;
#41670 =( BOUNDED_CURVE ( )  B_SPLINE_CURVE ( 3, ( #99268, #110156, #77577, #22424 ),
 .UNSPECIFIED., .F., .T. ) 
 B_SPLINE_CURVE_WITH_KNOTS ( ( 4, 4 ),
 ( 1.989451877885386466, 2.205626217416170487 ),
 .UNSPECIFIED. ) 
 CURVE ( )  GEOMETRIC_REPRESENTATION_ITEM ( )  RATIONAL_B_SPLINE_CURVE ( ( 1.000000000000000000, 0.9961095111196428542, 0.9961095111196428542, 1.000000000000000000 ) ) 
 REPRESENTATION_ITEM ( '' )  );
#41671 = CARTESIAN_POINT ( 'NONE',  ( 5.327707837555167636, 13.12214320084893870, -24.84562023559181654 ) ) ;
#41672 = ORIENTED_EDGE ( 'NONE', *, *, #19404, .F. ) ;
#41673 = EDGE_CURVE ( 'NONE', #72122, #108664, #23618, .T. ) ;
#41674 = LINE ( 'NONE', #74321, #108208 ) ;
#41675 = ORIENTED_EDGE ( 'NONE', *, *, #119384, .F. ) ;
#41676 = DIRECTION ( 'NONE',  ( -0.7071067811865486830, 0.7071067811865464625, 0.000000000000000000 ) ) ;
#41677 = VECTOR ( 'NONE', #92909, 1000.000000000000227 ) ;
#41678 = LINE ( 'NONE', #119223, #22014 ) ;
#41680 = ORIENTED_EDGE ( 'NONE', *, *, #68552, .F. ) ;
#41679 = LINE ( 'NONE', #133005, #114203 ) ;
#41681 = VERTEX_POINT ( 'NONE', #1131 ) ;
#41682 = DIRECTION ( 'NONE',  ( 0.7071067811865486830, -0.7071067811865464625, -0.000000000000000000 ) ) ;
#41683 = DIRECTION ( 'NONE',  ( -0.000000000000000000, 0.000000000000000000, 1.000000000000000000 ) ) ;
#41684 = EDGE_CURVE ( 'NONE', #12168, #84409, #13427, .T. ) ;
#41685 = ORIENTED_EDGE ( 'NONE', *, *, #2326, .T. ) ;
#41686 = AXIS2_PLACEMENT_3D ( 'NONE', #23579, #113429, #69991 ) ;
#41687 = CARTESIAN_POINT ( 'NONE',  ( 7.031635159221873543, 2.259292476615694323, 13.77329220150639166 ) ) ;
#41688 = ORIENTED_EDGE ( 'NONE', *, *, #27425, .F. ) ;
#41689 = EDGE_LOOP ( 'NONE', ( #127875, #38645, #140567, #46574 ) ) ;
#41690 = ORIENTED_EDGE ( 'NONE', *, *, #20282, .T. ) ;
#41691 = FACE_OUTER_BOUND ( 'NONE', #54526, .T. ) ;
#41692 = EDGE_CURVE ( 'NONE', #135883, #54005, #105637, .T. ) ;
#41693 = ADVANCED_FACE ( 'NONE', ( #43959 ), #57707, .F. ) ;
#41694 = DIRECTION ( 'NONE',  ( 0.000000000000000000, -1.000000000000000000, 0.000000000000000000 ) ) ;
#41695 = VECTOR ( 'NONE', #46437, 1000.000000000000000 ) ;
#41696 = CARTESIAN_POINT ( 'NONE',  ( 7.499999999999951150, -1.533600742197721134, 5.000000000000000000 ) ) ;
#41697 = DIRECTION ( 'NONE',  ( -0.000000000000000000, -0.3543493200069152693, 0.9351131265310292928 ) ) ;
#41698 = CARTESIAN_POINT ( 'NONE',  ( -26.99999999999981171, 10.21212019023806938, -2.019456568337736346 ) ) ;
#41699 = DIRECTION ( 'NONE',  ( -0.000000000000000000, 0.3543493200069153248, 0.9351131265310292928 ) ) ;
#41700 = EDGE_LOOP ( 'NONE', ( #75743, #1493, #110903, #130667 ) ) ;
#41701 = VECTOR ( 'NONE', #113869, 999.9999999999998863 ) ;
#41702 = CARTESIAN_POINT ( 'NONE',  ( 66.91666666666667140, -6.884901960086287076, -3.975000000000000977 ) ) ;
#41703 = ORIENTED_EDGE ( 'NONE', *, *, #123665, .F. ) ;
#41704 = VECTOR ( 'NONE', #39287, 1000.000000000000000 ) ;
#41705 = EDGE_CURVE ( 'NONE', #122015, #64534, #27903, .T. ) ;
#41706 = CARTESIAN_POINT ( 'NONE',  ( -6.706792507240696644, 20.25929247661552068, 20.83292124670816392 ) ) ;
#41707 = CARTESIAN_POINT ( 'NONE',  ( 28.12456980810188867, -6.871911579029512218, 3.967499999999996252 ) ) ;
#41708 = ORIENTED_EDGE ( 'NONE', *, *, #118194, .T. ) ;
#41709 = AXIS2_PLACEMENT_3D ( 'NONE', #27015, #91570, #60395 ) ;
#41710 = DIRECTION ( 'NONE',  ( -0.000000000000000000, 0.000000000000000000, 1.000000000000000000 ) ) ;
#41711 = CARTESIAN_POINT ( 'NONE',  ( 11.99451991528749417, 28.92564299267946382, 4.000000000000000000 ) ) ;
#41712 = ORIENTED_EDGE ( 'NONE', *, *, #99097, .F. ) ;
#41713 = VERTEX_POINT ( 'NONE', #59836 ) ;
#41714 = EDGE_CURVE ( 'NONE', #1349, #16863, #49690, .T. ) ;
#41715 = CARTESIAN_POINT ( 'NONE',  ( 55.18164086290604331, -49.14999999999998437, 41.64499999999997470 ) ) ;
#41716 = CARTESIAN_POINT ( 'NONE',  ( -29.99999999999978328, -16.44781430457067373, 5.000000000000000000 ) ) ;
#41717 = VECTOR ( 'NONE', #76341, 1000.000000000000000 ) ;
#41718 = LINE ( 'NONE', #97503, #63235 ) ;
#41719 = CARTESIAN_POINT ( 'NONE',  ( 12.70701326429294831, -21.74070752338406365, 4.999753212805217117 ) ) ;
#41720 = CARTESIAN_POINT ( 'NONE',  ( 0.3619179557531525537, -48.99280962439294740, -39.49606053969947084 ) ) ;
#41721 = CARTESIAN_POINT ( 'NONE',  ( 61.16209685856478728, -5.291415217122919401, 3.054999999999998384 ) ) ;
#41722 = DIRECTION ( 'NONE',  ( 0.000000000000000000, -1.000000000000000000, 0.000000000000000000 ) ) ;
#41723 = ADVANCED_FACE ( 'NONE', ( #50383 ), #4661, .T. ) ;
#41724 = DIRECTION ( 'NONE',  ( 1.000000000000000000, 0.000000000000000000, 0.000000000000000000 ) ) ;
#41725 = DIRECTION ( 'NONE',  ( 0.7071067811865487940, 0.7071067811865463515, -0.000000000000000000 ) ) ;
#41726 = LINE ( 'NONE', #116434, #134489 ) ;
#41727 = ADVANCED_FACE ( 'NONE', ( #82305 ), #104748, .T. ) ;
#41728 = ORIENTED_EDGE ( 'NONE', *, *, #138241, .F. ) ;
#41729 = PLANE ( 'NONE',  #132144 ) ;
#41730 = ORIENTED_EDGE ( 'NONE', *, *, #65059, .T. ) ;
#41731 = VECTOR ( 'NONE', #64687, 1000.000000000000000 ) ;
#41732 = CARTESIAN_POINT ( 'NONE',  ( 10.49999999999992895, -19.53360074219753884, 5.000000000000000000 ) ) ;
#41733 = CARTESIAN_POINT ( 'NONE',  ( -12.18398860626900060, 28.73617430169795739, 5.000000000000000000 ) ) ;
#41734 = ORIENTED_EDGE ( 'NONE', *, *, #123751, .T. ) ;
#41735 = EDGE_CURVE ( 'NONE', #121024, #65687, #5410, .T. ) ;
#41736 = PLANE ( 'NONE',  #103859 ) ;
#41738 = ORIENTED_EDGE ( 'NONE', *, *, #17842, .T. ) ;
#41737 = DIRECTION ( 'NONE',  ( 0.7071067811865486830, -0.7071067811865464625, -0.000000000000000000 ) ) ;
#41739 = CARTESIAN_POINT ( 'NONE',  ( 106.7291666666666572, 7.950000000000001954, -2.130196079827421762 ) ) ;
#41740 = LINE ( 'NONE', #19271, #64938 ) ;
#41741 = CARTESIAN_POINT ( 'NONE',  ( 6.792893218813409462, 12.75929247661559351, 5.000000000000000000 ) ) ;
#41742 = ORIENTED_EDGE ( 'NONE', *, *, #6103, .T. ) ;
#41743 = EDGE_LOOP ( 'NONE', ( #22230, #42646, #27589, #114517, #87616, #106458 ) ) ;
#41744 = DIRECTION ( 'NONE',  ( 0.000000000000000000, -0.3543493200069153803, -0.9351131265310292928 ) ) ;
#41745 = CARTESIAN_POINT ( 'NONE',  ( 14.42840764549667476, 3.061616997868380183E-16, -2.500000000000001332 ) ) ;
#41746 = UNCERTAINTY_MEASURE_WITH_UNIT (LENGTH_MEASURE( 1.000000000000000082E-05 ), #93581, 'distance_accuracy_value', 'NONE');
#41747 = VECTOR ( 'NONE', #142493, 1000.000000000000000 ) ;
#41748 = PLANE ( 'NONE',  #63543 ) ;
#41749 = CARTESIAN_POINT ( 'NONE',  ( 84.07919371712955581, 3.975000000000002753, -6.884901960086283523 ) ) ;
#41750 = CARTESIAN_POINT ( 'NONE',  ( 30.29974487139158867, -27.71228299555227537, 4.000000000000000000 ) ) ;
#41751 = LINE ( 'NONE', #98961, #18259 ) ;
#41752 = ORIENTED_EDGE ( 'NONE', *, *, #94215, .F. ) ;
#41753 = EDGE_CURVE ( 'NONE', #31872, #79777, #92422, .T. ) ;
#41754 = CARTESIAN_POINT ( 'NONE',  ( -54.48921356237310221, -27.52281430457093236, 5.000000000000000000 ) ) ;
#41755 = LINE ( 'NONE', #130206, #108722 ) ;
#41756 = CARTESIAN_POINT ( 'NONE',  ( 30.47916666666666430, 6.094999999999988205, -1.633150327867694651 ) ) ;
#41757 = ORIENTED_EDGE ( 'NONE', *, *, #49253, .F. ) ;
#41759 = EDGE_CURVE ( 'NONE', #83399, #126191, #138098, .T. ) ;
#41758 = VECTOR ( 'NONE', #133209, 1000.000000000000000 ) ;
#41760 = CARTESIAN_POINT ( 'NONE',  ( 34.49999999999975842, 15.05432934483078888, 4.994342998332163219 ) ) ;
#41761 = PRESENTATION_LAYER_ASSIGNMENT (  '', '', ( #129692 ) ) ;
#41762 = ORIENTED_EDGE ( 'NONE', *, *, #12935, .F. ) ;
#41763 = AXIS2_PLACEMENT_3D ( 'NONE', #67952, #113528, #135326 ) ;
#41764 = CARTESIAN_POINT ( 'NONE',  ( 78.75043019189810423, 3.055000000000002824, -5.291415217122919401 ) ) ;
#41765 = FACE_OUTER_BOUND ( 'NONE', #8391, .T. ) ;
#41766 = LINE ( 'NONE', #130939, #74897 ) ;
#41767 = ORIENTED_EDGE ( 'NONE', *, *, #116058, .F. ) ;
#41768 = VECTOR ( 'NONE', #7049, 1000.000000000000227 ) ;
#41769 = VECTOR ( 'NONE', #99276, 1000.000000000000227 ) ;
#41770 = COLOUR_RGB ( '', 0.31764706, 0.68627451, 0.89019608) ;
#41771 = VECTOR ( 'NONE', #18207, 1000.000000000000000 ) ;
#41772 = LINE ( 'NONE', #9083, #95200 ) ;
#41773 = AXIS2_PLACEMENT_3D ( 'NONE', #106351, #116553, #141145 ) ;
#41774 = DIRECTION ( 'NONE',  ( 0.7071067811865487940, 0.7071067811865463515, 0.000000000000000000 ) ) ;
#41775 = LINE ( 'NONE', #75144, #74084 ) ;
#41776 = FACE_OUTER_BOUND ( 'NONE', #7091, .T. ) ;
#41778 = ORIENTED_EDGE ( 'NONE', *, *, #70665, .T. ) ;
#41777 = LINE ( 'NONE', #50511, #15042 ) ;
#41779 = CARTESIAN_POINT ( 'NONE',  ( 131.7497271887055490, -49.14999999999999147, -40.57187971031610374 ) ) ;
#41780 = LINE ( 'NONE', #30174, #100868 ) ;
#41781 = CARTESIAN_POINT ( 'NONE',  ( 9.299744871391588674, -27.71228299555212971, 4.000000000000000000 ) ) ;
#41782 = AXIS2_PLACEMENT_3D ( 'NONE', #121787, #108041, #131990 ) ;
#41783 = CARTESIAN_POINT ( 'NONE',  ( 60.20833333333333570, -3.974999999999999201, -6.884901960086287964 ) ) ;
#41784 = ORIENTED_EDGE ( 'NONE', *, *, #120508, .T. ) ;
#41785 = EDGE_CURVE ( 'NONE', #59176, #118319, #137393, .T. ) ;
#41786 = ORIENTED_EDGE ( 'NONE', *, *, #14943, .F. ) ;
#41787 = CARTESIAN_POINT ( 'NONE',  ( 70.72959685856477563, -6.110000000000000320, -1.637169565754161393 ) ) ;
#41788 = ORIENTED_EDGE ( 'NONE', *, *, #74973, .T. ) ;
#41789 = CARTESIAN_POINT ( 'NONE',  ( 39.48921356237310221, -27.52281430457082934, 5.000000000000000000 ) ) ;
#41790 = PLANE ( 'NONE',  #22543 ) ;
#41791 = VECTOR ( 'NONE', #93461, 1000.000000000000227 ) ;
#41792 = CARTESIAN_POINT ( 'NONE',  ( -12.69999999999998153, 0.000000000000000000, 0.000000000000000000 ) ) ;
#41793 = ORIENTED_EDGE ( 'NONE', *, *, #62675, .F. ) ;
#41794 = DIRECTION ( 'NONE',  ( 0.3543493200069162685, -0.000000000000000000, -0.9351131265310288487 ) ) ;
#41795 = CARTESIAN_POINT ( 'NONE',  ( -9.183988606268997046, 28.73617430169793607, 5.000000000000000000 ) ) ;
#41796 = VECTOR ( 'NONE', #59318, 1000.000000000000000 ) ;
#41797 = ORIENTED_EDGE ( 'NONE', *, *, #29745, .F. ) ;
#41798 = VECTOR ( 'NONE', #14726, 1000.000000000000227 ) ;
#41799 = LINE ( 'NONE', #141842, #95381 ) ;
#41800 = VECTOR ( 'NONE', #7201, 999.9999999999998863 ) ;
#41801 = CARTESIAN_POINT ( 'NONE',  ( -15.79289321881334551, -11.24070752338416845, 5.000000000000000000 ) ) ;
#41802 = CARTESIAN_POINT ( 'NONE',  ( -5.816011393731002066, 28.73617430169783304, 5.000000000000000000 ) ) ;
#41803 = CIRCLE ( 'NONE', #125095, 4.999999999999997335 ) ;
#41804 = ORIENTED_EDGE ( 'NONE', *, *, #83244, .F. ) ;
#41805 = ORIENTED_EDGE ( 'NONE', *, *, #81638, .T. ) ;
#41806 = LINE ( 'NONE', #86021, #138005 ) ;
#41807 = STYLED_ITEM ( 'NONE', ( #104080 ), #81930 ) ;
#41808 = CARTESIAN_POINT ( 'NONE',  ( -12.79289321881336505, 9.759292476615616607, 5.000000000000000000 ) ) ;
#41809 = LINE ( 'NONE', #86023, #46679 ) ;
#41810 = DIRECTION ( 'NONE',  ( 1.000000000000000000, 0.000000000000000000, 0.000000000000000000 ) ) ;
#41811 = CARTESIAN_POINT ( 'NONE',  ( -1.171830600776462061, -8.240707523384200428, 4.000000000000000000 ) ) ;
#41812 = PLANE ( 'NONE',  #46635 ) ;
#41813 = PRESENTATION_STYLE_ASSIGNMENT (( #21492 ) ) ;
#41814 = ORIENTED_EDGE ( 'NONE', *, *, #54368, .T. ) ;
#41815 = ORIENTED_EDGE ( 'NONE', *, *, #79555, .F. ) ;
#41816 = VERTEX_POINT ( 'NONE', #116341 ) ;
#41817 = VERTEX_POINT ( 'NONE', #36630 ) ;
#41818 = VECTOR ( 'NONE', #54443, 1000.000000000000000 ) ;
#41819 = CARTESIAN_POINT ( 'NONE',  ( 183.8160784826765735, -51.89584459748879652, 39.24672819827913628 ) ) ;
#41820 = CARTESIAN_POINT ( 'NONE',  ( 16.61159235450331906, -2.500000000000000000, 3.061616997868384127E-16 ) ) ;
#41821 = CARTESIAN_POINT ( 'NONE',  ( 84.18398860626899705, 28.73617430169846187, 5.000000000000000000 ) ) ;
#41822 = ORIENTED_EDGE ( 'NONE', *, *, #142604, .F. ) ;
#41823 = CARTESIAN_POINT ( 'NONE',  ( 18.63425672184678916, 4.584330080086930965E-16, 0.000000000000000000 ) ) ;
#41824 = CARTESIAN_POINT ( 'NONE',  ( -80.99451991528748351, 28.92564299267994699, 4.000000000000000000 ) ) ;
#41826 = ADVANCED_FACE ( 'NONE', ( #38787 ), #64905, .T. ) ;
#41825 = CARTESIAN_POINT ( 'NONE',  ( 58.12086038379622721, -6.884901960086286188, 3.974999999999997424 ) ) ;
#41827 = DIRECTION ( 'NONE',  ( -1.000000000000000000, 0.000000000000000000, 0.000000000000000000 ) ) ;
#41828 = AXIS2_PLACEMENT_3D ( 'NONE', #65426, #109602, #82701 ) ;
#41829 = CARTESIAN_POINT ( 'NONE',  ( 5.999999999999963585, 11.58746187583912324, 4.000000000000000000 ) ) ;
#41830 = ORIENTED_EDGE ( 'NONE', *, *, #139933, .F. ) ;
#41831 = CARTESIAN_POINT ( 'NONE',  ( -7.591674519009952604, -0.7407075233842735917, 14.76736230305379038 ) ) ;
#41832 = DIRECTION ( 'NONE',  ( 0.000000000000000000, 0.000000000000000000, 1.000000000000000000 ) ) ;
#41833 = EDGE_CURVE ( 'NONE', #53085, #49793, #25033, .T. ) ;
#41834 = EDGE_LOOP ( 'NONE', ( #25141, #27670, #63883, #143263 ) ) ;
#41835 = LINE ( 'NONE', #73742, #62089 ) ;
#41836 = ORIENTED_EDGE ( 'NONE', *, *, #53157, .T. ) ;
#41837 = ORIENTED_EDGE ( 'NONE', *, *, #97429, .F. ) ;
#41838 = EDGE_CURVE ( 'NONE', #41256, #46950, #106141, .T. ) ;
#41839 = EDGE_CURVE ( 'NONE', #32425, #54912, #108278, .T. ) ;
#41840 = ORIENTED_EDGE ( 'NONE', *, *, #63153, .T. ) ;
#41841 = CARTESIAN_POINT ( 'NONE',  ( 64.02126352523143282, -4.472830434245838482, -4.472830434245840259 ) ) ;
#41843 = VERTEX_POINT ( 'NONE', #97420 ) ;
#41842 = AXIS2_PLACEMENT_3D ( 'NONE', #45173, #35731, #121952 ) ;
#41844 = ORIENTED_EDGE ( 'NONE', *, *, #35789, .T. ) ;
#41845 = VECTOR ( 'NONE', #113174, 1000.000000000000227 ) ;
#41846 = ADVANCED_FACE ( 'NONE', ( #73563 ), #130816, .F. ) ;
#41847 = EDGE_CURVE ( 'NONE', #45656, #73359, #64831, .T. ) ;
#41848 = LINE ( 'NONE', #104948, #51225 ) ;
#41849 = SURFACE_STYLE_USAGE ( .BOTH. , #141140 ) ;
#41850 = CARTESIAN_POINT ( 'NONE',  ( 102.5212635252314328, -4.472830434245838482, -4.472830434245840259 ) ) ;
#41851 = CARTESIAN_POINT ( 'NONE',  ( 19.49999999999986144, 9.127013188829479873, 4.802533355213541633 ) ) ;
#41852 = EDGE_CURVE ( 'NONE', #2265, #67530, #140246, .T. ) ;
#41853 = CARTESIAN_POINT ( 'NONE',  ( -16.22850677138654873, 20.25929247661551713, 7.808871592221731106 ) ) ;
#41854 = VERTEX_POINT ( 'NONE', #63430 ) ;
#41855 = CARTESIAN_POINT ( 'NONE',  ( 69.48921356237309510, -27.52281430457103895, 5.000000000000000000 ) ) ;
#41856 = EDGE_CURVE ( 'NONE', #138634, #32809, #40931, .T. ) ;
#41857 = AXIS2_PLACEMENT_3D ( 'NONE', #51185, #29409, #88091 ) ;
#41858 = DIRECTION ( 'NONE',  ( -0.7071067811865487940, 0.7071067811865463515, -0.000000000000000000 ) ) ;
#41859 = DIRECTION ( 'NONE',  ( -0.7071067811865487940, 0.7071067811865463515, 0.000000000000000000 ) ) ;
#41861 = LINE ( 'NONE', #72391, #91479 ) ;
#41860 = AXIS2_PLACEMENT_3D ( 'NONE', #36139, #99201, #90512 ) ;
#41862 = ADVANCED_FACE ( 'NONE', ( #109013 ), #85136, .F. ) ;
#41864 = EDGE_LOOP ( 'NONE', ( #38957, #63145, #102807, #106634 ) ) ;
#41863 = AXIS2_PLACEMENT_3D ( 'NONE', #79289, #123493, #111122 ) ;
#41865 =( NAMED_UNIT ( * ) PLANE_ANGLE_UNIT ( ) SI_UNIT ( $, .RADIAN. ) );
#41866 = ORIENTED_EDGE ( 'NONE', *, *, #405, .F. ) ;
#41867 = EDGE_LOOP ( 'NONE', ( #106535, #31992, #9067, #64086 ) ) ;
#41868 = EDGE_LOOP ( 'NONE', ( #107578, #13013, #23166, #102285 ) ) ;
#41869 = CARTESIAN_POINT ( 'NONE',  ( 124.1620968585647944, -5.291415217122919401, 3.054999999999997939 ) ) ;
#41870 = VECTOR ( 'NONE', #16158, 1000.000000000000000 ) ;
#41871 = AXIS2_PLACEMENT_3D ( 'NONE', #92518, #56394, #59242 ) ;
#41872 = VERTEX_POINT ( 'NONE', #7558 ) ;
#41873 = AXIS2_PLACEMENT_3D ( 'NONE', #86665, #17790, #97502 ) ;
#41874 = VECTOR ( 'NONE', #61768, 1000.000000000000000 ) ;
#41875 = LINE ( 'NONE', #8472, #70086 ) ;
#41876 = EDGE_CURVE ( 'NONE', #21943, #25521, #140936, .T. ) ;
#41877 = DIRECTION ( 'NONE',  ( -0.7071067811865487940, 0.7071067811865463515, 0.000000000000000000 ) ) ;
#41878 = ORIENTED_EDGE ( 'NONE', *, *, #36114, .F. ) ;
#41879 = SURFACE_STYLE_USAGE ( .BOTH. , #17935 ) ;
#41881 = ORIENTED_EDGE ( 'NONE', *, *, #65646, .F. ) ;
#41880 = VECTOR ( 'NONE', #81740, 999.9999999999998863 ) ;
#41882 = EDGE_CURVE ( 'NONE', #68883, #110486, #86589, .T. ) ;
#41883 = CARTESIAN_POINT ( 'NONE',  ( 2.895403141435219485, 2.126176841940962348, 7.934999999999989839 ) ) ;
#41884 = CARTESIAN_POINT ( 'NONE',  ( 0.000000000000000000, 0.000000000000000000, 5.000000000000000000 ) ) ;
#41885 = AXIS2_PLACEMENT_3D ( 'NONE', #15377, #26303, #106678 ) ;
#41886 = CARTESIAN_POINT ( 'NONE',  ( 38.91666666666665719, -6.884901960086287076, -3.975000000000000977 ) ) ;
#41887 = ORIENTED_EDGE ( 'NONE', *, *, #111079, .F. ) ;
#41888 = EDGE_LOOP ( 'NONE', ( #29656, #139120, #15899 ) ) ;
#41890 = ORIENTED_EDGE ( 'NONE', *, *, #9758, .T. ) ;
#41889 = EDGE_CURVE ( 'NONE', #99771, #29164, #75010, .T. ) ;
#41892 = VECTOR ( 'NONE', #105534, 1000.000000000000000 ) ;
#41891 = FACE_OUTER_BOUND ( 'NONE', #72368, .T. ) ;
#41893 = CARTESIAN_POINT ( 'NONE',  ( -18.48921356237309510, -27.52281430457068367, 5.000000000000000000 ) ) ;
#41894 = DIRECTION ( 'NONE',  ( 0.7071067811865486830, -0.7071067811865464625, -0.000000000000000000 ) ) ;
#41895 = FACE_OUTER_BOUND ( 'NONE', #42408, .T. ) ;
#41896 = DIRECTION ( 'NONE',  ( 0.6830127018922180770, -0.6830127018922204085, -0.2588190451025213501 ) ) ;
#41897 = AXIS2_PLACEMENT_3D ( 'NONE', #100995, #99552, #122751 ) ;
#41898 = ADVANCED_FACE ( 'NONE', ( #111902 ), #132247, .F. ) ;
#41899 = VECTOR ( 'NONE', #35036, 1000.000000000000000 ) ;
#41900 = CARTESIAN_POINT ( 'NONE',  ( 22.82816939922337696, 18.75929247661552779, 4.000000000000000000 ) ) ;
#41901 = CARTESIAN_POINT ( 'NONE',  ( 29.45876352523143993, 0.000000000000000000, -6.110000000000001208 ) ) ;
#41902 = DIRECTION ( 'NONE',  ( -0.000000000000000000, -1.000000000000000000, -0.000000000000000000 ) ) ;
#41903 = CARTESIAN_POINT ( 'NONE',  ( -19.17183060077631751, -20.24070752338406365, 4.000000000000000000 ) ) ;
#41904 = ADVANCED_FACE ( 'NONE', ( #55387 ), #99561, .F. ) ;
#41905 = AXIS2_PLACEMENT_3D ( 'NONE', #131007, #122234, #76640 ) ;
#41906 = EDGE_LOOP ( 'NONE', ( #112221, #118569, #57878, #107916 ) ) ;
#41907 = CARTESIAN_POINT ( 'NONE',  ( 3.183988606268992161, 28.73617430169789699, 5.000000000000000000 ) ) ;
#41909 = VECTOR ( 'NONE', #31932, 1000.000000000000000 ) ;
#41908 = DIRECTION ( 'NONE',  ( 0.7071067811865487940, 0.7071067811865463515, -0.000000000000000000 ) ) ;
#41910 = VERTEX_POINT ( 'NONE', #10413 ) ;
#41911 = EDGE_CURVE ( 'NONE', #132567, #64833, #11110, .T. ) ;
#41912 = ADVANCED_FACE ( 'NONE', ( #22698 ), #77157, .F. ) ;
#41913 = CARTESIAN_POINT ( 'NONE',  ( -25.39999999999996305, 0.000000000000000000, 0.000000000000000000 ) ) ;
#41915 = ORIENTED_EDGE ( 'NONE', *, *, #49128, .T. ) ;
#41914 = CARTESIAN_POINT ( 'NONE',  ( 29.20710678118634007, 18.75929247661552424, 5.000000000000000000 ) ) ;
#41916 = AXIS2_PLACEMENT_3D ( 'NONE', #18320, #8846, #66168 ) ;
#41917 = CARTESIAN_POINT ( 'NONE',  ( 30.79289321881325137, -14.24070752338413826, 5.000000000000000000 ) ) ;
#41918 = ORIENTED_EDGE ( 'NONE', *, *, #97281, .T. ) ;
#41919 = CARTESIAN_POINT ( 'NONE',  ( 20.20710678118640402, -5.240707523384230626, 5.000000000000000000 ) ) ;
#41920 = ORIENTED_EDGE ( 'NONE', *, *, #79394, .F. ) ;
#41921 = DIRECTION ( 'NONE',  ( -0.6830127018922180770, -0.6830127018922204085, -0.2588190451025213501 ) ) ;
#41922 = ORIENTED_EDGE ( 'NONE', *, *, #37913, .T. ) ;
#41923 = LINE ( 'NONE', #52076, #91462 ) ;
#41924 = CARTESIAN_POINT ( 'NONE',  ( 110.0375270504628986, -9.735942053221456900E-16, 7.949999999999998401 ) ) ;
#41925 = DIRECTION ( 'NONE',  ( 0.7071067811865487940, 0.7071067811865463515, 0.000000000000000000 ) ) ;
#41926 = VECTOR ( 'NONE', #54154, 1000.000000000000000 ) ;
#41927 = CARTESIAN_POINT ( 'NONE',  ( -34.25154412867554754, -11.24070752338416490, 10.39518518046017270 ) ) ;
#41928 = EDGE_CURVE ( 'NONE', #139710, #131546, #78562, .T. ) ;
#41929 = CARTESIAN_POINT ( 'NONE',  ( 11.67183060077639212, 20.25929247661552424, 4.000000000000000000 ) ) ;
#41930 = CARTESIAN_POINT ( 'NONE',  ( 22.49999999999983302, -14.70932175296475819, -11.46312253303842432 ) ) ;
#41931 = CARTESIAN_POINT ( 'NONE',  ( 31.49999999999977973, 15.43112307739202471, 4.000000000000000000 ) ) ;
#41933 = VECTOR ( 'NONE', #62832, 1000.000000000000000 ) ;
#41932 = CARTESIAN_POINT ( 'NONE',  ( 4.083333333333333925, -5.278424836066144543, 3.047499999999995879 ) ) ;
#41934 = CARTESIAN_POINT ( 'NONE',  ( 20.68706980810188867, -2.126176841940956130, 7.934999999999990727 ) ) ;
#41936 = VECTOR ( 'NONE', #39423, 1000.000000000000000 ) ;
#41935 = PLANE ( 'NONE',  #58306 ) ;
#41937 = CYLINDRICAL_SURFACE ( 'NONE', #17661, 6.499999999999999112 ) ;
#41938 = ORIENTED_EDGE ( 'NONE', *, *, #126522, .F. ) ;
#41939 = ORIENTED_EDGE ( 'NONE', *, *, #137605, .T. ) ;
#41940 = DIRECTION ( 'NONE',  ( -1.000000000000000000, -0.000000000000000000, -0.000000000000000000 ) ) ;
#41941 = ORIENTED_EDGE ( 'NONE', *, *, #122198, .T. ) ;
#41942 = CARTESIAN_POINT ( 'NONE',  ( 33.47336096364195157, -5.240707523384228850, 16.25846745537503324 ) ) ;
#41943 = LINE ( 'NONE', #32494, #43967 ) ;
#41944 = SURFACE_STYLE_USAGE ( .BOTH. , #52782 ) ;
#41945 = MECHANICAL_DESIGN_GEOMETRIC_PRESENTATION_REPRESENTATION (  '', ( #14075 ), #127512 ) ;
#41946 = CARTESIAN_POINT ( 'NONE',  ( 127.6984665281606368, -50.67230138428462993, -37.61253110040882319 ) ) ;
#41947 = EDGE_LOOP ( 'NONE', ( #31580, #51364, #48605, #98483 ) ) ;
#41948 = CARTESIAN_POINT ( 'NONE',  ( -34.49999999999975131, 9.431123077392088661, 4.000000000000000000 ) ) ;
#41949 = CARTESIAN_POINT ( 'NONE',  ( 93.31249999999998579, 5.819803920172571310, 5.819803920172576639 ) ) ;
#41950 = EDGE_CURVE ( 'NONE', #97682, #28445, #113504, .T. ) ;
#41952 = EDGE_LOOP ( 'NONE', ( #87528, #28787, #70562, #78280 ) ) ;
#41951 = DIRECTION ( 'NONE',  ( -0.7071067811865486830, -0.7071067811865464625, 0.000000000000000000 ) ) ;
#41953 = CARTESIAN_POINT ( 'NONE',  ( -34.92500000000001137, -11.24070752338416490, 4.255531930566251120 ) ) ;
#41954 = CARTESIAN_POINT ( 'NONE',  ( 25.39999999999999858, 0.000000000000000000, 0.000000000000000000 ) ) ;
#41955 = VECTOR ( 'NONE', #83312, 1000.000000000000000 ) ;
#41956 = CARTESIAN_POINT ( 'NONE',  ( 42.48921356237308800, -27.52281430457085065, 5.000000000000000000 ) ) ;
#41957 = CARTESIAN_POINT ( 'NONE',  ( -27.70710678118634718, -0.7407075233842701500, 5.000000000000000000 ) ) ;
#41958 = CARTESIAN_POINT ( 'NONE',  ( 60.42123663339494044, -43.84677628532234195, 34.92499999999998295 ) ) ;
#41959 = EDGE_LOOP ( 'NONE', ( #136274, #103984, #59909, #103960 ) ) ;
#41960 = ORIENTED_EDGE ( 'NONE', *, *, #125806, .T. ) ;
#41961 = ORIENTED_EDGE ( 'NONE', *, *, #133216, .F. ) ;
#41962 = CARTESIAN_POINT ( 'NONE',  ( 101.7920968585647756, -5.291415217122921177, 3.054999999999999272 ) ) ;
#41963 = EDGE_LOOP ( 'NONE', ( #32057, #122124, #60336, #40990 ) ) ;
#41964 = CARTESIAN_POINT ( 'NONE',  ( 127.7579555295392026, -48.22435659090666604, 37.54366622512468865 ) ) ;
#41965 = CARTESIAN_POINT ( 'NONE',  ( -27.18398860626900060, 28.73617430169806042, 5.000000000000000000 ) ) ;
#41966 = ORIENTED_EDGE ( 'NONE', *, *, #64639, .T. ) ;
#41967 = VECTOR ( 'NONE', #104435, 1000.000000000000000 ) ;
#41968 = LINE ( 'NONE', #87605, #14385 ) ;
#41971 = EDGE_CURVE ( 'NONE', #103076, #54110, #132964, .T. ) ;
#41970 =( BOUNDED_SURFACE ( )  B_SPLINE_SURFACE ( 3, 2, ( 
 ( #91813, #113561, #47651 ),
 ( #78824, #136036, #14958 ),
 ( #133214, #36042, #79578 ),
 ( #23711, #112850, #1216 ),
 ( #70125, #123763, #57799 ),
 ( #103388, #59239, #13519 ),
 ( #4035, #33890, #88989 ),
 ( #122284, #36720, #22957 ),
 ( #123035, #101989, #124449 ),
 ( #25119, #67226, #133904 ),
 ( #69378, #89677, #111422 ),
 ( #14259, #12107, #56391 ),
 ( #45500, #100572, #34595 ),
 ( #15639, #6908, #82393 ),
 ( #38176, #126572, #62076 ),
 ( #81697, #16373, #27263 ) ),
 .UNSPECIFIED., .F., .F., .F. ) 
 B_SPLINE_SURFACE_WITH_KNOTS ( ( 4, 2, 2, 2, 2, 2, 2, 4 ),
 ( 3, 3 ),
 ( -4.336808689942017736E-19, 0.0009973376669657767115, 0.001496006500448665393, 0.001994675333931553857, 0.002493344167414442321, 0.002992013000897330785, 0.003490681834380219249, 0.003989350667863107713 ),
 ( 0.000000000000000000, 1.000000000000000000 ),
 .UNSPECIFIED. ) 
 GEOMETRIC_REPRESENTATION_ITEM ( )  RATIONAL_B_SPLINE_SURFACE ( (
 ( 1.000000000000000000, 0.7366656399173067138, 1.000000000000000000),
 ( 1.000000000000000000, 0.7469946078304352532, 1.000000000000000000),
 ( 1.000000000000000000, 0.7550065080344044999, 1.000000000000000000),
 ( 1.000000000000000000, 0.7644701404565185099, 1.000000000000000000),
 ( 1.000000000000000000, 0.7671379903610555662, 1.000000000000000000),
 ( 1.000000000000000000, 0.7716469694716783234, 1.000000000000000000),
 ( 1.000000000000000000, 0.7735028669872892060, 1.000000000000000000),
 ( 1.000000000000000000, 0.7766014048701626038, 1.000000000000000000),
 ( 1.000000000000000000, 0.7778260050860584807, 1.000000000000000000),
 ( 1.000000000000000000, 0.7797609306255449679, 1.000000000000000000),
 ( 1.000000000000000000, 0.7804845266836839546, 1.000000000000000000),
 ( 1.000000000000000000, 0.7815908473005801493, 1.000000000000000000),
 ( 1.000000000000000000, 0.7819678579954093545, 1.000000000000000000),
 ( 1.000000000000000000, 0.7824545089705922107, 1.000000000000000000),
 ( 1.000000000000000000, 0.7825677149574248315, 1.000000000000000000),
 ( 1.000000000000000000, 0.7825691453495833283, 1.000000000000000000) ) ) 
 REPRESENTATION_ITEM ( '' )  SURFACE ( )  );
#41969 = CARTESIAN_POINT ( 'NONE',  ( 48.39583333333332860, -2.130196079827427091, 7.949999999999998401 ) ) ;
#41972 = AXIS2_PLACEMENT_3D ( 'NONE', #30977, #62170, #128829 ) ;
#41973 = VECTOR ( 'NONE', #104169, 1000.000000000000000 ) ;
#41974 = CARTESIAN_POINT ( 'NONE',  ( 98.05793019189812298, 6.110000000000000320, -1.637169565754156064 ) ) ;
#41975 = ADVANCED_FACE ( 'NONE', ( #121328 ), #45945, .F. ) ;
#41976 = ORIENTED_EDGE ( 'NONE', *, *, #106226, .F. ) ;
#41977 = CARTESIAN_POINT ( 'NONE',  ( 54.48921356237310221, -27.52281430457093236, 5.000000000000000000 ) ) ;
#41978 = DIRECTION ( 'NONE',  ( -0.000000000000000000, 0.000000000000000000, 1.000000000000000000 ) ) ;
#41979 = PRESENTATION_LAYER_ASSIGNMENT (  '', '', ( #141518 ) ) ;
#41980 = VECTOR ( 'NONE', #38016, 1000.000000000000000 ) ;
#41981 = CARTESIAN_POINT ( 'NONE',  ( 115.9166666666666714, -6.884901960086287076, -3.975000000000000977 ) ) ;
#41982 = TOROIDAL_SURFACE ( 'NONE', #136966, 31.92999999999999972, 3.000000000000000000 ) ;
#41983 = AXIS2_PLACEMENT_3D ( 'NONE', #86183, #23785, #80332 ) ;
#41984 = LINE ( 'NONE', #52127, #11502 ) ;
#41985 = AXIS2_PLACEMENT_3D ( 'NONE', #20445, #31356, #21177 ) ;
#41986 = ORIENTED_EDGE ( 'NONE', *, *, #123901, .F. ) ;
#41987 = ORIENTED_EDGE ( 'NONE', *, *, #117609, .F. ) ;
#41988 = EDGE_LOOP ( 'NONE', ( #3324, #84082, #43484 ) ) ;
#41989 = DIRECTION ( 'NONE',  ( 0.6830127018922180770, -0.6830127018922204085, -0.2588190451025213501 ) ) ;
#41990 = EDGE_CURVE ( 'NONE', #70009, #24205, #44108, .T. ) ;
#41991 = DIRECTION ( 'NONE',  ( 0.7071067811865487940, -0.7071067811865463515, 0.000000000000000000 ) ) ;
#41992 = CARTESIAN_POINT ( 'NONE',  ( 16.54623647476855552, -7.934999999999990727, 4.858786175617117713E-16 ) ) ;
#41993 = VECTOR ( 'NONE', #134503, 1000.000000000000000 ) ;
#41994 = DIRECTION ( 'NONE',  ( -1.000000000000000000, -1.224606353822377258E-16, -0.000000000000000000 ) ) ;
#41995 = DIRECTION ( 'NONE',  ( 0.7071067811865487940, 0.7071067811865463515, 0.000000000000000000 ) ) ;
#41996 = EDGE_LOOP ( 'NONE', ( #4088, #65261, #72577, #75967 ) ) ;
#41997 = ORIENTED_EDGE ( 'NONE', *, *, #86910, .F. ) ;
#41998 =( GEOMETRIC_REPRESENTATION_CONTEXT ( 3 ) GLOBAL_UNCERTAINTY_ASSIGNED_CONTEXT ( ( #9983 ) ) GLOBAL_UNIT_ASSIGNED_CONTEXT ( ( #133825, #7905, #122206 ) ) REPRESENTATION_CONTEXT ( 'NONE', 'WORKASPACE' ) );
#41999 = CARTESIAN_POINT ( 'NONE',  ( -51.29974487139158867, -27.71228299555242103, 4.000000000000000000 ) ) ;
#42000 = ORIENTED_EDGE ( 'NONE', *, *, #125258, .F. ) ;
#42001 = VERTEX_POINT ( 'NONE', #143091 ) ;
#42002 = CIRCLE ( 'NONE', #123025, 2.055000000000000604 ) ;
#42003 = VECTOR ( 'NONE', #44878, 999.9999999999998863 ) ;
#42004 = CARTESIAN_POINT ( 'NONE',  ( 0.7228143045705931469, -21.72500000000000142, 5.000000000000000000 ) ) ;
#42005 = VERTEX_POINT ( 'NONE', #57538 ) ;
#42006 = LINE ( 'NONE', #121670, #124757 ) ;
#42007 = FACE_OUTER_BOUND ( 'NONE', #37903, .T. ) ;
#42008 = VECTOR ( 'NONE', #56701, 1000.000000000000227 ) ;
#42009 = ADVANCED_FACE ( 'NONE', ( #76426 ), #44535, .T. ) ;
#42010 = EDGE_CURVE ( 'NONE', #14592, #25060, #122027, .T. ) ;
#42011 = DIRECTION ( 'NONE',  ( -0.6830127018922180770, -0.6830127018922204085, -0.2588190451025213501 ) ) ;
#42012 = CARTESIAN_POINT ( 'NONE',  ( 14.99451991528749595, 28.92564299267948513, 4.000000000000000000 ) ) ;
#42013 = VECTOR ( 'NONE', #135544, 1000.000000000000000 ) ;
#42014 = CARTESIAN_POINT ( 'NONE',  ( -72.18398860626899705, 28.73617430169837661, 5.000000000000000000 ) ) ;
#42015 = EDGE_LOOP ( 'NONE', ( #141381, #60730, #21280, #106094 ) ) ;
#42016 = VERTEX_POINT ( 'NONE', #134374 ) ;
#42017 = CARTESIAN_POINT ( 'NONE',  ( 25.40000000000000924, -4.504858206827953460, -6.583681173200965908 ) ) ;
#42018 = CARTESIAN_POINT ( 'NONE',  ( -4.499999999999967137, -17.91344420646042934, 1.358650452708453527 ) ) ;
#42019 = ORIENTED_EDGE ( 'NONE', *, *, #14873, .T. ) ;
#42020 = AXIS2_PLACEMENT_3D ( 'NONE', #12467, #79928, #13165 ) ;
#42021 = SURFACE_SIDE_STYLE ('',( #6463 ) ) ;
#42023 = VERTEX_POINT ( 'NONE', #79315 ) ;
#42022 = EDGE_CURVE ( 'NONE', #79351, #20950, #35074, .T. ) ;
#42024 = LINE ( 'NONE', #20225, #66734 ) ;
#42025 = ORIENTED_EDGE ( 'NONE', *, *, #37781, .F. ) ;
#42026 = ORIENTED_EDGE ( 'NONE', *, *, #34253, .T. ) ;
#42027 = EDGE_LOOP ( 'NONE', ( #114998, #86804, #110383, #92067 ) ) ;
#42028 = ADVANCED_FACE ( 'NONE', ( #111146 ), #87997, .T. ) ;
#42029 = EDGE_CURVE ( 'NONE', #14374, #111466, #56122, .T. ) ;
#42030 = CARTESIAN_POINT ( 'NONE',  ( 28.78709685856477307, 3.054999999999997495, 5.291415217122919401 ) ) ;
#42031 = CARTESIAN_POINT ( 'NONE',  ( 24.48921356237309510, -27.52281430457072631, 5.000000000000000000 ) ) ;
#42033 = EDGE_CURVE ( 'NONE', #108474, #81238, #45245, .T. ) ;
#42032 = CARTESIAN_POINT ( 'NONE',  ( 151.4000000000000057, -17.48000000000005016, 12.69999999999954454 ) ) ;
#42034 = FILL_AREA_STYLE_COLOUR ( '', #92439 ) ;
#42035 = DIRECTION ( 'NONE',  ( -0.7071067811865486830, -0.7071067811865464625, 0.000000000000000000 ) ) ;
#42036 = ADVANCED_FACE ( 'NONE', ( #21317 ), #109745, .F. ) ;
#42037 = LINE ( 'NONE', #28296, #126979 ) ;
#42038 = LINE ( 'NONE', #129017, #71322 ) ;
#42039 = VECTOR ( 'NONE', #81336, 1000.000000000000000 ) ;
#42040 = EDGE_CURVE ( 'NONE', #24858, #29128, #111119, .T. ) ;
#42041 = DIRECTION ( 'NONE',  ( -0.3543493200069162685, -0.000000000000000000, -0.9351131265310288487 ) ) ;
#42042 = DIRECTION ( 'NONE',  ( -0.3543493200069162685, -0.000000000000000000, -0.9351131265310288487 ) ) ;
#42043 = EDGE_CURVE ( 'NONE', #61841, #3531, #65909, .T. ) ;
#42044 = DIRECTION ( 'NONE',  ( 1.000000000000000000, 0.000000000000000000, 0.000000000000000000 ) ) ;
#42045 = DIRECTION ( 'NONE',  ( 0.5735764363510451602, 0.8191520442889924647, 0.000000000000000000 ) ) ;
#42046 = EDGE_CURVE ( 'NONE', #57920, #16561, #71261, .T. ) ;
#42047 = VERTEX_POINT ( 'NONE', #49528 ) ;
#42048 = VERTEX_POINT ( 'NONE', #61140 ) ;
#42049 = ORIENTED_EDGE ( 'NONE', *, *, #47497, .T. ) ;
#42050 = VECTOR ( 'NONE', #77220, 1000.000000000000227 ) ;
#42051 = ORIENTED_EDGE ( 'NONE', *, *, #11879, .F. ) ;
#42052 = CARTESIAN_POINT ( 'NONE',  ( -0.3480366351640904465, 1.285757288101296858, 3.988067004281481864 ) ) ;
#42053 = ORIENTED_EDGE ( 'NONE', *, *, #123013, .F. ) ;
#42054 = ORIENTED_EDGE ( 'NONE', *, *, #13043, .F. ) ;
#42055 = PLANE ( 'NONE',  #46816 ) ;
#42056 = DIRECTION ( 'NONE',  ( 0.000000000000000000, 0.000000000000000000, 1.000000000000000000 ) ) ;
#42057 = EDGE_CURVE ( 'NONE', #100907, #16046, #35797, .T. ) ;
#42058 = ADVANCED_FACE ( 'NONE', ( #58281 ), #136488, .F. ) ;
#42059 = CARTESIAN_POINT ( 'NONE',  ( -34.92500000000001137, 22.22500000000000142, 5.000000000000000000 ) ) ;
#42060 = EDGE_LOOP ( 'NONE', ( #14190, #52325, #31437, #67413 ) ) ;
#42061 = LINE ( 'NONE', #73260, #92727 ) ;
#42062 = CIRCLE ( 'NONE', #7233, 2.500000000000000888 ) ;
#42063 = EDGE_LOOP ( 'NONE', ( #22595, #65083, #812, #123104 ) ) ;
#42064 = EDGE_CURVE ( 'NONE', #42348, #92938, #90878, .T. ) ;
#42065 = CYLINDRICAL_SURFACE ( 'NONE', #23738, 6.000000000000000000 ) ;
#42066 = CARTESIAN_POINT ( 'NONE',  ( 13.92123647476855197, -9.717572351234235426E-16, -7.934999999999990727 ) ) ;
#42067 = VERTEX_POINT ( 'NONE', #102467 ) ;
#42068 = CARTESIAN_POINT ( 'NONE',  ( 88.28709685856478018, 3.054999999999997939, 5.291415217122920289 ) ) ;
#42069 = CARTESIAN_POINT ( 'NONE',  ( 10.32500000000000107, -8.432637487761466488, -4.375000000000001776 ) ) ;
#42070 = CARTESIAN_POINT ( 'NONE',  ( 55.18164086290597226, -49.14999999999998437, -41.64499999999999602 ) ) ;
#42071 = CARTESIAN_POINT ( 'NONE',  ( -27.70701326429286127, -21.74070752338406365, 4.999753212805221558 ) ) ;
#42072 = ORIENTED_EDGE ( 'NONE', *, *, #2329, .T. ) ;
#42073 = ORIENTED_EDGE ( 'NONE', *, *, #63865, .F. ) ;
#42074 = CARTESIAN_POINT ( 'NONE',  ( -12.70710678118646264, 14.25929247661557753, 5.000000000000000000 ) ) ;
#42075 = ORIENTED_EDGE ( 'NONE', *, *, #76609, .F. ) ;
#42076 = CARTESIAN_POINT ( 'NONE',  ( 33.72281430457037743, -21.72499999999999432, 5.000000000000000000 ) ) ;
#42077 = DIRECTION ( 'NONE',  ( -1.000000000000000000, -1.224606353822377258E-16, -0.000000000000000000 ) ) ;
#42078 = VECTOR ( 'NONE', #52576, 1000.000000000000000 ) ;
#42080 = DIRECTION ( 'NONE',  ( -0.6830127018922180770, -0.6830127018922204085, -0.2588190451025213501 ) ) ;
#42079 = CONICAL_SURFACE ( 'NONE', #18977, 2.055000000000000604, 0.9599310885968764806 ) ;
#42081 = CARTESIAN_POINT ( 'NONE',  ( 184.1383206845090967, -50.55966373067075637, -35.89041033429538885 ) ) ;
#42082 = ORIENTED_EDGE ( 'NONE', *, *, #48602, .F. ) ;
#42083 = AXIS2_PLACEMENT_3D ( 'NONE', #116197, #69143, #60420 ) ;
#42084 = CARTESIAN_POINT ( 'NONE',  ( -12.00548008471251293, 28.92564299267929684, 4.000000000000000000 ) ) ;
#42085 = VECTOR ( 'NONE', #76606, 999.9999999999998863 ) ;
#42086 = DIRECTION ( 'NONE',  ( 0.7071067811865487940, 0.7071067811865463515, -0.000000000000000000 ) ) ;
#42087 = DIRECTION ( 'NONE',  ( -0.5735764363510499342, -0.8191520442889891340, 0.000000000000000000 ) ) ;
#42088 = EDGE_CURVE ( 'NONE', #103220, #19931, #33321, .T. ) ;
#42089 = ORIENTED_EDGE ( 'NONE', *, *, #47697, .F. ) ;
#42090 = FACE_OUTER_BOUND ( 'NONE', #53604, .T. ) ;
#42091 = VECTOR ( 'NONE', #131765, 1000.000000000000227 ) ;
#42092 = COLOUR_RGB ( '', 0.66274510, 0.83137255, 0.94901961) ;
#42093 = AXIS2_PLACEMENT_3D ( 'NONE', #9104, #132414, #118626 ) ;
#42094 = DIRECTION ( 'NONE',  ( -0.7071067811865486830, -0.7071067811865464625, 0.000000000000000000 ) ) ;
#42096 = VERTEX_POINT ( 'NONE', #105289 ) ;
#42095 = MECHANICAL_DESIGN_GEOMETRIC_PRESENTATION_REPRESENTATION (  '', ( #55969 ), #81430 ) ;
#42098 = ORIENTED_EDGE ( 'NONE', *, *, #30948, .F. ) ;
#42097 = CARTESIAN_POINT ( 'NONE',  ( 0.07085943933670184325, -51.15040958483974975, -36.98623100868706359 ) ) ;
#42099 = ORIENTED_EDGE ( 'NONE', *, *, #52154, .T. ) ;
#42100 = PLANE ( 'NONE',  #130399 ) ;
#42101 = AXIS2_PLACEMENT_3D ( 'NONE', #3757, #113996, #61100 ) ;
#42102 = DIRECTION ( 'NONE',  ( 0.000000000000000000, 0.000000000000000000, -1.000000000000000000 ) ) ;
#42103 = ORIENTED_EDGE ( 'NONE', *, *, #24795, .T. ) ;
#42104 = FACE_OUTER_BOUND ( 'NONE', #24768, .T. ) ;
#42105 = EDGE_CURVE ( 'NONE', #30015, #119678, #37923, .T. ) ;
#42106 = DIRECTION ( 'NONE',  ( -0.000000000000000000, 0.3543493200069153248, 0.9351131265310292928 ) ) ;
#42107 = LINE ( 'NONE', #55113, #96992 ) ;
#42108 = DIRECTION ( 'NONE',  ( 0.7071067811865487940, 0.7071067811865463515, 0.000000000000000000 ) ) ;
#42109 = ADVANCED_FACE ( 'NONE', ( #103832 ), #70575, .F. ) ;
#42110 = PLANE ( 'NONE',  #28160 ) ;
#42111 = CARTESIAN_POINT ( 'NONE',  ( 46.50000000000000000, 0.000000000000000000, -7.950000000000000178 ) ) ;
#42112 = FACE_OUTER_BOUND ( 'NONE', #127242, .T. ) ;
#42113 = CARTESIAN_POINT ( 'NONE',  ( 2.994519915287485734, 28.92564299267940342, 4.000000000000000000 ) ) ;
#42114 = DIRECTION ( 'NONE',  ( -0.7071067811865486830, 0.7071067811865464625, 0.000000000000000000 ) ) ;
#42115 = LINE ( 'NONE', #140673, #108499 ) ;
#42116 = CARTESIAN_POINT ( 'NONE',  ( -4.499999999999966249, 19.46639925780206326, 5.000000000000000000 ) ) ;
#42117 = FACE_OUTER_BOUND ( 'NONE', #35501, .T. ) ;
#42118 = ORIENTED_EDGE ( 'NONE', *, *, #8812, .F. ) ;
#42119 = VECTOR ( 'NONE', #125995, 1000.000000000000000 ) ;
#42120 = ORIENTED_EDGE ( 'NONE', *, *, #10094, .T. ) ;
#42121 = ORIENTED_EDGE ( 'NONE', *, *, #104754, .F. ) ;
#42122 = CARTESIAN_POINT ( 'NONE',  ( 113.5833333333333428, 6.884901960086290629, -3.974999999999994316 ) ) ;
#42123 = VERTEX_POINT ( 'NONE', #137938 ) ;
#42124 = VERTEX_POINT ( 'NONE', #137224 ) ;
#42125 = EDGE_CURVE ( 'NONE', #143141, #30765, #113301, .T. ) ;
#42126 = VECTOR ( 'NONE', #2968, 1000.000000000000227 ) ;
#42127 = EDGE_LOOP ( 'NONE', ( #55082, #118621, #113287, #1835, #13489 ) ) ;
#42128 = DIRECTION ( 'NONE',  ( -0.000000000000000000, -0.3543493200069152693, 0.9351131265310292928 ) ) ;
#42129 = CARTESIAN_POINT ( 'NONE',  ( -45.18398860626900415, 28.73617430169818832, 5.000000000000000000 ) ) ;
#42130 = CONICAL_SURFACE ( 'NONE', #127804, 2.055000000000000604, 0.9599310885968764806 ) ;
#42131 = EDGE_LOOP ( 'NONE', ( #16153, #103782, #126978, #56509 ) ) ;
#42132 = LINE ( 'NONE', #64571, #53266 ) ;
#42133 = DIRECTION ( 'NONE',  ( -0.6830127018922180770, -0.6830127018922204085, -0.2588190451025213501 ) ) ;
#42134 = DIRECTION ( 'NONE',  ( 0.000000000000000000, -1.000000000000000000, 0.000000000000000000 ) ) ;
#42135 = CARTESIAN_POINT ( 'NONE',  ( 0.000000000000000000, 0.000000000000000000, 5.000000000000000000 ) ) ;
#42136 = CARTESIAN_POINT ( 'NONE',  ( 104.5629301918981184, 1.637169565754157174, 6.110000000000002984 ) ) ;
#42137 = EDGE_CURVE ( 'NONE', #52838, #5991, #135788, .T. ) ;
#42138 = ORIENTED_EDGE ( 'NONE', *, *, #27601, .T. ) ;
#42139 = CARTESIAN_POINT ( 'NONE',  ( 14.20335188619867672, 5.294102111022186641, -31.75876904902751718 ) ) ;
#42140 = FILL_AREA_STYLE_COLOUR ( '', #75213 ) ;
#42141 = FACE_OUTER_BOUND ( 'NONE', #92770, .T. ) ;
#42142 = CARTESIAN_POINT ( 'NONE',  ( -7.140000000000001457, -60.26999999999998892, -7.899272885403729738 ) ) ;
#42143 = CARTESIAN_POINT ( 'NONE',  ( 23.62500000000000355, 6.094999999999989981, -1.119633336120465690E-15 ) ) ;
#42144 = CARTESIAN_POINT ( 'NONE',  ( 22.82816939922337340, -5.240707523384230626, 4.000000000000000000 ) ) ;
#42145 = LINE ( 'NONE', #41396, #112281 ) ;
#42146 = DIRECTION ( 'NONE',  ( -0.7071067811865487940, 0.7071067811865463515, 0.000000000000000000 ) ) ;
#42147 = ORIENTED_EDGE ( 'NONE', *, *, #137017, .T. ) ;
#42148 = ORIENTED_EDGE ( 'NONE', *, *, #115004, .F. ) ;
#42149 = CARTESIAN_POINT ( 'NONE',  ( 27.54166666666665719, -3.975000000000002753, 6.884901960086286188 ) ) ;
#42150 = ORIENTED_EDGE ( 'NONE', *, *, #28407, .T. ) ;
#42151 = CARTESIAN_POINT ( 'NONE',  ( -13.35579869995845037, 22.22500000000000142, -3.173376671670978588 ) ) ;
#42152 = VECTOR ( 'NONE', #39107, 1000.000000000000227 ) ;
#42153 = LINE ( 'NONE', #76932, #22339 ) ;
#42154 = VECTOR ( 'NONE', #44433, 1000.000000000000000 ) ;
#42155 = CARTESIAN_POINT ( 'NONE',  ( -25.39999999999996305, 3.061616997868383141E-16, -2.500000000000000000 ) ) ;
#42156 = DIRECTION ( 'NONE',  ( 0.000000000000000000, -1.000000000000000000, 0.000000000000000000 ) ) ;
#42157 = DIRECTION ( 'NONE',  ( 0.7071067811865486830, -0.7071067811865464625, -0.000000000000000000 ) ) ;
#42158 = PLANE ( 'NONE',  #34955 ) ;
#42159 = CARTESIAN_POINT ( 'NONE',  ( 123.4329301918981088, 1.637169565754156508, 6.110000000000000320 ) ) ;
#42160 = ADVANCED_FACE ( 'NONE', ( #82849 ), #4485, .T. ) ;
#42161 = VERTEX_POINT ( 'NONE', #47405 ) ;
#42162 = DIRECTION ( 'NONE',  ( 0.7071067811865487940, 0.7071067811865463515, 0.000000000000000000 ) ) ;
#42163 = ORIENTED_EDGE ( 'NONE', *, *, #46748, .F. ) ;
#42164 = CARTESIAN_POINT ( 'NONE',  ( 69.93336038379619879, 2.130196079827431532, -7.949999999999996625 ) ) ;
#42165 = LINE ( 'NONE', #129144, #86062 ) ;
#42166 = CARTESIAN_POINT ( 'NONE',  ( -66.18398860626901126, 28.73617430169833753, 5.000000000000000000 ) ) ;
#42167 = VERTEX_POINT ( 'NONE', #36475 ) ;
#42168 = CARTESIAN_POINT ( 'NONE',  ( 50.45876352523143282, 0.000000000000000000, -6.110000000000001208 ) ) ;
#42169 = ORIENTED_EDGE ( 'NONE', *, *, #90649, .T. ) ;
#42170 = PLANE ( 'NONE',  #104964 ) ;
#42171 = EDGE_CURVE ( 'NONE', #100848, #96542, #80713, .T. ) ;
#42172 = LINE ( 'NONE', #31289, #25335 ) ;
#42173 = DIRECTION ( 'NONE',  ( -1.000000000000000000, -1.224606353822377258E-16, -0.000000000000000000 ) ) ;
#42174 = CARTESIAN_POINT ( 'NONE',  ( 66.28752705046289861, 0.000000000000000000, -7.949999999999998401 ) ) ;
#42175 =( BOUNDED_CURVE ( )  B_SPLINE_CURVE ( 2, ( #68181, #143543, #98605, #21770, #43519, #121773, #87741, #23163, #12308, #45001, #1411, #45696, #89865 ),
 .UNSPECIFIED., .F., .T. ) 
 B_SPLINE_CURVE_WITH_KNOTS ( ( 3, 2, 2, 2, 2, 2, 3 ),
 ( 0.1499999999999999944, 0.1527777777777777901, 0.1555555555555555580, 0.1583333333333333259, 0.1611111111111111216, 0.1638888888888888895, 0.1666666666666666574 ),
 .UNSPECIFIED. ) 
 CURVE ( )  GEOMETRIC_REPRESENTATION_ITEM ( )  RATIONAL_B_SPLINE_CURVE ( ( 1.000000000000000000, 0.9659258262890683122, 1.000000000000000000, 0.9659258262890683122, 1.000000000000000000, 0.9659258262890683122, 1.000000000000000000, 0.9659258262890683122, 1.000000000000000000, 0.9659258262890683122, 1.000000000000000000, 0.9659258262890683122, 1.000000000000000000 ) ) 
 REPRESENTATION_ITEM ( '' )  );
#42176 = CARTESIAN_POINT ( 'NONE',  ( 36.66209685856478018, -5.291415217122919401, 3.054999999999997939 ) ) ;
#42177 = ORIENTED_EDGE ( 'NONE', *, *, #8630, .T. ) ;
#42178 = CARTESIAN_POINT ( 'NONE',  ( 2.994519915287485734, 28.92564299267940342, 4.000000000000000000 ) ) ;
#42179 = EDGE_LOOP ( 'NONE', ( #47755, #4868, #9351, #97590 ) ) ;
#42180 = VERTEX_POINT ( 'NONE', #3791 ) ;
#42181 = VECTOR ( 'NONE', #66166, 999.9999999999998863 ) ;
#42182 = VECTOR ( 'NONE', #41697, 1000.000000000000000 ) ;
#42183 = ORIENTED_EDGE ( 'NONE', *, *, #136334, .T. ) ;
#42184 = VECTOR ( 'NONE', #7162, 1000.000000000000227 ) ;
#42185 = EDGE_CURVE ( 'NONE', #98878, #16866, #48075, .T. ) ;
#42186 = CARTESIAN_POINT ( 'NONE',  ( 2.207106781186528810, -8.240707523384198652, 5.000000000000000000 ) ) ;
#42187 = ORIENTED_EDGE ( 'NONE', *, *, #91524, .F. ) ;
#42188 = DIRECTION ( 'NONE',  ( -0.000000000000000000, 0.3543493200069153248, 0.9351131265310292928 ) ) ;
#42189 = VECTOR ( 'NONE', #132184, 999.9999999999998863 ) ;
#42190 = VECTOR ( 'NONE', #98273, 1000.000000000000000 ) ;
#42191 = VECTOR ( 'NONE', #28624, 1000.000000000000000 ) ;
#42192 = CARTESIAN_POINT ( 'NONE',  ( -34.92500000000001137, -22.22500000000000142, 4.000000000000000000 ) ) ;
#42193 = DIRECTION ( 'NONE',  ( 0.6830127018922181881, 0.6830127018922202975, -0.2588190451025214056 ) ) ;
#42194 = FACE_BOUND ( 'NONE', #35019, .T. ) ;
#42195 = EDGE_LOOP ( 'NONE', ( #113873, #88876, #4365, #108235 ) ) ;
#42196 = DIRECTION ( 'NONE',  ( -0.7071067811865486830, 0.7071067811865464625, 0.000000000000000000 ) ) ;
#42197 = CARTESIAN_POINT ( 'NONE',  ( -31.66020301277962190, -22.22500000000000142, 6.237153622978027556 ) ) ;
#42198 = VERTEX_POINT ( 'NONE', #15392 ) ;
#42199 = CARTESIAN_POINT ( 'NONE',  ( 4.898587196589412829E-16, -9.500000000000000000, -4.000000000000000000 ) ) ;
#42200 = ORIENTED_EDGE ( 'NONE', *, *, #50259, .T. ) ;
#42201 = VERTEX_POINT ( 'NONE', #92995 ) ;
#42202 = FACE_OUTER_BOUND ( 'NONE', #53171, .T. ) ;
#42203 = ORIENTED_EDGE ( 'NONE', *, *, #120341, .T. ) ;
#42204 = EDGE_CURVE ( 'NONE', #33831, #120928, #19703, .T. ) ;
#42205 = CARTESIAN_POINT ( 'NONE',  ( 58.24543019189810877, -5.291415217122918513, -3.055000000000000160 ) ) ;
#42206 = EDGE_LOOP ( 'NONE', ( #10905, #94532, #99044, #14744 ) ) ;
#42207 = PLANE ( 'NONE',  #120494 ) ;
#42208 = EDGE_CURVE ( 'NONE', #73777, #45804, #65720, .T. ) ;
#42209 = CARTESIAN_POINT ( 'NONE',  ( 48.48921356237309510, -27.52281430457089328, 5.000000000000000000 ) ) ;
#42210 = ORIENTED_EDGE ( 'NONE', *, *, #20982, .F. ) ;
#42211 = ADVANCED_FACE ( 'NONE', ( #63263 ), #97235, .F. ) ;
#42212 = CARTESIAN_POINT ( 'NONE',  ( 63.18398860626900415, 28.73617430169831621, 5.000000000000000000 ) ) ;
#42213 = CARTESIAN_POINT ( 'NONE',  ( 0.000000000000000000, 0.000000000000000000, 5.000000000000000000 ) ) ;
#42214 = ADVANCED_FACE ( 'NONE', ( #62527 ), #108115, .F. ) ;
#42215 = AXIS2_PLACEMENT_3D ( 'NONE', #122051, #44559, #38458 ) ;
#42216 = CONICAL_SURFACE ( 'NONE', #23336, 2.500000000000000888, 0.9599310885968822538 ) ;
#42217 = CARTESIAN_POINT ( 'NONE',  ( 24.41159235450331977, -2.500000000000000000, 3.061616997868384127E-16 ) ) ;
#42218 = CARTESIAN_POINT ( 'NONE',  ( -19.93618820137057668, -0.2700000000508183118, 500000.0000000000582 ) ) ;
#42219 = CARTESIAN_POINT ( 'NONE',  ( 19.10840764549667270, 2.500000000000003553, 3.061616997868386099E-16 ) ) ;
#42220 = CARTESIAN_POINT ( 'NONE',  ( 11.99999999999992717, -19.44781430457064175, 5.000000000000000000 ) ) ;
#42221 = DIRECTION ( 'NONE',  ( 0.000000000000000000, 0.000000000000000000, -1.000000000000000000 ) ) ;
#42222 = VERTEX_POINT ( 'NONE', #73400 ) ;
#42223 = VERTEX_POINT ( 'NONE', #28468 ) ;
#42224 = EDGE_LOOP ( 'NONE', ( #49672, #80623, #5438, #97425, #77802, #68324 ) ) ;
#42225 = VECTOR ( 'NONE', #130398, 1000.000000000000000 ) ;
#42226 = DIRECTION ( 'NONE',  ( 0.7071067811865486830, -0.7071067811865464625, -0.000000000000000000 ) ) ;
#42227 = CARTESIAN_POINT ( 'NONE',  ( -31.17183060077625356, -14.24070752338413648, 4.000000000000000000 ) ) ;
#42228 = EDGE_LOOP ( 'NONE', ( #37180, #103985, #54460, #42902 ) ) ;
#42229 = VERTEX_POINT ( 'NONE', #118293 ) ;
#42230 = EDGE_LOOP ( 'NONE', ( #3315, #84858, #130824, #126774 ) ) ;
#42231 = PLANE ( 'NONE',  #106865 ) ;
#42233 = EDGE_CURVE ( 'NONE', #143133, #57179, #72730, .T. ) ;
#42232 = DIRECTION ( 'NONE',  ( -0.7071067811865486830, 0.7071067811865464625, 0.000000000000000000 ) ) ;
#42234 = EDGE_CURVE ( 'NONE', #118451, #19758, #50217, .T. ) ;
#42235 = CARTESIAN_POINT ( 'NONE',  ( 0.000000000000000000, 0.000000000000000000, 5.000000000000000000 ) ) ;
#42236 = ORIENTED_EDGE ( 'NONE', *, *, #117786, .T. ) ;
#42237 = DIRECTION ( 'NONE',  ( 1.000000000000000000, -0.000000000000000000, 0.000000000000000000 ) ) ;
#42238 = MECHANICAL_DESIGN_GEOMETRIC_PRESENTATION_REPRESENTATION (  '', ( #74625 ), #25972 ) ;
#42239 = EDGE_CURVE ( 'NONE', #124916, #116175, #141500, .T. ) ;
#42240 = DIRECTION ( 'NONE',  ( 0.6830127018922180770, -0.6830127018922204085, -0.2588190451025213501 ) ) ;
#42241 = CARTESIAN_POINT ( 'NONE',  ( 15.08790314143521982, 6.871911579029515771, 3.967499999999989146 ) ) ;
#42242 = DIRECTION ( 'NONE',  ( -1.451651444332056451E-15, -1.000000000000000000, 0.000000000000000000 ) ) ;
#42243 = EDGE_LOOP ( 'NONE', ( #45741, #125222, #76864, #62332 ) ) ;
#42244 = CARTESIAN_POINT ( 'NONE',  ( 124.7454301918981230, -5.291415217122919401, -3.055000000000000604 ) ) ;
#42245 = DIRECTION ( 'NONE',  ( -0.7071067811865486830, -0.7071067811865464625, 0.000000000000000000 ) ) ;
#42246 = AXIS2_PLACEMENT_3D ( 'NONE', #116324, #17014, #72875 ) ;
#42247 = LINE ( 'NONE', #85007, #130609 ) ;
#42248 = ADVANCED_FACE ( 'NONE', ( #42202 ), #140088, .F. ) ;
#42250 = VERTEX_POINT ( 'NONE', #130645 ) ;
#42249 = DIRECTION ( 'NONE',  ( -0.000000000000000000, -0.3543493200069152693, 0.9351131265310292928 ) ) ;
#42251 = DIRECTION ( 'NONE',  ( 1.000000000000000000, 0.000000000000000000, 0.000000000000000000 ) ) ;
#42252 = ORIENTED_EDGE ( 'NONE', *, *, #121714, .F. ) ;
#42253 = LINE ( 'NONE', #31362, #107501 ) ;
#42254 = CARTESIAN_POINT ( 'NONE',  ( 20.67906569311139009, -2.055000000000000160, 0.000000000000000000 ) ) ;
#42255 = FACE_OUTER_BOUND ( 'NONE', #133150, .T. ) ;
#42256 = EDGE_LOOP ( 'NONE', ( #59570, #14217, #8769, #76568 ) ) ;
#42257 = DIRECTION ( 'NONE',  ( 0.3543493200069162685, -0.000000000000000000, -0.9351131265310288487 ) ) ;
#42258 = LINE ( 'NONE', #117615, #120772 ) ;
#42259 = ADVANCED_FACE ( 'NONE', ( #40767 ), #127781, .F. ) ;
#42260 = ORIENTED_EDGE ( 'NONE', *, *, #21727, .T. ) ;
#42261 = VECTOR ( 'NONE', #41595, 999.9999999999998863 ) ;
#42262 = DIRECTION ( 'NONE',  ( -1.000000000000000000, -1.224606353822377258E-16, -0.000000000000000000 ) ) ;
#42263 = DIRECTION ( 'NONE',  ( -0.000000000000000000, 0.3543493200069153248, 0.9351131265310292928 ) ) ;
#42264 = ORIENTED_EDGE ( 'NONE', *, *, #48068, .F. ) ;
#42265 = CARTESIAN_POINT ( 'NONE',  ( 4.666666666666666963, -5.278424836066145431, -3.047499999999993658 ) ) ;
#42266 = CARTESIAN_POINT ( 'NONE',  ( -20.99999999999985079, 10.93112307739207445, 4.000000000000000000 ) ) ;
#42267 = EDGE_LOOP ( 'NONE', ( #13562, #97727, #133419, #43961 ) ) ;
#42268 = ORIENTED_EDGE ( 'NONE', *, *, #64450, .F. ) ;
#42269 = AXIS2_PLACEMENT_3D ( 'NONE', #66732, #86354, #75472 ) ;
#42270 = CYLINDRICAL_SURFACE ( 'NONE', #10212, 0.5000000000000004441 ) ;
#42271 = CARTESIAN_POINT ( 'NONE',  ( -34.92500000000001137, 21.72500000000000142, 5.000000000000000000 ) ) ;
#42272 = EDGE_CURVE ( 'NONE', #76593, #116708, #20402, .T. ) ;
#42273 = CARTESIAN_POINT ( 'NONE',  ( 10.47873647476855119, -5.808823158059033709, 5.808823158059035485 ) ) ;
#42274 = SURFACE_STYLE_FILL_AREA ( #44426 ) ;
#42275 = CYLINDRICAL_SURFACE ( 'NONE', #108582, 0.5000000000000004441 ) ;
#42276 = CARTESIAN_POINT ( 'NONE',  ( -34.42500000000001137, -9.022814304570477617, 5.000000000000000000 ) ) ;
#42277 = VERTEX_POINT ( 'NONE', #94407 ) ;
#42278 =( NAMED_UNIT ( * ) PLANE_ANGLE_UNIT ( ) SI_UNIT ( $, .RADIAN. ) );
#42279 = CARTESIAN_POINT ( 'NONE',  ( -34.92500000000001137, 22.22500000000000142, 4.000000000000000000 ) ) ;
#42280 = CYLINDRICAL_SURFACE ( 'NONE', #37864, 2.500000000000000000 ) ;
#42281 = AXIS2_PLACEMENT_3D ( 'NONE', #81880, #126073, #84016 ) ;
#42282 = VECTOR ( 'NONE', #129405, 1000.000000000000227 ) ;
#42283 = VECTOR ( 'NONE', #58266, 1000.000000000000000 ) ;
#42284 = CARTESIAN_POINT ( 'NONE',  ( 8.719980320105909399, 0.7592924766157104211, 14.27032725228010968 ) ) ;
#42285 = CARTESIAN_POINT ( 'NONE',  ( 36.07876352523144448, -7.482591942790327058E-16, 6.109999999999999432 ) ) ;
#42286 = DIRECTION ( 'NONE',  ( 0.7071067811865487940, 0.7071067811865463515, 0.000000000000000000 ) ) ;
#42287 = VECTOR ( 'NONE', #37966, 1000.000000000000000 ) ;
#42288 = VECTOR ( 'NONE', #42745, 1000.000000000000000 ) ;
#42289 = ORIENTED_EDGE ( 'NONE', *, *, #7630, .T. ) ;
#42290 = ORIENTED_EDGE ( 'NONE', *, *, #117760, .F. ) ;
#42291 = PLANE ( 'NONE',  #83541 ) ;
#42292 = ORIENTED_EDGE ( 'NONE', *, *, #9344, .T. ) ;
#42293 = EDGE_CURVE ( 'NONE', #74842, #117708, #29158, .T. ) ;
#42294 = ORIENTED_EDGE ( 'NONE', *, *, #53156, .T. ) ;
#42295 = AXIS2_PLACEMENT_3D ( 'NONE', #74049, #118236, #18948 ) ;
#42296 = VECTOR ( 'NONE', #61917, 1000.000000000000000 ) ;
#42297 = CARTESIAN_POINT ( 'NONE',  ( -3.888376381052390141, 9.759292476615621936, 17.35367589129214139 ) ) ;
#42298 = LINE ( 'NONE', #140845, #25319 ) ;
#42299 = ORIENTED_EDGE ( 'NONE', *, *, #104713, .T. ) ;
#42300 = LINE ( 'NONE', #64742, #74376 ) ;
#42301 = DIRECTION ( 'NONE',  ( -0.3543493200069162685, -0.000000000000000000, -0.9351131265310288487 ) ) ;
#42302 = CARTESIAN_POINT ( 'NONE',  ( -1.499999999999980460, 13.46639925780212721, 5.000000000000000000 ) ) ;
#42303 = CARTESIAN_POINT ( 'NONE',  ( -11.99999999999991296, -6.033600742197678279, 5.000000000000000000 ) ) ;
#42304 = EDGE_CURVE ( 'NONE', #111726, #27599, #74102, .T. ) ;
#42305 = ORIENTED_EDGE ( 'NONE', *, *, #106018, .F. ) ;
#42306 = PLANE ( 'NONE',  #60348 ) ;
#42307 = CARTESIAN_POINT ( 'NONE',  ( 36.48921356237310221, -27.52281430457080802, 5.000000000000000000 ) ) ;
#42308 = DIRECTION ( 'NONE',  ( -0.000000000000000000, 0.3543493200069153248, 0.9351131265310292928 ) ) ;
#42309 = DIRECTION ( 'NONE',  ( 1.000000000000000000, 1.224606353822377258E-16, 0.000000000000000000 ) ) ;
#42310 = LINE ( 'NONE', #40181, #56715 ) ;
#42311 =( NAMED_UNIT ( * ) PLANE_ANGLE_UNIT ( ) SI_UNIT ( $, .RADIAN. ) );
#42312 = FACE_OUTER_BOUND ( 'NONE', #108508, .T. ) ;
#42313 = CARTESIAN_POINT ( 'NONE',  ( 59.28752705046289151, 0.000000000000000000, -7.949999999999998401 ) ) ;
#42315 = LINE ( 'NONE', #98105, #127153 ) ;
#42314 = AXIS2_PLACEMENT_3D ( 'NONE', #124272, #23526, #79395 ) ;
#42316 = ORIENTED_EDGE ( 'NONE', *, *, #14229, .T. ) ;
#42317 = ORIENTED_EDGE ( 'NONE', *, *, #24707, .T. ) ;
#42318 = CARTESIAN_POINT ( 'NONE',  ( 58.16666666666665719, 6.884901960086285300, 3.975000000000003642 ) ) ;
#42319 = LINE ( 'NONE', #113064, #16878 ) ;
#42320 = CARTESIAN_POINT ( 'NONE',  ( 1.499999999999987566, -6.839392718269127869, -8.480912228396089603 ) ) ;
#42321 = PLANE ( 'NONE',  #117905 ) ;
#42322 = VERTEX_POINT ( 'NONE', #129902 ) ;
#42323 = CARTESIAN_POINT ( 'NONE',  ( -8.916851932270635217, 21.75929247661549581, 7.311836541448030857 ) ) ;
#42324 = CARTESIAN_POINT ( 'NONE',  ( 46.81293019189811133, -1.637169565754159617, -6.110000000000001208 ) ) ;
#42325 = EDGE_CURVE ( 'NONE', #94991, #128697, #84971, .T. ) ;
#42326 = VECTOR ( 'NONE', #141922, 999.9999999999998863 ) ;
#42327 = VERTEX_POINT ( 'NONE', #116881 ) ;
#42328 = DIRECTION ( 'NONE',  ( 0.7071067811865487940, -0.7071067811865463515, 0.000000000000000000 ) ) ;
#42329 = VERTEX_POINT ( 'NONE', #17553 ) ;
#42330 = ORIENTED_EDGE ( 'NONE', *, *, #10111, .T. ) ;
#42331 = AXIS2_PLACEMENT_3D ( 'NONE', #85994, #107021, #127351 ) ;
#42332 = CARTESIAN_POINT ( 'NONE',  ( -69.48921356237309510, -27.52281430457103895, 5.000000000000000000 ) ) ;
#42333 = CARTESIAN_POINT ( 'NONE',  ( -51.29974487139158867, -27.71228299555242103, 4.000000000000000000 ) ) ;
#42334 = PLANE ( 'NONE',  #97538 ) ;
#42335 = DIRECTION ( 'NONE',  ( 0.7071067811865486830, -0.7071067811865464625, -0.000000000000000000 ) ) ;
#42337 = ADVANCED_FACE ( 'NONE', ( #61819 ), #105976, .T. ) ;
#42336 = ORIENTED_EDGE ( 'NONE', *, *, #47798, .T. ) ;
#42338 = LINE ( 'NONE', #43046, #65091 ) ;
#42340 = ORIENTED_EDGE ( 'NONE', *, *, #128585, .T. ) ;
#42339 = DIRECTION ( 'NONE',  ( 0.000000000000000000, 1.000000000000000000, 0.000000000000000000 ) ) ;
#42341 = CARTESIAN_POINT ( 'NONE',  ( 84.14626352523144703, -4.472830434245840259, 4.472830434245838482 ) ) ;
#42342 = EDGE_CURVE ( 'NONE', #110737, #2187, #40077, .T. ) ;
#42343 = CARTESIAN_POINT ( 'NONE',  ( 12.15612307739233344, -22.22500000000000142, 4.000000000000000000 ) ) ;
#42344 = CARTESIAN_POINT ( 'NONE',  ( 3.489213562373097322, -27.52281430457057709, 5.000000000000000000 ) ) ;
#42345 = FILL_AREA_STYLE ('',( #8911 ) ) ;
#42346 = CARTESIAN_POINT ( 'NONE',  ( -20.99451991528748707, 28.92564299267952777, 4.000000000000000000 ) ) ;
#42347 = LINE ( 'NONE', #88702, #2183 ) ;
#42348 = VERTEX_POINT ( 'NONE', #129174 ) ;
#42349 = CARTESIAN_POINT ( 'NONE',  ( 88.16252705046289861, 7.949999999999998401, 1.460391307983218338E-15 ) ) ;
#42350 = CARTESIAN_POINT ( 'NONE',  ( 63.78709685856477307, 3.054999999999997495, 5.291415217122919401 ) ) ;
#42351 = MANIFOLD_SOLID_BREP ( 'ThdSchPat', #60289 ) ;
#42352 = PLANE ( 'NONE',  #83474 ) ;
#42353 = AXIS2_PLACEMENT_3D ( 'NONE', #46126, #57009, #1140 ) ;
#42354 = DIRECTION ( 'NONE',  ( -0.7071067811865487940, 0.7071067811865463515, -0.000000000000000000 ) ) ;
#42355 = FACE_OUTER_BOUND ( 'NONE', #91364, .T. ) ;
#42356 = ORIENTED_EDGE ( 'NONE', *, *, #1248, .F. ) ;
#42357 = VERTEX_POINT ( 'NONE', #120408 ) ;
#42358 = AXIS2_PLACEMENT_3D ( 'NONE', #125188, #80283, #4777 ) ;
#42359 = CARTESIAN_POINT ( 'NONE',  ( -53.99451991528749062, 28.92564299267975869, 4.000000000000000000 ) ) ;
#42360 = ORIENTED_EDGE ( 'NONE', *, *, #9284, .F. ) ;
#42361 = EDGE_CURVE ( 'NONE', #56805, #108692, #51, .T. ) ;
#42362 = EDGE_LOOP ( 'NONE', ( #134533, #69314, #136090, #52131 ) ) ;
#42363 = LINE ( 'NONE', #119859, #35194 ) ;
#42364 = ORIENTED_EDGE ( 'NONE', *, *, #69089, .T. ) ;
#42365 = DIRECTION ( 'NONE',  ( 0.6830127018922180770, -0.6830127018922204085, -0.2588190451025213501 ) ) ;
#42366 = CARTESIAN_POINT ( 'NONE',  ( 9.792893218813397027, -14.24070752338413648, 5.000000000000000000 ) ) ;
#42367 = VECTOR ( 'NONE', #87610, 1000.000000000000000 ) ;
#42368 = CARTESIAN_POINT ( 'NONE',  ( -34.42500000000001137, -15.02281430457042077, 5.000000000000000000 ) ) ;
#42369 = FACE_BOUND ( 'NONE', #25276, .T. ) ;
#42370 = DIRECTION ( 'NONE',  ( 0.000000000000000000, 0.000000000000000000, 1.000000000000000000 ) ) ;
#42371 = CARTESIAN_POINT ( 'NONE',  ( 21.29974487139158512, -27.71228299555221142, 4.000000000000000000 ) ) ;
#42372 = VECTOR ( 'NONE', #33940, 1000.000000000000000 ) ;
#42373 = DIRECTION ( 'NONE',  ( 0.7071067811865487940, -0.7071067811865463515, 0.000000000000000000 ) ) ;
#42375 = ORIENTED_EDGE ( 'NONE', *, *, #45403, .T. ) ;
#42374 = DIRECTION ( 'NONE',  ( 1.000000000000000000, 0.000000000000000000, -0.000000000000000000 ) ) ;
#42376 = DIRECTION ( 'NONE',  ( -1.000000000000000000, 0.000000000000000000, 0.000000000000000000 ) ) ;
#42377 = ITEM_DEFINED_TRANSFORMATION ( 'NONE', 'NONE', #67881,  #127880 ) ;
#42378 = ORIENTED_EDGE ( 'NONE', *, *, #139300, .T. ) ;
#42380 = ORIENTED_EDGE ( 'NONE', *, *, #142809, .F. ) ;
#42379 = ADVANCED_FACE ( 'NONE', ( #81071 ), #87114, .F. ) ;
#42381 = CARTESIAN_POINT ( 'NONE',  ( 87.70376352523146579, 6.109999999999998543, 1.122388791418548911E-15 ) ) ;
#42382 = VERTEX_POINT ( 'NONE', #57908 ) ;
#42383 = DIRECTION ( 'NONE',  ( -0.000000000000000000, 0.3543493200069153248, 0.9351131265310292928 ) ) ;
#42384 = DIRECTION ( 'NONE',  ( 0.7071067811865487940, -0.7071067811865463515, 0.000000000000000000 ) ) ;
#42385 = EDGE_CURVE ( 'NONE', #3140, #97576, #51818, .T. ) ;
#42386 = VERTEX_POINT ( 'NONE', #131332 ) ;
#42387 = FACE_OUTER_BOUND ( 'NONE', #99896, .T. ) ;
#42388 = AXIS2_PLACEMENT_3D ( 'NONE', #37248, #14045, #80769 ) ;
#42389 = EDGE_CURVE ( 'NONE', #63176, #133299, #54120, .T. ) ;
#42391 = EDGE_CURVE ( 'NONE', #46293, #1659, #21134, .T. ) ;
#42390 = AXIS2_PLACEMENT_3D ( 'NONE', #47972, #103713, #35681 ) ;
#42392 = CIRCLE ( 'NONE', #53985, 2.055000000000000604 ) ;
#42393 = PLANE ( 'NONE',  #84265 ) ;
#42394 = PLANE ( 'NONE',  #103925 ) ;
#42395 = CARTESIAN_POINT ( 'NONE',  ( -11.18650864602353678, -15.74070752338411694, 8.904080028138968927 ) ) ;
#42396 = LINE ( 'NONE', #98184, #126889 ) ;
#42397 = FACE_OUTER_BOUND ( 'NONE', #81059, .T. ) ;
#42398 = CARTESIAN_POINT ( 'NONE',  ( -22.49999999999983302, 19.08746187583905041, 4.000000000000000000 ) ) ;
#42399 = ORIENTED_EDGE ( 'NONE', *, *, #103290, .F. ) ;
#42400 = VECTOR ( 'NONE', #70955, 999.9999999999998863 ) ;
#42401 = VECTOR ( 'NONE', #100609, 1000.000000000000000 ) ;
#42402 = AXIS2_PLACEMENT_3D ( 'NONE', #55556, #45410, #91051 ) ;
#42403 = FACE_OUTER_BOUND ( 'NONE', #54813, .T. ) ;
#42404 = ORIENTED_EDGE ( 'NONE', *, *, #140993, .T. ) ;
#42405 = FACE_OUTER_BOUND ( 'NONE', #78886, .T. ) ;
#42406 = CARTESIAN_POINT ( 'NONE',  ( -1.171830600776461617, 15.75929247661555443, 4.000000000000000000 ) ) ;
#42407 = EDGE_LOOP ( 'NONE', ( #41300, #89772, #14942, #117831 ) ) ;
#42408 = EDGE_LOOP ( 'NONE', ( #66180, #25062, #71220, #29971 ) ) ;
#42409 = EDGE_CURVE ( 'NONE', #99416, #5794, #47749, .T. ) ;
#42411 = ORIENTED_EDGE ( 'NONE', *, *, #236, .F. ) ;
#42410 = EDGE_CURVE ( 'NONE', #111848, #110816, #30919, .T. ) ;
#42412 = CARTESIAN_POINT ( 'NONE',  ( 37.04209685856476852, 5.291415217122923842, -3.054999999999996163 ) ) ;
#42413 = ORIENTED_EDGE ( 'NONE', *, *, #63832, .F. ) ;
#42414 = CARTESIAN_POINT ( 'NONE',  ( -6.005480084712508493, 28.92564299267933947, 4.000000000000000000 ) ) ;
#42415 = LINE ( 'NONE', #120631, #125696 ) ;
#42416 = VECTOR ( 'NONE', #79216, 1000.000000000000227 ) ;
#42417 = CARTESIAN_POINT ( 'NONE',  ( 26.29580628287044064, -5.278424836066144543, 3.047499999999995879 ) ) ;
#42418 = CARTESIAN_POINT ( 'NONE',  ( -3.802034438261828964, 13.42402838347469007, -24.61607834315348953 ) ) ;
#42419 = EDGE_CURVE ( 'NONE', #74460, #3311, #136138, .T. ) ;
#42420 = ORIENTED_EDGE ( 'NONE', *, *, #52586, .T. ) ;
#42421 = EDGE_LOOP ( 'NONE', ( #65163, #105106, #106884, #37094 ) ) ;
#42422 = CARTESIAN_POINT ( 'NONE',  ( 27.22000000000000242, 9.521314400968980422E-16, 0.000000000000000000 ) ) ;
#42423 = CARTESIAN_POINT ( 'NONE',  ( -34.42500000000001137, -21.72500000000000142, 5.000000000000000000 ) ) ;
#42424 = EDGE_CURVE ( 'NONE', #102767, #63264, #33480, .T. ) ;
#42426 = ORIENTED_EDGE ( 'NONE', *, *, #5336, .F. ) ;
#42425 = LINE ( 'NONE', #31524, #130477 ) ;
#42427 = VERTEX_POINT ( 'NONE', #87821 ) ;
#42428 = CARTESIAN_POINT ( 'NONE',  ( 115.1416937171295558, -2.130196079827424871, -7.949999999999998401 ) ) ;
#42429 = CARTESIAN_POINT ( 'NONE',  ( -0.4892135623730947680, -27.52281430457055578, 5.000000000000000000 ) ) ;
#42430 = VECTOR ( 'NONE', #58672, 1000.000000000000000 ) ;
#42431 = LINE ( 'NONE', #96734, #79611 ) ;
#42432 = ORIENTED_EDGE ( 'NONE', *, *, #142516, .T. ) ;
#42433 = DIRECTION ( 'NONE',  ( 0.7071067811865487940, 0.7071067811865463515, 0.000000000000000000 ) ) ;
#42434 = VERTEX_POINT ( 'NONE', #132063 ) ;
#42435 = ORIENTED_EDGE ( 'NONE', *, *, #96256, .T. ) ;
#42436 = VECTOR ( 'NONE', #142452, 999.9999999999998863 ) ;
#42437 = VERTEX_POINT ( 'NONE', #77681 ) ;
#42438 = CARTESIAN_POINT ( 'NONE',  ( -34.49999999999975131, -5.568876922607759461, 4.000000000000000000 ) ) ;
#42439 = EDGE_CURVE ( 'NONE', #68775, #81209, #66093, .T. ) ;
#42440 = CARTESIAN_POINT ( 'NONE',  ( -2.207106781186522149, 12.75929247661559351, 5.000000000000000000 ) ) ;
#42441 = PRESENTATION_STYLE_ASSIGNMENT (( #99625 ) ) ;
#42442 =( BOUNDED_CURVE ( )  B_SPLINE_CURVE ( 3, ( #89602, #11292, #133833, #78743 ),
 .UNSPECIFIED., .F., .T. ) 
 B_SPLINE_CURVE_WITH_KNOTS ( ( 4, 4 ),
 ( 1.208578181583226385, 1.359146454359472678 ),
 .UNSPECIFIED. ) 
 CURVE ( )  GEOMETRIC_REPRESENTATION_ITEM ( )  RATIONAL_B_SPLINE_CURVE ( ( 1.000000000000000000, 0.9981116584018941973, 0.9981116584018941973, 1.000000000000000000 ) ) 
 REPRESENTATION_ITEM ( '' )  );
#42444 = VECTOR ( 'NONE', #114093, 1000.000000000000227 ) ;
#42443 = DIRECTION ( 'NONE',  ( -0.7071067811865486830, 0.7071067811865464625, 0.000000000000000000 ) ) ;
#42445 = DIRECTION ( 'NONE',  ( -0.000000000000000000, -0.3543493200069152693, 0.9351131265310292928 ) ) ;
#42446 = CARTESIAN_POINT ( 'NONE',  ( -27.70710678118634718, 8.259292476615637923, 5.000000000000000000 ) ) ;
#42447 = ORIENTED_EDGE ( 'NONE', *, *, #53692, .F. ) ;
#42448 = PLANE ( 'NONE',  #7220 ) ;
#42449 = EDGE_CURVE ( 'NONE', #116046, #106721, #21688, .T. ) ;
#42450 = ORIENTED_EDGE ( 'NONE', *, *, #87905, .T. ) ;
#42451 = EDGE_CURVE ( 'NONE', #135769, #104204, #102818, .T. ) ;
#42452 = CARTESIAN_POINT ( 'NONE',  ( -34.49999999999975131, -19.53574439159930876, 4.994342998332169437 ) ) ;
#42453 = VECTOR ( 'NONE', #37818, 1000.000000000000000 ) ;
#42454 = ADVANCED_FACE ( 'NONE', ( #142232 ), #108830, .T. ) ;
#42455 = DIRECTION ( 'NONE',  ( -0.7071067811865486830, -0.7071067811865464625, 0.000000000000000000 ) ) ;
#42457 = EDGE_LOOP ( 'NONE', ( #80928, #100571, #115681, #91832, #117669, #58654 ) ) ;
#42456 = VECTOR ( 'NONE', #53278, 1000.000000000000000 ) ;
#42458 = DIRECTION ( 'NONE',  ( -0.000000000000000000, 0.000000000000000000, 1.000000000000000000 ) ) ;
#42459 = DIRECTION ( 'NONE',  ( 0.7071067811865486830, -0.7071067811865464625, -0.000000000000000000 ) ) ;
#42460 = ORIENTED_EDGE ( 'NONE', *, *, #44490, .T. ) ;
#42461 = VERTEX_POINT ( 'NONE', #116534 ) ;
#42462 = CARTESIAN_POINT ( 'NONE',  ( 55.47138350052870948, -49.14501756083438266, 40.36361034346624876 ) ) ;
#42463 = LINE ( 'NONE', #41002, #34954 ) ;
#42464 = DIRECTION ( 'NONE',  ( 0.6830127018922180770, -0.6830127018922204085, -0.2588190451025213501 ) ) ;
#42465 = VECTOR ( 'NONE', #72109, 1000.000000000000000 ) ;
#42466 = CARTESIAN_POINT ( 'NONE',  ( 72.29974487139158157, -27.71228299555256669, 4.000000000000000000 ) ) ;
#42467 = EDGE_CURVE ( 'NONE', #134528, #104985, #4864, .T. ) ;
#42468 = LINE ( 'NONE', #98935, #57488 ) ;
#42469 = CARTESIAN_POINT ( 'NONE',  ( 65.39126352523145158, -4.472830434245839371, -4.472830434245839371 ) ) ;
#42470 = CARTESIAN_POINT ( 'NONE',  ( 12.40000000000000213, 9.521314400968980422E-16, 0.000000000000000000 ) ) ;
#42471 = DIRECTION ( 'NONE',  ( -0.7071067811865487940, 0.7071067811865463515, 0.000000000000000000 ) ) ;
#42472 = LINE ( 'NONE', #76519, #122882 ) ;
#42473 = ORIENTED_EDGE ( 'NONE', *, *, #30580, .F. ) ;
#42474 = CARTESIAN_POINT ( 'NONE',  ( -34.49999999999975131, 7.087461875839177416, 4.000000000000000000 ) ) ;
#42475 = ORIENTED_EDGE ( 'NONE', *, *, #44883, .T. ) ;
#42476 = VECTOR ( 'NONE', #116400, 1000.000000000000000 ) ;
#42477 = DIRECTION ( 'NONE',  ( -0.000000000000000000, 0.000000000000000000, 1.000000000000000000 ) ) ;
#42478 = ORIENTED_EDGE ( 'NONE', *, *, #98170, .F. ) ;
#42479 = DIRECTION ( 'NONE',  ( -0.7071067811865487940, 0.7071067811865463515, 0.000000000000000000 ) ) ;
#42481 = EDGE_LOOP ( 'NONE', ( #77519, #139280, #125484, #75619 ) ) ;
#42480 = DIRECTION ( 'NONE',  ( -0.6830127018922180770, -0.6830127018922204085, -0.2588190451025213501 ) ) ;
#42482 = FACE_OUTER_BOUND ( 'NONE', #18176, .T. ) ;
#42483 = DIRECTION ( 'NONE',  ( -0.3543493200069162685, -0.000000000000000000, -0.9351131265310288487 ) ) ;
#42484 = DIRECTION ( 'NONE',  ( 0.7071067811865487940, 0.7071067811865463515, 0.000000000000000000 ) ) ;
#42485 = EDGE_LOOP ( 'NONE', ( #142236, #16434, #84280, #118538 ) ) ;
#42487 = VERTEX_POINT ( 'NONE', #60776 ) ;
#42486 = VECTOR ( 'NONE', #108411, 1000.000000000000000 ) ;
#42488 = LINE ( 'NONE', #32305, #134325 ) ;
#42489 = CARTESIAN_POINT ( 'NONE',  ( 24.70710678118637205, 8.259292476615627265, 5.000000000000000000 ) ) ;
#42490 = CARTESIAN_POINT ( 'NONE',  ( -12.69999999999998153, 0.000000000000000000, 0.000000000000000000 ) ) ;
#42491 = LINE ( 'NONE', #83289, #18166 ) ;
#42492 = CARTESIAN_POINT ( 'NONE',  ( 83.49586038379622721, -3.974999999999998312, -6.884901960086286188 ) ) ;
#42493 = DIRECTION ( 'NONE',  ( -0.3543493200069162685, -0.000000000000000000, -0.9351131265310288487 ) ) ;
#42494 = DIRECTION ( 'NONE',  ( -0.7071067811865486830, 0.7071067811865464625, 0.000000000000000000 ) ) ;
#42495 = ORIENTED_EDGE ( 'NONE', *, *, #122262, .T. ) ;
#42496 = CARTESIAN_POINT ( 'NONE',  ( -31.49999999999977973, 7.466399257802189382, 5.000000000000000000 ) ) ;
#42497 = ADVANCED_FACE ( 'NONE', ( #137582 ), #37563, .F. ) ;
#42498 = DIRECTION ( 'NONE',  ( 0.7071067811865486830, -0.7071067811865464625, -0.000000000000000000 ) ) ;
#42499 = CARTESIAN_POINT ( 'NONE',  ( 29.89583333333333925, 1.633150327867687324, -6.094999999999991758 ) ) ;
#42500 = VECTOR ( 'NONE', #118903, 1000.000000000000000 ) ;
#42501 = VERTEX_POINT ( 'NONE', #125997 ) ;
#42502 = AXIS2_PLACEMENT_3D ( 'NONE', #31331, #53811, #119722 ) ;
#42503 = LINE ( 'NONE', #86708, #93086 ) ;
#42504 = VERTEX_POINT ( 'NONE', #17893 ) ;
#42505 = CARTESIAN_POINT ( 'NONE',  ( 79.77126352523144703, 4.472830434245839371, 4.472830434245842035 ) ) ;
#42506 = SURFACE_STYLE_FILL_AREA ( #141809 ) ;
#42508 = LINE ( 'NONE', #54108, #63221 ) ;
#42507 = VECTOR ( 'NONE', #25550, 1000.000000000000000 ) ;
#42509 = VERTEX_POINT ( 'NONE', #94755 ) ;
#42510 = CARTESIAN_POINT ( 'NONE',  ( -27.18398860626900060, 28.73617430169806042, 5.000000000000000000 ) ) ;
#42511 = CARTESIAN_POINT ( 'NONE',  ( 42.18398860626899705, 28.73617430169816700, 5.000000000000000000 ) ) ;
#42512 = FACE_OUTER_BOUND ( 'NONE', #48794, .T. ) ;
#42513 = EDGE_CURVE ( 'NONE', #105446, #53582, #15058, .T. ) ;
#42514 = FACE_OUTER_BOUND ( 'NONE', #10919, .T. ) ;
#42516 = VERTEX_POINT ( 'NONE', #5602 ) ;
#42515 = CARTESIAN_POINT ( 'NONE',  ( 0.000000000000000000, 0.000000000000000000, 5.000000000000000000 ) ) ;
#42517 = EDGE_CURVE ( 'NONE', #23695, #112275, #10080, .T. ) ;
#42518 = DIRECTION ( 'NONE',  ( 0.000000000000000000, -1.224646799147353207E-16, 1.000000000000000000 ) ) ;
#42519 = LINE ( 'NONE', #41781, #42486 ) ;
#42520 = VECTOR ( 'NONE', #38619, 1000.000000000000227 ) ;
#42521 = SURFACE_STYLE_FILL_AREA ( #141824 ) ;
#42522 = EDGE_CURVE ( 'NONE', #132792, #133359, #94055, .T. ) ;
#42523 = VERTEX_POINT ( 'NONE', #138294 ) ;
#42524 = VERTEX_POINT ( 'NONE', #38972 ) ;
#42525 = CARTESIAN_POINT ( 'NONE',  ( 60.52126352523143282, -4.472830434245839371, -4.472830434245840259 ) ) ;
#42526 = VECTOR ( 'NONE', #83283, 1000.000000000000000 ) ;
#42527 = ORIENTED_EDGE ( 'NONE', *, *, #74131, .T. ) ;
#42528 = EDGE_CURVE ( 'NONE', #24434, #130179, #115064, .T. ) ;
#42529 = FACE_OUTER_BOUND ( 'NONE', #127335, .T. ) ;
#42530 = CARTESIAN_POINT ( 'NONE',  ( 3.087196949643289390, 2.500000000000000444, 3.061616997868383634E-16 ) ) ;
#42531 = CARTESIAN_POINT ( 'NONE',  ( -24.55388970886357569, 5.485012786255876627, 4.000000000000000000 ) ) ;
#42532 = LINE ( 'NONE', #107737, #17737 ) ;
#42533 = EDGE_LOOP ( 'NONE', ( #59024, #86274, #2837, #81601, #65724 ) ) ;
#42534 = CARTESIAN_POINT ( 'NONE',  ( 20.99451991528748707, 28.92564299267952777, 4.000000000000000000 ) ) ;
#42535 = DIRECTION ( 'NONE',  ( 0.7071067811865486830, -0.7071067811865464625, -0.000000000000000000 ) ) ;
#42536 = CIRCLE ( 'NONE', #61086, 2.500000000000000888 ) ;
#42537 = EDGE_CURVE ( 'NONE', #111332, #32577, #59336, .T. ) ;
#42538 = VERTEX_POINT ( 'NONE', #95482 ) ;
#42539 = VECTOR ( 'NONE', #8302, 1000.000000000000000 ) ;
#42540 = LINE ( 'NONE', #87455, #49047 ) ;
#42541 = FACE_OUTER_BOUND ( 'NONE', #99373, .T. ) ;
#42542 = DIRECTION ( 'NONE',  ( -0.7071067811865486830, 0.7071067811865464625, 0.000000000000000000 ) ) ;
#42543 = ADVANCED_FACE ( 'NONE', ( #82488 ), #117216, .T. ) ;
#42544 = ORIENTED_EDGE ( 'NONE', *, *, #22405, .F. ) ;
#42546 = ORIENTED_EDGE ( 'NONE', *, *, #67569, .F. ) ;
#42545 = AXIS2_PLACEMENT_3D ( 'NONE', #83639, #28529, #72787 ) ;
#42547 = FACE_BOUND ( 'NONE', #125055, .T. ) ;
#42548 = CARTESIAN_POINT ( 'NONE',  ( 180.9243601523649261, -48.88932940808383165, 39.16623080367948972 ) ) ;
#42549 = CARTESIAN_POINT ( 'NONE',  ( -28.49999999999980105, -8.947814304570739452, 5.000000000000000000 ) ) ;
#42550 = LINE ( 'NONE', #413, #119969 ) ;
#42551 = EDGE_CURVE ( 'NONE', #121666, #94981, #39715, .T. ) ;
#42552 = DIRECTION ( 'NONE',  ( 1.000000000000000000, 0.000000000000000000, 0.000000000000000000 ) ) ;
#42553 = AXIS2_PLACEMENT_3D ( 'NONE', #54685, #75022, #40942 ) ;
#42554 = CARTESIAN_POINT ( 'NONE',  ( 31.49999999999978684, -14.70932175296474398, -11.46312253303844209 ) ) ;
#42555 = EDGE_LOOP ( 'NONE', ( #86924, #47163, #135274, #47100 ) ) ;
#42556 = VECTOR ( 'NONE', #83404, 999.9999999999998863 ) ;
#42557 = EDGE_LOOP ( 'NONE', ( #37748, #2611, #107978, #61703 ) ) ;
#42558 = CARTESIAN_POINT ( 'NONE',  ( 109.2870968585647944, 3.054999999999997495, 5.291415217122919401 ) ) ;
#42559 = ORIENTED_EDGE ( 'NONE', *, *, #67824, .F. ) ;
#42560 = VERTEX_POINT ( 'NONE', #28101 ) ;
#42561 = ADVANCED_FACE ( 'NONE', ( #62169 ), #16479, .F. ) ;
#42562 = VECTOR ( 'NONE', #2439, 1000.000000000000227 ) ;
#42563 = CARTESIAN_POINT ( 'NONE',  ( 183.9019840361164029, -51.74944211519454740, 38.65549799471349957 ) ) ;
#42564 = DIRECTION ( 'NONE',  ( -0.000000000000000000, 0.000000000000000000, 1.000000000000000000 ) ) ;
#42565 = EDGE_CURVE ( 'NONE', #99104, #54925, #142919, .T. ) ;
#42566 = EDGE_CURVE ( 'NONE', #133461, #98838, #93355, .T. ) ;
#42567 = LINE ( 'NONE', #43972, #74945 ) ;
#42568 = ORIENTED_EDGE ( 'NONE', *, *, #33045, .T. ) ;
#42569 = CARTESIAN_POINT ( 'NONE',  ( 3.730677800976855973, -49.14999999999999147, -40.92499999999998295 ) ) ;
#42570 = LINE ( 'NONE', #41824, #70461 ) ;
#42571 = DIRECTION ( 'NONE',  ( 0.7071067811865487940, -0.7071067811865463515, 0.000000000000000000 ) ) ;
#42572 = CARTESIAN_POINT ( 'NONE',  ( 6.183988606268994381, 28.73617430169791476, 5.000000000000000000 ) ) ;
#42573 = VECTOR ( 'NONE', #77897, 1000.000000000000000 ) ;
#42574 = DIRECTION ( 'NONE',  ( -1.000000000000000000, -1.224606353822377258E-16, -0.000000000000000000 ) ) ;
#42575 = ORIENTED_EDGE ( 'NONE', *, *, #79801, .T. ) ;
#42576 = EDGE_CURVE ( 'NONE', #126076, #74252, #6286, .T. ) ;
#42577 = LINE ( 'NONE', #131703, #38054 ) ;
#42578 = CARTESIAN_POINT ( 'NONE',  ( 51.45833333333332860, 3.974999999999997424, 6.884901960086288852 ) ) ;
#42579 = ORIENTED_EDGE ( 'NONE', *, *, #32423, .F. ) ;
#42580 = DIRECTION ( 'NONE',  ( -0.000000000000000000, -0.3543493200069152693, 0.9351131265310292928 ) ) ;
#42581 = ORIENTED_EDGE ( 'NONE', *, *, #105978, .F. ) ;
#42582 = ADVANCED_FACE ( 'NONE', ( #50564 ), #114388, .F. ) ;
#42583 = ORIENTED_EDGE ( 'NONE', *, *, #64508, .T. ) ;
#42584 = EDGE_LOOP ( 'NONE', ( #18599, #66882, #126293, #109037 ) ) ;
#42585 = VECTOR ( 'NONE', #128276, 999.9999999999998863 ) ;
#42586 = CARTESIAN_POINT ( 'NONE',  ( 62.70876352523143993, -7.482591942790329030E-16, 6.110000000000001208 ) ) ;
#42587 = ORIENTED_EDGE ( 'NONE', *, *, #90195, .T. ) ;
#42588 = VERTEX_POINT ( 'NONE', #130998 ) ;
#42589 = CARTESIAN_POINT ( 'NONE',  ( -34.42499999999997584, -21.76999999999999247, -40.00000000000000000 ) ) ;
#42590 = VECTOR ( 'NONE', #69504, 1000.000000000000000 ) ;
#42591 = LINE ( 'NONE', #142596, #5642 ) ;
#42592 = CARTESIAN_POINT ( 'NONE',  ( 97.56293019189810423, 1.637169565754157174, 6.110000000000002984 ) ) ;
#42593 = LINE ( 'NONE', #142598, #35576 ) ;
#42594 = ADVANCED_FACE ( 'NONE', ( #120807 ), #21514, .T. ) ;
#42595 = CARTESIAN_POINT ( 'NONE',  ( -42.48921356237308800, -27.52281430457085065, 5.000000000000000000 ) ) ;
#42596 = EDGE_LOOP ( 'NONE', ( #63261, #35993, #117319, #137350 ) ) ;
#42597 = DIRECTION ( 'NONE',  ( -1.000000000000000000, 0.000000000000000000, 0.000000000000000000 ) ) ;
#42598 = EDGE_CURVE ( 'NONE', #31526, #10888, #20779, .T. ) ;
#42599 = CARTESIAN_POINT ( 'NONE',  ( 0.000000000000000000, 0.000000000000000000, 5.000000000000000000 ) ) ;
#42600 = CARTESIAN_POINT ( 'NONE',  ( -75.18398860626899705, 28.73617430169839793, 5.000000000000000000 ) ) ;
#42601 = CARTESIAN_POINT ( 'NONE',  ( 77.22502705046287019, 5.819803920172573974, -5.819803920172573086 ) ) ;
#42602 = VERTEX_POINT ( 'NONE', #7748 ) ;
#42603 = PRESENTATION_STYLE_ASSIGNMENT (( #33168 ) ) ;
#42604 = ORIENTED_EDGE ( 'NONE', *, *, #88027, .T. ) ;
#42605 = ORIENTED_EDGE ( 'NONE', *, *, #49930, .F. ) ;
#42606 = ORIENTED_EDGE ( 'NONE', *, *, #32757, .F. ) ;
#42607 = CARTESIAN_POINT ( 'NONE',  ( 118.3287635252314658, 0.000000000000000000, -6.109999999999998543 ) ) ;
#42608 = ORIENTED_EDGE ( 'NONE', *, *, #21551, .T. ) ;
#42609 = DIRECTION ( 'NONE',  ( -0.7071067811865487940, 0.7071067811865463515, -0.000000000000000000 ) ) ;
#42610 = CARTESIAN_POINT ( 'NONE',  ( 11.99999999999992006, 5.587461875839188075, 4.000000000000000000 ) ) ;
#42611 = ORIENTED_EDGE ( 'NONE', *, *, #61249, .F. ) ;
#42612 = DIRECTION ( 'NONE',  ( -0.7071067811865487940, 0.7071067811865463515, -0.000000000000000000 ) ) ;
#42613 = ORIENTED_EDGE ( 'NONE', *, *, #44347, .F. ) ;
#42614 = VECTOR ( 'NONE', #120621, 999.9999999999998863 ) ;
#42615 =( BOUNDED_CURVE ( )  B_SPLINE_CURVE ( 3, ( #68657, #91127, #48307, #136025 ),
 .UNSPECIFIED., .F., .T. ) 
 B_SPLINE_CURVE_WITH_KNOTS ( ( 4, 4 ),
 ( 1.208578181583235267, 1.359146454359474232 ),
 .UNSPECIFIED. ) 
 CURVE ( )  GEOMETRIC_REPRESENTATION_ITEM ( )  RATIONAL_B_SPLINE_CURVE ( ( 1.000000000000000000, 0.9981116584018943083, 0.9981116584018943083, 1.000000000000000000 ) ) 
 REPRESENTATION_ITEM ( '' )  );
#42616 = ADVANCED_FACE ( 'NONE', ( #9146 ), #118672, .F. ) ;
#42617 = EDGE_CURVE ( 'NONE', #55582, #39393, #18617, .T. ) ;
#42618 = VECTOR ( 'NONE', #124473, 1000.000000000000227 ) ;
#42619 = CARTESIAN_POINT ( 'NONE',  ( 17.47873647476855652, -5.808823158059033709, 5.808823158059035485 ) ) ;
#42620 = LINE ( 'NONE', #31712, #62478 ) ;
#42621 = DIRECTION ( 'NONE',  ( 0.7071067811865486830, -0.7071067811865464625, -0.000000000000000000 ) ) ;
#42622 = CARTESIAN_POINT ( 'NONE',  ( 156.1500000000000057, -57.14999999999999147, -49.92499999999968452 ) ) ;
#42623 = ORIENTED_EDGE ( 'NONE', *, *, #71017, .T. ) ;
#42624 = ORIENTED_EDGE ( 'NONE', *, *, #125979, .F. ) ;
#42625 = VERTEX_POINT ( 'NONE', #130290 ) ;
#42626 = CARTESIAN_POINT ( 'NONE',  ( 0.000000000000000000, 0.000000000000000000, 0.000000000000000000 ) ) ;
#42627 = FACE_OUTER_BOUND ( 'NONE', #9209, .T. ) ;
#42628 = CARTESIAN_POINT ( 'NONE',  ( -5.999999999999951150, -3.033600742197705369, 5.000000000000000000 ) ) ;
#42629 = ADVANCED_FACE ( 'NONE', ( #32394 ), #140422, .F. ) ;
#42630 = VECTOR ( 'NONE', #3833, 1000.000000000000227 ) ;
#42631 = DIRECTION ( 'NONE',  ( 0.000000000000000000, 0.000000000000000000, -1.000000000000000000 ) ) ;
#42632 = CARTESIAN_POINT ( 'NONE',  ( 34.92499999999998295, -13.19990548397269237, 4.759050581649323597 ) ) ;
#42633 = DIRECTION ( 'NONE',  ( 0.6830127018922181881, 0.6830127018922202975, -0.2588190451025214056 ) ) ;
#42634 = AXIS2_PLACEMENT_3D ( 'NONE', #142112, #42798, #31899 ) ;
#42635 = CARTESIAN_POINT ( 'NONE',  ( 27.85459685856477208, -1.637169565754161615, 6.110000000000000320 ) ) ;
#42636 = DIRECTION ( 'NONE',  ( 0.7071067811865487940, 0.7071067811865463515, -0.000000000000000000 ) ) ;
#42637 = DIRECTION ( 'NONE',  ( -0.7071067811865486830, -0.7071067811865464625, 0.000000000000000000 ) ) ;
#42638 = VERTEX_POINT ( 'NONE', #129533 ) ;
#42639 = DIRECTION ( 'NONE',  ( 0.000000000000000000, -1.000000000000000000, 0.000000000000000000 ) ) ;
#42640 = ORIENTED_EDGE ( 'NONE', *, *, #13497, .T. ) ;
#42641 = CARTESIAN_POINT ( 'NONE',  ( 69.18398860626899705, 28.73617430169835529, 5.000000000000000000 ) ) ;
#42642 = ORIENTED_EDGE ( 'NONE', *, *, #61724, .T. ) ;
#42643 = VECTOR ( 'NONE', #105181, 1000.000000000000000 ) ;
#42644 = CARTESIAN_POINT ( 'NONE',  ( 33.98911971346028338, -22.02621442084248216, 4.990779571109221102 ) ) ;
#42646 = ORIENTED_EDGE ( 'NONE', *, *, #142202, .T. ) ;
#42645 = CARTESIAN_POINT ( 'NONE',  ( 0.000000000000000000, 0.000000000000000000, 0.000000000000000000 ) ) ;
#42647 = DIRECTION ( 'NONE',  ( -0.6830127018922180770, -0.6830127018922204085, -0.2588190451025213501 ) ) ;
#42648 = ORIENTED_EDGE ( 'NONE', *, *, #117390, .T. ) ;
#42649 = ORIENTED_EDGE ( 'NONE', *, *, #50542, .F. ) ;
#42650 = DIRECTION ( 'NONE',  ( -0.000000000000000000, 0.000000000000000000, 1.000000000000000000 ) ) ;
#42651 = ORIENTED_EDGE ( 'NONE', *, *, #63811, .F. ) ;
#42652 = VECTOR ( 'NONE', #123527, 1000.000000000000000 ) ;
#42653 = CARTESIAN_POINT ( 'NONE',  ( 93.99586038379622721, -3.974999999999998312, -6.884901960086286188 ) ) ;
#42654 = CARTESIAN_POINT ( 'NONE',  ( 116.7458603837962272, 3.974999999999996980, 6.884901960086287964 ) ) ;
#42656 = VECTOR ( 'NONE', #2428, 1000.000000000000000 ) ;
#42655 = CARTESIAN_POINT ( 'NONE',  ( 7.499999999999952927, -4.533600742197692490, 5.000000000000000000 ) ) ;
#42657 = CARTESIAN_POINT ( 'NONE',  ( 181.1500000000000057, -3.180000000000061444, -31.92499999999998295 ) ) ;
#42658 = CARTESIAN_POINT ( 'NONE',  ( 7.939999999999994174, -39.93000000000000682, -10.00000000000000178 ) ) ;
#42659 = CARTESIAN_POINT ( 'NONE',  ( 10.37159235450332062, 9.902892378096218942E-16, 0.000000000000000000 ) ) ;
#42660 = EDGE_CURVE ( 'NONE', #41817, #99801, #62897, .T. ) ;
#42661 = DIRECTION ( 'NONE',  ( 1.412012880465675998E-16, 0.9667936545734397980, 0.2555582702174447052 ) ) ;
#42662 = CARTESIAN_POINT ( 'NONE',  ( 9.333333333333333925, 5.278424836066143655, -3.047499999999997655 ) ) ;
#42663 = CARTESIAN_POINT ( 'NONE',  ( 18.79123647476855652, -9.717572351234235426E-16, -7.934999999999990727 ) ) ;
#42664 = DIRECTION ( 'NONE',  ( -1.000000000000000000, -1.224606353822377258E-16, -0.000000000000000000 ) ) ;
#42665 = PLANE ( 'NONE',  #142796 ) ;
#42666 = ORIENTED_EDGE ( 'NONE', *, *, #133303, .F. ) ;
#42667 = ORIENTED_EDGE ( 'NONE', *, *, #67109, .F. ) ;
#42669 = EDGE_CURVE ( 'NONE', #45818, #74780, #107775, .T. ) ;
#42668 = DIRECTION ( 'NONE',  ( -0.000000000000000000, 0.000000000000000000, 1.000000000000000000 ) ) ;
#42670 = VERTEX_POINT ( 'NONE', #87484 ) ;
#42671 = CARTESIAN_POINT ( 'NONE',  ( -26.99999999999980815, 4.384688058510544550, -7.090945410444748020 ) ) ;
#42672 = LINE ( 'NONE', #142674, #16079 ) ;
#42673 = VECTOR ( 'NONE', #16536, 1000.000000000000000 ) ;
#42674 = CARTESIAN_POINT ( 'NONE',  ( 127.7579555295392595, -48.22435659090664473, -37.54366622512464602 ) ) ;
#42675 = EDGE_LOOP ( 'NONE', ( #10338, #122171, #53794, #135528 ) ) ;
#42676 = DIRECTION ( 'NONE',  ( -0.000000000000000000, 0.3543493200069153248, 0.9351131265310292928 ) ) ;
#42677 = DIRECTION ( 'NONE',  ( 0.3543493200069162685, -0.000000000000000000, -0.9351131265310288487 ) ) ;
#42678 = ADVANCED_FACE ( 'NONE', ( #120061 ), #31675, .F. ) ;
#42679 = DIRECTION ( 'NONE',  ( -0.3543493200069162685, -0.000000000000000000, -0.9351131265310288487 ) ) ;
#42680 = EDGE_CURVE ( 'NONE', #72157, #102238, #143279, .T. ) ;
#42681 = EDGE_CURVE ( 'NONE', #92779, #136084, #142585, .T. ) ;
#42682 = DIRECTION ( 'NONE',  ( 1.000000000000000000, 0.000000000000000000, 0.000000000000000000 ) ) ;
#42684 = VERTEX_POINT ( 'NONE', #20054 ) ;
#42683 = DIRECTION ( 'NONE',  ( 0.7071067811865486830, -0.7071067811865464625, -0.000000000000000000 ) ) ;
#42685 = DIRECTION ( 'NONE',  ( 0.1737853339090545957, -0.1737853339090541793, -0.9693282805305111216 ) ) ;
#42686 = CARTESIAN_POINT ( 'NONE',  ( -3.792893218813425005, 15.75929247661555799, 5.000000000000000000 ) ) ;
#42687 = DIRECTION ( 'NONE',  ( 0.6830127018922180770, -0.6830127018922204085, -0.2588190451025213501 ) ) ;
#42688 = FACE_OUTER_BOUND ( 'NONE', #3507, .T. ) ;
#42689 = EDGE_CURVE ( 'NONE', #129495, #134514, #86055, .T. ) ;
#42691 = ADVANCED_FACE ( 'NONE', ( #141885 ), #97625, .F. ) ;
#42690 = ORIENTED_EDGE ( 'NONE', *, *, #61545, .T. ) ;
#42692 = ORIENTED_EDGE ( 'NONE', *, *, #64784, .F. ) ;
#42693 = EDGE_LOOP ( 'NONE', ( #70474, #105397, #119018, #66647, #69385 ) ) ;
#42694 = CARTESIAN_POINT ( 'NONE',  ( 91.58376352523144703, -6.110000000000001208, -3.741295971395164515E-16 ) ) ;
#42695 = VERTEX_POINT ( 'NONE', #64300 ) ;
#42696 = EDGE_CURVE ( 'NONE', #62376, #97591, #42577, .T. ) ;
#42697 = CARTESIAN_POINT ( 'NONE',  ( 130.7303687233793710, -48.51451318982915950, 38.21513923099971777 ) ) ;
#42698 = CARTESIAN_POINT ( 'NONE',  ( -18.29974487139159223, -27.71228299555219010, 4.000000000000000000 ) ) ;
#42699 = ORIENTED_EDGE ( 'NONE', *, *, #6826, .F. ) ;
#42700 = CARTESIAN_POINT ( 'NONE',  ( 183.8964364361580408, -51.76057561339556656, 38.69631370864702546 ) ) ;
#42702 = VECTOR ( 'NONE', #81445, 1000.000000000000000 ) ;
#42701 = CARTESIAN_POINT ( 'NONE',  ( -19.49999999999986500, 11.52377502935401310, -1.522421517564041427 ) ) ;
#42703 = EDGE_CURVE ( 'NONE', #99005, #108854, #9903, .T. ) ;
#42704 = CARTESIAN_POINT ( 'NONE',  ( 92.22459685856479439, -1.637169565754160949, 6.109999999999997655 ) ) ;
#42705 = EDGE_LOOP ( 'NONE', ( #134188, #19389, #136492, #103252 ) ) ;
#42706 = CARTESIAN_POINT ( 'NONE',  ( -66.48921356237309510, -27.52281430457101763, 5.000000000000000000 ) ) ;
#42707 = DIRECTION ( 'NONE',  ( 0.000000000000000000, -1.000000000000000000, 0.000000000000000000 ) ) ;
#42708 = B_SPLINE_CURVE_WITH_KNOTS ( 'NONE', 3,
 ( #41214, #86166, #19470, #65146, #52098, #130391, #62282, #85419, #20158, #107873, #8542, #109336 ),
 .UNSPECIFIED., .F., .F.,
 ( 4, 2, 2, 2, 2, 4 ),
 ( 0.000000000000000000, 0.001816333612422246432, 0.002724500418633369649, 0.003632667224844492865, 0.005449000837266739297, 0.007265334449688985730 ),
 .UNSPECIFIED. ) ;
#42709 = ORIENTED_EDGE ( 'NONE', *, *, #120732, .F. ) ;
#42710 = ORIENTED_EDGE ( 'NONE', *, *, #66289, .F. ) ;
#42711 = VERTEX_POINT ( 'NONE', #73738 ) ;
#42712 = CARTESIAN_POINT ( 'NONE',  ( -34.92500000000001137, 22.22500000000000142, 4.000000000000000000 ) ) ;
#42713 = FACE_OUTER_BOUND ( 'NONE', #67918, .T. ) ;
#42714 = CARTESIAN_POINT ( 'NONE',  ( 16.83790314143521982, -6.871911579029513106, -3.967499999999993587 ) ) ;
#42715 = DIRECTION ( 'NONE',  ( -0.7071067811865486830, -0.7071067811865464625, 0.000000000000000000 ) ) ;
#42717 = ADVANCED_FACE ( 'NONE', ( #108467 ), #53416, .F. ) ;
#42716 = VECTOR ( 'NONE', #24025, 999.9999999999998863 ) ;
#42718 = CARTESIAN_POINT ( 'NONE',  ( 165.9183975471111410, 26.96999999999993847, 33.53367344373089054 ) ) ;
#42719 = DIRECTION ( 'NONE',  ( -0.3543493200069162685, -0.000000000000000000, -0.9351131265310288487 ) ) ;
#42720 = AXIS2_PLACEMENT_3D ( 'NONE', #44281, #23943, #88493 ) ;
#42721 = ORIENTED_EDGE ( 'NONE', *, *, #44018, .F. ) ;
#42722 = ORIENTED_EDGE ( 'NONE', *, *, #108437, .T. ) ;
#42723 = VECTOR ( 'NONE', #128581, 1000.000000000000000 ) ;
#42724 = CARTESIAN_POINT ( 'NONE',  ( 27.99999999999996803, -57.14999999999999147, 53.92499999999996874 ) ) ;
#42725 = VERTEX_POINT ( 'NONE', #88934 ) ;
#42726 = ORIENTED_EDGE ( 'NONE', *, *, #126862, .T. ) ;
#42727 = EDGE_CURVE ( 'NONE', #27164, #64534, #58481, .T. ) ;
#42728 = EDGE_CURVE ( 'NONE', #55336, #51167, #122224, .T. ) ;
#42729 = CARTESIAN_POINT ( 'NONE',  ( 4.499999999999968914, -14.56887692260766265, 4.000000000000000000 ) ) ;
#42730 = ORIENTED_EDGE ( 'NONE', *, *, #55192, .T. ) ;
#42731 = VECTOR ( 'NONE', #23882, 1000.000000000000000 ) ;
#42732 = DIRECTION ( 'NONE',  ( -0.000000000000000000, -0.3543493200069152693, 0.9351131265310292928 ) ) ;
#42733 = FACE_OUTER_BOUND ( 'NONE', #53017, .T. ) ;
#42734 = EDGE_CURVE ( 'NONE', #31006, #40381, #59540, .T. ) ;
#42735 = CARTESIAN_POINT ( 'NONE',  ( -14.99999999999989519, 12.25461709320619086, -10.07315571508700458 ) ) ;
#42736 = FACE_OUTER_BOUND ( 'NONE', #130735, .T. ) ;
#42737 = ADVANCED_FACE ( 'NONE', ( #99772 ), #95870, .T. ) ;
#42738 = CARTESIAN_POINT ( 'NONE',  ( 119.5624999999999858, -5.819803920172573086, -5.819803920172573974 ) ) ;
#42739 = ORIENTED_EDGE ( 'NONE', *, *, #63632, .F. ) ;
#42740 = ADVANCED_FACE ( 'NONE', ( #44740 ), #78754, .F. ) ;
#42741 = DIRECTION ( 'NONE',  ( 0.000000000000000000, -1.000000000000000000, 0.000000000000000000 ) ) ;
#42742 = ORIENTED_EDGE ( 'NONE', *, *, #76377, .F. ) ;
#42743 = FACE_OUTER_BOUND ( 'NONE', #18417, .T. ) ;
#42744 = ORIENTED_EDGE ( 'NONE', *, *, #53473, .T. ) ;
#42745 = DIRECTION ( 'NONE',  ( -0.7071067811865486830, -0.7071067811865464625, 0.000000000000000000 ) ) ;
#42746 = ORIENTED_EDGE ( 'NONE', *, *, #74083, .T. ) ;
#42747 = CARTESIAN_POINT ( 'NONE',  ( 66.29974487139159578, -27.71228299555252406, 4.000000000000000000 ) ) ;
#42748 = VERTEX_POINT ( 'NONE', #47587 ) ;
#42749 = VERTEX_POINT ( 'NONE', #1836 ) ;
#42750 = EDGE_CURVE ( 'NONE', #127190, #126386, #142166, .T. ) ;
#42751 = ORIENTED_EDGE ( 'NONE', *, *, #41097, .F. ) ;
#42752 = VECTOR ( 'NONE', #129759, 999.9999999999998863 ) ;
#42753 = CARTESIAN_POINT ( 'NONE',  ( 5.848407645496676466, 9.139736423841732040E-16, 0.000000000000000000 ) ) ;
#42754 = COLOUR_RGB ( '', 0.66274510, 0.83137255, 0.94901961) ;
#42755 = PRESENTATION_LAYER_ASSIGNMENT (  '', '', ( #119088 ) ) ;
#42756 = CARTESIAN_POINT ( 'NONE',  ( -45.48921356237309510, -27.52281430457087197, 5.000000000000000000 ) ) ;
#42757 = DIRECTION ( 'NONE',  ( 1.000000000000000000, 0.000000000000000000, 0.000000000000000000 ) ) ;
#42758 = DIRECTION ( 'NONE',  ( 0.000000000000000000, -1.000000000000000000, 0.000000000000000000 ) ) ;
#42759 = AXIS2_PLACEMENT_3D ( 'NONE', #102090, #2755, #111524 ) ;
#42760 = EDGE_CURVE ( 'NONE', #35346, #11548, #22896, .T. ) ;
#42761 = DIRECTION ( 'NONE',  ( 0.000000000000000000, 0.000000000000000000, 1.000000000000000000 ) ) ;
#42762 = CARTESIAN_POINT ( 'NONE',  ( 128.9683591370937563, -52.14999999999999147, 41.64499999999997470 ) ) ;
#42763 = CARTESIAN_POINT ( 'NONE',  ( -75.48921356237309510, -27.52281430457107803, 5.000000000000000000 ) ) ;
#42764 = CARTESIAN_POINT ( 'NONE',  ( 21.77004279457778324, 21.73644205237997795, 5.000000000000000888 ) ) ;
#42765 = FACE_OUTER_BOUND ( 'NONE', #58191, .T. ) ;
#42766 = CARTESIAN_POINT ( 'NONE',  ( 9.748407645496676821, -3.851859888774471706E-31, 2.500000000000001332 ) ) ;
#42767 = ORIENTED_EDGE ( 'NONE', *, *, #129572, .T. ) ;
#42768 = ORIENTED_EDGE ( 'NONE', *, *, #113926, .T. ) ;
#42769 = ORIENTED_EDGE ( 'NONE', *, *, #134586, .T. ) ;
#42770 = DIRECTION ( 'NONE',  ( -0.6830127018922181881, 0.6830127018922202975, -0.2588190451025214056 ) ) ;
#42771 = ORIENTED_EDGE ( 'NONE', *, *, #80027, .T. ) ;
#42772 = ORIENTED_EDGE ( 'NONE', *, *, #66589, .F. ) ;
#42773 = DIRECTION ( 'NONE',  ( -0.000000000000000000, 0.000000000000000000, 1.000000000000000000 ) ) ;
#42774 = DIRECTION ( 'NONE',  ( -0.7071067811865486830, 0.7071067811865464625, 0.000000000000000000 ) ) ;
#42775 = EDGE_CURVE ( 'NONE', #99771, #137862, #111352, .T. ) ;
#42776 = DIRECTION ( 'NONE',  ( -0.000000000000000000, 0.3543493200069153248, 0.9351131265310292928 ) ) ;
#42777 = VERTEX_POINT ( 'NONE', #25055 ) ;
#42778 = CARTESIAN_POINT ( 'NONE',  ( -3.299744871391591339, -27.71228299555208352, 4.000000000000000000 ) ) ;
#42779 = ORIENTED_EDGE ( 'NONE', *, *, #41692, .F. ) ;
#42780 = CARTESIAN_POINT ( 'NONE',  ( 0.000000000000000000, 0.000000000000000000, 5.000000000000000000 ) ) ;
#42781 = EDGE_CURVE ( 'NONE', #131451, #91250, #23648, .T. ) ;
#42782 = DIRECTION ( 'NONE',  ( 1.000000000000000000, 0.000000000000000000, 0.000000000000000000 ) ) ;
#42783 = CARTESIAN_POINT ( 'NONE',  ( 10.85873647476855197, 5.808823158059031044, -5.808823158059038150 ) ) ;
#42784 = ORIENTED_EDGE ( 'NONE', *, *, #9258, .F. ) ;
#42785 = CARTESIAN_POINT ( 'NONE',  ( 95.57876352523145158, -7.482591942790327058E-16, 6.109999999999999432 ) ) ;
#42786 = EDGE_CURVE ( 'NONE', #91471, #27362, #134575, .T. ) ;
#42787 = FACE_OUTER_BOUND ( 'NONE', #10123, .T. ) ;
#42788 = DIRECTION ( 'NONE',  ( 0.000000000000000000, 0.000000000000000000, 1.000000000000000000 ) ) ;
#42789 = CARTESIAN_POINT ( 'NONE',  ( -27.79333936457828358, 21.75929247661549581, 4.998822639870701856 ) ) ;
#42790 = VERTEX_POINT ( 'NONE', #35976 ) ;
#42791 = ORIENTED_EDGE ( 'NONE', *, *, #96887, .F. ) ;
#42792 = CARTESIAN_POINT ( 'NONE',  ( 13.92145407031093818, -2.500000000000000000, 3.061616997868383634E-16 ) ) ;
#42793 = VERTEX_POINT ( 'NONE', #22196 ) ;
#42794 = LINE ( 'NONE', #131208, #134290 ) ;
#42795 = CARTESIAN_POINT ( 'NONE',  ( -19.49999999999986500, -9.462702396501025959, -9.474982329943468784 ) ) ;
#42796 = PLANE ( 'NONE',  #36124 ) ;
#42797 = PLANE ( 'NONE',  #135376 ) ;
#42798 = DIRECTION ( 'NONE',  ( -0.6830127018922181881, 0.6830127018922202975, -0.2588190451025214056 ) ) ;
#42800 = VERTEX_POINT ( 'NONE', #12044 ) ;
#42799 = VECTOR ( 'NONE', #23838, 1000.000000000000227 ) ;
#42801 = DIRECTION ( 'NONE',  ( -0.000000000000000000, 0.3543493200069152138, -0.9351131265310292928 ) ) ;
#42802 = EDGE_CURVE ( 'NONE', #23744, #29345, #112103, .T. ) ;
#42803 = DIRECTION ( 'NONE',  ( -0.7071067811865487940, 0.7071067811865463515, -0.000000000000000000 ) ) ;
#42804 = DIRECTION ( 'NONE',  ( 0.7071067811865487940, -0.7071067811865463515, 0.000000000000000000 ) ) ;
#42805 = ORIENTED_EDGE ( 'NONE', *, *, #74954, .T. ) ;
#42806 = CARTESIAN_POINT ( 'NONE',  ( 1.042387978378689573, 4.202752102959690472E-16, 0.000000000000000000 ) ) ;
#42807 = CARTESIAN_POINT ( 'NONE',  ( -7.499999999999940492, 16.46639925780209524, 5.000000000000000000 ) ) ;
#42808 = ORIENTED_EDGE ( 'NONE', *, *, #45502, .F. ) ;
#42810 = ORIENTED_EDGE ( 'NONE', *, *, #12340, .F. ) ;
#42809 = FACE_OUTER_BOUND ( 'NONE', #56154, .T. ) ;
#42811 = VERTEX_POINT ( 'NONE', #13452 ) ;
#42812 = EDGE_CURVE ( 'NONE', #129512, #34230, #90324, .T. ) ;
#42813 = LINE ( 'NONE', #128382, #97893 ) ;
#42814 = CARTESIAN_POINT ( 'NONE',  ( 30.48921356237309510, -27.52281430457076894, 5.000000000000000000 ) ) ;
#42815 = EDGE_LOOP ( 'NONE', ( #97268, #54829, #49569, #22676 ) ) ;
#42816 = CARTESIAN_POINT ( 'NONE',  ( 17.20710678118641468, -20.24070752338408141, 5.000000000000000000 ) ) ;
#42817 = CARTESIAN_POINT ( 'NONE',  ( 14.24139925780194105, 21.72500000000000142, 5.000000000000000000 ) ) ;
#42818 = AXIS2_PLACEMENT_3D ( 'NONE', #115716, #82430, #48364 ) ;
#42819 = CARTESIAN_POINT ( 'NONE',  ( 8.999999999999937828, -7.068876922607741697, 4.000000000000000000 ) ) ;
#42820 = DIRECTION ( 'NONE',  ( -0.7071067811865486830, 0.7071067811865464625, 0.000000000000000000 ) ) ;
#42821 = CARTESIAN_POINT ( 'NONE',  ( 0.1600000000000038058, -0.6768933422324286964, -7.934999999999988951 ) ) ;
#42822 = CARTESIAN_POINT ( 'NONE',  ( -63.29974487139158867, -27.71228299555250274, 4.000000000000000000 ) ) ;
#42823 = LINE ( 'NONE', #65297, #137501 ) ;
#42824 = FACE_OUTER_BOUND ( 'NONE', #77413, .T. ) ;
#42825 = CARTESIAN_POINT ( 'NONE',  ( -26.24139925780185578, 21.72500000000000142, 5.000000000000000000 ) ) ;
#42826 = CARTESIAN_POINT ( 'NONE',  ( 2.241399257802041856, 21.72499999999999432, 5.000000000000000000 ) ) ;
#42827 = CARTESIAN_POINT ( 'NONE',  ( 25.99806943317883068, -22.22500000000000142, 4.500000000000000888 ) ) ;
#42828 = FACE_OUTER_BOUND ( 'NONE', #115829, .T. ) ;
#42829 = CARTESIAN_POINT ( 'NONE',  ( 28.82816939922333077, 9.759292476615618384, 4.000000000000000000 ) ) ;
#42830 = ORIENTED_EDGE ( 'NONE', *, *, #93905, .F. ) ;
#42831 =( BOUNDED_CURVE ( )  B_SPLINE_CURVE ( 3, ( #100727, #34762, #54396, #67405 ),
 .UNSPECIFIED., .F., .F. ) 
 B_SPLINE_CURVE_WITH_KNOTS ( ( 4, 4 ),
 ( 5.005968288816724510, 5.074607125596353185 ),
 .UNSPECIFIED. ) 
 CURVE ( )  GEOMETRIC_REPRESENTATION_ITEM ( )  RATIONAL_B_SPLINE_CURVE ( ( 1.000000000000000000, 0.9996074310407762065, 0.9996074310407762065, 1.000000000000000000 ) ) 
 REPRESENTATION_ITEM ( '' )  );
#42832 = EDGE_LOOP ( 'NONE', ( #72617, #127678, #124368, #25434 ) ) ;
#42833 = ORIENTED_EDGE ( 'NONE', *, *, #70717, .T. ) ;
#42834 = CARTESIAN_POINT ( 'NONE',  ( 98.27083333333332860, -7.949999999999999289, -2.130196079827426203 ) ) ;
#42835 = ORIENTED_EDGE ( 'NONE', *, *, #33720, .T. ) ;
#42836 = VECTOR ( 'NONE', #55463, 999.9999999999998863 ) ;
#42837 = EDGE_LOOP ( 'NONE', ( #76298, #33487, #69895, #67744 ) ) ;
#42838 = ORIENTED_EDGE ( 'NONE', *, *, #41635, .T. ) ;
#42839 = CARTESIAN_POINT ( 'NONE',  ( -28.49999999999980105, 18.43112307739199451, 4.000000000000000000 ) ) ;
#42840 = EDGE_CURVE ( 'NONE', #46695, #97392, #35275, .T. ) ;
#42841 = CARTESIAN_POINT ( 'NONE',  ( 90.10416666666668561, 2.130196079827460398, 7.949999999999981526 ) ) ;
#42842 = ORIENTED_EDGE ( 'NONE', *, *, #59264, .T. ) ;
#42843 =( BOUNDED_CURVE ( )  B_SPLINE_CURVE ( 3, ( #100526, #97650, #44759, #143299 ),
 .UNSPECIFIED., .F., .T. ) 
 B_SPLINE_CURVE_WITH_KNOTS ( ( 4, 4 ),
 ( 0.6783063634690170707, 0.7469765549618208045 ),
 .UNSPECIFIED. ) 
 CURVE ( )  GEOMETRIC_REPRESENTATION_ITEM ( )  RATIONAL_B_SPLINE_CURVE ( ( 1.000000000000000000, 0.9996070723374664846, 0.9996070723374664846, 1.000000000000000000 ) ) 
 REPRESENTATION_ITEM ( '' )  );
#42844 = CARTESIAN_POINT ( 'NONE',  ( 11.99451991528749417, 28.92564299267946382, 4.000000000000000000 ) ) ;
#42845 = DIRECTION ( 'NONE',  ( 1.192622389734054877E-16, -1.000000000000000000, 0.000000000000000000 ) ) ;
#42846 = PLANE ( 'NONE',  #104241 ) ;
#42847 = DIRECTION ( 'NONE',  ( 1.000000000000000000, 0.000000000000000000, 0.000000000000000000 ) ) ;
#42848 = ORIENTED_EDGE ( 'NONE', *, *, #105818, .F. ) ;
#42849 = EDGE_CURVE ( 'NONE', #38643, #129515, #124387, .T. ) ;
#42850 = PLANE ( 'NONE',  #132153 ) ;
#42851 = DIRECTION ( 'NONE',  ( 0.7071067811865487940, 0.7071067811865463515, 0.000000000000000000 ) ) ;
#42852 = CARTESIAN_POINT ( 'NONE',  ( 1.499999999999992673, 18.43112307739199451, 4.000000000000000000 ) ) ;
#42853 = LINE ( 'NONE', #97930, #56742 ) ;
#42854 = CARTESIAN_POINT ( 'NONE',  ( 1.629999999999999893, 0.4000000000000001887, -2.500000000000000000 ) ) ;
#42855 = DIRECTION ( 'NONE',  ( -0.000000000000000000, -0.000000000000000000, -1.000000000000000000 ) ) ;
#42856 = CARTESIAN_POINT ( 'NONE',  ( 29.53752705046289151, -9.735942053221456900E-16, 7.949999999999998401 ) ) ;
#42857 = AXIS2_PLACEMENT_3D ( 'NONE', #23565, #67834, #133077 ) ;
#42858 = DIRECTION ( 'NONE',  ( 0.7071067811865487940, 0.7071067811865463515, 0.000000000000000000 ) ) ;
#42859 = ADVANCED_FACE ( 'NONE', ( #15575 ), #50408, .F. ) ;
#42860 = EDGE_CURVE ( 'NONE', #119020, #64492, #38812, .T. ) ;
#42861 = ORIENTED_EDGE ( 'NONE', *, *, #61384, .T. ) ;
#42862 = VERTEX_POINT ( 'NONE', #3972 ) ;
#42863 = VECTOR ( 'NONE', #22916, 1000.000000000000227 ) ;
#42864 = CARTESIAN_POINT ( 'NONE',  ( 25.35416666666666430, -2.130196079827425315, -7.950000000000001066 ) ) ;
#42865 = ADVANCED_FACE ( 'NONE', ( #136680 ), #104773, .F. ) ;
#42866 = ORIENTED_EDGE ( 'NONE', *, *, #8938, .T. ) ;
#42867 = AXIS2_PLACEMENT_3D ( 'NONE', #63244, #107413, #8074 ) ;
#42868 = DIRECTION ( 'NONE',  ( 0.000000000000000000, 0.000000000000000000, -1.000000000000000000 ) ) ;
#42869 = EDGE_CURVE ( 'NONE', #123300, #141915, #103322, .T. ) ;
#42870 = CARTESIAN_POINT ( 'NONE',  ( 39.48921356237310221, -27.52281430457082934, 5.000000000000000000 ) ) ;
#42871 = EDGE_CURVE ( 'NONE', #79017, #330, #59173, .T. ) ;
#42872 = DIRECTION ( 'NONE',  ( 0.7071067811865487940, 0.7071067811865463515, -0.000000000000000000 ) ) ;
#42873 = CARTESIAN_POINT ( 'NONE',  ( 28.17183060077628554, 18.75929247661553845, 4.000000000000000000 ) ) ;
#42874 = CARTESIAN_POINT ( 'NONE',  ( 0.8500512854102346694, -8.240707523384200428, 17.25253755692239110 ) ) ;
#42875 = FILL_AREA_STYLE ('',( #110922 ) ) ;
#42876 = EDGE_CURVE ( 'NONE', #139000, #35892, #105464, .T. ) ;
#42877 = CARTESIAN_POINT ( 'NONE',  ( 121.2454301918981230, -5.291415217122918513, -3.055000000000000160 ) ) ;
#42878 = ORIENTED_EDGE ( 'NONE', *, *, #83088, .F. ) ;
#42879 = VERTEX_POINT ( 'NONE', #117061 ) ;
#42880 = CARTESIAN_POINT ( 'NONE',  ( 2.510786437626908008, -27.52281430457053446, 5.000000000000000000 ) ) ;
#42881 = CARTESIAN_POINT ( 'NONE',  ( 31.49999999999979039, 4.466399257802221356, 5.000000000000000000 ) ) ;
#42882 =( NAMED_UNIT ( * ) SI_UNIT ( $, .STERADIAN. ) SOLID_ANGLE_UNIT ( ) );
#42883 = ADVANCED_FACE ( 'NONE', ( #127984 ), #94595, .F. ) ;
#42884 = FACE_OUTER_BOUND ( 'NONE', #104239, .T. ) ;
#42885 = ORIENTED_EDGE ( 'NONE', *, *, #101805, .T. ) ;
#42886 = CARTESIAN_POINT ( 'NONE',  ( 43.60459685856476852, 1.637169565754164946, -6.109999999999999432 ) ) ;
#42887 = ORIENTED_EDGE ( 'NONE', *, *, #125704, .F. ) ;
#42888 = CARTESIAN_POINT ( 'NONE',  ( 39.18398860626899705, 28.73617430169814568, 5.000000000000000000 ) ) ;
#42889 = DIRECTION ( 'NONE',  ( -0.3543493200069162685, -0.000000000000000000, -0.9351131265310288487 ) ) ;
#42890 = LINE ( 'NONE', #100103, #20031 ) ;
#42891 =( NAMED_UNIT ( * ) PLANE_ANGLE_UNIT ( ) SI_UNIT ( $, .RADIAN. ) );
#42892 = EDGE_CURVE ( 'NONE', #74099, #94079, #5433, .T. ) ;
#42893 = CARTESIAN_POINT ( 'NONE',  ( 37.53709685856478018, -3.054999999999998828, -5.291415217122919401 ) ) ;
#42894 = EDGE_LOOP ( 'NONE', ( #60455, #121686, #57600, #38309 ) ) ;
#42895 = FACE_OUTER_BOUND ( 'NONE', #34902, .T. ) ;
#42896 = ORIENTED_EDGE ( 'NONE', *, *, #53467, .F. ) ;
#42897 = VERTEX_POINT ( 'NONE', #27929 ) ;
#42898 = ORIENTED_EDGE ( 'NONE', *, *, #132716, .F. ) ;
#42899 = CARTESIAN_POINT ( 'NONE',  ( -34.45011844616454511, 1.516280811637461534, 5.000000000000000888 ) ) ;
#42900 = DIRECTION ( 'NONE',  ( 0.7071067811865487940, 0.7071067811865463515, 0.000000000000000000 ) ) ;
#42901 = PRODUCT_DEFINITION_CONTEXT ( 'detailed design', #22594, 'design' ) ;
#42902 = ORIENTED_EDGE ( 'NONE', *, *, #40249, .T. ) ;
#42903 = LINE ( 'NONE', #76969, #85309 ) ;
#42904 = EDGE_CURVE ( 'NONE', #119580, #15522, #14899, .T. ) ;
#42905 = CARTESIAN_POINT ( 'NONE',  ( -35.99451991528749772, 28.92564299267963079, 4.000000000000000000 ) ) ;
#42906 = ADVANCED_FACE ( 'NONE', ( #17058 ), #125831, .F. ) ;
#42907 = FACE_OUTER_BOUND ( 'NONE', #125122, .T. ) ;
#42908 = FACE_BOUND ( 'NONE', #6468, .T. ) ;
#42909 = ORIENTED_EDGE ( 'NONE', *, *, #110418, .F. ) ;
#42910 = DIRECTION ( 'NONE',  ( -0.7071067811865486830, -0.7071067811865464625, -0.000000000000000000 ) ) ;
#42911 = DIRECTION ( 'NONE',  ( -0.6830127018922180770, -0.6830127018922204085, -0.2588190451025213501 ) ) ;
#42912 = LINE ( 'NONE', #63938, #129627 ) ;
#42913 = ORIENTED_EDGE ( 'NONE', *, *, #47003, .F. ) ;
#42914 = VERTEX_POINT ( 'NONE', #104027 ) ;
#42915 = ORIENTED_EDGE ( 'NONE', *, *, #82971, .T. ) ;
#42916 =( NAMED_UNIT ( * ) PLANE_ANGLE_UNIT ( ) SI_UNIT ( $, .RADIAN. ) );
#42917 = EDGE_CURVE ( 'NONE', #122079, #12703, #39543, .T. ) ;
#42918 = EDGE_LOOP ( 'NONE', ( #73741, #130986, #85786, #98094 ) ) ;
#42919 = CARTESIAN_POINT ( 'NONE',  ( 59.55793019189811588, 6.110000000000000320, -1.637169565754156064 ) ) ;
#42920 = ORIENTED_EDGE ( 'NONE', *, *, #24005, .F. ) ;
#42921 = LINE ( 'NONE', #21854, #132042 ) ;
#42922 = ORIENTED_EDGE ( 'NONE', *, *, #101338, .T. ) ;
#42923 = CARTESIAN_POINT ( 'NONE',  ( 5.816011393731002066, 28.73617430169783304, 5.000000000000000000 ) ) ;
#42924 = EDGE_CURVE ( 'NONE', #126581, #134968, #27201, .T. ) ;
#42925 = DIRECTION ( 'NONE',  ( -0.000000000000000000, -0.3543493200069152693, 0.9351131265310292928 ) ) ;
#42926 = ORIENTED_EDGE ( 'NONE', *, *, #80434, .F. ) ;
#42927 = CARTESIAN_POINT ( 'NONE',  ( 14.74000000000000021, 2.055000000000001492, 0.000000000000000000 ) ) ;
#42928 = FACE_OUTER_BOUND ( 'NONE', #6768, .T. ) ;
#42929 = PLANE ( 'NONE',  #108053 ) ;
#42930 = VECTOR ( 'NONE', #19606, 1000.000000000000227 ) ;
#42931 = PLANE ( 'NONE',  #87600 ) ;
#42932 = CARTESIAN_POINT ( 'NONE',  ( -33.18398860626899705, 28.73617430169810305, 5.000000000000000000 ) ) ;
#42933 = CARTESIAN_POINT ( 'NONE',  ( -12.79289321881336861, 6.759292476615645917, 5.000000000000000000 ) ) ;
#42934 = DIRECTION ( 'NONE',  ( 0.6830127018922181881, 0.6830127018922202975, -0.2588190451025214056 ) ) ;
#42935 = ORIENTED_EDGE ( 'NONE', *, *, #87182, .F. ) ;
#42936 = EDGE_LOOP ( 'NONE', ( #31021, #72614, #90313, #130181 ) ) ;
#42937 = EDGE_LOOP ( 'NONE', ( #110604, #85702, #31339, #125356, #56123 ) ) ;
#42938 = LINE ( 'NONE', #50950, #142263 ) ;
#42939 = CARTESIAN_POINT ( 'NONE',  ( -30.48921356237309510, -27.52281430457076894, 5.000000000000000000 ) ) ;
#42940 = ORIENTED_EDGE ( 'NONE', *, *, #81548, .T. ) ;
#42941 = ORIENTED_EDGE ( 'NONE', *, *, #46428, .T. ) ;
#42942 = DIRECTION ( 'NONE',  ( 0.000000000000000000, 0.000000000000000000, -1.000000000000000000 ) ) ;
#42943 = LINE ( 'NONE', #87143, #20162 ) ;
#42944 = ADVANCED_FACE ( 'NONE', ( #72198 ), #137415, .F. ) ;
#42945 = EDGE_CURVE ( 'NONE', #5793, #128151, #73500, .T. ) ;
#42946 = DIRECTION ( 'NONE',  ( 0.7071067811865486830, -0.7071067811865464625, -0.000000000000000000 ) ) ;
#42947 = ORIENTED_EDGE ( 'NONE', *, *, #118953, .T. ) ;
#42948 = DIRECTION ( 'NONE',  ( 0.7071067811865487940, -0.7071067811865463515, 0.000000000000000000 ) ) ;
#42949 = VECTOR ( 'NONE', #16608, 1000.000000000000000 ) ;
#42950 = CARTESIAN_POINT ( 'NONE',  ( -25.49999999999982236, -7.420205493532922247, -2.617629953481312111 ) ) ;
#42951 = CARTESIAN_POINT ( 'NONE',  ( 18.73373647476854842, 5.808823158059036373, 5.808823158059032821 ) ) ;
#42952 = VECTOR ( 'NONE', #113799, 1000.000000000000000 ) ;
#42953 = CARTESIAN_POINT ( 'NONE',  ( -57.48921356237308800, -27.52281430457095368, 5.000000000000000000 ) ) ;
#42954 = ORIENTED_EDGE ( 'NONE', *, *, #6618, .F. ) ;
#42955 = CARTESIAN_POINT ( 'NONE',  ( 119.0579301918981230, 6.110000000000001208, -1.637169565754156286 ) ) ;
#42956 = EDGE_CURVE ( 'NONE', #62751, #2459, #118952, .T. ) ;
#42957 = FACE_OUTER_BOUND ( 'NONE', #16244, .T. ) ;
#42958 = PLANE ( 'NONE',  #121352 ) ;
#42960 = VERTEX_POINT ( 'NONE', #138124 ) ;
#42959 = DIRECTION ( 'NONE',  ( -1.000000000000000000, -0.000000000000000000, -0.000000000000000000 ) ) ;
#42961 = LINE ( 'NONE', #32065, #141091 ) ;
#42962 = VERTEX_POINT ( 'NONE', #75726 ) ;
#42963 = AXIS2_PLACEMENT_3D ( 'NONE', #55641, #75265, #75954 ) ;
#42964 = CARTESIAN_POINT ( 'NONE',  ( 75.03752705046288440, -9.735942053221456900E-16, 7.949999999999998401 ) ) ;
#42965 = DIRECTION ( 'NONE',  ( 0.6830127018922181881, 0.6830127018922202975, -0.2588190451025214056 ) ) ;
#42966 = ADVANCED_FACE ( 'NONE', ( #139585 ), #142420, .F. ) ;
#42967 = CARTESIAN_POINT ( 'NONE',  ( 27.18398860626900060, 28.73617430169806042, 5.000000000000000000 ) ) ;
#42969 = EDGE_CURVE ( 'NONE', #37141, #7710, #117754, .T. ) ;
#42968 = VERTEX_POINT ( 'NONE', #109039 ) ;
#42970 = EDGE_CURVE ( 'NONE', #142404, #57387, #107619, .T. ) ;
#42971 = CARTESIAN_POINT ( 'NONE',  ( 2.924914550060625285, 4.584330080086930965E-16, 0.000000000000000000 ) ) ;
#42972 = CARTESIAN_POINT ( 'NONE',  ( -25.01987774928532460, -17.24070752338410983, 20.23474786156463523 ) ) ;
#42973 = ORIENTED_EDGE ( 'NONE', *, *, #28679, .F. ) ;
#42974 = DIRECTION ( 'NONE',  ( -0.7071067811865486830, -0.7071067811865464625, 0.000000000000000000 ) ) ;
#42975 = LINE ( 'NONE', #1547, #35360 ) ;
#42976 = ORIENTED_EDGE ( 'NONE', *, *, #85912, .F. ) ;
#42977 = LINE ( 'NONE', #9585, #46204 ) ;
#42979 = ORIENTED_EDGE ( 'NONE', *, *, #66912, .T. ) ;
#42978 = FACE_OUTER_BOUND ( 'NONE', #16885, .T. ) ;
#42980 = ADVANCED_FACE ( 'NONE', ( #42405 ), #18438, .F. ) ;
#42981 = ORIENTED_EDGE ( 'NONE', *, *, #55618, .T. ) ;
#42982 = CARTESIAN_POINT ( 'NONE',  ( 57.18398860626899705, 28.73617430169827358, 5.000000000000000000 ) ) ;
#42983 = CARTESIAN_POINT ( 'NONE',  ( -66.29974487139159578, -27.71228299555252406, 4.000000000000000000 ) ) ;
#42984 = VERTEX_POINT ( 'NONE', #128670 ) ;
#42985 = SURFACE_STYLE_USAGE ( .BOTH. , #77750 ) ;
#42986 = CARTESIAN_POINT ( 'NONE',  ( 23.99999999999982947, -11.35517001088070366, -1.126524801160051714 ) ) ;
#42987 = FACE_OUTER_BOUND ( 'NONE', #73295, .T. ) ;
#42988 = ORIENTED_EDGE ( 'NONE', *, *, #68952, .F. ) ;
#42989 = FACE_OUTER_BOUND ( 'NONE', #38980, .T. ) ;
#42990 = FACE_OUTER_BOUND ( 'NONE', #49322, .T. ) ;
#42991 = DIRECTION ( 'NONE',  ( 0.000000000000000000, 0.000000000000000000, 1.000000000000000000 ) ) ;
#42992 = FACE_OUTER_BOUND ( 'NONE', #25366, .T. ) ;
#42993 = CARTESIAN_POINT ( 'NONE',  ( 33.01626352523145158, -4.472830434245839371, 4.472830434245839371 ) ) ;
#42994 = CARTESIAN_POINT ( 'NONE',  ( -2.292986735706930457, -21.74070752338405299, 4.999753212805217117 ) ) ;
#42995 = EDGE_LOOP ( 'NONE', ( #63033, #24831, #124697, #134698 ) ) ;
#42996 = ORIENTED_EDGE ( 'NONE', *, *, #12709, .F. ) ;
#42997 = LINE ( 'NONE', #133569, #90559 ) ;
#42998 = ORIENTED_EDGE ( 'NONE', *, *, #4273, .T. ) ;
#42999 = ORIENTED_EDGE ( 'NONE', *, *, #68990, .T. ) ;
#43000 = CARTESIAN_POINT ( 'NONE',  ( 32.99999999999977263, 4.965500833774359357, -4.007596771432733185 ) ) ;
#43001 = CARTESIAN_POINT ( 'NONE',  ( 36.18398860626899705, 28.73617430169812437, 5.000000000000000000 ) ) ;
#43002 = ORIENTED_EDGE ( 'NONE', *, *, #12896, .T. ) ;
#43003 = FILL_AREA_STYLE_COLOUR ( '', #85552 ) ;
#43004 = PLANE ( 'NONE',  #48919 ) ;
#43005 = CARTESIAN_POINT ( 'NONE',  ( -12.18398860626900060, 28.73617430169795739, 5.000000000000000000 ) ) ;
#43006 = CARTESIAN_POINT ( 'NONE',  ( -2.292893218813436995, -15.74070752338412049, 5.000000000000000000 ) ) ;
#43007 = CARTESIAN_POINT ( 'NONE',  ( 26.43999999999999773, 9.521314400968980422E-16, 0.000000000000000000 ) ) ;
#43008 = ORIENTED_EDGE ( 'NONE', *, *, #45645, .F. ) ;
#43009 = CARTESIAN_POINT ( 'NONE',  ( 0.000000000000000000, 0.000000000000000000, 5.000000000000000000 ) ) ;
#43010 =( NAMED_UNIT ( * ) SI_UNIT ( $, .STERADIAN. ) SOLID_ANGLE_UNIT ( ) );
#43011 = DIRECTION ( 'NONE',  ( 0.7071067811865487940, -0.7071067811865463515, 0.000000000000000000 ) ) ;
#43012 = CARTESIAN_POINT ( 'NONE',  ( 32.29289321881323360, -9.740707523384182664, 5.000000000000000000 ) ) ;
#43013 = DIRECTION ( 'NONE',  ( -0.000000000000000000, 0.3543493200069153248, 0.9351131265310292928 ) ) ;
#43014 = CARTESIAN_POINT ( 'NONE',  ( -63.18398860626900415, 28.73617430169831621, 5.000000000000000000 ) ) ;
#43015 = CARTESIAN_POINT ( 'NONE',  ( 54.91252705046288440, -7.949999999999998401, -4.867971026610728450E-16 ) ) ;
#43016 = VECTOR ( 'NONE', #49041, 999.9999999999998863 ) ;
#43017 = EDGE_CURVE ( 'NONE', #78237, #81439, #9727, .T. ) ;
#43018 = CARTESIAN_POINT ( 'NONE',  ( 16.82816939922341604, -8.240707523384196875, 4.000000000000000000 ) ) ;
#43019 = ORIENTED_EDGE ( 'NONE', *, *, #133361, .T. ) ;
#43020 = VERTEX_POINT ( 'NONE', #85152 ) ;
#43021 = CARTESIAN_POINT ( 'NONE',  ( 59.04166666666665719, -3.975000000000002753, 6.884901960086286188 ) ) ;
#43022 = DIRECTION ( 'NONE',  ( 0.7071067811865486830, -0.7071067811865464625, -0.000000000000000000 ) ) ;
#43023 = EDGE_CURVE ( 'NONE', #138242, #52184, #96711, .T. ) ;
#43024 = EDGE_CURVE ( 'NONE', #75139, #53682, #93808, .T. ) ;
#43025 = AXIS2_PLACEMENT_3D ( 'NONE', #19844, #87260, #120559 ) ;
#43026 = DIRECTION ( 'NONE',  ( 0.6830127018922180770, -0.6830127018922204085, -0.2588190451025213501 ) ) ;
#43027 = EDGE_CURVE ( 'NONE', #45976, #13019, #43107, .T. ) ;
#43028 = DIRECTION ( 'NONE',  ( 0.7071067811865487940, -0.7071067811865463515, 0.000000000000000000 ) ) ;
#43029 = VERTEX_POINT ( 'NONE', #30809 ) ;
#43030 = EDGE_CURVE ( 'NONE', #90791, #101471, #140956, .T. ) ;
#43031 = CARTESIAN_POINT ( 'NONE',  ( 81.18398860626899705, 28.73617430169844056, 5.000000000000000000 ) ) ;
#43032 = CARTESIAN_POINT ( 'NONE',  ( 5.999999999999963585, 14.87792677143809783, -11.06722581663438554 ) ) ;
#43033 = CARTESIAN_POINT ( 'NONE',  ( 44.33376352523143993, 6.110000000000001208, 1.122388791418549305E-15 ) ) ;
#43035 = EDGE_CURVE ( 'NONE', #14168, #4072, #19889, .T. ) ;
#43034 = VERTEX_POINT ( 'NONE', #64134 ) ;
#43036 = CARTESIAN_POINT ( 'NONE',  ( -32.20003122016817088, 8.259292476615634371, 16.85664084051848732 ) ) ;
#43037 = ORIENTED_EDGE ( 'NONE', *, *, #30792, .F. ) ;
#43038 = ORIENTED_EDGE ( 'NONE', *, *, #84309, .T. ) ;
#43039 = CARTESIAN_POINT ( 'NONE',  ( 22.49999999999984368, -8.568876922607728375, 4.000000000000000000 ) ) ;
#43040 = CARTESIAN_POINT ( 'NONE',  ( -3.722814304570581712, -21.72499999999999432, 5.000000000000000000 ) ) ;
#43041 = CARTESIAN_POINT ( 'NONE',  ( -14.67183060077637080, -18.74070752338409562, 4.000000000000000000 ) ) ;
#43042 = EDGE_CURVE ( 'NONE', #94963, #110453, #52526, .T. ) ;
#43043 =( LENGTH_UNIT ( ) NAMED_UNIT ( * ) SI_UNIT ( .MILLI., .METRE. ) );
#43044 = ORIENTED_EDGE ( 'NONE', *, *, #85700, .F. ) ;
#43045 = EDGE_CURVE ( 'NONE', #6949, #113816, #75034, .T. ) ;
#43046 = CARTESIAN_POINT ( 'NONE',  ( -5.427106230460724490, -22.22500000000000142, 16.17785463845230609 ) ) ;
#43048 = VERTEX_POINT ( 'NONE', #106903 ) ;
#43047 = DIRECTION ( 'NONE',  ( 1.000000000000000000, 0.000000000000000000, 0.000000000000000000 ) ) ;
#43049 = CARTESIAN_POINT ( 'NONE',  ( 85.45876352523143282, 0.000000000000000000, -6.110000000000001208 ) ) ;
#43050 = CARTESIAN_POINT ( 'NONE',  ( -56.99451991528749062, 28.92564299267978001, 4.000000000000000000 ) ) ;
#43051 = LINE ( 'NONE', #129309, #73262 ) ;
#43052 = CARTESIAN_POINT ( 'NONE',  ( -6.183988606268994381, 28.73617430169791476, 5.000000000000000000 ) ) ;
#43053 = LINE ( 'NONE', #9674, #106494 ) ;
#43054 = FILL_AREA_STYLE_COLOUR ( '', #143381 ) ;
#43055 = EDGE_CURVE ( 'NONE', #140430, #135550, #140265, .T. ) ;
#43056 = AXIS2_PLACEMENT_3D ( 'NONE', #72313, #38217, #136087 ) ;
#43057 = VECTOR ( 'NONE', #82119, 1000.000000000000227 ) ;
#43058 = VERTEX_POINT ( 'NONE', #74305 ) ;
#43059 = VECTOR ( 'NONE', #88740, 1000.000000000000000 ) ;
#43060 = CARTESIAN_POINT ( 'NONE',  ( 21.48921356237309155, -27.52281430457070499, 5.000000000000000000 ) ) ;
#43061 = CARTESIAN_POINT ( 'NONE',  ( 71.66209685856478018, -5.291415217122919401, 3.054999999999997939 ) ) ;
#43062 = VECTOR ( 'NONE', #107368, 999.9999999999998863 ) ;
#43063 = PLANE ( 'NONE',  #55737 ) ;
#43064 = LINE ( 'NONE', #100290, #24601 ) ;
#43065 = DIRECTION ( 'NONE',  ( -0.7071067811865486830, 0.7071067811865464625, 0.000000000000000000 ) ) ;
#43066 = ORIENTED_EDGE ( 'NONE', *, *, #75314, .F. ) ;
#43067 = ORIENTED_EDGE ( 'NONE', *, *, #21136, .T. ) ;
#43068 = VECTOR ( 'NONE', #88826, 1000.000000000000000 ) ;
#43069 = FACE_OUTER_BOUND ( 'NONE', #14026, .T. ) ;
#43070 = CARTESIAN_POINT ( 'NONE',  ( -57.48921356237308800, -27.52281430457095368, 5.000000000000000000 ) ) ;
#43071 = ORIENTED_EDGE ( 'NONE', *, *, #10376, .T. ) ;
#43072 = VERTEX_POINT ( 'NONE', #118494 ) ;
#43073 = DIRECTION ( 'NONE',  ( -0.000000000000000000, -0.3543493200069152693, 0.9351131265310292928 ) ) ;
#43074 = ORIENTED_EDGE ( 'NONE', *, *, #90005, .T. ) ;
#43075 = CARTESIAN_POINT ( 'NONE',  ( 34.92499999999998295, 7.512461875839399283, 4.000000000000000000 ) ) ;
#43076 = LINE ( 'NONE', #86578, #29456 ) ;
#43077 = EDGE_CURVE ( 'NONE', #3834, #43787, #141702, .T. ) ;
#43078 = CARTESIAN_POINT ( 'NONE',  ( 45.18398860626900415, 28.73617430169818832, 5.000000000000000000 ) ) ;
#43079 = FACE_BOUND ( 'NONE', #87202, .T. ) ;
#43080 = CARTESIAN_POINT ( 'NONE',  ( 34.42500000000002558, -21.76999999999999247, -40.00000000000000000 ) ) ;
#43081 = CARTESIAN_POINT ( 'NONE',  ( -29.99451991528749417, 28.92564299267958816, 4.000000000000000000 ) ) ;
#43082 = DIRECTION ( 'NONE',  ( -0.3543493200069163240, 0.000000000000000000, 0.9351131265310288487 ) ) ;
#43084 = ORIENTED_EDGE ( 'NONE', *, *, #13851, .T. ) ;
#43083 = CARTESIAN_POINT ( 'NONE',  ( 50.68336038379622721, -2.130196079827426203, 7.949999999999996625 ) ) ;
#43085 = EDGE_CURVE ( 'NONE', #65778, #131028, #45970, .T. ) ;
#43086 = EDGE_LOOP ( 'NONE', ( #586, #58792, #97106, #79785 ) ) ;
#43087 = VERTEX_POINT ( 'NONE', #132275 ) ;
#43088 = CARTESIAN_POINT ( 'NONE',  ( 80.12043019189810877, 3.055000000000001936, -5.291415217122916737 ) ) ;
#43089 = VERTEX_POINT ( 'NONE', #112628 ) ;
#43090 = DIRECTION ( 'NONE',  ( -0.000000000000000000, 0.3543493200069153248, 0.9351131265310292928 ) ) ;
#43091 = EDGE_CURVE ( 'NONE', #26613, #25521, #122053, .T. ) ;
#43092 = ORIENTED_EDGE ( 'NONE', *, *, #111440, .T. ) ;
#43093 = CARTESIAN_POINT ( 'NONE',  ( -24.18398860626899705, 28.73617430169804265, 5.000000000000000000 ) ) ;
#43094 = COLOUR_RGB ( '', 0.08235294, 0.09019608, 0.10196078) ;
#43095 = B_SPLINE_CURVE_WITH_KNOTS ( 'NONE', 3,
 ( #38297, #18645, #62925, #7777 ),
 .UNSPECIFIED., .F., .F.,
 ( 4, 4 ),
 ( 0.008853860144884201713, 0.009403245473020210854 ),
 .UNSPECIFIED. ) ;
#43096 = DIRECTION ( 'NONE',  ( -0.3543493200069162685, -0.000000000000000000, -0.9351131265310288487 ) ) ;
#43097 = FACE_OUTER_BOUND ( 'NONE', #28229, .T. ) ;
#43098 = LINE ( 'NONE', #108291, #91729 ) ;
#43099 = ADVANCED_FACE ( 'NONE', ( #11129 ), #10439, .T. ) ;
#43100 = LINE ( 'NONE', #40945, #89855 ) ;
#43101 = DIRECTION ( 'NONE',  ( 0.7071067811865486830, -0.7071067811865464625, -0.000000000000000000 ) ) ;
#43102 = CARTESIAN_POINT ( 'NONE',  ( -51.48921356237309510, -27.52281430457091460, 5.000000000000000000 ) ) ;
#43103 = CARTESIAN_POINT ( 'NONE',  ( 2.816011393730999401, 28.73617430169785436, 5.000000000000000000 ) ) ;
#43104 = ORIENTED_EDGE ( 'NONE', *, *, #51044, .F. ) ;
#43105 = CARTESIAN_POINT ( 'NONE',  ( -26.99999999999980815, -0.8619312979532209873, -5.102805207349888406 ) ) ;
#43106 = ORIENTED_EDGE ( 'NONE', *, *, #97898, .T. ) ;
#43107 = LINE ( 'NONE', #63451, #116677 ) ;
#43108 = LINE ( 'NONE', #87314, #83696 ) ;
#43109 = ORIENTED_EDGE ( 'NONE', *, *, #25989, .T. ) ;
#43110 = VERTEX_POINT ( 'NONE', #77181 ) ;
#43111 = ADVANCED_FACE ( 'NONE', ( #33666 ), #88758, .F. ) ;
#43112 = CARTESIAN_POINT ( 'NONE',  ( 39.81293019189809712, -1.637169565754159617, -6.110000000000001208 ) ) ;
#43113 = EDGE_LOOP ( 'NONE', ( #19390, #54239, #21583, #122933 ) ) ;
#43114 = DIRECTION ( 'NONE',  ( 0.000000000000000000, 0.000000000000000000, 1.000000000000000000 ) ) ;
#43115 = VECTOR ( 'NONE', #73576, 1000.000000000000000 ) ;
#43116 = CARTESIAN_POINT ( 'NONE',  ( 80.99451991528748351, 28.92564299267994699, 4.000000000000000000 ) ) ;
#43117 = CARTESIAN_POINT ( 'NONE',  ( 24.83747294953710849, 6.094999999999989981, -1.119633336120465690E-15 ) ) ;
#43118 = CARTESIAN_POINT ( 'NONE',  ( 4.838719539454570118, 11.93618569029472276, -25.72792102991144958 ) ) ;
#43119 = ORIENTED_EDGE ( 'NONE', *, *, #135070, .T. ) ;
#43120 = VECTOR ( 'NONE', #85456, 1000.000000000000000 ) ;
#43121 = CARTESIAN_POINT ( 'NONE',  ( 0.000000000000000000, 0.000000000000000000, 5.000000000000000000 ) ) ;
#43122 = VERTEX_POINT ( 'NONE', #99584 ) ;
#43123 = DIRECTION ( 'NONE',  ( 0.7071067811865487940, 0.7071067811865463515, 0.000000000000000000 ) ) ;
#43125 = VERTEX_POINT ( 'NONE', #264 ) ;
#43124 = DIRECTION ( 'NONE',  ( 1.000000000000000000, 0.000000000000000000, 0.000000000000000000 ) ) ;
#43126 = ORIENTED_EDGE ( 'NONE', *, *, #44322, .F. ) ;
#43127 = DIRECTION ( 'NONE',  ( 0.7071067811865487940, -0.7071067811865463515, 0.000000000000000000 ) ) ;
#43128 = CARTESIAN_POINT ( 'NONE',  ( 25.39999999999999858, -43.14999999999999147, -34.92499999999998295 ) ) ;
#43129 = CARTESIAN_POINT ( 'NONE',  ( 27.53159235450332076, -2.500000000000000444, 3.061616997868384620E-16 ) ) ;
#43130 = ORIENTED_EDGE ( 'NONE', *, *, #112087, .F. ) ;
#43131 = CARTESIAN_POINT ( 'NONE',  ( -3.005480084712505828, 28.92564299267936079, 4.000000000000000000 ) ) ;
#43132 = ORIENTED_EDGE ( 'NONE', *, *, #123740, .T. ) ;
#43134 = ORIENTED_EDGE ( 'NONE', *, *, #120387, .F. ) ;
#43133 = EDGE_CURVE ( 'NONE', #111536, #128174, #69142, .T. ) ;
#43135 = ORIENTED_EDGE ( 'NONE', *, *, #118819, .T. ) ;
#43136 = VECTOR ( 'NONE', #37718, 1000.000000000000000 ) ;
#43137 = CARTESIAN_POINT ( 'NONE',  ( -60.48921356237309510, -27.52281430457097500, 5.000000000000000000 ) ) ;
#43138 = LINE ( 'NONE', #76488, #124888 ) ;
#43139 = DIRECTION ( 'NONE',  ( 1.000000000000000000, 0.000000000000000000, 0.000000000000000000 ) ) ;
#43140 = CARTESIAN_POINT ( 'NONE',  ( 13.60986171580761805, 4.202752102959690472E-16, 0.000000000000000000 ) ) ;
#43142 = EDGE_CURVE ( 'NONE', #28852, #138101, #90900, .T. ) ;
#43141 = CARTESIAN_POINT ( 'NONE',  ( 0.000000000000000000, 0.4000000000000001887, -2.500000000000000000 ) ) ;
#43143 = AXIS2_PLACEMENT_3D ( 'NONE', #12877, #102051, #3421 ) ;
#43144 = VERTEX_POINT ( 'NONE', #79338 ) ;
#43145 = EDGE_CURVE ( 'NONE', #45231, #21649, #68449, .T. ) ;
#43146 = CARTESIAN_POINT ( 'NONE',  ( -30.70710678118631876, -12.74070752338415247, 5.000000000000000000 ) ) ;
#43147 = EDGE_LOOP ( 'NONE', ( #136408, #140959, #1289, #131257 ) ) ;
#43148 = LINE ( 'NONE', #65648, #7731 ) ;
#43149 = VECTOR ( 'NONE', #22674, 1000.000000000000000 ) ;
#43150 = DIRECTION ( 'NONE',  ( 0.000000000000000000, 0.000000000000000000, 1.000000000000000000 ) ) ;
#43151 = VECTOR ( 'NONE', #5706, 999.9999999999998863 ) ;
#43152 = ORIENTED_EDGE ( 'NONE', *, *, #62911, .T. ) ;
#43153 = DIRECTION ( 'NONE',  ( -0.7071067811865486830, -0.7071067811865464625, 0.000000000000000000 ) ) ;
#43154 = DIRECTION ( 'NONE',  ( 1.000000000000000000, 0.000000000000000000, 0.000000000000000000 ) ) ;
#43155 = LINE ( 'NONE', #40998, #30474 ) ;
#43156 = ORIENTED_EDGE ( 'NONE', *, *, #72724, .T. ) ;
#43157 = VERTEX_POINT ( 'NONE', #22035 ) ;
#43158 = CARTESIAN_POINT ( 'NONE',  ( 3.981552653643277928, 18.75929247661552424, 20.33588619593442104 ) ) ;
#43159 = DIRECTION ( 'NONE',  ( -0.000000000000000000, 0.000000000000000000, 1.000000000000000000 ) ) ;
#43160 = DIRECTION ( 'NONE',  ( -0.000000000000000000, 0.000000000000000000, 1.000000000000000000 ) ) ;
#43161 = AXIS2_PLACEMENT_3D ( 'NONE', #74380, #48000, #4393 ) ;
#43162 = DIRECTION ( 'NONE',  ( 0.000000000000000000, 0.000000000000000000, -1.000000000000000000 ) ) ;
#43163 = CARTESIAN_POINT ( 'NONE',  ( 0.000000000000000000, 0.000000000000000000, 5.000000000000000000 ) ) ;
#43164 = CARTESIAN_POINT ( 'NONE',  ( 66.12043019189812298, 3.055000000000002380, -5.291415217122917625 ) ) ;
#43165 = EDGE_CURVE ( 'NONE', #18783, #100866, #111175, .T. ) ;
#43166 = DIRECTION ( 'NONE',  ( 0.7071067811865487940, 0.7071067811865463515, 0.000000000000000000 ) ) ;
#43167 = FILL_AREA_STYLE ('',( #19954 ) ) ;
#43168 = DIRECTION ( 'NONE',  ( -0.7071067811865486830, 0.7071067811865464625, 0.000000000000000000 ) ) ;
#43169 = DIRECTION ( 'NONE',  ( 0.7071067811865486830, -0.7071067811865464625, -0.000000000000000000 ) ) ;
#43170 = ORIENTED_EDGE ( 'NONE', *, *, #118139, .F. ) ;
#43171 = DIRECTION ( 'NONE',  ( -0.7071067811865487940, 0.7071067811865463515, -0.000000000000000000 ) ) ;
#43172 = ORIENTED_EDGE ( 'NONE', *, *, #117963, .T. ) ;
#43173 = CARTESIAN_POINT ( 'NONE',  ( 14.70025512860841133, -27.71228299555195917, 4.000000000000000000 ) ) ;
#43174 = CARTESIAN_POINT ( 'NONE',  ( 32.90156419391743725, 11.25929247661560950, 10.79108189686414399 ) ) ;
#43175 = ORIENTED_EDGE ( 'NONE', *, *, #97347, .F. ) ;
#43176 = CARTESIAN_POINT ( 'NONE',  ( 31.49999999999978684, -20.53675388469227414, 2.352720554255964380 ) ) ;
#43178 = ORIENTED_EDGE ( 'NONE', *, *, #93110, .F. ) ;
#43177 = LINE ( 'NONE', #85952, #118313 ) ;
#43179 = FILL_AREA_STYLE ('',( #21417 ) ) ;
#43180 = CARTESIAN_POINT ( 'NONE',  ( -12.48921356237309155, -27.52281430457064104, 5.000000000000000000 ) ) ;
#43181 = FACE_OUTER_BOUND ( 'NONE', #35037, .T. ) ;
#43182 = ORIENTED_EDGE ( 'NONE', *, *, #38312, .F. ) ;
#43183 = ORIENTED_EDGE ( 'NONE', *, *, #55299, .T. ) ;
#43184 = LINE ( 'NONE', #109129, #83400 ) ;
#43186 = EDGE_CURVE ( 'NONE', #14957, #138468, #138271, .T. ) ;
#43185 = DIRECTION ( 'NONE',  ( 0.7071067811865486830, -0.7071067811865464625, -0.000000000000000000 ) ) ;
#43187 = CARTESIAN_POINT ( 'NONE',  ( -5.999999999999963585, 7.588810512006205933, -3.013526669885213227 ) ) ;
#43188 = CARTESIAN_POINT ( 'NONE',  ( -27.29974487139158512, -27.71228299555225405, 4.000000000000000000 ) ) ;
#43189 = CARTESIAN_POINT ( 'NONE',  ( 82.18336038379619879, -2.130196079827426203, 7.949999999999997513 ) ) ;
#43190 = DIRECTION ( 'NONE',  ( -0.7071067811865486830, 0.7071067811865464625, 0.000000000000000000 ) ) ;
#43191 = EDGE_CURVE ( 'NONE', #105889, #66880, #8645, .T. ) ;
#43192 = CONICAL_SURFACE ( 'NONE', #142721, 2.055000000000001048, 0.9599310885968758145 ) ;
#43193 = CARTESIAN_POINT ( 'NONE',  ( -12.00548008471251293, 28.92564299267929684, 4.000000000000000000 ) ) ;
#43194 = ORIENTED_EDGE ( 'NONE', *, *, #102887, .F. ) ;
#43195 = CARTESIAN_POINT ( 'NONE',  ( 84.41666666666667140, -6.884901960086287076, -3.975000000000000977 ) ) ;
#43196 = PLANE ( 'NONE',  #49298 ) ;
#43197 = EDGE_CURVE ( 'NONE', #10130, #30937, #2403, .T. ) ;
#43198 = FACE_OUTER_BOUND ( 'NONE', #93454, .T. ) ;
#43199 = DIRECTION ( 'NONE',  ( -0.000000000000000000, 0.3543493200069153248, 0.9351131265310292928 ) ) ;
#43200 = AXIS2_PLACEMENT_3D ( 'NONE', #29441, #64234, #108395 ) ;
#43201 = VERTEX_POINT ( 'NONE', #54696 ) ;
#43202 = ADVANCED_FACE ( 'NONE', ( #100334 ), #78580, .T. ) ;
#43203 = ADVANCED_FACE ( 'NONE', ( #67736 ), #93610, .T. ) ;
#43204 = CARTESIAN_POINT ( 'NONE',  ( 10.77958563595370833, 4.584330080086930965E-16, 0.000000000000000000 ) ) ;
#43205 = ORIENTED_EDGE ( 'NONE', *, *, #139127, .T. ) ;
#43206 = CARTESIAN_POINT ( 'NONE',  ( 74.66709685856476142, -3.055000000000000160, -5.291415217122921177 ) ) ;
#43207 = CARTESIAN_POINT ( 'NONE',  ( -0.1839886062690032631, 28.73617430169787568, 5.000000000000000000 ) ) ;
#43208 = AXIS2_PLACEMENT_3D ( 'NONE', #54765, #14076, #101816 ) ;
#43209 = ORIENTED_EDGE ( 'NONE', *, *, #67622, .T. ) ;
#43210 = DIRECTION ( 'NONE',  ( 0.3543493200069162685, -0.000000000000000000, -0.9351131265310288487 ) ) ;
#43211 = FACE_OUTER_BOUND ( 'NONE', #136805, .T. ) ;
#43212 = CARTESIAN_POINT ( 'NONE',  ( 45.48921356237309510, -27.52281430457087197, 5.000000000000000000 ) ) ;
#43213 = EDGE_CURVE ( 'NONE', #48454, #3971, #132987, .T. ) ;
#43214 = DIRECTION ( 'NONE',  ( 0.7071067811865487940, 0.7071067811865463515, -0.000000000000000000 ) ) ;
#43215 = EDGE_CURVE ( 'NONE', #94724, #119206, #56867, .T. ) ;
#43216 = DIRECTION ( 'NONE',  ( -0.7071067811865486830, -0.7071067811865464625, -0.000000000000000000 ) ) ;
#43217 = ORIENTED_EDGE ( 'NONE', *, *, #70993, .T. ) ;
#43218 = CARTESIAN_POINT ( 'NONE',  ( 28.49999999999980105, -13.91253812416061564, 4.000000000000000000 ) ) ;
#43219 = CARTESIAN_POINT ( 'NONE',  ( 7.799999601179139042, 3.821174125832445049E-16, 0.000000000000000000 ) ) ;
#43220 = DIRECTION ( 'NONE',  ( -0.7071067811865486830, 0.7071067811865464625, 0.000000000000000000 ) ) ;
#43221 = DIRECTION ( 'NONE',  ( 0.000000000000000000, 0.000000000000000000, 1.000000000000000000 ) ) ;
#43222 = VERTEX_POINT ( 'NONE', #138679 ) ;
#43223 = EDGE_CURVE ( 'NONE', #84277, #131836, #114132, .T. ) ;
#43224 = ORIENTED_EDGE ( 'NONE', *, *, #34780, .T. ) ;
#43225 = CARTESIAN_POINT ( 'NONE',  ( 66.79209685856477563, -5.291415217122921177, 3.054999999999999272 ) ) ;
#43226 = ORIENTED_EDGE ( 'NONE', *, *, #117113, .F. ) ;
#43227 = VECTOR ( 'NONE', #119499, 1000.000000000000000 ) ;
#43229 = DIRECTION ( 'NONE',  ( 0.7071067811865487940, 0.7071067811865463515, 0.000000000000000000 ) ) ;
#43228 = PRODUCT_DEFINITION_SHAPE ( 'NONE', 'NONE',  #46631 ) ;
#43230 = DIRECTION ( 'NONE',  ( 0.000000000000000000, 0.000000000000000000, 1.000000000000000000 ) ) ;
#43231 = CARTESIAN_POINT ( 'NONE',  ( 24.58521188482543707, 5.410383847852841654, 4.279600586820021313 ) ) ;
#43232 = CARTESIAN_POINT ( 'NONE',  ( -36.48921356237310221, -27.52281430457080802, 5.000000000000000000 ) ) ;
#43233 = VERTEX_POINT ( 'NONE', #49546 ) ;
#43235 = EDGE_CURVE ( 'NONE', #115217, #58332, #26340, .T. ) ;
#43234 = VERTEX_POINT ( 'NONE', #83591 ) ;
#43236 = DIRECTION ( 'NONE',  ( 0.3543493200069163240, -0.000000000000000000, 0.9351131265310288487 ) ) ;
#43237 = DIRECTION ( 'NONE',  ( -0.6830127018922180770, -0.6830127018922204085, -0.2588190451025213501 ) ) ;
#43238 = ORIENTED_EDGE ( 'NONE', *, *, #37881, .F. ) ;
#43239 = AXIS2_PLACEMENT_3D ( 'NONE', #90308, #84465, #50393 ) ;
#43240 = LINE ( 'NONE', #22859, #67488 ) ;
#43241 = LINE ( 'NONE', #9109, #24700 ) ;
#43242 = EDGE_CURVE ( 'NONE', #35082, #116175, #59694, .T. ) ;
#43243 = CARTESIAN_POINT ( 'NONE',  ( 24.41159235450331977, 9.902892378096218942E-16, 0.000000000000000000 ) ) ;
#43244 = ORIENTED_EDGE ( 'NONE', *, *, #89446, .T. ) ;
#43245 = AXIS2_PLACEMENT_3D ( 'NONE', #31462, #87265, #30760 ) ;
#43246 = FACE_OUTER_BOUND ( 'NONE', #95266, .T. ) ;
#43247 = FACE_OUTER_BOUND ( 'NONE', #35507, .T. ) ;
#43248 = ADVANCED_FACE ( 'NONE', ( #104601 ), #93017, .F. ) ;
#43249 = DIRECTION ( 'NONE',  ( 0.7071067811865486830, -0.7071067811865464625, -0.000000000000000000 ) ) ;
#43250 = CARTESIAN_POINT ( 'NONE',  ( 17.24139925780192328, 21.72500000000000142, 5.000000000000000000 ) ) ;
#43251 = EDGE_CURVE ( 'NONE', #134235, #141074, #81459, .T. ) ;
#43252 = DIRECTION ( 'NONE',  ( 1.000000000000000000, 0.000000000000000000, 0.000000000000000000 ) ) ;
#43253 = CIRCLE ( 'NONE', #36308, 2.055000000000001048 ) ;
#43254 = AXIS2_PLACEMENT_3D ( 'NONE', #97209, #29834, #86392 ) ;
#43255 = CARTESIAN_POINT ( 'NONE',  ( 0.1422498215950962208, -0.6000000000000000888, 3.724967290803190334 ) ) ;
#43257 = EDGE_CURVE ( 'NONE', #30995, #94039, #40434, .T. ) ;
#43256 =( LENGTH_UNIT ( ) NAMED_UNIT ( * ) SI_UNIT ( .MILLI., .METRE. ) );
#43258 = ORIENTED_EDGE ( 'NONE', *, *, #110630, .T. ) ;
#43259 = VECTOR ( 'NONE', #91528, 1000.000000000000000 ) ;
#43260 = ORIENTED_EDGE ( 'NONE', *, *, #123353, .T. ) ;
#43261 = CARTESIAN_POINT ( 'NONE',  ( 115.8495968585647802, 6.109999999999996767, 1.637169565754163836 ) ) ;
#43262 = ORIENTED_EDGE ( 'NONE', *, *, #134427, .T. ) ;
#43263 = ORIENTED_EDGE ( 'NONE', *, *, #98828, .T. ) ;
#43264 = AXIS2_PLACEMENT_3D ( 'NONE', #14286, #56417, #58571 ) ;
#43265 = LINE ( 'NONE', #108452, #16662 ) ;
#43266 = FACE_OUTER_BOUND ( 'NONE', #13052, .T. ) ;
#43267 = CARTESIAN_POINT ( 'NONE',  ( -63.29974487139158867, -27.71228299555250274, 4.000000000000000000 ) ) ;
#43268 = EDGE_LOOP ( 'NONE', ( #108855, #31287, #92055, #59139 ) ) ;
#43269 = CARTESIAN_POINT ( 'NONE',  ( -6.183988606268994381, 28.73617430169791476, 5.000000000000000000 ) ) ;
#43270 = DIRECTION ( 'NONE',  ( -0.7071067811865487940, 0.7071067811865463515, -0.000000000000000000 ) ) ;
#43272 = CARTESIAN_POINT ( 'NONE',  ( -20.99999999999984368, 8.816494571476647835, 4.604407763760409722 ) ) ;
#43271 = LINE ( 'NONE', #86771, #8641 ) ;
#43273 = CARTESIAN_POINT ( 'NONE',  ( 9.717577386425601205, -21.73023691814493930, 5.000000000000000888 ) ) ;
#43274 = CARTESIAN_POINT ( 'NONE',  ( 4.288407645496676857, 3.061616997868380183E-16, -2.500000000000001332 ) ) ;
#43275 = EDGE_LOOP ( 'NONE', ( #120400, #52451, #12111, #108849 ) ) ;
#43276 = CARTESIAN_POINT ( 'NONE',  ( -69.48921356237309510, -27.52281430457103895, 5.000000000000000000 ) ) ;
#43277 = DIRECTION ( 'NONE',  ( -0.7071067811865486830, -0.7071067811865464625, 0.000000000000000000 ) ) ;
#43278 = ORIENTED_EDGE ( 'NONE', *, *, #109152, .T. ) ;
#43279 = VERTEX_POINT ( 'NONE', #14740 ) ;
#43280 = EDGE_LOOP ( 'NONE', ( #13943, #42608, #120872, #19234 ) ) ;
#43281 = CARTESIAN_POINT ( 'NONE',  ( 67.66709685856477563, -3.055000000000000160, -5.291415217122921177 ) ) ;
#43282 = VECTOR ( 'NONE', #135308, 1000.000000000000114 ) ;
#43283 = ORIENTED_EDGE ( 'NONE', *, *, #2361, .T. ) ;
#43284 = DIRECTION ( 'NONE',  ( 0.6830127018922180770, -0.6830127018922204085, -0.2588190451025213501 ) ) ;
#43285 = VECTOR ( 'NONE', #56975, 1000.000000000000000 ) ;
#43286 = CARTESIAN_POINT ( 'NONE',  ( -0.6833603837962275440, -1.633150327867691987, -6.094999999999989093 ) ) ;
#43287 = CARTESIAN_POINT ( 'NONE',  ( 99.89626352523141861, 4.472830434245840259, -4.472830434245838482 ) ) ;
#43288 = CARTESIAN_POINT ( 'NONE',  ( 0.1839886062690032631, 28.73617430169787568, 5.000000000000000000 ) ) ;
#43289 = ORIENTED_EDGE ( 'NONE', *, *, #20642, .T. ) ;
#43290 = DIRECTION ( 'NONE',  ( -1.000000000000000000, -1.224606353822377258E-16, -0.000000000000000000 ) ) ;
#43291 = DIRECTION ( 'NONE',  ( 0.000000000000000000, 1.000000000000000000, 5.782411586589357244E-15 ) ) ;
#43292 = CARTESIAN_POINT ( 'NONE',  ( 21.77612515620402078, 4.584330080086930965E-16, 0.000000000000000000 ) ) ;
#43293 = CARTESIAN_POINT ( 'NONE',  ( 14.91508676806229516, -12.74070752338415247, 18.74364270924357712 ) ) ;
#43294 = ORIENTED_EDGE ( 'NONE', *, *, #46501, .F. ) ;
#43295 = DIRECTION ( 'NONE',  ( -0.7071067811865487940, 0.7071067811865463515, 0.000000000000000000 ) ) ;
#43296 = VERTEX_POINT ( 'NONE', #47427 ) ;
#43297 = ORIENTED_EDGE ( 'NONE', *, *, #16848, .T. ) ;
#43298 = ORIENTED_EDGE ( 'NONE', *, *, #47632, .T. ) ;
#43300 = VECTOR ( 'NONE', #83479, 1000.000000000000000 ) ;
#43299 = CARTESIAN_POINT ( 'NONE',  ( 122.1204301918981230, 3.055000000000001936, -5.291415217122916737 ) ) ;
#43301 = ORIENTED_EDGE ( 'NONE', *, *, #114205, .F. ) ;
#43302 = DIRECTION ( 'NONE',  ( 0.7071067811865487940, -0.7071067811865463515, 0.000000000000000000 ) ) ;
#43303 = AXIS2_PLACEMENT_3D ( 'NONE', #22519, #110247, #10927 ) ;
#43304 = EDGE_CURVE ( 'NONE', #22488, #93303, #16127, .T. ) ;
#43305 = DIRECTION ( 'NONE',  ( 0.000000000000000000, -1.000000000000000000, 0.000000000000000000 ) ) ;
#43306 = ORIENTED_EDGE ( 'NONE', *, *, #72048, .F. ) ;
#43307 = EDGE_CURVE ( 'NONE', #32697, #117017, #89069, .T. ) ;
#43308 = LINE ( 'NONE', #109970, #125241 ) ;
#43309 = ORIENTED_EDGE ( 'NONE', *, *, #55817, .F. ) ;
#43310 = VECTOR ( 'NONE', #142245, 1000.000000000000000 ) ;
#43311 = CARTESIAN_POINT ( 'NONE',  ( 14.27040314143522082, -7.934999999999989839, 2.126176841940957907 ) ) ;
#43312 = PRESENTATION_STYLE_ASSIGNMENT (( #52733 ) ) ;
#43313 = FACE_OUTER_BOUND ( 'NONE', #11107, .T. ) ;
#43314 = VECTOR ( 'NONE', #101166, 1000.000000000000227 ) ;
#43315 = ADVANCED_FACE ( 'NONE', ( #59017 ), #121433, .T. ) ;
#43316 = CARTESIAN_POINT ( 'NONE',  ( 39.49999999999999289, 0.000000000000000000, -7.950000000000000178 ) ) ;
#43317 = ORIENTED_EDGE ( 'NONE', *, *, #52655, .F. ) ;
#43318 = ORIENTED_EDGE ( 'NONE', *, *, #45048, .T. ) ;
#43319 = ORIENTED_EDGE ( 'NONE', *, *, #23525, .F. ) ;
#43320 = CARTESIAN_POINT ( 'NONE',  ( 20.12500000000000000, 6.094999999999989981, -1.119633336120465690E-15 ) ) ;
#43321 = DIRECTION ( 'NONE',  ( -0.7071067811865486830, -0.7071067811865464625, 0.000000000000000000 ) ) ;
#43322 = LINE ( 'NONE', #56378, #79814 ) ;
#43323 = LINE ( 'NONE', #142631, #48288 ) ;
#43324 = EDGE_CURVE ( 'NONE', #13983, #122313, #1062, .T. ) ;
#43325 = DIRECTION ( 'NONE',  ( 0.6830127018922181881, 0.6830127018922202975, -0.2588190451025214056 ) ) ;
#43326 = CARTESIAN_POINT ( 'NONE',  ( 31.79209685856476852, -5.291415217122921177, 3.054999999999999272 ) ) ;
#43327 = LINE ( 'NONE', #78814, #55959 ) ;
#43328 = CYLINDRICAL_SURFACE ( 'NONE', #109060, 0.5000000000000004441 ) ;
#43329 = VERTEX_POINT ( 'NONE', #72016 ) ;
#43330 = CARTESIAN_POINT ( 'NONE',  ( -12.20000000000000462, -25.83999999999998565, 2.999999999999999112 ) ) ;
#43331 = ORIENTED_EDGE ( 'NONE', *, *, #111888, .F. ) ;
#43332 = EDGE_CURVE ( 'NONE', #71117, #30243, #125661, .T. ) ;
#43333 = LINE ( 'NONE', #131771, #110081 ) ;
#43334 = ORIENTED_EDGE ( 'NONE', *, *, #131425, .T. ) ;
#43335 = LINE ( 'NONE', #100574, #99200 ) ;
#43337 = ORIENTED_EDGE ( 'NONE', *, *, #82678, .T. ) ;
#43336 = CARTESIAN_POINT ( 'NONE',  ( -54.18398860626899705, 28.73617430169825226, 5.000000000000000000 ) ) ;
#43338 = AXIS2_PLACEMENT_3D ( 'NONE', #68753, #47041, #133987 ) ;
#43339 = CARTESIAN_POINT ( 'NONE',  ( 8.999999999999937828, -9.033600742197648970, 5.000000000000000000 ) ) ;
#43340 = ORIENTED_EDGE ( 'NONE', *, *, #102721, .F. ) ;
#43341 = VERTEX_POINT ( 'NONE', #116196 ) ;
#43342 = CARTESIAN_POINT ( 'NONE',  ( 26.99451991528749417, 28.92564299267956685, 4.000000000000000000 ) ) ;
#43343 = ORIENTED_EDGE ( 'NONE', *, *, #125327, .F. ) ;
#43344 = VECTOR ( 'NONE', #79303, 1000.000000000000000 ) ;
#43345 = VECTOR ( 'NONE', #31822, 1000.000000000000000 ) ;
#43346 = CARTESIAN_POINT ( 'NONE',  ( 93.12086038379622721, -6.884901960086286188, 3.974999999999997424 ) ) ;
#43348 = CARTESIAN_POINT ( 'NONE',  ( 111.2041937171295558, -6.884901960086285300, -3.975000000000000089 ) ) ;
#43347 = AXIS2_PLACEMENT_3D ( 'NONE', #122531, #23198, #100796 ) ;
#43349 = CARTESIAN_POINT ( 'NONE',  ( 29.99999999999979750, 7.552185695429093570, 5.000000000000000000 ) ) ;
#43350 = CARTESIAN_POINT ( 'NONE',  ( 0.000000000000000000, 0.000000000000000000, 5.000000000000000000 ) ) ;
#43351 = FACE_OUTER_BOUND ( 'NONE', #126721, .T. ) ;
#43353 = EDGE_CURVE ( 'NONE', #94037, #131599, #38641, .T. ) ;
#43352 = LINE ( 'NONE', #11381, #5520 ) ;
#43354 = CARTESIAN_POINT ( 'NONE',  ( -31.92499999999997584, 0.4299755680429847016, -27.68972139052992176 ) ) ;
#43355 = CARTESIAN_POINT ( 'NONE',  ( 7.291666666666667851, -3.047499999999994547, 5.278424836066145431 ) ) ;
#43356 = CARTESIAN_POINT ( 'NONE',  ( 20.97873647476855652, -5.808823158059033709, 5.808823158059035485 ) ) ;
#43357 = VECTOR ( 'NONE', #18203, 1000.000000000000114 ) ;
#43358 = CARTESIAN_POINT ( 'NONE',  ( 57.29974487139158157, -27.71228299555246011, 4.000000000000000000 ) ) ;
#43359 = FACE_OUTER_BOUND ( 'NONE', #70181, .T. ) ;
#43360 = ORIENTED_EDGE ( 'NONE', *, *, #2203, .F. ) ;
#43362 = ORIENTED_EDGE ( 'NONE', *, *, #34099, .F. ) ;
#43361 = EDGE_CURVE ( 'NONE', #96026, #88536, #3137, .T. ) ;
#43363 = EDGE_CURVE ( 'NONE', #46867, #6491, #25604, .T. ) ;
#43364 = DIRECTION ( 'NONE',  ( 1.000000000000000000, 0.000000000000000000, 0.000000000000000000 ) ) ;
#43365 = ORIENTED_EDGE ( 'NONE', *, *, #38419, .T. ) ;
#43366 = CARTESIAN_POINT ( 'NONE',  ( 34.92499999999998295, 9.006123077391862353, 4.000000000000000000 ) ) ;
#43367 = CARTESIAN_POINT ( 'NONE',  ( 128.1966263608623251, -51.41954113333838450, -38.53170190052303212 ) ) ;
#43368 = VERTEX_POINT ( 'NONE', #61160 ) ;
#43369 = ADVANCED_FACE ( 'NONE', ( #27036 ), #71282, .F. ) ;
#43370 = DIRECTION ( 'NONE',  ( 0.7071067811865487940, 0.7071067811865463515, -0.000000000000000000 ) ) ;
#43371 = FACE_OUTER_BOUND ( 'NONE', #48120, .T. ) ;
#43372 = CARTESIAN_POINT ( 'NONE',  ( 22.49999999999984368, -4.796895815300995736, -3.611700055028630896 ) ) ;
#43373 = EDGE_CURVE ( 'NONE', #75148, #102362, #50238, .T. ) ;
#43374 = EDGE_CURVE ( 'NONE', #99726, #88219, #133065, .T. ) ;
#43375 = DIRECTION ( 'NONE',  ( -1.000000000000000000, -0.000000000000000000, -0.000000000000000000 ) ) ;
#43377 = ORIENTED_EDGE ( 'NONE', *, *, #117886, .F. ) ;
#43376 = PLANE ( 'NONE',  #61366 ) ;
#43378 = LINE ( 'NONE', #86883, #74444 ) ;
#43379 = VECTOR ( 'NONE', #118510, 1000.000000000000000 ) ;
#43380 = PLANE ( 'NONE',  #36017 ) ;
#43381 = DIRECTION ( 'NONE',  ( -0.7071067811865486830, -0.7071067811865464625, -0.000000000000000000 ) ) ;
#43382 = LINE ( 'NONE', #65883, #95479 ) ;
#43383 = EDGE_LOOP ( 'NONE', ( #115965, #96531, #61473, #95142 ) ) ;
#43384 = ORIENTED_EDGE ( 'NONE', *, *, #62846, .F. ) ;
#43385 = ORIENTED_EDGE ( 'NONE', *, *, #71832, .T. ) ;
#43386 = CARTESIAN_POINT ( 'NONE',  ( 91.29209685856477563, -5.291415217122921177, 3.054999999999999272 ) ) ;
#43387 =( BOUNDED_CURVE ( )  B_SPLINE_CURVE ( 3, ( #100631, #33269, #1279, #143402 ),
 .UNSPECIFIED., .F., .T. ) 
 B_SPLINE_CURVE_WITH_KNOTS ( ( 4, 4 ),
 ( 4.735358278776982566, 4.752060726170251215 ),
 .UNSPECIFIED. ) 
 CURVE ( )  GEOMETRIC_REPRESENTATION_ITEM ( )  RATIONAL_B_SPLINE_CURVE ( ( 1.000000000000000000, 0.9999767524893692361, 0.9999767524893692361, 1.000000000000000000 ) ) 
 REPRESENTATION_ITEM ( '' )  );
#43388 = EDGE_LOOP ( 'NONE', ( #104515, #90814, #27383, #110265 ) ) ;
#43389 = EDGE_CURVE ( 'NONE', #33213, #66785, #108136, .T. ) ;
#43390 = CARTESIAN_POINT ( 'NONE',  ( 128.8595569075059188, -47.26730531257519630, 36.54674188582486494 ) ) ;
#43391 = VECTOR ( 'NONE', #35402, 1000.000000000000000 ) ;
#43392 = CARTESIAN_POINT ( 'NONE',  ( 5.292893218813425449, -9.740707523384184441, 5.000000000000000000 ) ) ;
#43393 = ORIENTED_EDGE ( 'NONE', *, *, #127916, .F. ) ;
#43394 = EDGE_CURVE ( 'NONE', #1311, #32610, #61838, .T. ) ;
#43395 = FACE_OUTER_BOUND ( 'NONE', #89650, .T. ) ;
#43396 = LINE ( 'NONE', #20178, #55864 ) ;
#43397 = CARTESIAN_POINT ( 'NONE',  ( 85.66209685856478018, -5.291415217122919401, 3.054999999999997939 ) ) ;
#43398 = VERTEX_POINT ( 'NONE', #7408 ) ;
#43399 = DIRECTION ( 'NONE',  ( 0.7071067811865487940, 0.7071067811865463515, -0.000000000000000000 ) ) ;
#43400 =( GEOMETRIC_REPRESENTATION_CONTEXT ( 3 ) GLOBAL_UNCERTAINTY_ASSIGNED_CONTEXT ( ( #87009 ) ) GLOBAL_UNIT_ASSIGNED_CONTEXT ( ( #60137, #49970, #126777 ) ) REPRESENTATION_CONTEXT ( 'NONE', 'WORKASPACE' ) );
#43401 = CARTESIAN_POINT ( 'NONE',  ( 116.3541666666666998, -2.130196079827387567, -7.950000000000023270 ) ) ;
#43402 = ORIENTED_EDGE ( 'NONE', *, *, #80680, .F. ) ;
#43403 = EDGE_LOOP ( 'NONE', ( #43788, #116965, #71747, #12449 ) ) ;
#43404 = VERTEX_POINT ( 'NONE', #63284 ) ;
#43405 = CARTESIAN_POINT ( 'NONE',  ( 51.48921356237309510, -27.52281430457091460, 5.000000000000000000 ) ) ;
#43406 = LINE ( 'NONE', #141273, #112642 ) ;
#43407 = CARTESIAN_POINT ( 'NONE',  ( 19.02540314143521982, 2.126176841940962348, 7.934999999999988951 ) ) ;
#43408 = CARTESIAN_POINT ( 'NONE',  ( 0.000000000000000000, 0.000000000000000000, 5.000000000000000000 ) ) ;
#43409 = FACE_OUTER_BOUND ( 'NONE', #71471, .T. ) ;
#43410 = DIRECTION ( 'NONE',  ( -0.6830127018922181881, 0.6830127018922202975, -0.2588190451025214056 ) ) ;
#43411 = EDGE_CURVE ( 'NONE', #3513, #8673, #116902, .T. ) ;
#43413 = EDGE_CURVE ( 'NONE', #63081, #55039, #85687, .T. ) ;
#43412 = FILL_AREA_STYLE ('',( #31818 ) ) ;
#43414 = ORIENTED_EDGE ( 'NONE', *, *, #4287, .F. ) ;
#43415 = AXIS2_PLACEMENT_3D ( 'NONE', #114022, #138646, #125633 ) ;
#43416 = EDGE_LOOP ( 'NONE', ( #134284, #34276, #96263, #85856, #39693 ) ) ;
#43417 = PLANE ( 'NONE',  #61886 ) ;
#43418 = ORIENTED_EDGE ( 'NONE', *, *, #112576, .F. ) ;
#43419 = ORIENTED_EDGE ( 'NONE', *, *, #125135, .F. ) ;
#43420 = EDGE_CURVE ( 'NONE', #89257, #64833, #129929, .T. ) ;
#43421 = AXIS2_PLACEMENT_3D ( 'NONE', #43713, #99492, #77782 ) ;
#43422 = DIRECTION ( 'NONE',  ( -0.3543493200069162685, -0.000000000000000000, -0.9351131265310288487 ) ) ;
#43423 = EDGE_LOOP ( 'NONE', ( #140290, #7013, #10561 ) ) ;
#43424 = CARTESIAN_POINT ( 'NONE',  ( 55.97916666666666430, -7.950000000000000178, 2.130196079827424427 ) ) ;
#43425 = PLANE ( 'NONE',  #53193 ) ;
#43426 = CARTESIAN_POINT ( 'NONE',  ( 17.07999999999999829, 2.055000000000001492, 2.516649172247811554E-16 ) ) ;
#43427 = DIRECTION ( 'NONE',  ( 1.000000000000000000, 0.000000000000000000, 0.000000000000000000 ) ) ;
#43428 = AXIS2_PLACEMENT_3D ( 'NONE', #34728, #91945, #102132 ) ;
#43429 = DIRECTION ( 'NONE',  ( -0.7071067811865486830, 0.7071067811865464625, -0.000000000000000000 ) ) ;
#43430 = VERTEX_POINT ( 'NONE', #9542 ) ;
#43431 = LINE ( 'NONE', #84789, #23307 ) ;
#43432 = EDGE_LOOP ( 'NONE', ( #107194, #27398, #99360, #44899 ) ) ;
#43433 = CARTESIAN_POINT ( 'NONE',  ( 19.92044161110034750, -3.134395820719624748, -35.08047115841593921 ) ) ;
#43434 = ORIENTED_EDGE ( 'NONE', *, *, #21501, .T. ) ;
#43435 = CARTESIAN_POINT ( 'NONE',  ( 117.0375270504628986, -9.735942053221456900E-16, 7.949999999999998401 ) ) ;
#43436 = ORIENTED_EDGE ( 'NONE', *, *, #119112, .T. ) ;
#43437 = CARTESIAN_POINT ( 'NONE',  ( -4.499999999999968914, 14.14708470758590764, -0.5283514160166454809 ) ) ;
#43438 = EDGE_LOOP ( 'NONE', ( #53200, #125121, #129098, #54475 ) ) ;
#43439 = VERTEX_POINT ( 'NONE', #41474 ) ;
#43440 = CIRCLE ( 'NONE', #75845, 2.055000000000000604 ) ;
#43441 = EDGE_LOOP ( 'NONE', ( #27018, #15421, #118352, #50687 ) ) ;
#43442 = AXIS2_PLACEMENT_3D ( 'NONE', #126326, #113295, #69853 ) ;
#43443 = VECTOR ( 'NONE', #38229, 1000.000000000000000 ) ;
#43444 = CARTESIAN_POINT ( 'NONE',  ( 66.48921356237309510, -27.52281430457101763, 5.000000000000000000 ) ) ;
#43445 = LINE ( 'NONE', #110104, #27511 ) ;
#43446 = DIRECTION ( 'NONE',  ( 0.7071067811865486830, -0.7071067811865464625, -0.000000000000000000 ) ) ;
#43447 = DIRECTION ( 'NONE',  ( -0.7071067811865486830, -0.7071067811865464625, 0.000000000000000000 ) ) ;
#43448 = CARTESIAN_POINT ( 'NONE',  ( -12.70710678118645909, 8.259292476615636147, 5.000000000000000000 ) ) ;
#43450 = EDGE_CURVE ( 'NONE', #86643, #50077, #88323, .T. ) ;
#43449 = DIRECTION ( 'NONE',  ( 0.000000000000000000, 1.000000000000000000, 0.000000000000000000 ) ) ;
#43451 = DIRECTION ( 'NONE',  ( -0.3543493200069163240, -0.000000000000000000, 0.9351131265310288487 ) ) ;
#43452 = LINE ( 'NONE', #143461, #141869 ) ;
#43453 = CARTESIAN_POINT ( 'NONE',  ( 18.18398860626898994, 28.73617430169800002, 5.000000000000000000 ) ) ;
#43454 = CARTESIAN_POINT ( 'NONE',  ( 17.85999999999999943, -2.055000000000000160, 2.789133085058098087E-16 ) ) ;
#43455 = CARTESIAN_POINT ( 'NONE',  ( 2.994519915287485734, 28.92564299267940342, 4.000000000000000000 ) ) ;
#43456 = ORIENTED_EDGE ( 'NONE', *, *, #74363, .F. ) ;
#43457 = ORIENTED_EDGE ( 'NONE', *, *, #41539, .T. ) ;
#43458 = ORIENTED_EDGE ( 'NONE', *, *, #61617, .F. ) ;
#43459 = CARTESIAN_POINT ( 'NONE',  ( 11.20710678118646797, 15.75929247661555976, 5.000000000000000000 ) ) ;
#43460 = VERTEX_POINT ( 'NONE', #119039 ) ;
#43462 = EDGE_LOOP ( 'NONE', ( #71775, #3814, #1102, #89208 ) ) ;
#43461 = ADVANCED_FACE ( 'NONE', ( #53057 ), #84314, .T. ) ;
#43463 = DIRECTION ( 'NONE',  ( -0.7071067811865487940, 0.7071067811865463515, -0.000000000000000000 ) ) ;
#43464 = CARTESIAN_POINT ( 'NONE',  ( 10.49999999999993605, 16.46639925780209524, 5.000000000000000000 ) ) ;
#43465 = EDGE_CURVE ( 'NONE', #1803, #11699, #29878, .T. ) ;
#43466 = CARTESIAN_POINT ( 'NONE',  ( 30.48921356237309510, -27.52281430457076894, 5.000000000000000000 ) ) ;
#43467 = VERTEX_POINT ( 'NONE', #98018 ) ;
#43468 = AXIS2_PLACEMENT_3D ( 'NONE', #38658, #82888, #131695 ) ;
#43469 = CARTESIAN_POINT ( 'NONE',  ( -66.18398860626901126, 28.73617430169833753, 5.000000000000000000 ) ) ;
#43470 = ORIENTED_EDGE ( 'NONE', *, *, #27940, .T. ) ;
#43472 = EDGE_CURVE ( 'NONE', #75329, #61250, #42938, .T. ) ;
#43471 = PLANE ( 'NONE',  #76962 ) ;
#43473 = EDGE_CURVE ( 'NONE', #65849, #8597, #128120, .T. ) ;
#43474 = FACE_OUTER_BOUND ( 'NONE', #30737, .T. ) ;
#43475 = COLOUR_RGB ( '', 0.66274510, 0.83137255, 0.94901961) ;
#43476 = CARTESIAN_POINT ( 'NONE',  ( 23.25456980810188767, -6.871911579029512218, 3.967499999999996252 ) ) ;
#43477 = VERTEX_POINT ( 'NONE', #29179 ) ;
#43478 = CARTESIAN_POINT ( 'NONE',  ( 93.39126352523143737, -4.472830434245839371, -4.472830434245839371 ) ) ;
#43479 = CARTESIAN_POINT ( 'NONE',  ( 10.03605673236671869, -8.432637487761464712, -4.375000000000002665 ) ) ;
#43480 = EDGE_CURVE ( 'NONE', #81439, #112461, #19602, .T. ) ;
#43481 = PLANE ( 'NONE',  #106834 ) ;
#43482 = LINE ( 'NONE', #87693, #25701 ) ;
#43483 = VERTEX_POINT ( 'NONE', #95861 ) ;
#43484 = ORIENTED_EDGE ( 'NONE', *, *, #83419, .T. ) ;
#43485 = EDGE_LOOP ( 'NONE', ( #133572, #142327, #115421, #113660 ) ) ;
#43486 = FACE_OUTER_BOUND ( 'NONE', #139227, .T. ) ;
#43487 = DIRECTION ( 'NONE',  ( 0.7071067811865486830, -0.7071067811865464625, -0.000000000000000000 ) ) ;
#43488 = LINE ( 'NONE', #65989, #86710 ) ;
#43489 = ORIENTED_EDGE ( 'NONE', *, *, #35989, .F. ) ;
#43490 = DIRECTION ( 'NONE',  ( -0.3543493200069162685, -0.000000000000000000, -0.9351131265310288487 ) ) ;
#43491 = EDGE_CURVE ( 'NONE', #133481, #111466, #140108, .T. ) ;
#43492 = FACE_OUTER_BOUND ( 'NONE', #62771, .T. ) ;
#43493 = LINE ( 'NONE', #87708, #65354 ) ;
#43494 = ORIENTED_EDGE ( 'NONE', *, *, #31901, .F. ) ;
#43495 = CARTESIAN_POINT ( 'NONE',  ( 7.499999999999940492, -14.56887692260766443, 4.000000000000000000 ) ) ;
#43496 = EDGE_CURVE ( 'NONE', #89022, #37569, #19021, .T. ) ;
#43497 = CARTESIAN_POINT ( 'NONE',  ( -33.70710678118631165, 20.25929247661551713, 5.000000000000000000 ) ) ;
#43498 = EDGE_LOOP ( 'NONE', ( #31315, #10286, #8855, #99210 ) ) ;
#43500 = EDGE_LOOP ( 'NONE', ( #107245, #65034, #31988, #134595 ) ) ;
#43499 = DIRECTION ( 'NONE',  ( -0.7071067811865487940, 0.7071067811865463515, -0.000000000000000000 ) ) ;
#43501 = EDGE_LOOP ( 'NONE', ( #121487, #106453, #120983, #66241 ) ) ;
#43502 = LINE ( 'NONE', #55832, #60993 ) ;
#43503 = CARTESIAN_POINT ( 'NONE',  ( 61.46640106136302961, -1.600000000000086020, -34.92499999999998295 ) ) ;
#43504 = EDGE_CURVE ( 'NONE', #94991, #118382, #55226, .T. ) ;
#43505 = ORIENTED_EDGE ( 'NONE', *, *, #133372, .F. ) ;
#43506 = CARTESIAN_POINT ( 'NONE',  ( 12.48921356237309155, -27.52281430457064104, 5.000000000000000000 ) ) ;
#43507 = UNCERTAINTY_MEASURE_WITH_UNIT (LENGTH_MEASURE( 1.000000000000000082E-05 ), #29495, 'distance_accuracy_value', 'NONE');
#43508 = LINE ( 'NONE', #121056, #114608 ) ;
#43509 = CYLINDRICAL_SURFACE ( 'NONE', #117796, 2.500000000000000444 ) ;
#43510 = CARTESIAN_POINT ( 'NONE',  ( -15.48921356237309510, -27.52281430457066236, 5.000000000000000000 ) ) ;
#43511 = CARTESIAN_POINT ( 'NONE',  ( 0.1599999999999984490, -7.872400080523645371, -1.050197800354446098 ) ) ;
#43512 = DIRECTION ( 'NONE',  ( 0.7071067811865486830, -0.7071067811865464625, -0.000000000000000000 ) ) ;
#43514 = EDGE_CURVE ( 'NONE', #29884, #16309, #67555, .T. ) ;
#43513 = LINE ( 'NONE', #100048, #116576 ) ;
#43515 = PLANE ( 'NONE',  #71529 ) ;
#43516 = CARTESIAN_POINT ( 'NONE',  ( 0.7928932188134502068, 18.75929247661552779, 5.000000000000000000 ) ) ;
#43517 = DIRECTION ( 'NONE',  ( 0.000000000000000000, 0.000000000000000000, -1.000000000000000000 ) ) ;
#43518 = DIRECTION ( 'NONE',  ( -0.6830127018922181881, 0.6830127018922202975, -0.2588190451025214056 ) ) ;
#43519 = CARTESIAN_POINT ( 'NONE',  ( 110.6666666666666572, 6.884901960086285300, 3.975000000000003642 ) ) ;
#43520 = CARTESIAN_POINT ( 'NONE',  ( -34.17183060077623225, -14.24070752338413293, 4.000000000000000000 ) ) ;
#43521 = ORIENTED_EDGE ( 'NONE', *, *, #122457, .F. ) ;
#43522 = ORIENTED_EDGE ( 'NONE', *, *, #12634, .F. ) ;
#43523 = ADVANCED_FACE ( 'NONE', ( #100165 ), #45104, .F. ) ;
#43524 = CARTESIAN_POINT ( 'NONE',  ( 105.1250000000000000, -7.950000000000000178, -4.867971026610729436E-16 ) ) ;
#43525 = VECTOR ( 'NONE', #92194, 1000.000000000000000 ) ;
#43526 = ORIENTED_EDGE ( 'NONE', *, *, #39170, .T. ) ;
#43527 = ORIENTED_EDGE ( 'NONE', *, *, #36977, .T. ) ;
#43528 = EDGE_CURVE ( 'NONE', #10002, #37807, #123359, .T. ) ;
#43529 = ORIENTED_EDGE ( 'NONE', *, *, #66169, .F. ) ;
#43530 = LINE ( 'NONE', #19631, #24761 ) ;
#43531 = DIRECTION ( 'NONE',  ( 1.000000000000000000, 0.000000000000000000, 0.000000000000000000 ) ) ;
#43532 = VERTEX_POINT ( 'NONE', #814 ) ;
#43533 = VECTOR ( 'NONE', #85175, 1000.000000000000000 ) ;
#43534 = CARTESIAN_POINT ( 'NONE',  ( -4.499999999999962697, 8.319652575858382804, -8.582050562765838109 ) ) ;
#43535 = EDGE_CURVE ( 'NONE', #92108, #26770, #21160, .T. ) ;
#43536 = CARTESIAN_POINT ( 'NONE',  ( -24.18398860626899705, 28.73617430169804265, 5.000000000000000000 ) ) ;
#43537 = VECTOR ( 'NONE', #28464, 1000.000000000000000 ) ;
#43538 = DIRECTION ( 'NONE',  ( -0.7071067811865486830, -0.7071067811865464625, 0.000000000000000000 ) ) ;
#43539 = CARTESIAN_POINT ( 'NONE',  ( -34.64175702458838657, 15.75929247661555088, 19.34181609438707738 ) ) ;
#43540 = ORIENTED_EDGE ( 'NONE', *, *, #107764, .F. ) ;
#43541 = LINE ( 'NONE', #74771, #18684 ) ;
#43542 = DIRECTION ( 'NONE',  ( 1.000000000000000000, 0.000000000000000000, 0.000000000000000000 ) ) ;
#43544 = DIRECTION ( 'NONE',  ( 0.6830127018922180770, -0.6830127018922204085, -0.2588190451025213501 ) ) ;
#43543 = AXIS2_PLACEMENT_3D ( 'NONE', #73412, #41468, #117576 ) ;
#43545 = CARTESIAN_POINT ( 'NONE',  ( 8.999999999999937828, 18.08204922493374767, 0.9627537363044690322 ) ) ;
#43546 = DIRECTION ( 'NONE',  ( -0.7071067811865487940, 0.7071067811865463515, -0.000000000000000000 ) ) ;
#43547 = CARTESIAN_POINT ( 'NONE',  ( 26.91252705046288796, -7.949999999999998401, -4.867971026610728450E-16 ) ) ;
#43548 = LINE ( 'NONE', #55151, #79305 ) ;
#43549 = VERTEX_POINT ( 'NONE', #79157 ) ;
#43550 = ORIENTED_EDGE ( 'NONE', *, *, #109366, .F. ) ;
#43551 = CARTESIAN_POINT ( 'NONE',  ( 121.4795968585647614, 6.109999999999999432, 1.637169565754164280 ) ) ;
#43552 = EDGE_LOOP ( 'NONE', ( #98572, #77869, #131187, #13926 ) ) ;
#43553 = EDGE_CURVE ( 'NONE', #132816, #2809, #89278, .T. ) ;
#43554 = PLANE ( 'NONE',  #18484 ) ;
#43555 = LINE ( 'NONE', #20350, #94177 ) ;
#43556 = CARTESIAN_POINT ( 'NONE',  ( -27.48921356237309155, -27.52281430457074762, 5.000000000000000000 ) ) ;
#43557 = EDGE_CURVE ( 'NONE', #64166, #11127, #133504, .T. ) ;
#43558 = DIRECTION ( 'NONE',  ( 0.000000000000000000, 0.000000000000000000, -1.000000000000000000 ) ) ;
#43559 = LINE ( 'NONE', #32705, #23487 ) ;
#43560 =( NAMED_UNIT ( * ) PLANE_ANGLE_UNIT ( ) SI_UNIT ( $, .RADIAN. ) );
#43561 = CARTESIAN_POINT ( 'NONE',  ( 115.2662635252314374, 4.472830434245839371, -4.472830434245838482 ) ) ;
#43562 = ORIENTED_EDGE ( 'NONE', *, *, #13274, .F. ) ;
#43563 = ORIENTED_EDGE ( 'NONE', *, *, #103934, .T. ) ;
#43564 = CARTESIAN_POINT ( 'NONE',  ( -11.99999999999991296, 20.70535890316560312, 1.956823837851944470 ) ) ;
#43565 = DIRECTION ( 'NONE',  ( -0.000000000000000000, 0.000000000000000000, 1.000000000000000000 ) ) ;
#43566 = CIRCLE ( 'NONE', #50506, 2.500000000000000888 ) ;
#43567 = VERTEX_POINT ( 'NONE', #122603 ) ;
#43568 = ORIENTED_EDGE ( 'NONE', *, *, #44045, .T. ) ;
#43569 = CARTESIAN_POINT ( 'NONE',  ( 34.70876352523143282, -7.482591942790329030E-16, 6.110000000000001208 ) ) ;
#43570 = ORIENTED_EDGE ( 'NONE', *, *, #10182, .T. ) ;
#43571 = FACE_OUTER_BOUND ( 'NONE', #13454, .T. ) ;
#43572 = ADVANCED_FACE ( 'NONE', ( #75 ), #44378, .F. ) ;
#43573 = DIRECTION ( 'NONE',  ( -0.3543493200069163240, -0.000000000000000000, -0.9351131265310288487 ) ) ;
#43574 = AXIS2_PLACEMENT_3D ( 'NONE', #21144, #38805, #82321 ) ;
#43575 = CARTESIAN_POINT ( 'NONE',  ( -14.99999999999988098, -22.06887692260758982, 4.000000000000000000 ) ) ;
#43576 = CARTESIAN_POINT ( 'NONE',  ( 38.70376352523144448, 6.109999999999998543, 1.122388791418548911E-15 ) ) ;
#43577 = ORIENTED_EDGE ( 'NONE', *, *, #92487, .T. ) ;
#43578 = CARTESIAN_POINT ( 'NONE',  ( 25.49999999999982592, 12.43112307739206024, 4.000000000000000000 ) ) ;
#43579 = VERTEX_POINT ( 'NONE', #13116 ) ;
#43580 = VERTEX_POINT ( 'NONE', #54530 ) ;
#43581 = VECTOR ( 'NONE', #58668, 1000.000000000000000 ) ;
#43582 = ORIENTED_EDGE ( 'NONE', *, *, #91700, .T. ) ;
#43583 = EDGE_CURVE ( 'NONE', #104658, #20345, #2223, .T. ) ;
#43584 = VECTOR ( 'NONE', #122118, 999.9999999999998863 ) ;
#43585 = EDGE_CURVE ( 'NONE', #4021, #131028, #88585, .T. ) ;
#43586 = DIRECTION ( 'NONE',  ( 0.000000000000000000, -1.000000000000000000, 0.000000000000000000 ) ) ;
#43587 = EDGE_LOOP ( 'NONE', ( #51171, #43582, #131710, #90492, #30493, #56979 ) ) ;
#43588 = CARTESIAN_POINT ( 'NONE',  ( 1.353980332882009252, 4.584330080086930965E-16, 0.000000000000000000 ) ) ;
#43589 = LINE ( 'NONE', #142904, #82629 ) ;
#43590 =( LENGTH_UNIT ( ) NAMED_UNIT ( * ) SI_UNIT ( .MILLI., .METRE. ) );
#43591 = CARTESIAN_POINT ( 'NONE',  ( -77.99451991528749772, 28.92564299267992567, 4.000000000000000000 ) ) ;
#43592 = FACE_BOUND ( 'NONE', #128021, .T. ) ;
#43594 = EDGE_CURVE ( 'NONE', #68410, #65170, #43621, .T. ) ;
#43593 = ORIENTED_EDGE ( 'NONE', *, *, #89660, .T. ) ;
#43595 = DIRECTION ( 'NONE',  ( 0.000000000000000000, 0.000000000000000000, 1.000000000000000000 ) ) ;
#43596 = DIRECTION ( 'NONE',  ( -1.000000000000000000, -1.224606353822377258E-16, -0.000000000000000000 ) ) ;
#43597 = CARTESIAN_POINT ( 'NONE',  ( 0.005480084712502889671, 28.92564299267938210, 4.000000000000000000 ) ) ;
#43598 = ORIENTED_EDGE ( 'NONE', *, *, #53196, .F. ) ;
#43599 = CARTESIAN_POINT ( 'NONE',  ( 25.26393171409163330, 4.523673662833495257, 4.354767379111166292 ) ) ;
#43600 = ORIENTED_EDGE ( 'NONE', *, *, #136575, .F. ) ;
#43601 = EDGE_LOOP ( 'NONE', ( #71905, #14008, #80422, #82995, #61269 ) ) ;
#43602 = ORIENTED_EDGE ( 'NONE', *, *, #35920, .T. ) ;
#43603 = CARTESIAN_POINT ( 'NONE',  ( 49.49543019189811588, 5.291415217122916737, 3.055000000000001936 ) ) ;
#43604 = EDGE_LOOP ( 'NONE', ( #62526, #121628, #80534, #10996, #73229, #51929 ) ) ;
#43605 = AXIS2_PLACEMENT_3D ( 'NONE', #50232, #60409, #27029 ) ;
#43606 = CARTESIAN_POINT ( 'NONE',  ( 27.18398860626900060, 28.73617430169806042, 5.000000000000000000 ) ) ;
#43607 = CARTESIAN_POINT ( 'NONE',  ( -14.99451991528749595, 28.92564299267948513, 4.000000000000000000 ) ) ;
#43608 = CARTESIAN_POINT ( 'NONE',  ( 69.48921356237309510, -27.52281430457103895, 5.000000000000000000 ) ) ;
#43609 = ORIENTED_EDGE ( 'NONE', *, *, #49006, .T. ) ;
#43610 = LINE ( 'NONE', #123344, #35311 ) ;
#43611 = DIRECTION ( 'NONE',  ( 0.7071067811865486830, -0.7071067811865464625, -0.000000000000000000 ) ) ;
#43612 = PLANE ( 'NONE',  #142751 ) ;
#43613 = DIRECTION ( 'NONE',  ( -0.6830127018922180770, -0.6830127018922204085, -0.2588190451025213501 ) ) ;
#43614 = FACE_OUTER_BOUND ( 'NONE', #126286, .T. ) ;
#43615 = FACE_OUTER_BOUND ( 'NONE', #73674, .T. ) ;
#43616 = CARTESIAN_POINT ( 'NONE',  ( 0.000000000000000000, 0.000000000000000000, 5.000000000000000000 ) ) ;
#43617 = ORIENTED_EDGE ( 'NONE', *, *, #9406, .F. ) ;
#43618 = EDGE_CURVE ( 'NONE', #115783, #949, #100860, .T. ) ;
#43619 = ORIENTED_EDGE ( 'NONE', *, *, #16119, .T. ) ;
#43620 = EDGE_LOOP ( 'NONE', ( #134121, #821, #10295, #7035 ) ) ;
#43621 = LINE ( 'NONE', #46539, #17229 ) ;
#43622 = VECTOR ( 'NONE', #7000, 999.9999999999998863 ) ;
#43624 = CARTESIAN_POINT ( 'NONE',  ( 16.49999999999988987, -1.592773361805348342, -6.492772025301264627 ) ) ;
#43623 = VECTOR ( 'NONE', #141354, 1000.000000000000000 ) ;
#43625 = VERTEX_POINT ( 'NONE', #10269 ) ;
#43627 = VERTEX_POINT ( 'NONE', #98709 ) ;
#43626 = VECTOR ( 'NONE', #88549, 1000.000000000000000 ) ;
#43628 = DIRECTION ( 'NONE',  ( 0.000000000000000000, 0.000000000000000000, 1.000000000000000000 ) ) ;
#43629 = FACE_OUTER_BOUND ( 'NONE', #74810, .T. ) ;
#43630 = VECTOR ( 'NONE', #111408, 1000.000000000000000 ) ;
#43631 = EDGE_CURVE ( 'NONE', #2199, #96833, #55965, .T. ) ;
#43632 = ADVANCED_FACE ( 'NONE', ( #66813 ), #76270, .F. ) ;
#43633 = DIRECTION ( 'NONE',  ( 0.7071067811865487940, 0.7071067811865463515, 0.000000000000000000 ) ) ;
#43634 = VERTEX_POINT ( 'NONE', #87846 ) ;
#43635 = LINE ( 'NONE', #78416, #30125 ) ;
#43636 = AXIS2_PLACEMENT_3D ( 'NONE', #114571, #124747, #124044 ) ;
#43637 = VECTOR ( 'NONE', #121226, 1000.000000000000000 ) ;
#43639 = EDGE_CURVE ( 'NONE', #71793, #5240, #54314, .T. ) ;
#43638 = DIRECTION ( 'NONE',  ( -0.6830127018922181881, 0.6830127018922202975, -0.2588190451025214056 ) ) ;
#43640 = EDGE_CURVE ( 'NONE', #79902, #125706, #21870, .T. ) ;
#43641 = CARTESIAN_POINT ( 'NONE',  ( 14.21290314143522160, 3.967499999999992699, -6.871911579029513994 ) ) ;
#43642 = PLANE ( 'NONE',  #32308 ) ;
#43643 = ADVANCED_FACE ( 'NONE', ( #15944 ), #126873, .F. ) ;
#43644 = ORIENTED_EDGE ( 'NONE', *, *, #5245, .T. ) ;
#43645 = CARTESIAN_POINT ( 'NONE',  ( 116.5787635252314516, -7.482591942790327058E-16, 6.109999999999999432 ) ) ;
#43646 = EDGE_CURVE ( 'NONE', #66484, #132969, #132757, .T. ) ;
#43647 = DIRECTION ( 'NONE',  ( 0.000000000000000000, -1.000000000000000000, 0.000000000000000000 ) ) ;
#43648 = CARTESIAN_POINT ( 'NONE',  ( 26.53839644629413286, -9.740707523384177335, 17.74957260769616951 ) ) ;
#43650 = ORIENTED_EDGE ( 'NONE', *, *, #134544, .T. ) ;
#43649 = DIRECTION ( 'NONE',  ( 0.7071067811865487940, 0.7071067811865463515, 0.000000000000000000 ) ) ;
#43651 = CARTESIAN_POINT ( 'NONE',  ( 66.57919371712955581, 3.975000000000002753, -6.884901960086283523 ) ) ;
#43652 = ORIENTED_EDGE ( 'NONE', *, *, #65123, .T. ) ;
#43653 = ADVANCED_FACE ( 'NONE', ( #103683 ), #79875, .T. ) ;
#43654 = CARTESIAN_POINT ( 'NONE',  ( 51.48921356237309510, -27.52281430457091460, 5.000000000000000000 ) ) ;
#43655 = CARTESIAN_POINT ( 'NONE',  ( 38.99451991528749062, 28.92564299267965211, 4.000000000000000000 ) ) ;
#43657 = VERTEX_POINT ( 'NONE', #102320 ) ;
#43656 =( BOUNDED_CURVE ( )  B_SPLINE_CURVE ( 2, ( #76423, #131508, #132244, #74277, #88733, #32190, #85845, #65573, #32935, #99558, #31481, #43083, #43781 ),
 .UNSPECIFIED., .F., .T. ) 
 B_SPLINE_CURVE_WITH_KNOTS ( ( 3, 2, 2, 2, 2, 2, 3 ),
 ( 0.7333333333333332815, 0.7361111111111111605, 0.7388888888888889284, 0.7416666666666666963, 0.7444444444444444642, 0.7472222222222222321, 0.7500000000000000000 ),
 .UNSPECIFIED. ) 
 CURVE ( )  GEOMETRIC_REPRESENTATION_ITEM ( )  RATIONAL_B_SPLINE_CURVE ( ( 1.000000000000000000, 0.9659258262890683122, 1.000000000000000000, 0.9659258262890683122, 1.000000000000000000, 0.9659258262890683122, 1.000000000000000000, 0.9659258262890683122, 1.000000000000000000, 0.9659258262890683122, 1.000000000000000000, 0.9659258262890683122, 1.000000000000000000 ) ) 
 REPRESENTATION_ITEM ( '' )  );
#43658 = EDGE_CURVE ( 'NONE', #92295, #133006, #47946, .T. ) ;
#43659 = CARTESIAN_POINT ( 'NONE',  ( -11.20710678118646442, -8.240707523384198652, 5.000000000000000000 ) ) ;
#43660 = CARTESIAN_POINT ( 'NONE',  ( 57.29974487139158157, -27.71228299555246011, 4.000000000000000000 ) ) ;
#43661 = VERTEX_POINT ( 'NONE', #24724 ) ;
#43662 = VECTOR ( 'NONE', #73147, 1000.000000000000000 ) ;
#43663 = LINE ( 'NONE', #19056, #101795 ) ;
#43664 =( BOUNDED_CURVE ( )  B_SPLINE_CURVE ( 3, ( #83884, #7694, #130224, #128089 ),
 .UNSPECIFIED., .F., .T. ) 
 B_SPLINE_CURVE_WITH_KNOTS ( ( 4, 4 ),
 ( 1.500914606003786567, 1.515984175831967429 ),
 .UNSPECIFIED. ) 
 CURVE ( )  GEOMETRIC_REPRESENTATION_ITEM ( )  RATIONAL_B_SPLINE_CURVE ( ( 1.000000000000000000, 0.9999810757616318657, 0.9999810757616318657, 1.000000000000000000 ) ) 
 REPRESENTATION_ITEM ( '' )  );
#43666 = VECTOR ( 'NONE', #51362, 1000.000000000000000 ) ;
#43665 = DIRECTION ( 'NONE',  ( 0.7071067811865486830, -0.7071067811865464625, -0.000000000000000000 ) ) ;
#43667 = ORIENTED_EDGE ( 'NONE', *, *, #120606, .T. ) ;
#43668 = ADVANCED_FACE ( 'NONE', ( #93562 ), #113145, .T. ) ;
#43669 = VECTOR ( 'NONE', #16507, 1000.000000000000000 ) ;
#43670 = CARTESIAN_POINT ( 'NONE',  ( 63.48921356237309510, -27.52281430457099631, 5.000000000000000000 ) ) ;
#43672 = ORIENTED_EDGE ( 'NONE', *, *, #82601, .F. ) ;
#43671 = LINE ( 'NONE', #71152, #39400 ) ;
#43673 = EDGE_LOOP ( 'NONE', ( #63473, #49014, #105239, #79551, #129603, #45786 ) ) ;
#43674 = DIRECTION ( 'NONE',  ( 0.7071067811865487940, 0.7071067811865463515, 0.000000000000000000 ) ) ;
#43675 = AXIS2_PLACEMENT_3D ( 'NONE', #60863, #29594, #6373 ) ;
#43676 = DIRECTION ( 'NONE',  ( 0.7071067811865487940, 0.7071067811865463515, 0.000000000000000000 ) ) ;
#43677 = EDGE_CURVE ( 'NONE', #100225, #116904, #27561, .T. ) ;
#43678 = ORIENTED_EDGE ( 'NONE', *, *, #346, .F. ) ;
#43679 = DIRECTION ( 'NONE',  ( -1.000000000000000000, -1.224606353822377258E-16, -0.000000000000000000 ) ) ;
#43680 = DIRECTION ( 'NONE',  ( -1.000000000000000000, 0.000000000000000000, 0.000000000000000000 ) ) ;
#43681 = LINE ( 'NONE', #77052, #5181 ) ;
#43682 = ORIENTED_EDGE ( 'NONE', *, *, #5464, .F. ) ;
#43683 = DIRECTION ( 'NONE',  ( -0.7071067811865487940, 0.7071067811865463515, 0.000000000000000000 ) ) ;
#43684 = DIRECTION ( 'NONE',  ( -0.000000000000000000, 0.3543493200069153248, 0.9351131265310292928 ) ) ;
#43685 = CARTESIAN_POINT ( 'NONE',  ( 0.000000000000000000, 0.000000000000000000, 6.750000000000000888 ) ) ;
#43686 = CIRCLE ( 'NONE', #117742, 2.500000000000000888 ) ;
#43687 = CARTESIAN_POINT ( 'NONE',  ( 37.68293019189810167, -1.637169565754159173, -6.109999999999999432 ) ) ;
#43688 = CARTESIAN_POINT ( 'NONE',  ( 13.78302761116349728, -22.22500000000000142, 23.45729246355647746 ) ) ;
#43689 = AXIS2_PLACEMENT_3D ( 'NONE', #73475, #6020, #96595 ) ;
#43690 = VERTEX_POINT ( 'NONE', #135643 ) ;
#43691 = ORIENTED_EDGE ( 'NONE', *, *, #128854, .F. ) ;
#43692 = EDGE_CURVE ( 'NONE', #69387, #71257, #124753, .T. ) ;
#43693 = CARTESIAN_POINT ( 'NONE',  ( 125.9791666666666572, -7.950000000000001066, 2.130196079827424427 ) ) ;
#43694 = ORIENTED_EDGE ( 'NONE', *, *, #43528, .T. ) ;
#43695 = ADVANCED_FACE ( 'NONE', ( #115998 ), #26168, .F. ) ;
#43696 = VERTEX_POINT ( 'NONE', #105142 ) ;
#43697 = LINE ( 'NONE', #118384, #33986 ) ;
#43698 = DIRECTION ( 'NONE',  ( -0.000000000000000000, 0.000000000000000000, 1.000000000000000000 ) ) ;
#43699 = ORIENTED_EDGE ( 'NONE', *, *, #112485, .T. ) ;
#43700 = EDGE_CURVE ( 'NONE', #35704, #58993, #61114, .T. ) ;
#43701 = FACE_OUTER_BOUND ( 'NONE', #37169, .T. ) ;
#43702 = CARTESIAN_POINT ( 'NONE',  ( 21.48921356237309155, -27.52281430457070499, 5.000000000000000000 ) ) ;
#43703 = CARTESIAN_POINT ( 'NONE',  ( 4.499999999999972466, -2.947814304570806065, 5.000000000000000000 ) ) ;
#43704 = CARTESIAN_POINT ( 'NONE',  ( 63.48921356237309510, -27.52281430457099631, 5.000000000000000000 ) ) ;
#43705 = CARTESIAN_POINT ( 'NONE',  ( 120.6045968585647614, 1.637169565754164946, -6.109999999999999432 ) ) ;
#43706 = ORIENTED_EDGE ( 'NONE', *, *, #56184, .T. ) ;
#43707 = LINE ( 'NONE', #108933, #85759 ) ;
#43708 = SURFACE_SIDE_STYLE ('',( #35001 ) ) ;
#43709 = LINE ( 'NONE', #121259, #68097 ) ;
#43710 = LINE ( 'NONE', #108210, #114985 ) ;
#43711 = CARTESIAN_POINT ( 'NONE',  ( 21.48921356237309155, -27.52281430457070499, 5.000000000000000000 ) ) ;
#43712 = CARTESIAN_POINT ( 'NONE',  ( -42.18398860626899705, 28.73617430169816700, 5.000000000000000000 ) ) ;
#43713 = CARTESIAN_POINT ( 'NONE',  ( 0.000000000000000000, 0.000000000000000000, 5.000000000000000000 ) ) ;
#43714 = CARTESIAN_POINT ( 'NONE',  ( 52.57919371712956291, 3.975000000000002753, -6.884901960086283523 ) ) ;
#43715 = DIRECTION ( 'NONE',  ( -0.7071067811865486830, -0.7071067811865464625, 0.000000000000000000 ) ) ;
#43716 = FACE_OUTER_BOUND ( 'NONE', #83555, .T. ) ;
#43717 = EDGE_LOOP ( 'NONE', ( #99061, #58848, #110115, #86965 ) ) ;
#43718 = ORIENTED_EDGE ( 'NONE', *, *, #122037, .F. ) ;
#43719 = CARTESIAN_POINT ( 'NONE',  ( 41.24999999999999289, -9.735942053221458872E-16, 7.950000000000000178 ) ) ;
#43720 = EDGE_CURVE ( 'NONE', #122494, #29125, #92110, .T. ) ;
#43721 = CYLINDRICAL_SURFACE ( 'NONE', #71739, 0.5000000000000004441 ) ;
#43722 = CARTESIAN_POINT ( 'NONE',  ( 60.48921356237309510, -27.52281430457097500, 5.000000000000000000 ) ) ;
#43723 = ORIENTED_EDGE ( 'NONE', *, *, #23206, .T. ) ;
#43724 = DIRECTION ( 'NONE',  ( 0.7071067811865487940, 0.7071067811865463515, 0.000000000000000000 ) ) ;
#43725 = CARTESIAN_POINT ( 'NONE',  ( 66.48921356237309510, -27.52281430457101763, 5.000000000000000000 ) ) ;
#43726 = CARTESIAN_POINT ( 'NONE',  ( 45.79209685856476852, -5.291415217122921177, 3.054999999999999272 ) ) ;
#43727 = EDGE_LOOP ( 'NONE', ( #15313, #48654, #87876, #5437 ) ) ;
#43728 = ORIENTED_EDGE ( 'NONE', *, *, #120365, .T. ) ;
#43729 = ORIENTED_EDGE ( 'NONE', *, *, #60406, .T. ) ;
#43730 = FACE_OUTER_BOUND ( 'NONE', #131024, .T. ) ;
#43731 = VECTOR ( 'NONE', #66276, 1000.000000000000000 ) ;
#43732 = AXIS2_PLACEMENT_3D ( 'NONE', #13498, #91791, #88971 ) ;
#43733 = VECTOR ( 'NONE', #71077, 1000.000000000000000 ) ;
#43734 = DIRECTION ( 'NONE',  ( -0.7071067811865486830, -0.7071067811865464625, -0.000000000000000000 ) ) ;
#43735 = CARTESIAN_POINT ( 'NONE',  ( 38.99451991528749062, 28.92564299267965211, 4.000000000000000000 ) ) ;
#43736 = VECTOR ( 'NONE', #36294, 1000.000000000000000 ) ;
#43737 = CARTESIAN_POINT ( 'NONE',  ( -14.67183060077637080, -15.74070752338413115, 4.000000000000000000 ) ) ;
#43738 = ORIENTED_EDGE ( 'NONE', *, *, #26899, .F. ) ;
#43739 = EDGE_CURVE ( 'NONE', #8017, #7243, #81278, .T. ) ;
#43740 = DIRECTION ( 'NONE',  ( 0.000000000000000000, -1.000000000000000000, 0.000000000000000000 ) ) ;
#43741 = B_SPLINE_CURVE_WITH_KNOTS ( 'NONE', 3,
 ( #89177, #76158, #77603, #120322 ),
 .UNSPECIFIED., .F., .F.,
 ( 4, 4 ),
 ( 0.001163520961193508819, 0.001596196080316354942 ),
 .UNSPECIFIED. ) ;
#43743 = ORIENTED_EDGE ( 'NONE', *, *, #139300, .F. ) ;
#43742 = PLANE ( 'NONE',  #96161 ) ;
#43744 = CARTESIAN_POINT ( 'NONE',  ( 77.87543019189810423, -5.291415217122920289, -3.055000000000001492 ) ) ;
#43745 = CARTESIAN_POINT ( 'NONE',  ( 15.75000000000000000, -7.464222240803106570E-16, -6.094999999999989981 ) ) ;
#43746 = EDGE_CURVE ( 'NONE', #116279, #97308, #35647, .T. ) ;
#43747 = FACE_OUTER_BOUND ( 'NONE', #142268, .T. ) ;
#43749 = CARTESIAN_POINT ( 'NONE',  ( 4.898587196589412829E-16, 8.616843969807042924, -4.000000000000000000 ) ) ;
#43748 = AXIS2_PLACEMENT_3D ( 'NONE', #142609, #75226, #119388 ) ;
#43750 = CARTESIAN_POINT ( 'NONE',  ( 34.92499999999998295, 19.80009451602697013, 4.759050581649324485 ) ) ;
#43751 = AXIS2_PLACEMENT_3D ( 'NONE', #66869, #111041, #20474 ) ;
#43752 = ADVANCED_FACE ( 'NONE', ( #8633 ), #31172, .F. ) ;
#43753 = ORIENTED_EDGE ( 'NONE', *, *, #77390, .F. ) ;
#43754 = DIRECTION ( 'NONE',  ( 0.000000000000000000, 0.000000000000000000, -1.000000000000000000 ) ) ;
#43755 = CARTESIAN_POINT ( 'NONE',  ( 67.14126352523145158, 4.472830434245836706, 4.472830434245840259 ) ) ;
#43756 = CARTESIAN_POINT ( 'NONE',  ( -34.92500000000001137, 9.856123077392346943, 4.000000000000000000 ) ) ;
#43757 = CARTESIAN_POINT ( 'NONE',  ( 9.005480084712511157, 28.92564299267931816, 4.000000000000000000 ) ) ;
#43758 = PLANE ( 'NONE',  #43245 ) ;
#43759 = ORIENTED_EDGE ( 'NONE', *, *, #110966, .T. ) ;
#43760 = ORIENTED_EDGE ( 'NONE', *, *, #109080, .F. ) ;
#43761 = VECTOR ( 'NONE', #126918, 1000.000000000000000 ) ;
#43762 = LINE ( 'NONE', #19152, #84067 ) ;
#43763 = ORIENTED_EDGE ( 'NONE', *, *, #48362, .T. ) ;
#43764 = ADVANCED_FACE ( 'NONE', ( #129744 ), #901, .T. ) ;
#43765 = ORIENTED_EDGE ( 'NONE', *, *, #57189, .T. ) ;
#43766 = VECTOR ( 'NONE', #36570, 1000.000000000000000 ) ;
#43767 = ADVANCED_FACE ( 'NONE', ( #96372 ), #62374, .F. ) ;
#43768 = LINE ( 'NONE', #53199, #116185 ) ;
#43769 = ORIENTED_EDGE ( 'NONE', *, *, #143215, .T. ) ;
#43770 = DIRECTION ( 'NONE',  ( 0.7071067811865486830, -0.7071067811865464625, -0.000000000000000000 ) ) ;
#43771 = CARTESIAN_POINT ( 'NONE',  ( 19.17183060077634593, 12.75929247661559529, 4.000000000000000000 ) ) ;
#43772 = CIRCLE ( 'NONE', #127161, 2.500000000000000444 ) ;
#43773 = VECTOR ( 'NONE', #36557, 1000.000000000000000 ) ;
#43775 = AXIS2_PLACEMENT_3D ( 'NONE', #23703, #101979, #122276 ) ;
#43774 = LINE ( 'NONE', #68417, #37348 ) ;
#43776 = FACE_BOUND ( 'NONE', #54160, .T. ) ;
#43777 = EDGE_CURVE ( 'NONE', #78073, #42223, #139832, .T. ) ;
#43778 = FACE_OUTER_BOUND ( 'NONE', #121669, .T. ) ;
#43779 = PLANE ( 'NONE',  #139263 ) ;
#43780 = FACE_OUTER_BOUND ( 'NONE', #86971, .T. ) ;
#43782 = VERTEX_POINT ( 'NONE', #127622 ) ;
#43781 = CARTESIAN_POINT ( 'NONE',  ( 50.53752705046289861, -9.735942053221456900E-16, 7.949999999999998401 ) ) ;
#43783 = AXIS2_PLACEMENT_3D ( 'NONE', #72998, #125919, #139673 ) ;
#43784 = AXIS2_PLACEMENT_3D ( 'NONE', #27544, #48612, #5060 ) ;
#43785 = CARTESIAN_POINT ( 'NONE',  ( -12.69999999999998153, 0.000000000000000000, 0.000000000000000000 ) ) ;
#43786 = CONTEXT_DEPENDENT_SHAPE_REPRESENTATION ( #12455, #50437 ) ;
#43787 = VERTEX_POINT ( 'NONE', #73946 ) ;
#43788 = ORIENTED_EDGE ( 'NONE', *, *, #93771, .T. ) ;
#43789 = CARTESIAN_POINT ( 'NONE',  ( 79.82876352523145158, 0.000000000000000000, -6.109999999999998543 ) ) ;
#43790 = EDGE_LOOP ( 'NONE', ( #2356, #132845, #1538, #33686 ) ) ;
#43791 = DIRECTION ( 'NONE',  ( -0.000000000000000000, -0.3543493200069152693, 0.9351131265310292928 ) ) ;
#43792 = LINE ( 'NONE', #65582, #76786 ) ;
#43793 = ORIENTED_EDGE ( 'NONE', *, *, #23235, .T. ) ;
#43794 = FACE_OUTER_BOUND ( 'NONE', #60167, .T. ) ;
#43795 = VECTOR ( 'NONE', #32819, 1000.000000000000227 ) ;
#43796 = LINE ( 'NONE', #97434, #54252 ) ;
#43797 = LINE ( 'NONE', #77855, #113146 ) ;
#43798 = DIRECTION ( 'NONE',  ( 1.000000000000000000, 0.000000000000000000, 0.000000000000000000 ) ) ;
#43799 = DIRECTION ( 'NONE',  ( -0.6830127018922180770, -0.6830127018922204085, -0.2588190451025213501 ) ) ;
#43800 = LINE ( 'NONE', #88016, #49612 ) ;
#43801 = CARTESIAN_POINT ( 'NONE',  ( -24.77004279457776548, 21.73644205237997795, 5.000000000000000000 ) ) ;
#43802 = LINE ( 'NONE', #30802, #23096 ) ;
#43803 = ADVANCED_FACE ( 'NONE', ( #139228 ), #30448, .F. ) ;
#43804 = ORIENTED_EDGE ( 'NONE', *, *, #106867, .T. ) ;
#43805 = DIRECTION ( 'NONE',  ( -0.7071067811865486830, -0.7071067811865464625, -0.000000000000000000 ) ) ;
#43806 = ORIENTED_EDGE ( 'NONE', *, *, #111079, .T. ) ;
#43807 = CARTESIAN_POINT ( 'NONE',  ( 51.29974487139158867, -27.71228299555242103, 4.000000000000000000 ) ) ;
#43808 = PLANE ( 'NONE',  #72114 ) ;
#43809 = EDGE_LOOP ( 'NONE', ( #44951, #83109, #99205, #126001, #99260 ) ) ;
#43810 = ORIENTED_EDGE ( 'NONE', *, *, #118549, .T. ) ;
#43811 = CARTESIAN_POINT ( 'NONE',  ( 48.48921356237309510, -27.52281430457089328, 5.000000000000000000 ) ) ;
#43812 = EDGE_CURVE ( 'NONE', #49913, #99410, #108668, .T. ) ;
#43813 = CARTESIAN_POINT ( 'NONE',  ( -71.99451991528749772, 28.92564299267988304, 4.000000000000000000 ) ) ;
#43814 = ORIENTED_EDGE ( 'NONE', *, *, #120353, .T. ) ;
#43815 = LINE ( 'NONE', #67000, #46322 ) ;
#43816 = CARTESIAN_POINT ( 'NONE',  ( 89.32919371712955581, -3.975000000000001865, 6.884901960086284411 ) ) ;
#43817 = ADVANCED_FACE ( 'NONE', ( #140613 ), #139942, .F. ) ;
#43818 = CARTESIAN_POINT ( 'NONE',  ( 21.77497294953710494, 4.461849672132300881, 4.461849672132299105 ) ) ;
#43819 = CARTESIAN_POINT ( 'NONE',  ( -1.130389105715452036, 13.74331369484366761, -24.36998560215478804 ) ) ;
#43820 = EDGE_CURVE ( 'NONE', #29128, #110130, #24007, .T. ) ;
#43821 = ORIENTED_EDGE ( 'NONE', *, *, #53389, .F. ) ;
#43822 = CARTESIAN_POINT ( 'NONE',  ( 14.39532882439692862, -2.055000000000000160, 0.000000000000000000 ) ) ;
#43824 = ORIENTED_EDGE ( 'NONE', *, *, #124068, .T. ) ;
#43823 = ADVANCED_FACE ( 'NONE', ( #141336 ), #65753, .T. ) ;
#43825 = FACE_OUTER_BOUND ( 'NONE', #140763, .T. ) ;
#43826 = DIRECTION ( 'NONE',  ( 0.7071067811865487940, 0.7071067811865463515, 0.000000000000000000 ) ) ;
#43827 = ORIENTED_EDGE ( 'NONE', *, *, #1838, .T. ) ;
#43828 = VERTEX_POINT ( 'NONE', #52185 ) ;
#43829 = EDGE_CURVE ( 'NONE', #62423, #58035, #138498, .T. ) ;
#43830 = DIRECTION ( 'NONE',  ( 0.7071067811865487940, 0.7071067811865463515, 0.000000000000000000 ) ) ;
#43831 = DIRECTION ( 'NONE',  ( 0.7071067811865486830, -0.7071067811865464625, -0.000000000000000000 ) ) ;
#43832 = CARTESIAN_POINT ( 'NONE',  ( 66.48921356237309510, -27.52281430457101763, 5.000000000000000000 ) ) ;
#43833 = VERTEX_POINT ( 'NONE', #94960 ) ;
#43834 = CIRCLE ( 'NONE', #143373, 2.500000000000000888 ) ;
#43835 = VERTEX_POINT ( 'NONE', #39181 ) ;
#43836 = ORIENTED_EDGE ( 'NONE', *, *, #108431, .T. ) ;
#43837 = EDGE_CURVE ( 'NONE', #86852, #142915, #19556, .T. ) ;
#43838 = DIRECTION ( 'NONE',  ( -0.7071067811865487940, 0.7071067811865463515, -0.000000000000000000 ) ) ;
#43839 = DIRECTION ( 'NONE',  ( -0.000000000000000000, -0.3543493200069152693, 0.9351131265310292928 ) ) ;
#43840 = VECTOR ( 'NONE', #34141, 1000.000000000000227 ) ;
#43841 = PRESENTATION_LAYER_ASSIGNMENT (  '', '', ( #115595 ) ) ;
#43842 = AXIS2_PLACEMENT_3D ( 'NONE', #36543, #34406, #69187 ) ;
#43843 = VECTOR ( 'NONE', #95264, 1000.000000000000000 ) ;
#43844 = FACE_OUTER_BOUND ( 'NONE', #60093, .T. ) ;
#43845 = PLANE ( 'NONE',  #79403 ) ;
#43846 = PLANE ( 'NONE',  #39910 ) ;
#43847 = VECTOR ( 'NONE', #81621, 1000.000000000000114 ) ;
#43848 = EDGE_CURVE ( 'NONE', #72010, #23963, #97130, .T. ) ;
#43849 = DIRECTION ( 'NONE',  ( -0.7071067811865486830, -0.7071067811865464625, 0.000000000000000000 ) ) ;
#43850 = DIRECTION ( 'NONE',  ( 0.000000000000000000, 0.000000000000000000, 1.000000000000000000 ) ) ;
#43851 = EDGE_CURVE ( 'NONE', #99565, #58487, #34028, .T. ) ;
#43852 = ORIENTED_EDGE ( 'NONE', *, *, #127837, .T. ) ;
#43853 = DIRECTION ( 'NONE',  ( 0.6830127018922180770, -0.6830127018922204085, -0.2588190451025214056 ) ) ;
#43854 = ORIENTED_EDGE ( 'NONE', *, *, #126316, .T. ) ;
#43855 = VECTOR ( 'NONE', #131232, 1000.000000000000000 ) ;
#43856 = DIRECTION ( 'NONE',  ( -0.000000000000000000, -0.3543493200069152693, 0.9351131265310292928 ) ) ;
#43858 = EDGE_CURVE ( 'NONE', #3663, #115089, #44941, .T. ) ;
#43857 =( BOUNDED_CURVE ( )  B_SPLINE_CURVE ( 3, ( #77768, #68351, #46613, #103083 ),
 .UNSPECIFIED., .F., .T. ) 
 B_SPLINE_CURVE_WITH_KNOTS ( ( 4, 4 ),
 ( 5.043186909253405403, 5.074607125596340751 ),
 .UNSPECIFIED. ) 
 CURVE ( )  GEOMETRIC_REPRESENTATION_ITEM ( )  RATIONAL_B_SPLINE_CURVE ( ( 1.000000000000000000, 0.9999177325257868620, 0.9999177325257868620, 1.000000000000000000 ) ) 
 REPRESENTATION_ITEM ( '' )  );
#43859 = CARTESIAN_POINT ( 'NONE',  ( 13.17183060077637968, 15.75929247661555443, 4.000000000000000000 ) ) ;
#43860 = DIRECTION ( 'NONE',  ( -1.000000000000000000, 0.000000000000000000, 0.000000000000000000 ) ) ;
#43861 = ORIENTED_EDGE ( 'NONE', *, *, #19614, .F. ) ;
#43862 = DIRECTION ( 'NONE',  ( -0.6830127018922180770, -0.6830127018922204085, -0.2588190451025213501 ) ) ;
#43863 = DIRECTION ( 'NONE',  ( -0.7071067811865486830, -0.7071067811865464625, 0.000000000000000000 ) ) ;
#43864 = CARTESIAN_POINT ( 'NONE',  ( -25.17183060077629619, -14.24070752338412937, 4.000000000000000000 ) ) ;
#43865 = ORIENTED_EDGE ( 'NONE', *, *, #66637, .F. ) ;
#43866 = ORIENTED_EDGE ( 'NONE', *, *, #134161, .F. ) ;
#43867 = CARTESIAN_POINT ( 'NONE',  ( 55.45435323442900710, -52.10358567239564564, 40.45860062937861557 ) ) ;
#43868 = CARTESIAN_POINT ( 'NONE',  ( 18.48921356237309510, -27.52281430457068367, 5.000000000000000000 ) ) ;
#43869 = CARTESIAN_POINT ( 'NONE',  ( -2.999999999999978240, -13.44781430457069327, 5.000000000000000000 ) ) ;
#43870 = MECHANICAL_DESIGN_GEOMETRIC_PRESENTATION_REPRESENTATION (  '', ( #138769 ), #80912 ) ;
#43871 = CARTESIAN_POINT ( 'NONE',  ( -7.828169399223474656, -11.24070752338416845, 4.000000000000000000 ) ) ;
#43872 = CARTESIAN_POINT ( 'NONE',  ( 10.00193056682090642, -22.22500000000000142, 4.500000000000000888 ) ) ;
#43873 = CARTESIAN_POINT ( 'NONE',  ( 63.20376352523145158, 6.109999999999999432, 1.122388791418549108E-15 ) ) ;
#43874 = DIRECTION ( 'NONE',  ( -1.000000000000000000, -0.000000000000000000, -0.000000000000000000 ) ) ;
#43876 = LINE ( 'NONE', #33027, #134129 ) ;
#43875 = VECTOR ( 'NONE', #135733, 1000.000000000000000 ) ;
#43877 = CARTESIAN_POINT ( 'NONE',  ( 6.299744871391586898, -27.71228299555210484, 4.000000000000000000 ) ) ;
#43878 = DIRECTION ( 'NONE',  ( 0.7071067811865486830, 0.7071067811865464625, 0.000000000000000000 ) ) ;
#43879 = VERTEX_POINT ( 'NONE', #131903 ) ;
#43880 = EDGE_CURVE ( 'NONE', #67478, #21645, #120255, .T. ) ;
#43881 = ORIENTED_EDGE ( 'NONE', *, *, #121071, .F. ) ;
#43882 = DIRECTION ( 'NONE',  ( 0.7071067811865487940, 0.7071067811865463515, 0.000000000000000000 ) ) ;
#43883 = DIRECTION ( 'NONE',  ( 0.7071067811865487940, 0.7071067811865463515, -0.000000000000000000 ) ) ;
#43884 = VECTOR ( 'NONE', #69090, 999.9999999999998863 ) ;
#43885 = VECTOR ( 'NONE', #106795, 1000.000000000000227 ) ;
#43886 = VECTOR ( 'NONE', #137120, 1000.000000000000227 ) ;
#43887 = PLANE ( 'NONE',  #20678 ) ;
#43888 = CARTESIAN_POINT ( 'NONE',  ( -34.92500000000001137, 21.72500000000000142, 5.000000000000000000 ) ) ;
#43889 = DIRECTION ( 'NONE',  ( 0.7071067811865487940, 0.7071067811865463515, 0.000000000000000000 ) ) ;
#43890 = CARTESIAN_POINT ( 'NONE',  ( -11.81601139373100651, 28.73617430169779041, 5.000000000000000000 ) ) ;
#43891 = LINE ( 'NONE', #9814, #7842 ) ;
#43892 = ORIENTED_EDGE ( 'NONE', *, *, #126862, .F. ) ;
#43893 = ORIENTED_EDGE ( 'NONE', *, *, #21944, .F. ) ;
#43894 = CARTESIAN_POINT ( 'NONE',  ( 7.251592354503322291, 9.902892378096218942E-16, 0.000000000000000000 ) ) ;
#43895 = FACE_OUTER_BOUND ( 'NONE', #1224, .T. ) ;
#43896 = VECTOR ( 'NONE', #28580, 1000.000000000000000 ) ;
#43897 = CARTESIAN_POINT ( 'NONE',  ( -13.17183060077638324, -17.24070752338410628, 4.000000000000000000 ) ) ;
#43898 = ADVANCED_FACE ( 'NONE', ( #134049 ), #21706, .F. ) ;
#43899 = CARTESIAN_POINT ( 'NONE',  ( 5.999999999999956479, -8.151047557385066256, -8.977947279169812944 ) ) ;
#43900 = CARTESIAN_POINT ( 'NONE',  ( 86.99586038379622721, -3.974999999999998312, -6.884901960086286188 ) ) ;
#43901 = DIRECTION ( 'NONE',  ( 0.7071067811865487940, 0.7071067811865463515, 0.000000000000000000 ) ) ;
#43902 = DIRECTION ( 'NONE',  ( -0.7071067811865487940, 0.7071067811865463515, 0.000000000000000000 ) ) ;
#43903 = VERTEX_POINT ( 'NONE', #43459 ) ;
#43904 = CARTESIAN_POINT ( 'NONE',  ( 70.70833333333332860, -3.974999999999999201, -6.884901960086287964 ) ) ;
#43905 = DIRECTION ( 'NONE',  ( -0.000000000000000000, 0.000000000000000000, 1.000000000000000000 ) ) ;
#43906 = EDGE_CURVE ( 'NONE', #42897, #62746, #44191, .T. ) ;
#43907 = DIRECTION ( 'NONE',  ( 0.7071067811865487940, 0.7071067811865463515, 0.000000000000000000 ) ) ;
#43908 = FACE_OUTER_BOUND ( 'NONE', #102112, .T. ) ;
#43909 = VECTOR ( 'NONE', #121671, 1000.000000000000000 ) ;
#43910 = VERTEX_POINT ( 'NONE', #77543 ) ;
#43911 = DIRECTION ( 'NONE',  ( -0.6830127018922181881, 0.6830127018922202975, -0.2588190451025214056 ) ) ;
#43912 = ORIENTED_EDGE ( 'NONE', *, *, #96919, .T. ) ;
#43913 = EDGE_CURVE ( 'NONE', #63953, #75609, #34734, .T. ) ;
#43914 = PLANE ( 'NONE',  #53540 ) ;
#43915 = CARTESIAN_POINT ( 'NONE',  ( 72.04209685856477563, 5.291415217122923842, -3.054999999999996163 ) ) ;
#43916 = CARTESIAN_POINT ( 'NONE',  ( -2.816011393730999401, 28.73617430169785436, 5.000000000000000000 ) ) ;
#43917 = ORIENTED_EDGE ( 'NONE', *, *, #123118, .F. ) ;
#43918 = DIRECTION ( 'NONE',  ( 0.7071067811865486830, -0.7071067811865464625, -0.000000000000000000 ) ) ;
#43919 = LINE ( 'NONE', #51411, #110072 ) ;
#43920 = CARTESIAN_POINT ( 'NONE',  ( -18.18398860626898994, 28.73617430169800002, 5.000000000000000000 ) ) ;
#43921 = LINE ( 'NONE', #33080, #11437 ) ;
#43922 = EDGE_CURVE ( 'NONE', #89491, #26834, #97843, .T. ) ;
#43923 = DIRECTION ( 'NONE',  ( -0.7071067811865487940, -0.7071067811865463515, -0.000000000000000000 ) ) ;
#43925 = ORIENTED_EDGE ( 'NONE', *, *, #17009, .F. ) ;
#43924 = CARTESIAN_POINT ( 'NONE',  ( 127.0000000000000568, 1.764297610274628392, 6.170334904552290389 ) ) ;
#43926 = SURFACE_STYLE_FILL_AREA ( #109165 ) ;
#43927 = CARTESIAN_POINT ( 'NONE',  ( -36.48921356237310221, -27.52281430457080802, 5.000000000000000000 ) ) ;
#43928 = DIRECTION ( 'NONE',  ( 0.000000000000000000, 0.000000000000000000, 1.000000000000000000 ) ) ;
#43929 = LINE ( 'NONE', #77988, #41442 ) ;
#43930 = ORIENTED_EDGE ( 'NONE', *, *, #113931, .T. ) ;
#43931 = ORIENTED_EDGE ( 'NONE', *, *, #49249, .T. ) ;
#43932 = CARTESIAN_POINT ( 'NONE',  ( 66.64626352523144703, -4.472830434245840259, 4.472830434245839371 ) ) ;
#43933 = ORIENTED_EDGE ( 'NONE', *, *, #9128, .F. ) ;
#43934 = CARTESIAN_POINT ( 'NONE',  ( 22.49999999999984723, 18.05218569542898877, 5.000000000000000000 ) ) ;
#43935 = DIRECTION ( 'NONE',  ( 0.7071067811865486830, -0.7071067811865464625, -0.000000000000000000 ) ) ;
#43936 = CARTESIAN_POINT ( 'NONE',  ( 124.7666937171295274, -7.949999999999998401, 2.130196079827423983 ) ) ;
#43937 = ORIENTED_EDGE ( 'NONE', *, *, #56638, .F. ) ;
#43938 = VERTEX_POINT ( 'NONE', #142769 ) ;
#43939 = DIRECTION ( 'NONE',  ( -0.7071067811865487940, 0.7071067811865463515, -0.000000000000000000 ) ) ;
#43940 = LINE ( 'NONE', #7712, #104568 ) ;
#43941 = ORIENTED_EDGE ( 'NONE', *, *, #83255, .F. ) ;
#43942 = EDGE_CURVE ( 'NONE', #97938, #97859, #31869, .T. ) ;
#43943 = CARTESIAN_POINT ( 'NONE',  ( 12.79289321881337571, -2.240707523384255939, 5.000000000000000000 ) ) ;
#43944 = CARTESIAN_POINT ( 'NONE',  ( -66.48921356237309510, -27.52281430457101763, 5.000000000000000000 ) ) ;
#43945 = LINE ( 'NONE', #88170, #97919 ) ;
#43946 = VECTOR ( 'NONE', #132823, 1000.000000000000000 ) ;
#43947 = AXIS2_PLACEMENT_3D ( 'NONE', #121917, #24065, #32820 ) ;
#43948 = CIRCLE ( 'NONE', #46252, 2.500000000000000888 ) ;
#43949 = VERTEX_POINT ( 'NONE', #98544 ) ;
#43950 = AXIS2_PLACEMENT_3D ( 'NONE', #61323, #27924, #96025 ) ;
#43951 = EDGE_CURVE ( 'NONE', #111481, #110666, #11498, .T. ) ;
#43952 = FACE_BOUND ( 'NONE', #93664, .T. ) ;
#43953 = EDGE_CURVE ( 'NONE', #39036, #54633, #142083, .T. ) ;
#43954 = CARTESIAN_POINT ( 'NONE',  ( -14.51078643762690490, -27.52281430457045275, 5.000000000000000000 ) ) ;
#43955 = DIRECTION ( 'NONE',  ( -0.7071067811865487940, 0.7071067811865463515, -0.000000000000000000 ) ) ;
#43956 = DIRECTION ( 'NONE',  ( 0.6830127018922181881, 0.6830127018922202975, -0.2588190451025214056 ) ) ;
#43957 = VECTOR ( 'NONE', #105015, 1000.000000000000000 ) ;
#43958 = DIRECTION ( 'NONE',  ( -0.7071067811865486830, -0.7071067811865464625, -0.000000000000000000 ) ) ;
#43959 = FACE_OUTER_BOUND ( 'NONE', #70755, .T. ) ;
#43960 =( NAMED_UNIT ( * ) PLANE_ANGLE_UNIT ( ) SI_UNIT ( $, .RADIAN. ) );
#43961 = ORIENTED_EDGE ( 'NONE', *, *, #95007, .T. ) ;
#43962 = ORIENTED_EDGE ( 'NONE', *, *, #115960, .F. ) ;
#43963 = CARTESIAN_POINT ( 'NONE',  ( 114.9745968585647802, 1.637169565754164280, -6.109999999999996767 ) ) ;
#43964 = ORIENTED_EDGE ( 'NONE', *, *, #6788, .T. ) ;
#43965 = EDGE_LOOP ( 'NONE', ( #18515, #100743, #143426, #88936 ) ) ;
#43966 = VECTOR ( 'NONE', #97153, 1000.000000000000000 ) ;
#43967 = VECTOR ( 'NONE', #29606, 1000.000000000000000 ) ;
#43968 = CARTESIAN_POINT ( 'NONE',  ( -21.29974487139158512, -27.71228299555221142, 4.000000000000000000 ) ) ;
#43969 = EDGE_CURVE ( 'NONE', #78430, #141426, #67374, .T. ) ;
#43970 = CARTESIAN_POINT ( 'NONE',  ( 128.5894344200537773, -52.00875322212549179, -39.86617647058817226 ) ) ;
#43971 = AXIS2_PLACEMENT_3D ( 'NONE', #137525, #59967, #127342 ) ;
#43972 = CARTESIAN_POINT ( 'NONE',  ( -34.92500000000001137, 16.81783344222318632, 7.048977539241899848 ) ) ;
#43973 = ORIENTED_EDGE ( 'NONE', *, *, #90756, .F. ) ;
#43974 = DIRECTION ( 'NONE',  ( -0.6830127018922181881, 0.6830127018922202975, -0.2588190451025214056 ) ) ;
#43975 = CARTESIAN_POINT ( 'NONE',  ( 61.46640106136302961, -43.14999999999999147, -34.92499999999998295 ) ) ;
#43976 = CARTESIAN_POINT ( 'NONE',  ( 37.60416666666665719, 2.130196079827498146, 7.949999999999958433 ) ) ;
#43978 = PLANE ( 'NONE',  #64303 ) ;
#43977 = FACE_OUTER_BOUND ( 'NONE', #64064, .T. ) ;
#43979 = CARTESIAN_POINT ( 'NONE',  ( 2.524972949537106270, -4.461849672132299993, -4.461849672132299105 ) ) ;
#43980 = VECTOR ( 'NONE', #141817, 1000.000000000000000 ) ;
#43981 = CARTESIAN_POINT ( 'NONE',  ( 0.8725517856990301357, 0.9952662357582434671, 3.904172814578533934 ) ) ;
#43982 = ORIENTED_EDGE ( 'NONE', *, *, #10968, .T. ) ;
#43983 = CIRCLE ( 'NONE', #108817, 2.500000000000000444 ) ;
#43984 = DIRECTION ( 'NONE',  ( -0.7071067811865486830, -0.7071067811865464625, -0.000000000000000000 ) ) ;
#43985 = DIRECTION ( 'NONE',  ( 0.000000000000000000, 0.000000000000000000, 1.000000000000000000 ) ) ;
#43986 = ORIENTED_EDGE ( 'NONE', *, *, #116947, .F. ) ;
#43987 = ORIENTED_EDGE ( 'NONE', *, *, #142063, .F. ) ;
#43988 = AXIS2_PLACEMENT_3D ( 'NONE', #56455, #47013, #13578 ) ;
#43989 = ORIENTED_EDGE ( 'NONE', *, *, #56784, .F. ) ;
#43991 = AXIS2_PLACEMENT_3D ( 'NONE', #81746, #10889, #103437 ) ;
#43990 = CARTESIAN_POINT ( 'NONE',  ( 63.72959685856477563, -6.110000000000000320, -1.637169565754161393 ) ) ;
#43992 = ORIENTED_EDGE ( 'NONE', *, *, #17224, .F. ) ;
#43993 = CARTESIAN_POINT ( 'NONE',  ( 25.49999999999983302, 13.46639925780212721, 5.000000000000000000 ) ) ;
#43994 = ADVANCED_FACE ( 'NONE', ( #121008 ), #100705, .F. ) ;
#43995 = DIRECTION ( 'NONE',  ( 0.7071067811865487940, -0.7071067811865463515, 0.000000000000000000 ) ) ;
#43996 = CARTESIAN_POINT ( 'NONE',  ( 100.4795968585647614, 6.109999999999999432, 1.637169565754164280 ) ) ;
#43997 = LINE ( 'NONE', #52015, #109606 ) ;
#43998 = EDGE_CURVE ( 'NONE', #63418, #115520, #40278, .T. ) ;
#43999 = EDGE_LOOP ( 'NONE', ( #125626, #116166, #69031, #67151 ) ) ;
#44000 = CARTESIAN_POINT ( 'NONE',  ( -17.99999999999986855, -18.41253812416056945, 4.000000000000000000 ) ) ;
#44001 = VECTOR ( 'NONE', #79237, 1000.000000000000227 ) ;
#44002 = PLANE ( 'NONE',  #12276 ) ;
#44003 = EDGE_CURVE ( 'NONE', #116046, #21906, #65962, .T. ) ;
#44004 = EDGE_CURVE ( 'NONE', #115328, #81524, #10795, .T. ) ;
#44005 =( LENGTH_UNIT ( ) NAMED_UNIT ( * ) SI_UNIT ( .MILLI., .METRE. ) );
#44006 = LINE ( 'NONE', #111376, #82190 ) ;
#44007 = ORIENTED_EDGE ( 'NONE', *, *, #12795, .F. ) ;
#44008 = CARTESIAN_POINT ( 'NONE',  ( 10.32500000000000107, -9.500000000000001776, -4.375000000000001776 ) ) ;
#44009 = VERTEX_POINT ( 'NONE', #53635 ) ;
#44010 = EDGE_LOOP ( 'NONE', ( #86174, #24001, #112815, #33947 ) ) ;
#44011 = EDGE_LOOP ( 'NONE', ( #103345, #30033, #84713, #53133 ) ) ;
#44012 = CARTESIAN_POINT ( 'NONE',  ( 122.4120968585647802, 5.291415217122921177, -3.054999999999994831 ) ) ;
#44013 = ORIENTED_EDGE ( 'NONE', *, *, #131370, .F. ) ;
#44014 = AXIS2_PLACEMENT_3D ( 'NONE', #93739, #36505, #27759 ) ;
#44015 = PLANE ( 'NONE',  #44630 ) ;
#44016 = ADVANCED_FACE ( 'NONE', ( #112299 ), #20976, .F. ) ;
#44017 = DIRECTION ( 'NONE',  ( 0.7071067811865487940, 0.7071067811865463515, -0.000000000000000000 ) ) ;
#44018 = EDGE_CURVE ( 'NONE', #18115, #74547, #65240, .T. ) ;
#44019 = ORIENTED_EDGE ( 'NONE', *, *, #76930, .T. ) ;
#44020 = LINE ( 'NONE', #131030, #97482 ) ;
#44021 = EDGE_LOOP ( 'NONE', ( #45730, #21044, #105349, #57866 ) ) ;
#44022 = VECTOR ( 'NONE', #138198, 1000.000000000000000 ) ;
#44023 = CLOSED_SHELL ( 'NONE', ( #92436, #17146, #69405, #18554, #103238, #131894, #61088, #79794, #12141, #59177 ) ) ;
#44024 = EDGE_CURVE ( 'NONE', #26437, #23833, #87676, .T. ) ;
#44025 = CARTESIAN_POINT ( 'NONE',  ( 10.91623647476855297, -7.934999999999990727, 4.858786175617117713E-16 ) ) ;
#44026 = FACE_OUTER_BOUND ( 'NONE', #65973, .T. ) ;
#44027 = DIRECTION ( 'NONE',  ( -0.000000000000000000, 0.000000000000000000, 1.000000000000000000 ) ) ;
#44028 = LINE ( 'NONE', #77397, #25797 ) ;
#44029 = ORIENTED_EDGE ( 'NONE', *, *, #89079, .F. ) ;
#44030 = ORIENTED_EDGE ( 'NONE', *, *, #39914, .T. ) ;
#44031 = ORIENTED_EDGE ( 'NONE', *, *, #107002, .F. ) ;
#44032 = CARTESIAN_POINT ( 'NONE',  ( 36.29974487139159578, -27.71228299555231445, 4.000000000000000000 ) ) ;
#44033 = CARTESIAN_POINT ( 'NONE',  ( 58.60416666666665719, 2.130196079827422206, 7.950000000000001954 ) ) ;
#44034 = EDGE_CURVE ( 'NONE', #78816, #53035, #25996, .T. ) ;
#44035 = CARTESIAN_POINT ( 'NONE',  ( -21.18398860626899349, 28.73617430169802134, 5.000000000000000000 ) ) ;
#44036 = CARTESIAN_POINT ( 'NONE',  ( -34.49999999999975131, 19.08746187583904685, 4.000000000000000000 ) ) ;
#44037 = VECTOR ( 'NONE', #3331, 1000.000000000000000 ) ;
#44038 = CARTESIAN_POINT ( 'NONE',  ( -34.49999999999975131, -13.91253812416061031, 4.000000000000000000 ) ) ;
#44039 = LINE ( 'NONE', #33196, #102764 ) ;
#44040 = CARTESIAN_POINT ( 'NONE',  ( -5.999999999999958256, 7.931123077392102871, 4.000000000000000000 ) ) ;
#44041 = DIRECTION ( 'NONE',  ( -1.000000000000000000, -1.224606353822377258E-16, -0.000000000000000000 ) ) ;
#44042 = VERTEX_POINT ( 'NONE', #113709 ) ;
#44043 = DIRECTION ( 'NONE',  ( 0.6830127018922181881, 0.6830127018922202975, -0.2588190451025214056 ) ) ;
#44044 = VECTOR ( 'NONE', #78525, 1000.000000000000000 ) ;
#44045 = EDGE_CURVE ( 'NONE', #18266, #82873, #91949, .T. ) ;
#44046 = ORIENTED_EDGE ( 'NONE', *, *, #38402, .F. ) ;
#44047 = VECTOR ( 'NONE', #104238, 999.9999999999998863 ) ;
#44048 = VECTOR ( 'NONE', #73992, 1000.000000000000000 ) ;
#44049 = VECTOR ( 'NONE', #37054, 1000.000000000000000 ) ;
#44050 = DIRECTION ( 'NONE',  ( 0.7071067811865487940, 0.7071067811865463515, -0.000000000000000000 ) ) ;
#44051 = ORIENTED_EDGE ( 'NONE', *, *, #123131, .F. ) ;
#44052 = AXIS2_PLACEMENT_3D ( 'NONE', #32034, #99399, #88580 ) ;
#44053 = FACE_OUTER_BOUND ( 'NONE', #142612, .T. ) ;
#44054 = EDGE_LOOP ( 'NONE', ( #74139, #39295, #69821 ) ) ;
#44055 = DIRECTION ( 'NONE',  ( -0.7071067811865486830, -0.7071067811865464625, 0.000000000000000000 ) ) ;
#44056 = EDGE_LOOP ( 'NONE', ( #29460, #106274, #115273, #89510 ) ) ;
#44057 = PLANE ( 'NONE',  #99392 ) ;
#44058 = EDGE_LOOP ( 'NONE', ( #55254, #118075, #16254, #95821 ) ) ;
#44059 = FACE_OUTER_BOUND ( 'NONE', #134116, .T. ) ;
#44060 = AXIS2_PLACEMENT_3D ( 'NONE', #38193, #82407, #136763 ) ;
#44061 = EDGE_LOOP ( 'NONE', ( #121102, #121151 ) ) ;
#44062 = LINE ( 'NONE', #33218, #82357 ) ;
#44063 = EDGE_CURVE ( 'NONE', #38058, #85621, #60063, .T. ) ;
#44064 = CARTESIAN_POINT ( 'NONE',  ( 116.1625270504628986, 7.949999999999998401, 1.460391307983218338E-15 ) ) ;
#44065 = CARTESIAN_POINT ( 'NONE',  ( -12.69999999999998153, 0.000000000000000000, 0.000000000000000000 ) ) ;
#44066 = CARTESIAN_POINT ( 'NONE',  ( -34.92500000000001137, 18.94777415420116995, 3.758136617891472131 ) ) ;
#44067 = LINE ( 'NONE', #123785, #134776 ) ;
#44068 = LINE ( 'NONE', #88289, #65813 ) ;
#44069 = CARTESIAN_POINT ( 'NONE',  ( 12.29974487139158512, -27.71228299555214747, 4.000000000000000000 ) ) ;
#44070 = CARTESIAN_POINT ( 'NONE',  ( 14.58333333333333570, -5.278424836066144543, 3.047499999999995879 ) ) ;
#44072 = MECHANICAL_DESIGN_GEOMETRIC_PRESENTATION_REPRESENTATION (  '', ( #4668 ), #69545 ) ;
#44071 = CARTESIAN_POINT ( 'NONE',  ( 18.20790314143522082, -6.871911579029513106, -3.967499999999993587 ) ) ;
#44073 = CARTESIAN_POINT ( 'NONE',  ( -2.540161610502588374, 18.75929247661552779, 8.305906642995479316 ) ) ;
#44074 = CARTESIAN_POINT ( 'NONE',  ( -34.42500000000001137, 0.000000000000000000, 4.500000000000000888 ) ) ;
#44075 = VERTEX_POINT ( 'NONE', #36853 ) ;
#44076 =( BOUNDED_CURVE ( )  B_SPLINE_CURVE ( 3, ( #101311, #57841, #133254, #23760 ),
 .UNSPECIFIED., .F., .F. ) 
 B_SPLINE_CURVE_WITH_KNOTS ( ( 4, 4 ),
 ( 1.901594255663599853, 1.933014472006561624 ),
 .UNSPECIFIED. ) 
 CURVE ( )  GEOMETRIC_REPRESENTATION_ITEM ( )  RATIONAL_B_SPLINE_CURVE ( ( 1.000000000000000000, 0.9999177325257867510, 0.9999177325257867510, 1.000000000000000000 ) ) 
 REPRESENTATION_ITEM ( '' )  );
#44077 = EDGE_LOOP ( 'NONE', ( #70047, #29655, #49563, #60402 ) ) ;
#44078 = STYLED_ITEM ( 'NONE', ( #143048 ), #97639 ) ;
#44079 = CARTESIAN_POINT ( 'NONE',  ( -12.79289321881337038, -2.240707523384259492, 5.000000000000000000 ) ) ;
#44080 = EDGE_LOOP ( 'NONE', ( #31334, #90458, #21997, #24663, #94576 ) ) ;
#44081 = VECTOR ( 'NONE', #10252, 1000.000000000000000 ) ;
#44082 = EDGE_CURVE ( 'NONE', #78195, #27223, #3488, .T. ) ;
#44083 = AXIS2_PLACEMENT_3D ( 'NONE', #100416, #75811, #53317 ) ;
#44084 = DIRECTION ( 'NONE',  ( -0.7071067811865487940, 0.7071067811865463515, 0.000000000000000000 ) ) ;
#44085 = LINE ( 'NONE', #8533, #37018 ) ;
#44086 = CARTESIAN_POINT ( 'NONE',  ( 9.183988606268997046, 28.73617430169793607, 5.000000000000000000 ) ) ;
#44087 = CARTESIAN_POINT ( 'NONE',  ( 34.47516574401891631, 21.02806734111559450, 4.998110765256834398 ) ) ;
#44088 = ORIENTED_EDGE ( 'NONE', *, *, #139427, .F. ) ;
#44089 = VECTOR ( 'NONE', #21403, 999.9999999999998863 ) ;
#44090 = DIRECTION ( 'NONE',  ( -0.7071067811865486830, -0.7071067811865464625, 0.000000000000000000 ) ) ;
#44091 = CARTESIAN_POINT ( 'NONE',  ( 0.000000000000000000, -10.06887692260771416, 4.000000000000000000 ) ) ;
#44092 = PLANE ( 'NONE',  #113573 ) ;
#44093 = SURFACE_STYLE_USAGE ( .BOTH. , #133255 ) ;
#44094 = EDGE_CURVE ( 'NONE', #119104, #105661, #57942, .T. ) ;
#44095 = VECTOR ( 'NONE', #75785, 999.9999999999998863 ) ;
#44096 = LINE ( 'NONE', #122327, #44868 ) ;
#44098 = ORIENTED_EDGE ( 'NONE', *, *, #82165, .F. ) ;
#44097 = LINE ( 'NONE', #141992, #130790 ) ;
#44099 =( NAMED_UNIT ( * ) PLANE_ANGLE_UNIT ( ) SI_UNIT ( $, .RADIAN. ) );
#44100 = DIRECTION ( 'NONE',  ( 0.7071067811865486830, -0.7071067811865464625, -0.000000000000000000 ) ) ;
#44101 = FILL_AREA_STYLE_COLOUR ( '', #23832 ) ;
#44102 = CARTESIAN_POINT ( 'NONE',  ( 9.083148067729251096, 21.75929247661549226, 7.311836541448074378 ) ) ;
#44103 = DIRECTION ( 'NONE',  ( 0.6830127018922181881, 0.6830127018922202975, -0.2588190451025214056 ) ) ;
#44104 = ORIENTED_EDGE ( 'NONE', *, *, #135695, .T. ) ;
#44105 = ORIENTED_EDGE ( 'NONE', *, *, #60846, .F. ) ;
#44106 = ORIENTED_EDGE ( 'NONE', *, *, #62543, .F. ) ;
#44107 = CARTESIAN_POINT ( 'NONE',  ( 91.14626352523144703, -4.472830434245840259, 4.472830434245839371 ) ) ;
#44108 = CIRCLE ( 'NONE', #125104, 2.500000000000000888 ) ;
#44109 = ORIENTED_EDGE ( 'NONE', *, *, #110362, .F. ) ;
#44110 = CARTESIAN_POINT ( 'NONE',  ( -7.940000000000007496, -60.26999999999998892, -10.00000000000000178 ) ) ;
#44111 = VECTOR ( 'NONE', #17996, 1000.000000000000000 ) ;
#44112 = DIRECTION ( 'NONE',  ( -0.5735764363510499342, -0.8191520442889891340, 0.000000000000000000 ) ) ;
#44113 = VERTEX_POINT ( 'NONE', #90545 ) ;
#44114 = DIRECTION ( 'NONE',  ( -0.000000000000000000, 0.3543493200069153248, 0.9351131265310292928 ) ) ;
#44115 = DIRECTION ( 'NONE',  ( -0.000000000000000000, -0.3543493200069152693, 0.9351131265310292928 ) ) ;
#44116 = CARTESIAN_POINT ( 'NONE',  ( 82.30793019189809456, -6.109999999999998543, 1.637169565754158063 ) ) ;
#44117 = ORIENTED_EDGE ( 'NONE', *, *, #60220, .T. ) ;
#44118 = EDGE_CURVE ( 'NONE', #130915, #125898, #24553, .T. ) ;
#44119 = CARTESIAN_POINT ( 'NONE',  ( 0.8691381963085933471, 0.5999999999999987566, -4.444516329276119393 ) ) ;
#44120 = FACE_OUTER_BOUND ( 'NONE', #21174, .T. ) ;
#44121 = VECTOR ( 'NONE', #104424, 1000.000000000000000 ) ;
#44122 = ORIENTED_EDGE ( 'NONE', *, *, #114054, .T. ) ;
#44123 = ORIENTED_EDGE ( 'NONE', *, *, #53732, .T. ) ;
#44124 = EDGE_CURVE ( 'NONE', #17758, #18398, #136891, .T. ) ;
#44125 = ORIENTED_EDGE ( 'NONE', *, *, #19660, .T. ) ;
#44126 = CARTESIAN_POINT ( 'NONE',  ( -30.18398860626900060, 28.73617430169808173, 5.000000000000000000 ) ) ;
#44127 = ADVANCED_FACE ( 'NONE', ( #102850 ), #47781, .F. ) ;
#44128 = CARTESIAN_POINT ( 'NONE',  ( 153.4000000000000057, -1.600000000000094458, 34.92499999999998295 ) ) ;
#44129 = CARTESIAN_POINT ( 'NONE',  ( 14.65040314143522160, 7.934999999999988951, -2.126176841940961904 ) ) ;
#44130 = LINE ( 'NONE', #7361, #58152 ) ;
#44131 = VECTOR ( 'NONE', #71351, 1000.000000000000227 ) ;
#44132 = CARTESIAN_POINT ( 'NONE',  ( 3.191216777807910354, -48.83231052142030393, -38.98973348322098076 ) ) ;
#44133 = LINE ( 'NONE', #98495, #62708 ) ;
#44134 = DIRECTION ( 'NONE',  ( -0.3543493200069163240, 0.000000000000000000, -0.9351131265310288487 ) ) ;
#44135 = VERTEX_POINT ( 'NONE', #36167 ) ;
#44137 = EDGE_LOOP ( 'NONE', ( #127206, #33808, #118102, #8674 ) ) ;
#44136 = EDGE_CURVE ( 'NONE', #11916, #23830, #47094, .T. ) ;
#44138 = CARTESIAN_POINT ( 'NONE',  ( 0.000000000000000000, 0.000000000000000000, 5.000000000000000000 ) ) ;
#44139 = ORIENTED_EDGE ( 'NONE', *, *, #96509, .F. ) ;
#44140 = ORIENTED_EDGE ( 'NONE', *, *, #142102, .F. ) ;
#44141 = VECTOR ( 'NONE', #42925, 1000.000000000000000 ) ;
#44142 = ADVANCED_FACE ( 'NONE', ( #71648 ), #15090, .T. ) ;
#44143 = VECTOR ( 'NONE', #94543, 1000.000000000000000 ) ;
#44144 = FACE_OUTER_BOUND ( 'NONE', #26189, .T. ) ;
#44145 = ORIENTED_EDGE ( 'NONE', *, *, #70019, .T. ) ;
#44146 = CARTESIAN_POINT ( 'NONE',  ( 55.54166666666665719, -3.975000000000002753, 6.884901960086286188 ) ) ;
#44147 = CARTESIAN_POINT ( 'NONE',  ( 25.39999999999999858, 0.000000000000000000, 0.000000000000000000 ) ) ;
#44148 = FACE_OUTER_BOUND ( 'NONE', #109438, .T. ) ;
#44149 = CARTESIAN_POINT ( 'NONE',  ( 24.84463820744543838, 1.742823668393624903, 4.000000000000000000 ) ) ;
#44150 = AXIS2_PLACEMENT_3D ( 'NONE', #27784, #138712, #83631 ) ;
#44151 = AXIS2_PLACEMENT_3D ( 'NONE', #117830, #71518, #73654 ) ;
#44152 = AXIS2_PLACEMENT_3D ( 'NONE', #1890, #109984, #10650 ) ;
#44153 = PRESENTATION_LAYER_ASSIGNMENT (  '', '', ( #65069 ) ) ;
#44154 = CARTESIAN_POINT ( 'NONE',  ( 118.5416666666666714, -3.975000000000002753, 6.884901960086286188 ) ) ;
#44155 = ORIENTED_EDGE ( 'NONE', *, *, #26901, .F. ) ;
#44156 = VECTOR ( 'NONE', #11144, 1000.000000000000000 ) ;
#44157 = PLANE ( 'NONE',  #18640 ) ;
#44158 = EDGE_LOOP ( 'NONE', ( #47018, #122745, #122258, #24504 ) ) ;
#44159 = CARTESIAN_POINT ( 'NONE',  ( 19.93618820137057668, -3.269999999999996465, -36.39086428169088094 ) ) ;
#44160 = ORIENTED_EDGE ( 'NONE', *, *, #4077, .F. ) ;
#44161 = CARTESIAN_POINT ( 'NONE',  ( 27.18398860626900060, 28.73617430169806042, 5.000000000000000000 ) ) ;
#44162 = VERTEX_POINT ( 'NONE', #124587 ) ;
#44163 = DIRECTION ( 'NONE',  ( 0.6830127018922180770, -0.6830127018922204085, -0.2588190451025213501 ) ) ;
#44164 = VERTEX_POINT ( 'NONE', #70262 ) ;
#44165 = ORIENTED_EDGE ( 'NONE', *, *, #10016, .T. ) ;
#44166 = B_SPLINE_CURVE_WITH_KNOTS ( 'NONE', 3,
 ( #142826, #109482, #140667, #30507, #118183, #40669, #65295, #43511, #118921, #41355, #87732, #29759, #64549, #85569, #129799, #76148, #19611, #63858, #108018, #108729, #9410, #53695, #42821, #87018 ),
 .UNSPECIFIED., .F., .F.,
 ( 4, 2, 2, 1, 2, 2, 2, 2, 2, 1, 2, 2, 4 ),
 ( 1.221256415468642823E-17, 0.002003734080813304470, 0.003005601121219949549, 0.004007468161626595061, 0.005009335202033241008, 0.006011202242439885220, 0.008014936323253174510, 0.01001867040406646293, 0.01102053744447310628, 0.01202240448487974789, 0.01302427152528639297, 0.01402613856569303458, 0.01602987264650632127 ),
 .UNSPECIFIED. ) ;
#44167 = AXIS2_PLACEMENT_3D ( 'NONE', #78316, #1426, #67465 ) ;
#44168 = ORIENTED_EDGE ( 'NONE', *, *, #46487, .F. ) ;
#44169 = FACE_OUTER_BOUND ( 'NONE', #67714, .T. ) ;
#44170 = EDGE_CURVE ( 'NONE', #65084, #50417, #26702, .T. ) ;
#44171 = DIRECTION ( 'NONE',  ( -1.000000000000000000, -1.224606353822377258E-16, -0.000000000000000000 ) ) ;
#44172 = LINE ( 'NONE', #131886, #75046 ) ;
#44173 = CARTESIAN_POINT ( 'NONE',  ( 123.0837635252314470, -6.110000000000001208, -3.741295971395164515E-16 ) ) ;
#44174 = FACE_OUTER_BOUND ( 'NONE', #42127, .T. ) ;
#44175 = EDGE_CURVE ( 'NONE', #121970, #19406, #125307, .T. ) ;
#44176 = LINE ( 'NONE', #142070, #45988 ) ;
#44178 = CARTESIAN_POINT ( 'NONE',  ( 51.29974487139158867, -27.71228299555242103, 4.000000000000000000 ) ) ;
#44177 = CARTESIAN_POINT ( 'NONE',  ( -30.48921356237309510, -27.52281430457076894, 5.000000000000000000 ) ) ;
#44179 = VECTOR ( 'NONE', #103385, 1000.000000000000000 ) ;
#44180 = DIRECTION ( 'NONE',  ( 0.000000000000000000, 1.000000000000000000, 0.000000000000000000 ) ) ;
#44181 = EDGE_CURVE ( 'NONE', #133096, #48518, #137621, .T. ) ;
#44182 = EDGE_CURVE ( 'NONE', #71067, #115114, #27389, .T. ) ;
#44183 = AXIS2_PLACEMENT_3D ( 'NONE', #86921, #119502, #41995 ) ;
#44184 = VECTOR ( 'NONE', #104339, 1000.000000000000000 ) ;
#44185 = CARTESIAN_POINT ( 'NONE',  ( 19.05000000000000071, 3.174999999999997158, 1.444000000000000394 ) ) ;
#44186 = CARTESIAN_POINT ( 'NONE',  ( 2.613322195557306049, -2.055000000000000160, 2.789133085058097101E-16 ) ) ;
#44187 = VERTEX_POINT ( 'NONE', #104230 ) ;
#44188 = VECTOR ( 'NONE', #56048, 1000.000000000000227 ) ;
#44189 = ORIENTED_EDGE ( 'NONE', *, *, #139454, .T. ) ;
#44190 = VERTEX_POINT ( 'NONE', #12947 ) ;
#44191 = LINE ( 'NONE', #23091, #121268 ) ;
#44192 = EDGE_LOOP ( 'NONE', ( #82535, #49373, #41712, #41260 ) ) ;
#44194 = EDGE_CURVE ( 'NONE', #113156, #38919, #57222, .T. ) ;
#44193 = AXIS2_PLACEMENT_3D ( 'NONE', #126939, #47999, #71897 ) ;
#44195 = ORIENTED_EDGE ( 'NONE', *, *, #1868, .T. ) ;
#44196 = DIRECTION ( 'NONE',  ( 0.7071067811865487940, 0.7071067811865463515, -0.000000000000000000 ) ) ;
#44197 = CARTESIAN_POINT ( 'NONE',  ( 106.9750270504628986, -5.819803920172573086, 5.819803920172573086 ) ) ;
#44198 = EDGE_CURVE ( 'NONE', #120928, #128903, #79713, .T. ) ;
#44199 =( GEOMETRIC_REPRESENTATION_CONTEXT ( 3 ) GLOBAL_UNCERTAINTY_ASSIGNED_CONTEXT ( ( #90978 ) ) GLOBAL_UNIT_ASSIGNED_CONTEXT ( ( #122113, #108349, #120676 ) ) REPRESENTATION_CONTEXT ( 'NONE', 'WORKASPACE' ) );
#44200 = DIRECTION ( 'NONE',  ( -0.7071067811865487940, 0.7071067811865463515, -0.000000000000000000 ) ) ;
#44201 = EDGE_CURVE ( 'NONE', #92353, #17336, #91274, .T. ) ;
#44202 = FACE_OUTER_BOUND ( 'NONE', #29836, .T. ) ;
#44203 = EDGE_LOOP ( 'NONE', ( #15604, #6101, #74907, #107004 ) ) ;
#44204 = DIRECTION ( 'NONE',  ( -0.7071067811865487940, 0.7071067811865463515, -0.000000000000000000 ) ) ;
#44205 = ORIENTED_EDGE ( 'NONE', *, *, #22020, .F. ) ;
#44206 = CARTESIAN_POINT ( 'NONE',  ( 12.48921356237309155, -27.52281430457064104, 5.000000000000000000 ) ) ;
#44207 = ADVANCED_FACE ( 'NONE', ( #75754 ), #143134, .F. ) ;
#44208 = AXIS2_PLACEMENT_3D ( 'NONE', #135872, #14798, #59072 ) ;
#44209 = CARTESIAN_POINT ( 'NONE',  ( 21.35873647476855552, 5.808823158059031044, -5.808823158059038150 ) ) ;
#44210 = ORIENTED_EDGE ( 'NONE', *, *, #74189, .F. ) ;
#44211 = CARTESIAN_POINT ( 'NONE',  ( 86.97459685856479439, 1.637169565754164280, -6.109999999999997655 ) ) ;
#44212 = EDGE_CURVE ( 'NONE', #116810, #23874, #54720, .T. ) ;
#44213 = CARTESIAN_POINT ( 'NONE',  ( 5.950517365466079234, -9.499761739870839605, 0.3008884456578363453 ) ) ;
#44214 = DIRECTION ( 'NONE',  ( -0.6830127018922181881, 0.6830127018922202975, -0.2588190451025214056 ) ) ;
#44215 = VERTEX_POINT ( 'NONE', #109062 ) ;
#44216 = EDGE_LOOP ( 'NONE', ( #32599, #67418, #136472, #123959 ) ) ;
#44217 = VECTOR ( 'NONE', #11404, 1000.000000000000227 ) ;
#44218 = EDGE_LOOP ( 'NONE', ( #31962, #124733, #38449, #88182 ) ) ;
#44219 = DIRECTION ( 'NONE',  ( 0.6830127018922181881, 0.6830127018922202975, -0.2588190451025214056 ) ) ;
#44220 = LINE ( 'NONE', #2072, #57946 ) ;
#44221 = CARTESIAN_POINT ( 'NONE',  ( -18.48921356237309510, -27.52281430457068367, 5.000000000000000000 ) ) ;
#44222 = EDGE_CURVE ( 'NONE', #125554, #1609, #138322, .T. ) ;
#44223 = CARTESIAN_POINT ( 'NONE',  ( 24.18398860626899705, 28.73617430169804265, 5.000000000000000000 ) ) ;
#44224 = LINE ( 'NONE', #112323, #102846 ) ;
#44225 = ORIENTED_EDGE ( 'NONE', *, *, #61419, .F. ) ;
#44226 = DIRECTION ( 'NONE',  ( 0.000000000000000000, -1.000000000000000000, 0.000000000000000000 ) ) ;
#44227 = CARTESIAN_POINT ( 'NONE',  ( 0.000000000000000000, -0.2811185226894302724, -5.995736974527512864 ) ) ;
#44228 = FACE_OUTER_BOUND ( 'NONE', #129567, .T. ) ;
#44229 = ORIENTED_EDGE ( 'NONE', *, *, #29763, .T. ) ;
#44230 = CARTESIAN_POINT ( 'NONE',  ( -14.81601139373099585, 28.73617430169776910, 5.000000000000000000 ) ) ;
#44231 = EDGE_CURVE ( 'NONE', #65716, #11235, #98900, .T. ) ;
#44232 = AXIS2_PLACEMENT_3D ( 'NONE', #75930, #33178, #44775 ) ;
#44233 = LINE ( 'NONE', #121046, #116458 ) ;
#44234 = VERTEX_POINT ( 'NONE', #28134 ) ;
#44236 = ORIENTED_EDGE ( 'NONE', *, *, #58518, .F. ) ;
#44235 = CARTESIAN_POINT ( 'NONE',  ( -23.33153258840129496, -18.74070752338409207, 20.73178291233835679 ) ) ;
#44237 = ORIENTED_EDGE ( 'NONE', *, *, #34108, .T. ) ;
#44238 = FACE_OUTER_BOUND ( 'NONE', #36419, .T. ) ;
#44240 = EDGE_CURVE ( 'NONE', #121031, #34714, #54019, .T. ) ;
#44239 = CARTESIAN_POINT ( 'NONE',  ( 34.49999999999975131, -20.94567065516883630, 4.994342998332155226 ) ) ;
#44242 = ORIENTED_EDGE ( 'NONE', *, *, #46676, .T. ) ;
#44241 = VECTOR ( 'NONE', #110554, 1000.000000000000227 ) ;
#44243 = CARTESIAN_POINT ( 'NONE',  ( -31.49999999999977973, -12.66682484999668823, -0.6294897503864678168 ) ) ;
#44244 = DIRECTION ( 'NONE',  ( 0.6830127018922181881, 0.6830127018922202975, -0.2588190451025214056 ) ) ;
#44245 = EDGE_CURVE ( 'NONE', #132249, #137138, #120645, .T. ) ;
#44246 = SURFACE_STYLE_USAGE ( .BOTH. , #98593 ) ;
#44247 =( BOUNDED_CURVE ( )  B_SPLINE_CURVE ( 3, ( #14315, #70183, #81025, #16430 ),
 .UNSPECIFIED., .F., .T. ) 
 B_SPLINE_CURVE_WITH_KNOTS ( ( 4, 4 ),
 ( 1.378368140454908408, 1.408685637663195545 ),
 .UNSPECIFIED. ) 
 CURVE ( )  GEOMETRIC_REPRESENTATION_ITEM ( )  RATIONAL_B_SPLINE_CURVE ( ( 1.000000000000000000, 0.9999234055803066790, 0.9999234055803066790, 1.000000000000000000 ) ) 
 REPRESENTATION_ITEM ( '' )  );
#44248 = DIRECTION ( 'NONE',  ( -0.6830127018922181881, 0.6830127018922202975, -0.2588190451025214056 ) ) ;
#44249 = CARTESIAN_POINT ( 'NONE',  ( 34.42499999999998295, 22.22500000000000142, 0.4999999999999995559 ) ) ;
#44250 = CARTESIAN_POINT ( 'NONE',  ( 51.18398860626899705, 28.73617430169823095, 5.000000000000000000 ) ) ;
#44251 = DIRECTION ( 'NONE',  ( -1.000000000000000000, -6.248375730189539568E-15, 0.000000000000000000 ) ) ;
#44252 = CARTESIAN_POINT ( 'NONE',  ( 17.91623647476855652, -7.934999999999990727, 4.858786175617117713E-16 ) ) ;
#44253 = DIRECTION ( 'NONE',  ( -0.000000000000000000, 1.000000000000000000, -0.000000000000000000 ) ) ;
#44254 = LINE ( 'NONE', #121771, #15881 ) ;
#44256 = EDGE_CURVE ( 'NONE', #32728, #124559, #119920, .T. ) ;
#44255 =( GEOMETRIC_REPRESENTATION_CONTEXT ( 3 ) GLOBAL_UNCERTAINTY_ASSIGNED_CONTEXT ( ( #41746 ) ) GLOBAL_UNIT_ASSIGNED_CONTEXT ( ( #93581, #105160, #39202 ) ) REPRESENTATION_CONTEXT ( 'NONE', 'WORKASPACE' ) );
#44257 = CARTESIAN_POINT ( 'NONE',  ( -27.18398860626900060, 28.73617430169806042, 5.000000000000000000 ) ) ;
#44258 = CARTESIAN_POINT ( 'NONE',  ( -23.59118151920504403, -0.6989376001503790903, 4.102600482792084335 ) ) ;
#44259 = ORIENTED_EDGE ( 'NONE', *, *, #63457, .T. ) ;
#44260 = ORIENTED_EDGE ( 'NONE', *, *, #18257, .T. ) ;
#44261 = VECTOR ( 'NONE', #38973, 1000.000000000000000 ) ;
#44262 = CARTESIAN_POINT ( 'NONE',  ( 100.6041666666666430, 2.130196079827422206, 7.950000000000001954 ) ) ;
#44263 = AXIS2_PLACEMENT_3D ( 'NONE', #67311, #37542, #3438 ) ;
#44264 = VERTEX_POINT ( 'NONE', #39008 ) ;
#44265 = VERTEX_POINT ( 'NONE', #76476 ) ;
#44266 = VERTEX_POINT ( 'NONE', #97472 ) ;
#44267 = DIRECTION ( 'NONE',  ( 2.781805975412905274E-17, -0.3543493200069152138, 0.9351131265310292928 ) ) ;
#44268 = DIRECTION ( 'NONE',  ( 0.000000000000000000, 0.000000000000000000, -1.000000000000000000 ) ) ;
#44269 = VECTOR ( 'NONE', #104263, 1000.000000000000000 ) ;
#44270 = VECTOR ( 'NONE', #2474, 1000.000000000000000 ) ;
#44271 = CIRCLE ( 'NONE', #120582, 0.5000000000000004441 ) ;
#44272 =( GEOMETRIC_REPRESENTATION_CONTEXT ( 3 ) GLOBAL_UNCERTAINTY_ASSIGNED_CONTEXT ( ( #27250 ) ) GLOBAL_UNIT_ASSIGNED_CONTEXT ( ( #109529, #43560, #132011 ) ) REPRESENTATION_CONTEXT ( 'NONE', 'WORKASPACE' ) );
#44273 = EDGE_LOOP ( 'NONE', ( #134590, #55409, #78117, #22180 ) ) ;
#44274 = DIRECTION ( 'NONE',  ( -0.7071067811865486830, -0.7071067811865464625, -0.000000000000000000 ) ) ;
#44275 = VECTOR ( 'NONE', #42245, 1000.000000000000000 ) ;
#44276 = DIRECTION ( 'NONE',  ( -0.7071067811865486830, 0.7071067811865464625, 0.000000000000000000 ) ) ;
#44277 = DIRECTION ( 'NONE',  ( 0.7071067811865487940, 0.7071067811865463515, -0.000000000000000000 ) ) ;
#44278 = PLANE ( 'NONE',  #95224 ) ;
#44279 = VERTEX_POINT ( 'NONE', #141726 ) ;
#44280 = DIRECTION ( 'NONE',  ( 0.6830127018922180770, -0.6830127018922204085, -0.2588190451025213501 ) ) ;
#44281 = CARTESIAN_POINT ( 'NONE',  ( -9.489213562373095101, -27.52281430457062328, 5.000000000000000000 ) ) ;
#44282 = VECTOR ( 'NONE', #3399, 999.9999999999998863 ) ;
#44283 = DIRECTION ( 'NONE',  ( -0.000000000000000000, 0.3543493200069153248, 0.9351131265310292928 ) ) ;
#44284 = CARTESIAN_POINT ( 'NONE',  ( 25.49999999999983658, 13.56627193232217898, -10.57019076586062845 ) ) ;
#44285 = LINE ( 'NONE', #133424, #88625 ) ;
#44286 = LINE ( 'NONE', #129841, #36126 ) ;
#44287 = CARTESIAN_POINT ( 'NONE',  ( 27.48921356237309155, -27.52281430457074762, 5.000000000000000000 ) ) ;
#44288 = CARTESIAN_POINT ( 'NONE',  ( 20.20519093902540320, 4.584330080086930965E-16, 0.000000000000000000 ) ) ;
#44289 = ORIENTED_EDGE ( 'NONE', *, *, #65798, .F. ) ;
#44290 = ORIENTED_EDGE ( 'NONE', *, *, #11872, .T. ) ;
#44291 = CARTESIAN_POINT ( 'NONE',  ( 125.1254301918981184, 5.291415217122919401, 3.055000000000002824 ) ) ;
#44292 = VERTEX_POINT ( 'NONE', #28851 ) ;
#44293 = VECTOR ( 'NONE', #17720, 1000.000000000000000 ) ;
#44294 = ADVANCED_FACE ( 'NONE', ( #116565 ), #131554, .F. ) ;
#44295 = CARTESIAN_POINT ( 'NONE',  ( 10.49999999999992717, -10.53360074219763298, 5.000000000000000000 ) ) ;
#44296 = FACE_OUTER_BOUND ( 'NONE', #47236, .T. ) ;
#44297 = LINE ( 'NONE', #87068, #14282 ) ;
#44298 = LINE ( 'NONE', #88512, #111285 ) ;
#44299 = VECTOR ( 'NONE', #18409, 1000.000000000000000 ) ;
#44300 = VECTOR ( 'NONE', #30193, 999.9999999999998863 ) ;
#44301 = CARTESIAN_POINT ( 'NONE',  ( 113.3704301918981230, -3.055000000000001492, 5.291415217122917625 ) ) ;
#44302 = VERTEX_POINT ( 'NONE', #32239 ) ;
#44303 = AXIS2_PLACEMENT_3D ( 'NONE', #91256, #69501, #68789 ) ;
#44304 = ORIENTED_EDGE ( 'NONE', *, *, #8731, .F. ) ;
#44305 = DIRECTION ( 'NONE',  ( 0.7071067811865487940, -0.7071067811865463515, 0.000000000000000000 ) ) ;
#44306 = AXIS2_PLACEMENT_3D ( 'NONE', #22609, #77760, #98763 ) ;
#44307 = CARTESIAN_POINT ( 'NONE',  ( -19.05499999999999261, 3.130000000000007887, 0.000000000000000000 ) ) ;
#44308 = VERTEX_POINT ( 'NONE', #142440 ) ;
#44309 = ORIENTED_EDGE ( 'NONE', *, *, #4287, .T. ) ;
#44310 = CARTESIAN_POINT ( 'NONE',  ( 36.02126352523142572, -4.472830434245839371, -4.472830434245840259 ) ) ;
#44311 = EDGE_CURVE ( 'NONE', #82006, #33848, #109780, .T. ) ;
#44312 = ORIENTED_EDGE ( 'NONE', *, *, #6803, .T. ) ;
#44313 = VECTOR ( 'NONE', #39244, 999.9999999999998863 ) ;
#44314 = DIRECTION ( 'NONE',  ( 0.7071067811865487940, 0.7071067811865463515, -0.000000000000000000 ) ) ;
#44315 = DIRECTION ( 'NONE',  ( 0.000000000000000000, 0.000000000000000000, 1.000000000000000000 ) ) ;
#44316 = EDGE_CURVE ( 'NONE', #83402, #121702, #74350, .T. ) ;
#44317 =( LENGTH_UNIT ( ) NAMED_UNIT ( * ) SI_UNIT ( .MILLI., .METRE. ) );
#44318 = ADVANCED_FACE ( 'NONE', ( #61511 ), #86638, .F. ) ;
#44319 = EDGE_CURVE ( 'NONE', #143429, #115828, #82097, .T. ) ;
#44320 = CARTESIAN_POINT ( 'NONE',  ( 34.03709685856478018, -3.054999999999998828, -5.291415217122919401 ) ) ;
#44321 = ORIENTED_EDGE ( 'NONE', *, *, #127947, .T. ) ;
#44322 = EDGE_CURVE ( 'NONE', #71223, #83238, #17925, .T. ) ;
#44323 = CARTESIAN_POINT ( 'NONE',  ( -12.06039522340302028, -22.22500000000000142, -3.664253473662678839 ) ) ;
#44324 = VERTEX_POINT ( 'NONE', #113342 ) ;
#44325 = ORIENTED_EDGE ( 'NONE', *, *, #136392, .T. ) ;
#44326 = VECTOR ( 'NONE', #115367, 1000.000000000000000 ) ;
#44327 = EDGE_LOOP ( 'NONE', ( #131246, #101543, #95465, #47274 ) ) ;
#44328 = VECTOR ( 'NONE', #69375, 1000.000000000000000 ) ;
#44329 = EDGE_CURVE ( 'NONE', #123070, #68539, #14027, .T. ) ;
#44330 = CARTESIAN_POINT ( 'NONE',  ( 0.2569208697893812232, 0.4000000000000001332, -2.015694669338588429 ) ) ;
#44331 = CARTESIAN_POINT ( 'NONE',  ( 78.68336038379622721, -2.130196079827426203, 7.949999999999996625 ) ) ;
#44332 = ORIENTED_EDGE ( 'NONE', *, *, #12714, .F. ) ;
#44333 = LINE ( 'NONE', #131317, #117785 ) ;
#44334 = AXIS2_PLACEMENT_3D ( 'NONE', #8545, #20161, #84731 ) ;
#44335 = VECTOR ( 'NONE', #32636, 1000.000000000000000 ) ;
#44336 = SURFACE_STYLE_USAGE ( .BOTH. , #45768 ) ;
#44337 = EDGE_CURVE ( 'NONE', #105294, #87228, #79361, .T. ) ;
#44338 = FACE_OUTER_BOUND ( 'NONE', #110399, .T. ) ;
#44339 = FACE_BOUND ( 'NONE', #58720, .T. ) ;
#44340 = ORIENTED_EDGE ( 'NONE', *, *, #119085, .F. ) ;
#44341 = DIRECTION ( 'NONE',  ( -1.000000000000000000, -0.000000000000000000, -0.000000000000000000 ) ) ;
#44342 = CARTESIAN_POINT ( 'NONE',  ( 63.48921356237309510, -27.52281430457099631, 5.000000000000000000 ) ) ;
#44343 = DIRECTION ( 'NONE',  ( -0.7071067811865486830, -0.7071067811865464625, 0.000000000000000000 ) ) ;
#44344 = ORIENTED_EDGE ( 'NONE', *, *, #40207, .F. ) ;
#44345 = DIRECTION ( 'NONE',  ( 0.7071067811865486830, -0.7071067811865464625, -0.000000000000000000 ) ) ;
#44346 = ORIENTED_EDGE ( 'NONE', *, *, #57982, .T. ) ;
#44348 = ORIENTED_EDGE ( 'NONE', *, *, #46480, .T. ) ;
#44347 = EDGE_CURVE ( 'NONE', #132741, #3971, #101767, .T. ) ;
#44349 = VECTOR ( 'NONE', #125761, 999.9999999999998863 ) ;
#44350 = DIRECTION ( 'NONE',  ( -0.000000000000000000, 0.000000000000000000, 1.000000000000000000 ) ) ;
#44351 = VERTEX_POINT ( 'NONE', #55426 ) ;
#44352 = CARTESIAN_POINT ( 'NONE',  ( 45.26626352523144448, 4.472830434245838482, -4.472830434245837594 ) ) ;
#44353 = EDGE_LOOP ( 'NONE', ( #45370, #40333, #66355, #101145 ) ) ;
#44354 = CARTESIAN_POINT ( 'NONE',  ( -84.48921356237309510, -27.52281430457114197, 5.000000000000000000 ) ) ;
#44355 = DIRECTION ( 'NONE',  ( -0.5735764363510503783, -0.8191520442889886899, 0.000000000000000000 ) ) ;
#44356 = LINE ( 'NONE', #55212, #2386 ) ;
#44357 = EDGE_CURVE ( 'NONE', #110443, #58071, #68470, .T. ) ;
#44358 = EDGE_LOOP ( 'NONE', ( #114048, #51872, #33364, #39437 ) ) ;
#44359 = DIRECTION ( 'NONE',  ( 0.7071067811865487940, 0.7071067811865463515, -0.000000000000000000 ) ) ;
#44360 = CARTESIAN_POINT ( 'NONE',  ( 24.00548008471250938, 28.92564299267921513, 4.000000000000000000 ) ) ;
#44361 = AXIS2_PLACEMENT_3D ( 'NONE', #13499, #46931, #100552 ) ;
#44362 = ADVANCED_FACE ( 'NONE', ( #23493 ), #134419, .T. ) ;
#44364 = EDGE_CURVE ( 'NONE', #100733, #105469, #123563, .T. ) ;
#44363 = AXIS2_PLACEMENT_3D ( 'NONE', #129930, #61839, #128511 ) ;
#44365 = VECTOR ( 'NONE', #28637, 1000.000000000000227 ) ;
#44366 = PRESENTATION_STYLE_ASSIGNMENT (( #79868 ) ) ;
#44367 = CARTESIAN_POINT ( 'NONE',  ( -3.489213562373097322, -27.52281430457057709, 5.000000000000000000 ) ) ;
#44368 = FACE_BOUND ( 'NONE', #69242, .T. ) ;
#44369 = FACE_OUTER_BOUND ( 'NONE', #108667, .T. ) ;
#44370 = DIRECTION ( 'NONE',  ( 0.7071067811865486830, -0.7071067811865464625, -0.000000000000000000 ) ) ;
#44371 = ORIENTED_EDGE ( 'NONE', *, *, #30022, .F. ) ;
#44372 = AXIS2_PLACEMENT_3D ( 'NONE', #58539, #57794, #114283 ) ;
#44373 = VECTOR ( 'NONE', #72460, 1000.000000000000000 ) ;
#44374 = EDGE_LOOP ( 'NONE', ( #111715, #105692, #121706, #139605, #27229, #64519 ) ) ;
#44375 = VECTOR ( 'NONE', #136936, 1000.000000000000000 ) ;
#44376 = ORIENTED_EDGE ( 'NONE', *, *, #14160, .F. ) ;
#44377 = AXIS2_PLACEMENT_3D ( 'NONE', #21473, #43237, #8400 ) ;
#44378 = PLANE ( 'NONE',  #61273 ) ;
#44379 = LINE ( 'NONE', #66119, #130137 ) ;
#44380 = ORIENTED_EDGE ( 'NONE', *, *, #59584, .T. ) ;
#44381 = EDGE_CURVE ( 'NONE', #77421, #121710, #13311, .T. ) ;
#44382 = EDGE_LOOP ( 'NONE', ( #64167, #55060, #77339, #39073 ) ) ;
#44383 = CARTESIAN_POINT ( 'NONE',  ( 162.5099761671747274, 26.96999999999994557, -34.76218228780558661 ) ) ;
#44384 = DIRECTION ( 'NONE',  ( -0.7071067811865486830, -0.7071067811865464625, -0.000000000000000000 ) ) ;
#44385 = EDGE_CURVE ( 'NONE', #98086, #24434, #69163, .T. ) ;
#44386 = FACE_OUTER_BOUND ( 'NONE', #105760, .T. ) ;
#44387 = VERTEX_POINT ( 'NONE', #135151 ) ;
#44388 =( GEOMETRIC_REPRESENTATION_CONTEXT ( 3 ) GLOBAL_UNCERTAINTY_ASSIGNED_CONTEXT ( ( #44788 ) ) GLOBAL_UNIT_ASSIGNED_CONTEXT ( ( #88140, #122157, #113428 ) ) REPRESENTATION_CONTEXT ( 'NONE', 'WORKASPACE' ) );
#44389 = FACE_OUTER_BOUND ( 'NONE', #15128, .T. ) ;
#44390 = FACE_OUTER_BOUND ( 'NONE', #111314, .T. ) ;
#44391 = CARTESIAN_POINT ( 'NONE',  ( 24.71290314143521982, 3.967499999999992699, -6.871911579029513994 ) ) ;
#44392 = LINE ( 'NONE', #121891, #87859 ) ;
#44393 = EDGE_LOOP ( 'NONE', ( #26955, #98469, #64935, #16054 ) ) ;
#44394 = CARTESIAN_POINT ( 'NONE',  ( 108.4120968585647944, 5.291415217122922066, -3.054999999999995275 ) ) ;
#44396 = EDGE_CURVE ( 'NONE', #116339, #103515, #91614, .T. ) ;
#44395 = VECTOR ( 'NONE', #75017, 1000.000000000000000 ) ;
#44397 = LINE ( 'NONE', #142271, #92872 ) ;
#44398 = CARTESIAN_POINT ( 'NONE',  ( -16.82816939922341959, -17.24070752338410983, 4.000000000000000000 ) ) ;
#44400 = ORIENTED_EDGE ( 'NONE', *, *, #5130, .F. ) ;
#44399 = CARTESIAN_POINT ( 'NONE',  ( -60.18398860626900415, 28.73617430169829490, 5.000000000000000000 ) ) ;
#44401 = CARTESIAN_POINT ( 'NONE',  ( -29.99999999999977973, 14.58746187583909126, 4.000000000000000000 ) ) ;
#44402 = ORIENTED_EDGE ( 'NONE', *, *, #123134, .T. ) ;
#44403 = DIRECTION ( 'NONE',  ( -0.7071067811865486830, -0.7071067811865464625, -0.000000000000000000 ) ) ;
#44405 = ADVANCED_FACE ( 'NONE', ( #124239 ), #24916, .F. ) ;
#44404 = CARTESIAN_POINT ( 'NONE',  ( -27.48921356237309155, -27.52281430457074762, 5.000000000000000000 ) ) ;
#44406 = CARTESIAN_POINT ( 'NONE',  ( -53.99451991528749062, 28.92564299267975869, 4.000000000000000000 ) ) ;
#44407 = LINE ( 'NONE', #124082, #132876 ) ;
#44408 = ORIENTED_EDGE ( 'NONE', *, *, #10926, .T. ) ;
#44409 = CONICAL_SURFACE ( 'NONE', #74506, 2.500000000000000888, 0.9599310885968822538 ) ;
#44410 = VECTOR ( 'NONE', #106130, 1000.000000000000000 ) ;
#44411 = LINE ( 'NONE', #123396, #51090 ) ;
#44412 = CARTESIAN_POINT ( 'NONE',  ( -37.06996025486385093, -0.7407075233842735917, 13.87443053587619701 ) ) ;
#44413 = ORIENTED_EDGE ( 'NONE', *, *, #126582, .F. ) ;
#44414 = LINE ( 'NONE', #75593, #127237 ) ;
#44415 = VECTOR ( 'NONE', #7105, 1000.000000000000000 ) ;
#44416 = DIRECTION ( 'NONE',  ( 0.7071067811865487940, 0.7071067811865463515, -0.000000000000000000 ) ) ;
#44417 = VERTEX_POINT ( 'NONE', #110481 ) ;
#44418 = CARTESIAN_POINT ( 'NONE',  ( -5.999999999999958256, 2.966399257802234235, 5.000000000000000000 ) ) ;
#44420 = ORIENTED_EDGE ( 'NONE', *, *, #37070, .F. ) ;
#44419 = CARTESIAN_POINT ( 'NONE',  ( -2.816011393730999401, 28.73617430169785436, 5.000000000000000000 ) ) ;
#44421 = ORIENTED_EDGE ( 'NONE', *, *, #121421, .F. ) ;
#44422 = CARTESIAN_POINT ( 'NONE',  ( 13.36114865838684374, 9.181040837666923693, -27.38535958397034520 ) ) ;
#44423 = CARTESIAN_POINT ( 'NONE',  ( 31.49999999999978684, 18.05218569542898521, 5.000000000000000000 ) ) ;
#44424 = VECTOR ( 'NONE', #76435, 1000.000000000000000 ) ;
#44425 = VERTEX_POINT ( 'NONE', #11150 ) ;
#44426 = FILL_AREA_STYLE ('',( #52400 ) ) ;
#44427 = ADVANCED_FACE ( 'NONE', ( #285 ), #100357, .F. ) ;
#44428 = FACE_OUTER_BOUND ( 'NONE', #51800, .T. ) ;
#44429 = CARTESIAN_POINT ( 'NONE',  ( 1.353980332882009252, 4.584330080086930965E-16, 0.000000000000000000 ) ) ;
#44430 = ORIENTED_EDGE ( 'NONE', *, *, #14729, .F. ) ;
#44431 = PRODUCT ( '1.8 Handle Rod', '1.8 Handle Rod', '', ( #83010 ) ) ;
#44432 = CARTESIAN_POINT ( 'NONE',  ( -12.18398860626900060, 28.73617430169795739, 5.000000000000000000 ) ) ;
#44433 = DIRECTION ( 'NONE',  ( 0.7071067811865487940, 0.7071067811865463515, -0.000000000000000000 ) ) ;
#44434 = AXIS2_PLACEMENT_3D ( 'NONE', #63580, #115734, #139707 ) ;
#44435 = DIRECTION ( 'NONE',  ( 0.7071067811865486830, -0.7071067811865464625, -0.000000000000000000 ) ) ;
#44436 = VECTOR ( 'NONE', #96592, 1000.000000000000000 ) ;
#44437 = DIRECTION ( 'NONE',  ( -0.000000000000000000, 0.3543493200069153248, 0.9351131265310292928 ) ) ;
#44438 = CARTESIAN_POINT ( 'NONE',  ( 28.20376352523144803, 6.109999999999999432, 1.122388791418549108E-15 ) ) ;
#44439 = FACE_OUTER_BOUND ( 'NONE', #63661, .T. ) ;
#44440 = ORIENTED_EDGE ( 'NONE', *, *, #46790, .T. ) ;
#44441 = EDGE_LOOP ( 'NONE', ( #118807, #48674, #19725, #83975 ) ) ;
#44442 = DIRECTION ( 'NONE',  ( -0.000000000000000000, 0.3543493200069153248, 0.9351131265310292928 ) ) ;
#44443 = EDGE_LOOP ( 'NONE', ( #35230, #110435, #40396, #125901 ) ) ;
#44444 = VECTOR ( 'NONE', #68798, 1000.000000000000000 ) ;
#44445 = VERTEX_POINT ( 'NONE', #38666 ) ;
#44446 = CIRCLE ( 'NONE', #408, 3.000000000000000000 ) ;
#44447 = LINE ( 'NONE', #108922, #27034 ) ;
#44448 = CARTESIAN_POINT ( 'NONE',  ( 0.000000000000000000, 0.000000000000000000, 5.000000000000000000 ) ) ;
#44449 = EDGE_LOOP ( 'NONE', ( #1621, #19059, #70254, #65073 ) ) ;
#44450 = DIRECTION ( 'NONE',  ( 1.000000000000000000, 0.000000000000000000, 0.000000000000000000 ) ) ;
#44451 = DIRECTION ( 'NONE',  ( 0.000000000000000000, 0.000000000000000000, 1.000000000000000000 ) ) ;
#44452 = DIRECTION ( 'NONE',  ( 0.6830127018922181881, 0.6830127018922202975, -0.2588190451025214056 ) ) ;
#44453 = CARTESIAN_POINT ( 'NONE',  ( 124.6879301918981042, 6.110000000000002984, -1.637169565754156730 ) ) ;
#44454 = ORIENTED_EDGE ( 'NONE', *, *, #15465, .T. ) ;
#44455 = DIRECTION ( 'NONE',  ( 0.000000000000000000, -1.000000000000000000, 0.000000000000000000 ) ) ;
#44456 = LINE ( 'NONE', #111833, #125604 ) ;
#44458 = VECTOR ( 'NONE', #13008, 1000.000000000000000 ) ;
#44457 = CARTESIAN_POINT ( 'NONE',  ( -12.69999999999998153, 3.061616997868383634E-16, -2.500000000000000444 ) ) ;
#44459 = DIRECTION ( 'NONE',  ( 0.7071067811865487940, -0.7071067811865463515, 0.000000000000000000 ) ) ;
#44460 = FACE_BOUND ( 'NONE', #106387, .T. ) ;
#44461 = PLANE ( 'NONE',  #101359 ) ;
#44462 = CARTESIAN_POINT ( 'NONE',  ( 51.70419371712956291, -6.884901960086285300, -3.975000000000000089 ) ) ;
#44463 = DIRECTION ( 'NONE',  ( -0.7071067811865486830, 0.7071067811865464625, 0.000000000000000000 ) ) ;
#44464 = LINE ( 'NONE', #132904, #43875 ) ;
#44465 = ORIENTED_EDGE ( 'NONE', *, *, #10619, .T. ) ;
#44466 = ORIENTED_EDGE ( 'NONE', *, *, #65344, .F. ) ;
#44467 = CARTESIAN_POINT ( 'NONE',  ( 47.22916666666665719, 7.950000000000001954, -2.130196079827421762 ) ) ;
#44468 = EDGE_CURVE ( 'NONE', #47327, #142384, #114074, .T. ) ;
#44469 = DIRECTION ( 'NONE',  ( 0.7071067811865487940, -0.7071067811865463515, 0.000000000000000000 ) ) ;
#44470 = ORIENTED_EDGE ( 'NONE', *, *, #59209, .F. ) ;
#44471 = AXIS2_PLACEMENT_3D ( 'NONE', #136555, #83652, #138728 ) ;
#44472 = VECTOR ( 'NONE', #103020, 1000.000000000000227 ) ;
#44473 = DIRECTION ( 'NONE',  ( 0.7071067811865486830, -0.7071067811865464625, -0.000000000000000000 ) ) ;
#44474 = FACE_OUTER_BOUND ( 'NONE', #13576, .T. ) ;
#44475 = AXIS2_PLACEMENT_3D ( 'NONE', #132959, #56117, #35070 ) ;
#44476 = EDGE_CURVE ( 'NONE', #9428, #138835, #36519, .T. ) ;
#44477 = CARTESIAN_POINT ( 'NONE',  ( 38.64626352523144703, -4.472830434245840259, 4.472830434245839371 ) ) ;
#44478 = ORIENTED_EDGE ( 'NONE', *, *, #57872, .T. ) ;
#44479 = EDGE_CURVE ( 'NONE', #100907, #34581, #26364, .T. ) ;
#44480 = CARTESIAN_POINT ( 'NONE',  ( 15.21590231913187630, -1.409216073889147491, 4.328383627671532174 ) ) ;
#44481 = VERTEX_POINT ( 'NONE', #70621 ) ;
#44482 = ADVANCED_FACE ( 'NONE', ( #25628 ), #17179, .T. ) ;
#44483 = EDGE_LOOP ( 'NONE', ( #97070, #109743, #88933, #132190 ) ) ;
#44484 = VECTOR ( 'NONE', #26599, 1000.000000000000227 ) ;
#44485 = PRESENTATION_LAYER_ASSIGNMENT (  '', '', ( #90725 ) ) ;
#44486 =( GEOMETRIC_REPRESENTATION_CONTEXT ( 3 ) GLOBAL_UNCERTAINTY_ASSIGNED_CONTEXT ( ( #124435 ) ) GLOBAL_UNIT_ASSIGNED_CONTEXT ( ( #114529, #132222, #47894 ) ) REPRESENTATION_CONTEXT ( 'NONE', 'WORKASPACE' ) );
#44487 = DIRECTION ( 'NONE',  ( -0.7071067811865486830, -0.7071067811865464625, 0.000000000000000000 ) ) ;
#44488 = CARTESIAN_POINT ( 'NONE',  ( 81.45419371712955581, 6.884901960086283523, 3.975000000000002753 ) ) ;
#44489 = SURFACE_STYLE_FILL_AREA ( #23397 ) ;
#44490 = EDGE_CURVE ( 'NONE', #62199, #122251, #14762, .T. ) ;
#44491 = DIRECTION ( 'NONE',  ( -0.3543493200069162685, -0.000000000000000000, -0.9351131265310288487 ) ) ;
#44492 = ORIENTED_EDGE ( 'NONE', *, *, #122229, .T. ) ;
#44493 = LINE ( 'NONE', #122723, #41899 ) ;
#44494 = EDGE_CURVE ( 'NONE', #40635, #45746, #16910, .T. ) ;
#44495 = EDGE_CURVE ( 'NONE', #39017, #45797, #105333, .T. ) ;
#44496 = VERTEX_POINT ( 'NONE', #61864 ) ;
#44497 = CARTESIAN_POINT ( 'NONE',  ( 86.77126352523143282, 4.472830434245838482, 4.472830434245842035 ) ) ;
#44498 = CARTESIAN_POINT ( 'NONE',  ( -38.99451991528749062, 28.92564299267965211, 4.000000000000000000 ) ) ;
#44499 = CARTESIAN_POINT ( 'NONE',  ( 8.207106781186489286, -14.24070752338414181, 5.000000000000000000 ) ) ;
#44500 = CARTESIAN_POINT ( 'NONE',  ( -5.816011393731002066, 28.73617430169783304, 5.000000000000000000 ) ) ;
#44501 = CARTESIAN_POINT ( 'NONE',  ( -16.82816939922340893, 12.75929247661558819, 4.000000000000000000 ) ) ;
#44502 = EDGE_CURVE ( 'NONE', #59940, #80353, #50264, .T. ) ;
#44503 = ADVANCED_FACE ( 'NONE', ( #116928 ), #94453, .F. ) ;
#44504 = EDGE_LOOP ( 'NONE', ( #111072, #60424, #58341, #1546 ) ) ;
#44505 = CARTESIAN_POINT ( 'NONE',  ( -34.42499999999997584, -22.26999999999999247, -0.5000000000000000000 ) ) ;
#44506 = CARTESIAN_POINT ( 'NONE',  ( 61.45376352523145158, -6.109999999999998543, -3.741295971395162543E-16 ) ) ;
#44507 = CARTESIAN_POINT ( 'NONE',  ( 21.46453280170069888, 4.202752102959690472E-16, 0.000000000000000000 ) ) ;
#44508 = EDGE_CURVE ( 'NONE', #42793, #121499, #83622, .T. ) ;
#44509 = CARTESIAN_POINT ( 'NONE',  ( -21.18398860626899349, 28.73617430169802134, 5.000000000000000000 ) ) ;
#44510 = FACE_OUTER_BOUND ( 'NONE', #66001, .T. ) ;
#44511 = ORIENTED_EDGE ( 'NONE', *, *, #37521, .T. ) ;
#44512 = ORIENTED_EDGE ( 'NONE', *, *, #16145, .T. ) ;
#44513 = DIRECTION ( 'NONE',  ( -0.6830127018922180770, -0.6830127018922204085, -0.2588190451025213501 ) ) ;
#44514 =( NAMED_UNIT ( * ) SI_UNIT ( $, .STERADIAN. ) SOLID_ANGLE_UNIT ( ) );
#44515 = ORIENTED_EDGE ( 'NONE', *, *, #56477, .T. ) ;
#44516 = VECTOR ( 'NONE', #70057, 1000.000000000000000 ) ;
#44517 = ADVANCED_FACE ( 'NONE', ( #137269 ), #5288, .T. ) ;
#44518 = VECTOR ( 'NONE', #111317, 1000.000000000000000 ) ;
#44519 = DIRECTION ( 'NONE',  ( -0.000000000000000000, 0.000000000000000000, 1.000000000000000000 ) ) ;
#44520 = ORIENTED_EDGE ( 'NONE', *, *, #108266, .F. ) ;
#44521 = AXIS2_PLACEMENT_3D ( 'NONE', #76094, #61671, #140617 ) ;
#44522 = CARTESIAN_POINT ( 'NONE',  ( -44.99451991528749772, 28.92564299267969474, 4.000000000000000000 ) ) ;
#44523 = DIRECTION ( 'NONE',  ( 0.7071067811865486830, -0.7071067811865464625, -0.000000000000000000 ) ) ;
#44524 = PLANE ( 'NONE',  #134180 ) ;
#44525 = VECTOR ( 'NONE', #111083, 1000.000000000000000 ) ;
#44526 = CARTESIAN_POINT ( 'NONE',  ( -60.18398860626900415, 28.73617430169829490, 5.000000000000000000 ) ) ;
#44527 = FACE_BOUND ( 'NONE', #56530, .T. ) ;
#44528 = CARTESIAN_POINT ( 'NONE',  ( -81.48921356237309510, -27.52281430457112066, 5.000000000000000000 ) ) ;
#44529 = DIRECTION ( 'NONE',  ( -0.000000000000000000, 0.3543493200069153248, 0.9351131265310292928 ) ) ;
#44530 = CARTESIAN_POINT ( 'NONE',  ( 29.52487387214936376, 14.25929247661557397, 9.797011795316704408 ) ) ;
#44532 = EDGE_LOOP ( 'NONE', ( #111454, #42103, #16699, #21340 ) ) ;
#44531 = CARTESIAN_POINT ( 'NONE',  ( -1.499999999999987566, -7.420205493532900931, -2.617629953481256599 ) ) ;
#44533 = EDGE_CURVE ( 'NONE', #8796, #47010, #50971, .T. ) ;
#44534 = AXIS2_PLACEMENT_3D ( 'NONE', #134206, #142242, #12401 ) ;
#44535 = CYLINDRICAL_SURFACE ( 'NONE', #57, 2.500000000000000444 ) ;
#44536 = CONTEXT_DEPENDENT_SHAPE_REPRESENTATION ( #81955, #29603 ) ;
#44537 = ORIENTED_EDGE ( 'NONE', *, *, #100455, .T. ) ;
#44538 = ORIENTED_EDGE ( 'NONE', *, *, #21484, .T. ) ;
#44539 = CARTESIAN_POINT ( 'NONE',  ( 78.95376352523145158, -6.109999999999998543, -3.741295971395162543E-16 ) ) ;
#44540 = VERTEX_POINT ( 'NONE', #49572 ) ;
#44541 = CARTESIAN_POINT ( 'NONE',  ( 84.18398860626899705, 28.73617430169846187, 5.000000000000000000 ) ) ;
#44542 = CARTESIAN_POINT ( 'NONE',  ( -3.792893218813422340, 9.759292476615620160, 5.000000000000000000 ) ) ;
#44543 = VECTOR ( 'NONE', #85274, 1000.000000000000000 ) ;
#44544 = EDGE_CURVE ( 'NONE', #86478, #92341, #116717, .T. ) ;
#44545 = EDGE_LOOP ( 'NONE', ( #125795, #51782, #21528, #29535 ) ) ;
#44546 = CARTESIAN_POINT ( 'NONE',  ( 17.99999999999986855, -22.06887692260758271, 4.000000000000000000 ) ) ;
#44547 = VECTOR ( 'NONE', #55116, 1000.000000000000227 ) ;
#44548 = DIRECTION ( 'NONE',  ( -0.000000000000000000, -0.3543493200069152693, 0.9351131265310292928 ) ) ;
#44549 = EDGE_CURVE ( 'NONE', #12475, #57697, #92303, .T. ) ;
#44550 = CARTESIAN_POINT ( 'NONE',  ( 18.48921356237309510, -27.52281430457068367, 5.000000000000000000 ) ) ;
#44551 = DIRECTION ( 'NONE',  ( 0.3543493200069162685, -0.000000000000000000, -0.9351131265310288487 ) ) ;
#44552 = DIRECTION ( 'NONE',  ( -0.7071067811865486830, -0.7071067811865464625, -0.000000000000000000 ) ) ;
#44553 = FACE_OUTER_BOUND ( 'NONE', #63281, .T. ) ;
#44554 = ADVANCED_FACE ( 'NONE', ( #125684 ), #114760, .T. ) ;
#44555 = DIRECTION ( 'NONE',  ( 0.6830127018922181881, 0.6830127018922202975, -0.2588190451025214056 ) ) ;
#44556 = DIRECTION ( 'NONE',  ( 0.6830127018922180770, -0.6830127018922204085, -0.2588190451025213501 ) ) ;
#44557 = ORIENTED_EDGE ( 'NONE', *, *, #119078, .F. ) ;
#44558 = VECTOR ( 'NONE', #34770, 1000.000000000000000 ) ;
#44559 = DIRECTION ( 'NONE',  ( -0.000000000000000000, 0.000000000000000000, 1.000000000000000000 ) ) ;
#44560 = EDGE_LOOP ( 'NONE', ( #9282, #12767, #82876, #38886 ) ) ;
#44561 =( BOUNDED_CURVE ( )  B_SPLINE_CURVE ( 3, ( #120919, #78150, #122324, #87584 ),
 .UNSPECIFIED., .F., .T. ) 
 B_SPLINE_CURVE_WITH_KNOTS ( ( 4, 4 ),
 ( 1.864375635226937611, 1.933014472006542750 ),
 .UNSPECIFIED. ) 
 CURVE ( )  GEOMETRIC_REPRESENTATION_ITEM ( )  RATIONAL_B_SPLINE_CURVE ( ( 1.000000000000000000, 0.9996074310407765395, 0.9996074310407765395, 1.000000000000000000 ) ) 
 REPRESENTATION_ITEM ( '' )  );
#44562 = CARTESIAN_POINT ( 'NONE',  ( -26.99451991528749417, 28.92564299267956685, 4.000000000000000000 ) ) ;
#44563 = ADVANCED_FACE ( 'NONE', ( #115462 ), #10222, .T. ) ;
#44564 = ORIENTED_EDGE ( 'NONE', *, *, #1250, .T. ) ;
#44565 = ORIENTED_EDGE ( 'NONE', *, *, #75145, .F. ) ;
#44566 = CARTESIAN_POINT ( 'NONE',  ( 25.22959685856476497, -6.110000000000000320, -1.637169565754161393 ) ) ;
#44567 = AXIS2_PLACEMENT_3D ( 'NONE', #69789, #49465, #37115 ) ;
#44568 = EDGE_LOOP ( 'NONE', ( #96405, #98014, #41200, #78570, #93717 ) ) ;
#44569 = CARTESIAN_POINT ( 'NONE',  ( -3.299744871391591339, -27.71228299555208352, 4.000000000000000000 ) ) ;
#44570 = EDGE_CURVE ( 'NONE', #44719, #128385, #82201, .T. ) ;
#44571 = CARTESIAN_POINT ( 'NONE',  ( 18.70612307739183322, 22.22500000000000142, 4.000000000000000000 ) ) ;
#44572 = CARTESIAN_POINT ( 'NONE',  ( 4.004569808101885897, 6.871911579029510442, -3.967499999999998916 ) ) ;
#44573 = DIRECTION ( 'NONE',  ( 0.6830127018922180770, -0.6830127018922204085, -0.2588190451025213501 ) ) ;
#44574 = VERTEX_POINT ( 'NONE', #137985 ) ;
#44575 = EDGE_CURVE ( 'NONE', #80908, #43048, #109617, .T. ) ;
#44576 = PLANE ( 'NONE',  #82822 ) ;
#44577 = EDGE_LOOP ( 'NONE', ( #81197, #117918, #110046, #119005 ) ) ;
#44578 = CARTESIAN_POINT ( 'NONE',  ( -8.999999999999936051, 18.08204922493372990, 0.9627537363045106655 ) ) ;
#44579 = LINE ( 'NONE', #101041, #70702 ) ;
#44580 = VECTOR ( 'NONE', #126745, 1000.000000000000114 ) ;
#44581 = VECTOR ( 'NONE', #119932, 1000.000000000000227 ) ;
#44583 = VERTEX_POINT ( 'NONE', #74889 ) ;
#44582 = LINE ( 'NONE', #130859, #107263 ) ;
#44584 = VECTOR ( 'NONE', #74621, 1000.000000000000227 ) ;
#44585 = ORIENTED_EDGE ( 'NONE', *, *, #134100, .F. ) ;
#44586 = CARTESIAN_POINT ( 'NONE',  ( -32.99999999999977263, 16.93112307739200872, 4.000000000000000000 ) ) ;
#44587 = VECTOR ( 'NONE', #59040, 1000.000000000000000 ) ;
#44588 = DIRECTION ( 'NONE',  ( -0.7071067811865486830, 0.7071067811865464625, 0.000000000000000000 ) ) ;
#44590 = EDGE_LOOP ( 'NONE', ( #141527, #106401, #107079 ) ) ;
#44589 = AXIS2_PLACEMENT_3D ( 'NONE', #97048, #28991, #108646 ) ;
#44591 = LINE ( 'NONE', #31010, #68758 ) ;
#44592 = ORIENTED_EDGE ( 'NONE', *, *, #68731, .F. ) ;
#44593 = EDGE_CURVE ( 'NONE', #13610, #24129, #117607, .T. ) ;
#44594 = PLANE ( 'NONE',  #109702 ) ;
#44595 = CARTESIAN_POINT ( 'NONE',  ( 34.92499999999998295, 2.816654386410421207, 4.500000000000000888 ) ) ;
#44596 = DIRECTION ( 'NONE',  ( 0.7071067811865487940, 0.7071067811865463515, -0.000000000000000000 ) ) ;
#44597 = VECTOR ( 'NONE', #11786, 1000.000000000000000 ) ;
#44598 = STYLED_ITEM ( 'NONE', ( #67319 ), #50002 ) ;
#44599 = LINE ( 'NONE', #33001, #6757 ) ;
#44600 = CARTESIAN_POINT ( 'NONE',  ( -31.92499999999997584, -6.270000000000012008, -37.00000000000000000 ) ) ;
#44601 = DIRECTION ( 'NONE',  ( 0.6830127018922180770, -0.6830127018922204085, -0.2588190451025213501 ) ) ;
#44602 = DIRECTION ( 'NONE',  ( 0.7071067811865486830, -0.7071067811865464625, -0.000000000000000000 ) ) ;
#44603 = EDGE_CURVE ( 'NONE', #103813, #115637, #42253, .T. ) ;
#44604 = LINE ( 'NONE', #88795, #11266 ) ;
#44605 = ORIENTED_EDGE ( 'NONE', *, *, #76279, .F. ) ;
#44607 = EDGE_CURVE ( 'NONE', #129536, #25281, #14196, .T. ) ;
#44606 = CARTESIAN_POINT ( 'NONE',  ( -26.99999999999980105, 2.966399257802232459, 5.000000000000000000 ) ) ;
#44608 = ORIENTED_EDGE ( 'NONE', *, *, #95558, .T. ) ;
#44609 = CARTESIAN_POINT ( 'NONE',  ( 24.79289321881328334, -11.24070752338417378, 5.000000000000000000 ) ) ;
#44610 = DIRECTION ( 'NONE',  ( -1.000000000000000000, -0.000000000000000000, -0.000000000000000000 ) ) ;
#44611 = DIRECTION ( 'NONE',  ( 1.000000000000000000, 0.000000000000000000, 0.000000000000000000 ) ) ;
#44612 = DIRECTION ( 'NONE',  ( 1.000000000000000000, -0.000000000000000000, -0.000000000000000000 ) ) ;
#44613 = EDGE_LOOP ( 'NONE', ( #28478, #93137, #127936, #127992 ) ) ;
#44614 = CARTESIAN_POINT ( 'NONE',  ( 36.48921356237310221, -27.52281430457080802, 5.000000000000000000 ) ) ;
#44615 = CARTESIAN_POINT ( 'NONE',  ( 9.183988606268997046, 28.73617430169793607, 5.000000000000000000 ) ) ;
#44616 = CARTESIAN_POINT ( 'NONE',  ( -72.18398860626899705, 28.73617430169837661, 5.000000000000000000 ) ) ;
#44617 = EDGE_LOOP ( 'NONE', ( #10148, #27644, #55268, #24104 ) ) ;
#44618 = DIRECTION ( 'NONE',  ( -0.000000000000000000, -0.3543493200069152693, 0.9351131265310292928 ) ) ;
#44619 = PLANE ( 'NONE',  #115925 ) ;
#44620 = DIRECTION ( 'NONE',  ( -0.7071067811865486830, -0.7071067811865464625, -0.000000000000000000 ) ) ;
#44621 = SURFACE_STYLE_USAGE ( .BOTH. , #11183 ) ;
#44622 = FACE_OUTER_BOUND ( 'NONE', #52050, .T. ) ;
#44623 = CARTESIAN_POINT ( 'NONE',  ( 54.89126352523145158, -4.472830434245839371, -4.472830434245839371 ) ) ;
#44624 = EDGE_CURVE ( 'NONE', #74278, #137039, #129219, .T. ) ;
#44625 = CARTESIAN_POINT ( 'NONE',  ( -0.7201904164744685755, -22.22500000000000142, -7.961480994124567445 ) ) ;
#44626 = CARTESIAN_POINT ( 'NONE',  ( -7.828169399223469327, -17.24070752338410628, 4.000000000000000000 ) ) ;
#44627 = EDGE_CURVE ( 'NONE', #100863, #70912, #30659, .T. ) ;
#44628 = DIRECTION ( 'NONE',  ( 0.7071067811865486830, -0.7071067811865464625, -0.000000000000000000 ) ) ;
#44629 = DIRECTION ( 'NONE',  ( 0.6830127018922181881, 0.6830127018922202975, -0.2588190451025214056 ) ) ;
#44630 = AXIS2_PLACEMENT_3D ( 'NONE', #67191, #111388, #131739 ) ;
#44631 = ORIENTED_EDGE ( 'NONE', *, *, #42517, .F. ) ;
#44632 = CARTESIAN_POINT ( 'NONE',  ( 0.000000000000000000, 9.913515839097813477E-16, -8.094999999999991758 ) ) ;
#44633 = VERTEX_POINT ( 'NONE', #20452 ) ;
#44634 = CARTESIAN_POINT ( 'NONE',  ( 1.499999999999980460, 22.08746187583903975, 4.000000000000000000 ) ) ;
#44636 = CIRCLE ( 'NONE', #74616, 2.500000000000000888 ) ;
#44635 = DIRECTION ( 'NONE',  ( 0.7071067811865487940, 0.7071067811865463515, 0.000000000000000000 ) ) ;
#44637 = LINE ( 'NONE', #23544, #29881 ) ;
#44638 = CARTESIAN_POINT ( 'NONE',  ( -7.828169399223476432, 3.759292476615681888, 4.000000000000000000 ) ) ;
#44639 = DIRECTION ( 'NONE',  ( -1.000000000000000000, 0.000000000000000000, 0.000000000000000000 ) ) ;
#44640 = ADVANCED_FACE ( 'NONE', ( #140804 ), #62567, .F. ) ;
#44641 = CARTESIAN_POINT ( 'NONE',  ( -32.99999999999977263, 17.96639925780207747, 5.000000000000000000 ) ) ;
#44642 = CARTESIAN_POINT ( 'NONE',  ( -29.99999999999978684, 11.58746187583912679, 4.000000000000000000 ) ) ;
#44643 = ORIENTED_EDGE ( 'NONE', *, *, #138941, .F. ) ;
#44644 = EDGE_LOOP ( 'NONE', ( #51526, #97017, #61574, #4161 ) ) ;
#44645 = PLANE ( 'NONE',  #99619 ) ;
#44646 = PLANE ( 'NONE',  #106939 ) ;
#44647 = UNCERTAINTY_MEASURE_WITH_UNIT (LENGTH_MEASURE( 1.000000000000000082E-05 ), #58733, 'distance_accuracy_value', 'NONE');
#44648 = DIRECTION ( 'NONE',  ( -0.6830127018922180770, -0.6830127018922204085, -0.2588190451025213501 ) ) ;
#44649 = DIRECTION ( 'NONE',  ( 0.5735764363510453823, -0.8191520442889923537, 1.003171929053525486E-16 ) ) ;
#44650 = CARTESIAN_POINT ( 'NONE',  ( 81.30836038379624142, 7.949999999999997513, 2.130196079827431088 ) ) ;
#44651 = DIRECTION ( 'NONE',  ( 0.7071067811865487940, -0.7071067811865463515, 0.000000000000000000 ) ) ;
#44652 = CARTESIAN_POINT ( 'NONE',  ( -25.49999999999982236, 18.43112307739199451, 4.000000000000000000 ) ) ;
#44653 = VERTEX_POINT ( 'NONE', #52380 ) ;
#44654 = CARTESIAN_POINT ( 'NONE',  ( 74.35416666666664298, -2.130196079827425315, -7.950000000000001066 ) ) ;
#44655 = LINE ( 'NONE', #32316, #137234 ) ;
#44656 = LINE ( 'NONE', #14098, #32404 ) ;
#44658 = AXIS2_PLACEMENT_3D ( 'NONE', #55536, #11267, #401 ) ;
#44657 = LINE ( 'NONE', #77964, #61403 ) ;
#44659 = EDGE_LOOP ( 'NONE', ( #81083, #3162, #96886, #108466 ) ) ;
#44660 = CARTESIAN_POINT ( 'NONE',  ( 29.67183060077626422, -0.7407075233842770334, 4.000000000000000000 ) ) ;
#44661 = EDGE_LOOP ( 'NONE', ( #124137, #12842, #14218 ) ) ;
#44662 = EDGE_CURVE ( 'NONE', #110589, #24532, #139441, .T. ) ;
#44663 = DIRECTION ( 'NONE',  ( -0.5735764363510503783, -0.8191520442889886899, 0.000000000000000000 ) ) ;
#44664 = CARTESIAN_POINT ( 'NONE',  ( 61.97959685856476852, 6.109999999999999432, 1.637169565754164280 ) ) ;
#44665 = PLANE ( 'NONE',  #91709 ) ;
#44666 = EDGE_LOOP ( 'NONE', ( #18212, #109786, #128975, #44122 ) ) ;
#44667 = VECTOR ( 'NONE', #114360, 1000.000000000000000 ) ;
#44668 = CARTESIAN_POINT ( 'NONE',  ( 18.18398860626898994, 28.73617430169800002, 5.000000000000000000 ) ) ;
#44669 = FACE_OUTER_BOUND ( 'NONE', #107023, .T. ) ;
#44670 = PRESENTATION_STYLE_ASSIGNMENT (( #377 ) ) ;
#44671 = LINE ( 'NONE', #30912, #111094 ) ;
#44672 = CARTESIAN_POINT ( 'NONE',  ( -63.48921356237309510, -27.52281430457099631, 5.000000000000000000 ) ) ;
#44673 = ADVANCED_FACE ( 'NONE', ( #63308 ), #118342, .T. ) ;
#44675 = ORIENTED_EDGE ( 'NONE', *, *, #126154, .F. ) ;
#44674 = CARTESIAN_POINT ( 'NONE',  ( 34.42499999999998295, -9.022814304570511368, 5.000000000000000000 ) ) ;
#44676 = PRESENTATION_STYLE_ASSIGNMENT (( #19999 ) ) ;
#44677 = CARTESIAN_POINT ( 'NONE',  ( 8.999999999999937828, -15.41253812416059787, 4.000000000000000000 ) ) ;
#44678 = VECTOR ( 'NONE', #103097, 1000.000000000000000 ) ;
#44679 = DIRECTION ( 'NONE',  ( 0.7071067811865487940, 0.7071067811865463515, 0.000000000000000000 ) ) ;
#44680 = CARTESIAN_POINT ( 'NONE',  ( -35.99451991528749772, 28.92564299267963079, 4.000000000000000000 ) ) ;
#44681 = ORIENTED_EDGE ( 'NONE', *, *, #60372, .F. ) ;
#44683 = ORIENTED_EDGE ( 'NONE', *, *, #64980, .T. ) ;
#44682 = EDGE_CURVE ( 'NONE', #73050, #63324, #98315, .T. ) ;
#44684 = EDGE_CURVE ( 'NONE', #66820, #49172, #96566, .T. ) ;
#44685 = CARTESIAN_POINT ( 'NONE',  ( 65.62543019189810423, 5.291415217122919401, 3.055000000000002824 ) ) ;
#44686 = VERTEX_POINT ( 'NONE', #98044 ) ;
#44687 = EDGE_CURVE ( 'NONE', #133905, #24699, #89161, .T. ) ;
#44688 = DIRECTION ( 'NONE',  ( 0.000000000000000000, -1.000000000000000000, 0.000000000000000000 ) ) ;
#44689 = CARTESIAN_POINT ( 'NONE',  ( 0.000000000000000000, 0.000000000000000000, 10.00000000000000000 ) ) ;
#44690 = EDGE_CURVE ( 'NONE', #46869, #140963, #131386, .T. ) ;
#44691 = PLANE ( 'NONE',  #105929 ) ;
#44692 = CARTESIAN_POINT ( 'NONE',  ( 22.85159235450332105, 9.902892378096218942E-16, 0.000000000000000000 ) ) ;
#44693 = ORIENTED_EDGE ( 'NONE', *, *, #142369, .F. ) ;
#44694 = ORIENTED_EDGE ( 'NONE', *, *, #32951, .T. ) ;
#44695 = CIRCLE ( 'NONE', #114069, 2.500000000000000444 ) ;
#44696 = EDGE_CURVE ( 'NONE', #143429, #123374, #84338, .T. ) ;
#44697 = CARTESIAN_POINT ( 'NONE',  ( -7.499999999999945821, -20.53675388469231322, 2.352720554255875562 ) ) ;
#44698 = AXIS2_PLACEMENT_3D ( 'NONE', #60447, #136527, #124240 ) ;
#44699 = VECTOR ( 'NONE', #63279, 1000.000000000000000 ) ;
#44700 = EDGE_CURVE ( 'NONE', #5088, #64283, #51694, .T. ) ;
#44701 = ORIENTED_EDGE ( 'NONE', *, *, #131723, .F. ) ;
#44702 = DIRECTION ( 'NONE',  ( 0.7071067811865487940, 0.7071067811865463515, 0.000000000000000000 ) ) ;
#44704 = DIRECTION ( 'NONE',  ( 0.7071067811865487940, 0.7071067811865463515, 0.000000000000000000 ) ) ;
#44703 = VECTOR ( 'NONE', #72760, 1000.000000000000000 ) ;
#44705 = DIRECTION ( 'NONE',  ( 0.7071067811865487940, 0.7071067811865463515, 0.000000000000000000 ) ) ;
#44706 = AXIS2_PLACEMENT_3D ( 'NONE', #111463, #1942, #78867 ) ;
#44707 =( GEOMETRIC_REPRESENTATION_CONTEXT ( 3 ) GLOBAL_UNCERTAINTY_ASSIGNED_CONTEXT ( ( #101081 ) ) GLOBAL_UNIT_ASSIGNED_CONTEXT ( ( #15718, #17203, #62150 ) ) REPRESENTATION_CONTEXT ( 'NONE', 'WORKASPACE' ) );
#44708 = ORIENTED_EDGE ( 'NONE', *, *, #53464, .T. ) ;
#44709 = EDGE_CURVE ( 'NONE', #44574, #139771, #122631, .T. ) ;
#44710 = EDGE_CURVE ( 'NONE', #38177, #45110, #89998, .T. ) ;
#44711 = FACE_BOUND ( 'NONE', #124200, .T. ) ;
#44712 = CARTESIAN_POINT ( 'NONE',  ( 14.70692117890024697, 4.584330080086930965E-16, 0.000000000000000000 ) ) ;
#44713 = CARTESIAN_POINT ( 'NONE',  ( -31.49999999999979039, -7.420205493532932017, -2.617629953481324101 ) ) ;
#44714 = CARTESIAN_POINT ( 'NONE',  ( -17.21574841994372562, 22.22500000000000142, 11.71069743027089061 ) ) ;
#44715 = CARTESIAN_POINT ( 'NONE',  ( -7.171830600776418763, 21.75929247661548871, 4.000000000000000000 ) ) ;
#44716 = ADVANCED_FACE ( 'NONE', ( #134246 ), #55255, .F. ) ;
#44717 = CARTESIAN_POINT ( 'NONE',  ( 20.99999999999985079, -21.03360074219752462, 5.000000000000000000 ) ) ;
#44718 = FILL_AREA_STYLE ('',( #63598 ) ) ;
#44719 = VERTEX_POINT ( 'NONE', #21894 ) ;
#44720 = ORIENTED_EDGE ( 'NONE', *, *, #143162, .T. ) ;
#44721 = CARTESIAN_POINT ( 'NONE',  ( 102.8704301918981230, -3.055000000000001492, 5.291415217122917625 ) ) ;
#44722 = VERTEX_POINT ( 'NONE', #12440 ) ;
#44723 = DIRECTION ( 'NONE',  ( -0.000000000000000000, 0.000000000000000000, 1.000000000000000000 ) ) ;
#44724 = ORIENTED_EDGE ( 'NONE', *, *, #127366, .F. ) ;
#44725 = PLANE ( 'NONE',  #141900 ) ;
#44726 = VECTOR ( 'NONE', #113698, 1000.000000000000000 ) ;
#44727 = DIRECTION ( 'NONE',  ( -1.321231229586337907E-16, 0.9647414015272155474, -0.2631995976047525887 ) ) ;
#44728 = DIRECTION ( 'NONE',  ( -0.7071067811865486830, 0.7071067811865464625, 0.000000000000000000 ) ) ;
#44729 = EDGE_LOOP ( 'NONE', ( #48603, #83775, #62174, #128259 ) ) ;
#44730 = CARTESIAN_POINT ( 'NONE',  ( 0.7061230773919568993, 22.22500000000000142, 4.000000000000000000 ) ) ;
#44731 = CARTESIAN_POINT ( 'NONE',  ( 15.00548008471250228, 28.92564299267927552, 4.000000000000000000 ) ) ;
#44732 = LINE ( 'NONE', #127585, #12960 ) ;
#44733 = DIRECTION ( 'NONE',  ( -0.7071067811865486830, 0.7071067811865464625, 0.000000000000000000 ) ) ;
#44735 = CARTESIAN_POINT ( 'NONE',  ( -20.77868544475317947, 8.889383937919465239, 4.212719859983343973 ) ) ;
#44734 = CARTESIAN_POINT ( 'NONE',  ( -15.79333936457836707, 21.75929247661549937, 4.998822639870700080 ) ) ;
#44736 = EDGE_CURVE ( 'NONE', #138729, #136079, #77029, .T. ) ;
#44737 = CARTESIAN_POINT ( 'NONE',  ( 2.510786437626908008, -27.52281430457053446, 5.000000000000000000 ) ) ;
#44738 = DIRECTION ( 'NONE',  ( -0.000000000000000000, 0.000000000000000000, 1.000000000000000000 ) ) ;
#44739 = VERTEX_POINT ( 'NONE', #66843 ) ;
#44740 = FACE_OUTER_BOUND ( 'NONE', #123726, .T. ) ;
#44741 = CARTESIAN_POINT ( 'NONE',  ( 26.29289321881327623, -3.740707523384243505, 5.000000000000000000 ) ) ;
#44742 = VERTEX_POINT ( 'NONE', #99436 ) ;
#44743 = ORIENTED_EDGE ( 'NONE', *, *, #5050, .F. ) ;
#44744 = ORIENTED_EDGE ( 'NONE', *, *, #44245, .T. ) ;
#44745 = CARTESIAN_POINT ( 'NONE',  ( 56.14626352523143993, -4.472830434245840259, 4.472830434245838482 ) ) ;
#44746 = VERTEX_POINT ( 'NONE', #87873 ) ;
#44747 = ADVANCED_FACE ( 'NONE', ( #24752 ), #110310, .F. ) ;
#44748 = AXIS2_PLACEMENT_3D ( 'NONE', #30126, #115138, #85215 ) ;
#44749 = DIRECTION ( 'NONE',  ( 0.7071067811865486830, -0.7071067811865464625, -0.000000000000000000 ) ) ;
#44750 = CARTESIAN_POINT ( 'NONE',  ( -1.995860383796227877, -3.047499999999994547, 5.278424836066145431 ) ) ;
#44751 = CARTESIAN_POINT ( 'NONE',  ( 87.64626352523143282, -4.472830434245840259, 4.472830434245838482 ) ) ;
#44752 = CARTESIAN_POINT ( 'NONE',  ( 36.29974487139159578, -27.71228299555231445, 4.000000000000000000 ) ) ;
#44753 = MANIFOLD_SOLID_BREP ( 'Cut-Extrude1', #4621 ) ;
#44754 = ADVANCED_FACE ( 'NONE', ( #34939 ), #56723, .F. ) ;
#44755 = VECTOR ( 'NONE', #74993, 1000.000000000000000 ) ;
#44756 = EDGE_LOOP ( 'NONE', ( #109580, #107068, #123158, #80882 ) ) ;
#44757 = DIRECTION ( 'NONE',  ( 0.7071067811865487940, -0.7071067811865463515, 0.000000000000000000 ) ) ;
#44758 = VECTOR ( 'NONE', #50674, 1000.000000000000000 ) ;
#44759 = CARTESIAN_POINT ( 'NONE',  ( 25.00934544866806064, 2.809161053235903704, 4.346514962826528716 ) ) ;
#44760 = EDGE_LOOP ( 'NONE', ( #22725, #15060, #105210, #71362 ) ) ;
#44761 = DIRECTION ( 'NONE',  ( 0.000000000000000000, -1.000000000000000000, 0.000000000000000000 ) ) ;
#44762 = LINE ( 'NONE', #100530, #77632 ) ;
#44763 = ORIENTED_EDGE ( 'NONE', *, *, #137972, .T. ) ;
#44764 = CARTESIAN_POINT ( 'NONE',  ( 23.50183651486029746, -17.24070752338409918, 8.407044977365172755 ) ) ;
#44765 = EDGE_CURVE ( 'NONE', #72919, #48675, #91388, .T. ) ;
#44766 = EDGE_LOOP ( 'NONE', ( #79828, #24021, #55624, #114857 ) ) ;
#44767 = ORIENTED_EDGE ( 'NONE', *, *, #110314, .T. ) ;
#44768 = ORIENTED_EDGE ( 'NONE', *, *, #88062, .T. ) ;
#44769 = CARTESIAN_POINT ( 'NONE',  ( 119.7870968585647802, 3.054999999999997495, 5.291415217122919401 ) ) ;
#44770 = AXIS2_PLACEMENT_3D ( 'NONE', #92479, #46923, #68637 ) ;
#44771 = FACE_OUTER_BOUND ( 'NONE', #48447, .T. ) ;
#44772 = ADVANCED_FACE ( 'NONE', ( #77727 ), #121902, .F. ) ;
#44773 = CARTESIAN_POINT ( 'NONE',  ( 34.92499999999997584, 13.80009451602703408, 4.759050581649328038 ) ) ;
#44774 = ORIENTED_EDGE ( 'NONE', *, *, #14161, .F. ) ;
#44775 = DIRECTION ( 'NONE',  ( 1.000000000000000000, 0.000000000000000000, 0.000000000000000000 ) ) ;
#44776 = AXIS2_PLACEMENT_3D ( 'NONE', #38382, #82597, #121625 ) ;
#44777 = ORIENTED_EDGE ( 'NONE', *, *, #45723, .F. ) ;
#44778 = CARTESIAN_POINT ( 'NONE',  ( 13.24956980810188689, 3.967499999999998916, 6.871911579029510442 ) ) ;
#44779 = EDGE_CURVE ( 'NONE', #43782, #94364, #45821, .T. ) ;
#44780 =( NAMED_UNIT ( * ) SI_UNIT ( $, .STERADIAN. ) SOLID_ANGLE_UNIT ( ) );
#44781 = CARTESIAN_POINT ( 'NONE',  ( 34.92500000000001137, 22.27000000000000668, 0.000000000000000000 ) ) ;
#44782 = CARTESIAN_POINT ( 'NONE',  ( -2.292893218813438772, 5.259292476615662792, 5.000000000000000000 ) ) ;
#44783 = ORIENTED_EDGE ( 'NONE', *, *, #118575, .F. ) ;
#44784 = ORIENTED_EDGE ( 'NONE', *, *, #4316, .T. ) ;
#44785 = ORIENTED_EDGE ( 'NONE', *, *, #6469, .F. ) ;
#44786 = DIRECTION ( 'NONE',  ( 0.7071067811865486830, -0.7071067811865464625, -0.000000000000000000 ) ) ;
#44787 = CARTESIAN_POINT ( 'NONE',  ( -9.489213562373095101, -27.52281430457062328, 5.000000000000000000 ) ) ;
#44788 = UNCERTAINTY_MEASURE_WITH_UNIT (LENGTH_MEASURE( 1.000000000000000082E-05 ), #88140, 'distance_accuracy_value', 'NONE');
#44789 = VECTOR ( 'NONE', #49234, 1000.000000000000000 ) ;
#44790 = DIRECTION ( 'NONE',  ( -0.000000000000000000, 0.000000000000000000, 1.000000000000000000 ) ) ;
#44792 = ADVANCED_FACE ( 'NONE', ( #13139 ), #24050, .F. ) ;
#44791 = LINE ( 'NONE', #133205, #66823 ) ;
#44794 = EDGE_CURVE ( 'NONE', #98171, #102362, #113904, .T. ) ;
#44793 = VECTOR ( 'NONE', #119035, 1000.000000000000000 ) ;
#44795 = CARTESIAN_POINT ( 'NONE',  ( 33.29974487139158867, -27.71228299555229313, 4.000000000000000000 ) ) ;
#44796 = EDGE_CURVE ( 'NONE', #20040, #114456, #2992, .T. ) ;
#44797 = CARTESIAN_POINT ( 'NONE',  ( 34.45011844616453800, 16.51628081163733697, 5.000000000000001776 ) ) ;
#44798 = CARTESIAN_POINT ( 'NONE',  ( 24.48921356237309510, -27.52281430457072631, 5.000000000000000000 ) ) ;
#44799 = FACE_OUTER_BOUND ( 'NONE', #106982, .T. ) ;
#44800 = ORIENTED_EDGE ( 'NONE', *, *, #53652, .F. ) ;
#44801 = CARTESIAN_POINT ( 'NONE',  ( -34.42500000000001137, -22.22500000000000142, 5.000000000000000000 ) ) ;
#44802 = VECTOR ( 'NONE', #31610, 1000.000000000000000 ) ;
#44804 = VERTEX_POINT ( 'NONE', #26894 ) ;
#44803 = PRODUCT_DEFINITION_FORMATION_WITH_SPECIFIED_SOURCE ( 'ANY', '', #140743, .NOT_KNOWN. ) ;
#44805 = CARTESIAN_POINT ( 'NONE',  ( 27.98155265364313848, 18.75929247661553134, 20.33588619593436775 ) ) ;
#44806 = ORIENTED_EDGE ( 'NONE', *, *, #109008, .F. ) ;
#44807 = MECHANICAL_DESIGN_GEOMETRIC_PRESENTATION_REPRESENTATION (  '', ( #14645 ), #33207 ) ;
#44808 = CARTESIAN_POINT ( 'NONE',  ( 57.29974487139158157, -27.71228299555246011, 4.000000000000000000 ) ) ;
#44810 = ORIENTED_EDGE ( 'NONE', *, *, #19150, .T. ) ;
#44809 = DIRECTION ( 'NONE',  ( -1.000000000000000000, -0.000000000000000000, -0.000000000000000000 ) ) ;
#44811 = ADVANCED_FACE ( 'NONE', ( #82718 ), #104442, .F. ) ;
#44812 = CARTESIAN_POINT ( 'NONE',  ( 0.000000000000000000, 0.000000000000000000, 5.000000000000000000 ) ) ;
#44813 = DIRECTION ( 'NONE',  ( -0.6830127018922180770, -0.6830127018922204085, -0.2588190451025213501 ) ) ;
#44814 = ORIENTED_EDGE ( 'NONE', *, *, #26658, .T. ) ;
#44815 = CARTESIAN_POINT ( 'NONE',  ( 8.510786437626906675, -27.52281430457049183, 5.000000000000000000 ) ) ;
#44816 = ORIENTED_EDGE ( 'NONE', *, *, #2410, .F. ) ;
#44817 = CARTESIAN_POINT ( 'NONE',  ( 3.489213562373097322, -27.52281430457057709, 5.000000000000000000 ) ) ;
#44818 = UNCERTAINTY_MEASURE_WITH_UNIT (LENGTH_MEASURE( 1.000000000000000082E-05 ), #99293, 'distance_accuracy_value', 'NONE');
#44819 = ORIENTED_EDGE ( 'NONE', *, *, #70723, .T. ) ;
#44820 = DIRECTION ( 'NONE',  ( -0.000000000000000000, 0.000000000000000000, 1.000000000000000000 ) ) ;
#44821 = CARTESIAN_POINT ( 'NONE',  ( 113.9750270504628986, -5.819803920172572198, 5.819803920172572198 ) ) ;
#44822 = AXIS2_PLACEMENT_3D ( 'NONE', #105196, #114634, #49432 ) ;
#44823 = CARTESIAN_POINT ( 'NONE',  ( -14.70025512860841133, -27.71228299555195917, 4.000000000000000000 ) ) ;
#44824 = DIRECTION ( 'NONE',  ( 1.000000000000000000, 1.224606353822377258E-16, 0.000000000000000000 ) ) ;
#44825 = DIRECTION ( 'NONE',  ( -0.7071067811865487940, 0.7071067811865463515, -0.000000000000000000 ) ) ;
#44826 = FACE_OUTER_BOUND ( 'NONE', #123817, .T. ) ;
#44827 = CARTESIAN_POINT ( 'NONE',  ( 18.37500000000000355, -6.094999999999989981, 3.732111120401553285E-16 ) ) ;
#44828 = CARTESIAN_POINT ( 'NONE',  ( 22.14540314143522082, -2.126176841940958351, -7.934999999999988951 ) ) ;
#44829 = CARTESIAN_POINT ( 'NONE',  ( 24.79289321881328334, 12.75929247661559529, 5.000000000000000000 ) ) ;
#44830 = CARTESIAN_POINT ( 'NONE',  ( 39.48921356237310221, -27.52281430457082934, 5.000000000000000000 ) ) ;
#44831 = ORIENTED_EDGE ( 'NONE', *, *, #15657, .F. ) ;
#44832 = VECTOR ( 'NONE', #38127, 1000.000000000000227 ) ;
#44833 = ORIENTED_EDGE ( 'NONE', *, *, #123583, .F. ) ;
#44834 = CARTESIAN_POINT ( 'NONE',  ( 8.999999999999937828, -22.06887692260758982, 4.000000000000000000 ) ) ;
#44835 = ORIENTED_EDGE ( 'NONE', *, *, #39907, .T. ) ;
#44836 = VECTOR ( 'NONE', #136528, 1000.000000000000000 ) ;
#44837 = CARTESIAN_POINT ( 'NONE',  ( 104.2712635252314470, 4.472830434245839371, 4.472830434245842035 ) ) ;
#44838 = DIRECTION ( 'NONE',  ( 0.7071067811865486830, -0.7071067811865464625, -0.000000000000000000 ) ) ;
#44839 = CARTESIAN_POINT ( 'NONE',  ( 3.005480084712505828, 28.92564299267936079, 4.000000000000000000 ) ) ;
#44840 = FACE_OUTER_BOUND ( 'NONE', #69119, .T. ) ;
#44841 = CARTESIAN_POINT ( 'NONE',  ( 125.9798776214792468, -48.09441802426616164, -35.89947574910151928 ) ) ;
#44842 = ORIENTED_EDGE ( 'NONE', *, *, #25417, .T. ) ;
#44843 = DIRECTION ( 'NONE',  ( -0.7071067811865486830, -0.7071067811865464625, 0.000000000000000000 ) ) ;
#44844 = DIRECTION ( 'NONE',  ( 0.5735764363510453823, -0.8191520442889923537, 1.003171929053525486E-16 ) ) ;
#44846 = EDGE_CURVE ( 'NONE', #99762, #7658, #69722, .T. ) ;
#44845 = VECTOR ( 'NONE', #27232, 1000.000000000000000 ) ;
#44847 = DIRECTION ( 'NONE',  ( -0.7071067811865486830, -0.7071067811865464625, -0.000000000000000000 ) ) ;
#44848 = CARTESIAN_POINT ( 'NONE',  ( 14.42840764549667476, 9.139736423841732040E-16, 0.000000000000000000 ) ) ;
#44850 = ORIENTED_EDGE ( 'NONE', *, *, #125258, .T. ) ;
#44849 = DIRECTION ( 'NONE',  ( 0.3543493200069162685, -0.000000000000000000, -0.9351131265310288487 ) ) ;
#44851 = DIRECTION ( 'NONE',  ( 0.000000000000000000, 0.000000000000000000, 1.000000000000000000 ) ) ;
#44852 = DIRECTION ( 'NONE',  ( 8.673617379884034239E-17, -1.000000000000000000, 0.000000000000000000 ) ) ;
#44853 = LINE ( 'NONE', #86171, #72514 ) ;
#44854 = DIRECTION ( 'NONE',  ( -0.7071067811865486830, -0.7071067811865464625, 0.000000000000000000 ) ) ;
#44855 = CARTESIAN_POINT ( 'NONE',  ( 12.32816939922344446, 17.25929247661554200, 4.000000000000000000 ) ) ;
#44856 = VECTOR ( 'NONE', #135964, 999.9999999999998863 ) ;
#44857 = ORIENTED_EDGE ( 'NONE', *, *, #52381, .T. ) ;
#44858 = EDGE_LOOP ( 'NONE', ( #142668, #90678, #135366, #93276 ) ) ;
#44859 = ORIENTED_EDGE ( 'NONE', *, *, #62855, .F. ) ;
#44860 = ADVANCED_FACE ( 'NONE', ( #58875 ), #49404, .F. ) ;
#44861 = CARTESIAN_POINT ( 'NONE',  ( 92.60459685856478984, 1.637169565754164946, -6.109999999999999432 ) ) ;
#44862 = VECTOR ( 'NONE', #81671, 1000.000000000000000 ) ;
#44863 = ORIENTED_EDGE ( 'NONE', *, *, #56488, .F. ) ;
#44864 = ADVANCED_FACE ( 'NONE', ( #36357, #27595 ), #116026, .F. ) ;
#44865 = LINE ( 'NONE', #68044, #25431 ) ;
#44866 = CARTESIAN_POINT ( 'NONE',  ( -19.49999999999986500, 16.77039438581777375, 0.4657186855308182438 ) ) ;
#44867 = EDGE_CURVE ( 'NONE', #14544, #65084, #81302, .T. ) ;
#44868 = VECTOR ( 'NONE', #100615, 1000.000000000000000 ) ;
#44869 = DIRECTION ( 'NONE',  ( 0.000000000000000000, -1.000000000000000000, 0.000000000000000000 ) ) ;
#44870 = DIRECTION ( 'NONE',  ( -0.000000000000000000, 0.000000000000000000, 1.000000000000000000 ) ) ;
#44871 = VERTEX_POINT ( 'NONE', #26195 ) ;
#44872 = EDGE_CURVE ( 'NONE', #115828, #143429, #35831, .T. ) ;
#44873 = DIRECTION ( 'NONE',  ( -1.000000000000000000, -1.224606353822377258E-16, -0.000000000000000000 ) ) ;
#44874 = FACE_OUTER_BOUND ( 'NONE', #84428, .T. ) ;
#44875 =( BOUNDED_CURVE ( )  B_SPLINE_CURVE ( 3, ( #115085, #85332, #7027, #96202 ),
 .UNSPECIFIED., .F., .F. ) 
 B_SPLINE_CURVE_WITH_KNOTS ( ( 4, 4 ),
 ( 4.735358278776982566, 4.752060726170250327 ),
 .UNSPECIFIED. ) 
 CURVE ( )  GEOMETRIC_REPRESENTATION_ITEM ( )  RATIONAL_B_SPLINE_CURVE ( ( 1.000000000000000000, 0.9999767524893692361, 0.9999767524893692361, 1.000000000000000000 ) ) 
 REPRESENTATION_ITEM ( '' )  );
#44876 = CARTESIAN_POINT ( 'NONE',  ( 82.59959685856478018, -6.109999999999997655, -1.637169565754160283 ) ) ;
#44877 = VERTEX_POINT ( 'NONE', #103711 ) ;
#44878 = DIRECTION ( 'NONE',  ( -0.7071067811865487940, 0.7071067811865463515, -0.000000000000000000 ) ) ;
#44879 = VECTOR ( 'NONE', #48128, 1000.000000000000000 ) ;
#44880 = CARTESIAN_POINT ( 'NONE',  ( -30.18398860626900060, 28.73617430169808173, 5.000000000000000000 ) ) ;
#44881 = ORIENTED_EDGE ( 'NONE', *, *, #106769, .F. ) ;
#44882 = ORIENTED_EDGE ( 'NONE', *, *, #121511, .F. ) ;
#44883 = EDGE_CURVE ( 'NONE', #53957, #61426, #4357, .T. ) ;
#44884 = ORIENTED_EDGE ( 'NONE', *, *, #2526, .F. ) ;
#44885 = CYLINDRICAL_SURFACE ( 'NONE', #79359, 0.5000000000000004441 ) ;
#44886 = ADVANCED_FACE ( 'NONE', ( #121659 ), #1303, .T. ) ;
#44887 = LINE ( 'NONE', #67309, #66301 ) ;
#44888 = CARTESIAN_POINT ( 'NONE',  ( 23.98373647476855197, -5.808823158059035485, -5.808823158059033709 ) ) ;
#44889 = AXIS2_PLACEMENT_3D ( 'NONE', #116306, #61955, #3925 ) ;
#44890 = DIRECTION ( 'NONE',  ( 0.7071067811865486830, -0.7071067811865464625, -0.000000000000000000 ) ) ;
#44891 = CARTESIAN_POINT ( 'NONE',  ( 166.6278473451638149, 26.96999999999994557, 32.76352092273798178 ) ) ;
#44892 = EDGE_CURVE ( 'NONE', #76456, #119529, #89757, .T. ) ;
#44893 = LINE ( 'NONE', #79665, #107600 ) ;
#44894 = VECTOR ( 'NONE', #133853, 1000.000000000000000 ) ;
#44895 = ORIENTED_EDGE ( 'NONE', *, *, #76097, .T. ) ;
#44896 = ORIENTED_EDGE ( 'NONE', *, *, #21840, .T. ) ;
#44897 = DIRECTION ( 'NONE',  ( -0.000000000000000000, -0.3543493200069152693, 0.9351131265310292928 ) ) ;
#44898 = ORIENTED_EDGE ( 'NONE', *, *, #140939, .F. ) ;
#44899 = ORIENTED_EDGE ( 'NONE', *, *, #136303, .T. ) ;
#44900 = EDGE_CURVE ( 'NONE', #13236, #45628, #11457, .T. ) ;
#44901 = VECTOR ( 'NONE', #89086, 1000.000000000000000 ) ;
#44902 = DIRECTION ( 'NONE',  ( 1.000000000000000000, 0.000000000000000000, 0.000000000000000000 ) ) ;
#44903 = VERTEX_POINT ( 'NONE', #55729 ) ;
#44904 = LINE ( 'NONE', #112950, #110754 ) ;
#44905 = DIRECTION ( 'NONE',  ( -0.7071067811865486830, -0.7071067811865464625, 0.000000000000000000 ) ) ;
#44906 = CARTESIAN_POINT ( 'NONE',  ( 19.41999999999999815, -2.055000000000000160, 2.789133085058098087E-16 ) ) ;
#44907 = ADVANCED_FACE ( 'NONE', ( #100657 ), #35428, .F. ) ;
#44908 = CARTESIAN_POINT ( 'NONE',  ( 27.00000000000000355, 0.000000000000000000, 0.000000000000000000 ) ) ;
#44909 = CARTESIAN_POINT ( 'NONE',  ( 25.39999999999999858, -14.29000000000013593, 12.69999999999954632 ) ) ;
#44910 = ORIENTED_EDGE ( 'NONE', *, *, #22341, .F. ) ;
#44911 = VERTEX_POINT ( 'NONE', #102076 ) ;
#44912 = LINE ( 'NONE', #35450, #126714 ) ;
#44913 = ORIENTED_EDGE ( 'NONE', *, *, #50250, .T. ) ;
#44914 = DIRECTION ( 'NONE',  ( 1.000000000000000000, 0.000000000000000000, 0.000000000000000000 ) ) ;
#44915 = ORIENTED_EDGE ( 'NONE', *, *, #81553, .F. ) ;
#44916 = APPLICATION_CONTEXT ( 'automotive_design' ) ;
#44917 = LINE ( 'NONE', #89098, #103736 ) ;
#44918 = VERTEX_POINT ( 'NONE', #69468 ) ;
#44919 = ORIENTED_EDGE ( 'NONE', *, *, #73436, .F. ) ;
#44920 = VECTOR ( 'NONE', #49160, 1000.000000000000227 ) ;
#44921 = ORIENTED_EDGE ( 'NONE', *, *, #138664, .T. ) ;
#44922 = CARTESIAN_POINT ( 'NONE',  ( -9.183988606268997046, 28.73617430169793607, 5.000000000000000000 ) ) ;
#44923 = VECTOR ( 'NONE', #60122, 1000.000000000000000 ) ;
#44924 = DIRECTION ( 'NONE',  ( -0.7071067811865487940, 0.7071067811865463515, 0.000000000000000000 ) ) ;
#44925 = FACE_OUTER_BOUND ( 'NONE', #34064, .T. ) ;
#44926 = LINE ( 'NONE', #132634, #24255 ) ;
#44927 = EDGE_CURVE ( 'NONE', #28039, #46695, #99932, .T. ) ;
#44928 = CYLINDRICAL_SURFACE ( 'NONE', #64485, 0.5000000000000000000 ) ;
#44929 = CARTESIAN_POINT ( 'NONE',  ( 0.000000000000000000, -4.600000000000012079, -20.40202195861968093 ) ) ;
#44931 = LINE ( 'NONE', #142761, #67902 ) ;
#44930 = VECTOR ( 'NONE', #42959, 1000.000000000000000 ) ;
#44932 = DIRECTION ( 'NONE',  ( 0.7071067811865487940, 0.7071067811865463515, 0.000000000000000000 ) ) ;
#44933 = ORIENTED_EDGE ( 'NONE', *, *, #34944, .T. ) ;
#44934 = LINE ( 'NONE', #45625, #105901 ) ;
#44935 = VECTOR ( 'NONE', #132114, 1000.000000000000000 ) ;
#44936 = LINE ( 'NONE', #89118, #86573 ) ;
#44937 = ADVANCED_FACE ( 'NONE', ( #36121 ), #12899, .F. ) ;
#44938 = ORIENTED_EDGE ( 'NONE', *, *, #29487, .T. ) ;
#44939 = ORIENTED_EDGE ( 'NONE', *, *, #112637, .F. ) ;
#44940 = ORIENTED_EDGE ( 'NONE', *, *, #108598, .T. ) ;
#44941 = LINE ( 'NONE', #143470, #26394 ) ;
#44942 = ORIENTED_EDGE ( 'NONE', *, *, #125471, .T. ) ;
#44943 = VECTOR ( 'NONE', #50989, 1000.000000000000000 ) ;
#44944 = ORIENTED_EDGE ( 'NONE', *, *, #44316, .F. ) ;
#44945 = LINE ( 'NONE', #55066, #2760 ) ;
#44946 = CARTESIAN_POINT ( 'NONE',  ( 14.92080628287044064, 3.047499999999997655, 5.278424836066143655 ) ) ;
#44947 = AXIS2_PLACEMENT_3D ( 'NONE', #21179, #29196, #74883 ) ;
#44948 = EDGE_CURVE ( 'NONE', #85310, #11989, #91227, .T. ) ;
#44949 = CARTESIAN_POINT ( 'NONE',  ( 0.000000000000000000, 0.000000000000000000, 5.000000000000000000 ) ) ;
#44950 = DIRECTION ( 'NONE',  ( 0.6830127018922181881, 0.6830127018922202975, -0.2588190451025214056 ) ) ;
#44951 = ORIENTED_EDGE ( 'NONE', *, *, #141743, .F. ) ;
#44952 = DIRECTION ( 'NONE',  ( 0.6830127018922181881, 0.6830127018922202975, -0.2588190451025214056 ) ) ;
#44953 = ORIENTED_EDGE ( 'NONE', *, *, #24004, .T. ) ;
#44955 = VECTOR ( 'NONE', #111159, 1000.000000000000000 ) ;
#44954 = LINE ( 'NONE', #24565, #130243 ) ;
#44956 = VECTOR ( 'NONE', #81102, 1000.000000000000000 ) ;
#44957 = CARTESIAN_POINT ( 'NONE',  ( 22.81706980810188767, -2.126176841940956130, 7.934999999999991616 ) ) ;
#44958 = EDGE_LOOP ( 'NONE', ( #106723, #112483, #119406, #96657 ) ) ;
#44959 = CARTESIAN_POINT ( 'NONE',  ( 85.66209685856478018, -5.291415217122919401, 3.054999999999998384 ) ) ;
#44960 = CARTESIAN_POINT ( 'NONE',  ( 6.538661199317437500, -9.242530024995444293, 2.210267608354182123 ) ) ;
#44961 = CARTESIAN_POINT ( 'NONE',  ( -47.99451991528749062, 28.92564299267971251, 4.000000000000000000 ) ) ;
#44962 = ORIENTED_EDGE ( 'NONE', *, *, #46178, .F. ) ;
#44963 = ORIENTED_EDGE ( 'NONE', *, *, #64287, .F. ) ;
#44964 = EDGE_LOOP ( 'NONE', ( #116382, #25883, #119043, #40097 ) ) ;
#44965 = CARTESIAN_POINT ( 'NONE',  ( 28.00000000000002487, -49.14999999999999147, -59.92499999999979821 ) ) ;
#44967 = VECTOR ( 'NONE', #10512, 1000.000000000000000 ) ;
#44966 = CARTESIAN_POINT ( 'NONE',  ( -30.00000000000000355, 2.375000000000000000, 4.319999999999998508 ) ) ;
#44968 = FACE_OUTER_BOUND ( 'NONE', #89315, .T. ) ;
#44969 = DIRECTION ( 'NONE',  ( 0.7071067811865487940, 0.7071067811865463515, 0.000000000000000000 ) ) ;
#44970 = ORIENTED_EDGE ( 'NONE', *, *, #33220, .T. ) ;
#44971 = FILL_AREA_STYLE_COLOUR ( '', #142922 ) ;
#44972 = EDGE_CURVE ( 'NONE', #101635, #46980, #68069, .T. ) ;
#44973 = CARTESIAN_POINT ( 'NONE',  ( 69.29974487139159578, -27.71228299555254537, 4.000000000000000000 ) ) ;
#44974 = CARTESIAN_POINT ( 'NONE',  ( 1.499999999999994449, 6.052185695429108669, 5.000000000000000000 ) ) ;
#44975 = ORIENTED_EDGE ( 'NONE', *, *, #60587, .F. ) ;
#44976 = LINE ( 'NONE', #121746, #106792 ) ;
#44977 = AXIS2_PLACEMENT_3D ( 'NONE', #116932, #28521, #17601 ) ;
#44978 = LINE ( 'NONE', #22425, #141938 ) ;
#44979 = ORIENTED_EDGE ( 'NONE', *, *, #73352, .T. ) ;
#44980 = EDGE_CURVE ( 'NONE', #106369, #22146, #102963, .T. ) ;
#44982 = EDGE_LOOP ( 'NONE', ( #6926, #43602, #71208, #8886 ) ) ;
#44981 = CARTESIAN_POINT ( 'NONE',  ( -19.05000000000000071, 3.174999999999997158, 4.000000000000000000 ) ) ;
#44983 = ORIENTED_EDGE ( 'NONE', *, *, #36217, .T. ) ;
#44984 = EDGE_CURVE ( 'NONE', #34599, #130423, #44893, .T. ) ;
#44985 = CARTESIAN_POINT ( 'NONE',  ( 0.000000000000000000, -21.76999999999999247, -0.5000000000000000000 ) ) ;
#44986 = CARTESIAN_POINT ( 'NONE',  ( -34.00193056682073944, -22.22500000000000142, 4.500000000000000888 ) ) ;
#44987 = VERTEX_POINT ( 'NONE', #80346 ) ;
#44988 = CARTESIAN_POINT ( 'NONE',  ( -0.7228143045705931469, -21.72500000000000142, 5.000000000000000000 ) ) ;
#44989 = UNCERTAINTY_MEASURE_WITH_UNIT (LENGTH_MEASURE( 1.000000000000000082E-05 ), #81499, 'distance_accuracy_value', 'NONE');
#44990 = LINE ( 'NONE', #78289, #130900 ) ;
#44992 = AXIS2_PLACEMENT_3D ( 'NONE', #275, #133000, #112640 ) ;
#44991 = CARTESIAN_POINT ( 'NONE',  ( -14.70025512860841133, -27.71228299555195917, 4.000000000000000000 ) ) ;
#44993 = FACE_OUTER_BOUND ( 'NONE', #33372, .T. ) ;
#44994 = PLANE ( 'NONE',  #74418 ) ;
#44995 = DIRECTION ( 'NONE',  ( 0.7071067811865487940, 0.7071067811865463515, 0.000000000000000000 ) ) ;
#44996 = CARTESIAN_POINT ( 'NONE',  ( 33.18398860626899705, 28.73617430169810305, 5.000000000000000000 ) ) ;
#44997 = CARTESIAN_POINT ( 'NONE',  ( 57.48921356237308800, -27.52281430457095368, 5.000000000000000000 ) ) ;
#44998 = CARTESIAN_POINT ( 'NONE',  ( 23.74956980810188867, 3.967499999999998916, 6.871911579029510442 ) ) ;
#44999 = DIRECTION ( 'NONE',  ( -0.000000000000000000, 0.3543493200069153248, 0.9351131265310292928 ) ) ;
#45000 = DIRECTION ( 'NONE',  ( 0.7071067811865487940, 0.7071067811865463515, -0.000000000000000000 ) ) ;
#45001 = CARTESIAN_POINT ( 'NONE',  ( 109.9375000000000000, 5.819803920172574863, -5.819803920172573086 ) ) ;
#45002 = ORIENTED_EDGE ( 'NONE', *, *, #31238, .T. ) ;
#45003 = ADVANCED_FACE ( 'NONE', ( #24500 ), #133991, .F. ) ;
#45004 = CIRCLE ( 'NONE', #123723, 2.500000000000000444 ) ;
#45005 = EDGE_LOOP ( 'NONE', ( #136173, #83300, #108995, #91716 ) ) ;
#45006 = CARTESIAN_POINT ( 'NONE',  ( 99.00000000000000000, 0.000000000000000000, -7.950000000000000178 ) ) ;
#45007 = ORIENTED_EDGE ( 'NONE', *, *, #8124, .T. ) ;
#45008 = ORIENTED_EDGE ( 'NONE', *, *, #41640, .F. ) ;
#45009 = ORIENTED_EDGE ( 'NONE', *, *, #49665, .T. ) ;
#45010 = DIRECTION ( 'NONE',  ( -0.000000000000000000, -0.3543493200069152693, 0.9351131265310292928 ) ) ;
#45011 = CARTESIAN_POINT ( 'NONE',  ( -14.68370490163491482, -22.22500000000000142, -2.670183372115248588 ) ) ;
#45012 = ORIENTED_EDGE ( 'NONE', *, *, #131479, .T. ) ;
#45013 = DIRECTION ( 'NONE',  ( 0.6830127018922180770, -0.6830127018922204085, -0.2588190451025213501 ) ) ;
#45014 = DIRECTION ( 'NONE',  ( -1.000000000000000000, -1.224606353822377258E-16, -0.000000000000000000 ) ) ;
#45015 = CARTESIAN_POINT ( 'NONE',  ( -24.70710678118636494, -15.74070752338412049, 5.000000000000000000 ) ) ;
#45016 = PLANE ( 'NONE',  #76742 ) ;
#45017 = ORIENTED_EDGE ( 'NONE', *, *, #104661, .F. ) ;
#45018 = CARTESIAN_POINT ( 'NONE',  ( 18.18398860626898994, 28.73617430169800002, 5.000000000000000000 ) ) ;
#45019 = DIRECTION ( 'NONE',  ( -1.000000000000000000, -1.224606353822377258E-16, -0.000000000000000000 ) ) ;
#45020 = AXIS2_PLACEMENT_3D ( 'NONE', #59856, #49713, #81627 ) ;
#45021 = CARTESIAN_POINT ( 'NONE',  ( -31.17183060077624646, -2.240707523384260824, 4.000000000000000000 ) ) ;
#45022 = CARTESIAN_POINT ( 'NONE',  ( 24.06249999999999645, 4.461849672132300881, 4.461849672132299105 ) ) ;
#45023 = CARTESIAN_POINT ( 'NONE',  ( 75.18398860626899705, 28.73617430169839793, 5.000000000000000000 ) ) ;
#45024 = DIRECTION ( 'NONE',  ( 0.6830127018922180770, -0.6830127018922204085, -0.2588190451025213501 ) ) ;
#45025 = CARTESIAN_POINT ( 'NONE',  ( 0.000000000000000000, 0.000000000000000000, 5.000000000000000000 ) ) ;
#45026 = CONICAL_SURFACE ( 'NONE', #135243, 1.898649999999993065, 1.029744258676648316 ) ;
#45027 = ORIENTED_EDGE ( 'NONE', *, *, #136802, .T. ) ;
#45028 = VERTEX_POINT ( 'NONE', #57176 ) ;
#45029 = EDGE_CURVE ( 'NONE', #89614, #2635, #595, .T. ) ;
#45030 = CARTESIAN_POINT ( 'NONE',  ( 119.4379301918981042, -6.110000000000001208, 1.637169565754158951 ) ) ;
#45031 = ORIENTED_EDGE ( 'NONE', *, *, #9256, .T. ) ;
#45032 = EDGE_CURVE ( 'NONE', #125583, #66944, #102801, .T. ) ;
#45033 = VECTOR ( 'NONE', #104850, 1000.000000000000000 ) ;
#45034 = CARTESIAN_POINT ( 'NONE',  ( -12.69999999999998153, 0.000000000000000000, 2.500000000000000444 ) ) ;
#45035 = CARTESIAN_POINT ( 'NONE',  ( -56.99451991528749062, 28.92564299267978001, 4.000000000000000000 ) ) ;
#45036 = ADVANCED_FACE ( 'NONE', ( #132597 ), #133294, .F. ) ;
#45037 = EDGE_CURVE ( 'NONE', #119359, #138000, #56478, .T. ) ;
#45038 = CARTESIAN_POINT ( 'NONE',  ( 51.18398860626899705, 28.73617430169823095, 5.000000000000000000 ) ) ;
#45039 = CARTESIAN_POINT ( 'NONE',  ( 113.8079301918981230, -6.109999999999998543, 1.637169565754158063 ) ) ;
#45040 = VECTOR ( 'NONE', #52055, 1000.000000000000000 ) ;
#45041 = VERTEX_POINT ( 'NONE', #123132 ) ;
#45042 = ORIENTED_EDGE ( 'NONE', *, *, #135533, .T. ) ;
#45043 = LINE ( 'NONE', #122538, #76280 ) ;
#45044 = FACE_OUTER_BOUND ( 'NONE', #72603, .T. ) ;
#45045 = VERTEX_POINT ( 'NONE', #23802 ) ;
#45046 = VERTEX_POINT ( 'NONE', #27217 ) ;
#45048 = EDGE_CURVE ( 'NONE', #135923, #65251, #51141, .T. ) ;
#45047 = CARTESIAN_POINT ( 'NONE',  ( 38.93793019189809002, -6.110000000000001208, 1.637169565754158951 ) ) ;
#45049 = VECTOR ( 'NONE', #129050, 999.9999999999998863 ) ;
#45050 = EDGE_LOOP ( 'NONE', ( #117875, #41207, #41244, #66066 ) ) ;
#45051 = DIRECTION ( 'NONE',  ( -0.7071067811865486830, 0.7071067811865463515, 0.000000000000000000 ) ) ;
#45052 = ADVANCED_FACE ( 'NONE', ( #104789 ), #82348, .F. ) ;
#45053 = CARTESIAN_POINT ( 'NONE',  ( 45.18398860626900415, 28.73617430169818832, 5.000000000000000000 ) ) ;
#45054 = DIRECTION ( 'NONE',  ( -0.7071067811865487940, 0.7071067811865463515, -0.000000000000000000 ) ) ;
#45055 = CIRCLE ( 'NONE', #142297, 0.5000000000000000000 ) ;
#45056 = EDGE_CURVE ( 'NONE', #65959, #99234, #126143, .T. ) ;
#45057 = AXIS2_PLACEMENT_3D ( 'NONE', #20625, #49906, #88046 ) ;
#45058 = VECTOR ( 'NONE', #10825, 999.9999999999998863 ) ;
#45059 = CARTESIAN_POINT ( 'NONE',  ( 29.07876352523144803, -7.482591942790325086E-16, 6.109999999999998543 ) ) ;
#45060 = ORIENTED_EDGE ( 'NONE', *, *, #26247, .F. ) ;
#45061 = CARTESIAN_POINT ( 'NONE',  ( -57.48921356237308800, -27.52281430457095368, 5.000000000000000000 ) ) ;
#45062 = VERTEX_POINT ( 'NONE', #49000 ) ;
#45063 = ORIENTED_EDGE ( 'NONE', *, *, #141195, .T. ) ;
#45064 = EDGE_CURVE ( 'NONE', #31209, #8801, #128000, .T. ) ;
#45065 = ORIENTED_EDGE ( 'NONE', *, *, #79162, .T. ) ;
#45066 = CARTESIAN_POINT ( 'NONE',  ( 20.99999999999985789, -12.41253812416062807, 4.000000000000000000 ) ) ;
#45067 = ORIENTED_EDGE ( 'NONE', *, *, #72997, .F. ) ;
#45068 = CARTESIAN_POINT ( 'NONE',  ( 0.000000000000000000, 0.000000000000000000, 5.000000000000000000 ) ) ;
#45069 = CARTESIAN_POINT ( 'NONE',  ( -9.758600742197899081, 21.72500000000000853, 5.000000000000000000 ) ) ;
#45070 = ADVANCED_FACE ( 'NONE', ( #106185 ), #83790, .F. ) ;
#45071 = CARTESIAN_POINT ( 'NONE',  ( -26.99999999999980815, 4.931123077392133069, 4.000000000000000000 ) ) ;
#45072 = FACE_BOUND ( 'NONE', #1492, .T. ) ;
#45073 = ORIENTED_EDGE ( 'NONE', *, *, #21725, .F. ) ;
#45074 = FACE_OUTER_BOUND ( 'NONE', #89963, .T. ) ;
#45075 = CARTESIAN_POINT ( 'NONE',  ( 2.999999999999992450, 17.96639925780208102, 5.000000000000000000 ) ) ;
#45076 = DIRECTION ( 'NONE',  ( -0.3543493200069162685, -0.000000000000000000, -0.9351131265310288487 ) ) ;
#45077 = CARTESIAN_POINT ( 'NONE',  ( -15.18398860626900237, 28.73617430169797871, 5.000000000000000000 ) ) ;
#45078 = EDGE_LOOP ( 'NONE', ( #56597, #52914, #38067, #117099 ) ) ;
#45079 = EDGE_CURVE ( 'NONE', #142885, #141807, #6863, .T. ) ;
#45080 = CARTESIAN_POINT ( 'NONE',  ( -31.49999999999977973, -8.947814304570734123, 5.000000000000000000 ) ) ;
#45081 = VERTEX_POINT ( 'NONE', #95335 ) ;
#45082 = EDGE_CURVE ( 'NONE', #113229, #95696, #94611, .T. ) ;
#45083 = ORIENTED_EDGE ( 'NONE', *, *, #82314, .F. ) ;
#45084 = VERTEX_POINT ( 'NONE', #40285 ) ;
#45085 = ADVANCED_FACE ( 'NONE', ( #72215 ), #29359, .T. ) ;
#45086 = CARTESIAN_POINT ( 'NONE',  ( 43.22459685856478728, -1.637169565754160949, 6.109999999999997655 ) ) ;
#45087 = ORIENTED_EDGE ( 'NONE', *, *, #31343, .T. ) ;
#45088 = CARTESIAN_POINT ( 'NONE',  ( -27.48921356237309155, -27.52281430457074762, 5.000000000000000000 ) ) ;
#45089 = PLANE ( 'NONE',  #35782 ) ;
#45090 = FACE_OUTER_BOUND ( 'NONE', #26738, .T. ) ;
#45091 = ORIENTED_EDGE ( 'NONE', *, *, #20549, .T. ) ;
#45092 = LINE ( 'NONE', #133492, #23684 ) ;
#45093 = CARTESIAN_POINT ( 'NONE',  ( -24.29974487139158867, -27.71228299555223273, 4.000000000000000000 ) ) ;
#45094 = VECTOR ( 'NONE', #60219, 1000.000000000000227 ) ;
#45095 = FACE_OUTER_BOUND ( 'NONE', #20084, .T. ) ;
#45096 = CARTESIAN_POINT ( 'NONE',  ( 3.398789304146613954, 4.202752102959690472E-16, 0.000000000000000000 ) ) ;
#45097 = DIRECTION ( 'NONE',  ( 0.6830127018922180770, -0.6830127018922204085, -0.2588190451025213501 ) ) ;
#45098 = FACE_OUTER_BOUND ( 'NONE', #32750, .T. ) ;
#45099 = DIRECTION ( 'NONE',  ( -1.000000000000000000, -1.224606353822377258E-16, -0.000000000000000000 ) ) ;
#45100 = ORIENTED_EDGE ( 'NONE', *, *, #123572, .T. ) ;
#45101 = ORIENTED_EDGE ( 'NONE', *, *, #93098, .T. ) ;
#45102 = VERTEX_POINT ( 'NONE', #72927 ) ;
#45103 = ORIENTED_EDGE ( 'NONE', *, *, #67773, .T. ) ;
#45104 = PLANE ( 'NONE',  #112139 ) ;
#45105 = DIRECTION ( 'NONE',  ( 0.6830127018922181881, 0.6830127018922202975, -0.2588190451025214056 ) ) ;
#45106 = ORIENTED_EDGE ( 'NONE', *, *, #30038, .T. ) ;
#45107 = ORIENTED_EDGE ( 'NONE', *, *, #86562, .T. ) ;
#45108 = CARTESIAN_POINT ( 'NONE',  ( -29.99999999999979039, 19.55218569542897100, 5.000000000000000000 ) ) ;
#45109 = CARTESIAN_POINT ( 'NONE',  ( 3.710381658649933634, 4.584330080086930965E-16, 0.000000000000000000 ) ) ;
#45110 = VERTEX_POINT ( 'NONE', #59872 ) ;
#45111 = CARTESIAN_POINT ( 'NONE',  ( 27.99999999999999645, -49.14999999999999147, -45.92499999999969873 ) ) ;
#45112 = LINE ( 'NONE', #34202, #39812 ) ;
#45113 = VECTOR ( 'NONE', #103093, 1000.000000000000227 ) ;
#45114 = CARTESIAN_POINT ( 'NONE',  ( 31.71290314143522693, 3.967499999999992699, -6.871911579029513994 ) ) ;
#45115 = FACE_OUTER_BOUND ( 'NONE', #123447, .T. ) ;
#45116 = ORIENTED_EDGE ( 'NONE', *, *, #66223, .T. ) ;
#45117 = CARTESIAN_POINT ( 'NONE',  ( 112.3495968585647802, 6.109999999999997655, 1.637169565754163836 ) ) ;
#45118 = VECTOR ( 'NONE', #106074, 1000.000000000000000 ) ;
#45119 = PLANE ( 'NONE',  #46685 ) ;
#45120 = PLANE ( 'NONE',  #85825 ) ;
#45121 = ADVANCED_FACE ( 'NONE', ( #39561 ), #105486, .F. ) ;
#45122 = LINE ( 'NONE', #98726, #137524 ) ;
#45124 = VERTEX_POINT ( 'NONE', #138867 ) ;
#45123 = LINE ( 'NONE', #91453, #68106 ) ;
#45125 = CARTESIAN_POINT ( 'NONE',  ( 11.99999999999992006, -0.2811185226894198363, -5.995736974527541285 ) ) ;
#45126 = ORIENTED_EDGE ( 'NONE', *, *, #57976, .F. ) ;
#45127 = PRESENTATION_STYLE_ASSIGNMENT (( #78435 ) ) ;
#45128 = CARTESIAN_POINT ( 'NONE',  ( -33.18398860626899705, 28.73617430169810305, 5.000000000000000000 ) ) ;
#45129 = CARTESIAN_POINT ( 'NONE',  ( 120.2916666666666714, 3.975000000000003642, -6.884901960086285300 ) ) ;
#45130 = ORIENTED_EDGE ( 'NONE', *, *, #50669, .T. ) ;
#45131 = DIRECTION ( 'NONE',  ( -0.7071067811865486830, -0.7071067811865464625, 0.000000000000000000 ) ) ;
#45132 =( GEOMETRIC_REPRESENTATION_CONTEXT ( 3 ) GLOBAL_UNCERTAINTY_ASSIGNED_CONTEXT ( ( #37291 ) ) GLOBAL_UNIT_ASSIGNED_CONTEXT ( ( #132329, #58898, #20661 ) ) REPRESENTATION_CONTEXT ( 'NONE', 'WORKASPACE' ) );
#45133 = LINE ( 'NONE', #132118, #106608 ) ;
#45134 = CARTESIAN_POINT ( 'NONE',  ( 16.49999999999989697, 16.08746187583907528, 4.000000000000000000 ) ) ;
#45135 = EDGE_LOOP ( 'NONE', ( #112926, #120526, #50655, #2142 ) ) ;
#45136 = LINE ( 'NONE', #130704, #56284 ) ;
#45137 = ORIENTED_EDGE ( 'NONE', *, *, #102350, .T. ) ;
#45138 = FACE_OUTER_BOUND ( 'NONE', #109800, .T. ) ;
#45139 = EDGE_CURVE ( 'NONE', #123479, #83438, #79886, .T. ) ;
#45141 = EDGE_LOOP ( 'NONE', ( #108603, #135497, #37567 ) ) ;
#45140 = CARTESIAN_POINT ( 'NONE',  ( -34.92500000000001137, 22.22500000000000142, 4.000000000000000000 ) ) ;
#45143 = ORIENTED_EDGE ( 'NONE', *, *, #57914, .T. ) ;
#45142 = EDGE_CURVE ( 'NONE', #59938, #109867, #17755, .T. ) ;
#45144 = CARTESIAN_POINT ( 'NONE',  ( 18.46695620621371248, 3.075185539296316328, -30.04948271178109920 ) ) ;
#45145 = DIRECTION ( 'NONE',  ( -0.000000000000000000, -0.3543493200069152693, 0.9351131265310292928 ) ) ;
#45146 = ORIENTED_EDGE ( 'NONE', *, *, #119112, .F. ) ;
#45147 = AXIS2_PLACEMENT_3D ( 'NONE', #88072, #35142, #44611 ) ;
#45148 = LINE ( 'NONE', #122652, #73778 ) ;
#45149 = VECTOR ( 'NONE', #54891, 1000.000000000000227 ) ;
#45150 = SURFACE_STYLE_USAGE ( .BOTH. , #102367 ) ;
#45151 = DIRECTION ( 'NONE',  ( 0.3543493200069162685, -0.000000000000000000, -0.9351131265310288487 ) ) ;
#45152 = VERTEX_POINT ( 'NONE', #48266 ) ;
#45153 = ADVANCED_FACE ( 'NONE', ( #93198 ), #92465, .F. ) ;
#45154 = CARTESIAN_POINT ( 'NONE',  ( 20.65000000000000213, 0.000000000000000000, 9.500000000000000000 ) ) ;
#45155 = DIRECTION ( 'NONE',  ( -1.000000000000000000, 0.000000000000000000, 0.000000000000000000 ) ) ;
#45156 = LINE ( 'NONE', #123418, #137297 ) ;
#45157 = CARTESIAN_POINT ( 'NONE',  ( 0.000000000000000000, 0.000000000000000000, 5.000000000000000000 ) ) ;
#45158 = CARTESIAN_POINT ( 'NONE',  ( 31.99543019189811233, 5.291415217122917625, 3.055000000000002380 ) ) ;
#45159 = DIRECTION ( 'NONE',  ( -0.6830127018922180770, -0.6830127018922204085, -0.2588190451025213501 ) ) ;
#45160 = EDGE_CURVE ( 'NONE', #97544, #60323, #15592, .T. ) ;
#45161 = ORIENTED_EDGE ( 'NONE', *, *, #105669, .T. ) ;
#45162 = VERTEX_POINT ( 'NONE', #5450 ) ;
#45163 = CARTESIAN_POINT ( 'NONE',  ( 124.9583333333333428, 3.974999999999997424, 6.884901960086288852 ) ) ;
#45164 = ORIENTED_EDGE ( 'NONE', *, *, #66902, .T. ) ;
#45165 = ORIENTED_EDGE ( 'NONE', *, *, #95420, .F. ) ;
#45166 = CARTESIAN_POINT ( 'NONE',  ( 1.392138667788030526, -2.420047799299299474, -6.258046653434560014 ) ) ;
#45167 = CARTESIAN_POINT ( 'NONE',  ( 24.42327845806339326, 11.25929247661560950, 17.85071094206578834 ) ) ;
#45168 = EDGE_CURVE ( 'NONE', #118671, #25909, #49732, .T. ) ;
#45169 = EDGE_LOOP ( 'NONE', ( #10730, #120333, #70263 ) ) ;
#45170 = DIRECTION ( 'NONE',  ( 0.7071067811865487940, 0.7071067811865463515, 0.000000000000000000 ) ) ;
#45171 = DIRECTION ( 'NONE',  ( 0.6830127018922181881, 0.6830127018922202975, -0.2588190451025214056 ) ) ;
#45172 = CARTESIAN_POINT ( 'NONE',  ( 48.48921356237309510, -27.52281430457089328, 5.000000000000000000 ) ) ;
#45173 = CARTESIAN_POINT ( 'NONE',  ( 25.19159235450331735, 9.902892378096218942E-16, 0.000000000000000000 ) ) ;
#45174 = CARTESIAN_POINT ( 'NONE',  ( 121.7712635252314328, 4.472830434245839371, 4.472830434245842035 ) ) ;
#45175 = ORIENTED_EDGE ( 'NONE', *, *, #65517, .T. ) ;
#45176 = CARTESIAN_POINT ( 'NONE',  ( 23.59118151920504047, -0.6989376001503817548, 4.102600482792097658 ) ) ;
#45177 = LINE ( 'NONE', #133586, #12147 ) ;
#45178 = EDGE_CURVE ( 'NONE', #132084, #48450, #93908, .T. ) ;
#45179 = CARTESIAN_POINT ( 'NONE',  ( 78.58333333333334281, 6.884901960086290629, -3.974999999999994316 ) ) ;
#45180 = LINE ( 'NONE', #124126, #20134 ) ;
#45181 = CARTESIAN_POINT ( 'NONE',  ( 13.82816939922343380, -17.24070752338410628, 4.000000000000000000 ) ) ;
#45182 = PLANE ( 'NONE',  #517 ) ;
#45183 = CARTESIAN_POINT ( 'NONE',  ( 3.710381658649933634, 4.584330080086930965E-16, 0.000000000000000000 ) ) ;
#45184 = CARTESIAN_POINT ( 'NONE',  ( 45.72502705046288440, 5.819803920172573086, -5.819803920172572198 ) ) ;
#45185 = CARTESIAN_POINT ( 'NONE',  ( 10.46799328145038821, 2.055000000000001048, 0.000000000000000000 ) ) ;
#45186 = DIRECTION ( 'NONE',  ( 0.7071067811865487940, 0.7071067811865463515, -0.000000000000000000 ) ) ;
#45187 = EDGE_LOOP ( 'NONE', ( #115162, #109233, #34118, #40256, #90721 ) ) ;
#45188 = VERTEX_POINT ( 'NONE', #141719 ) ;
#45189 = CARTESIAN_POINT ( 'NONE',  ( 44.31249999999999289, 5.819803920172571310, 5.819803920172575751 ) ) ;
#45190 = LINE ( 'NONE', #34278, #23142 ) ;
#45191 = ADVANCED_FACE ( 'NONE', ( #129385 ), #64158, .F. ) ;
#45192 = DIRECTION ( 'NONE',  ( -0.7071067811865487940, 0.7071067811865463515, -0.000000000000000000 ) ) ;
#45193 = ORIENTED_EDGE ( 'NONE', *, *, #13700, .T. ) ;
#45194 = CARTESIAN_POINT ( 'NONE',  ( -1.153248962236076647, -0.6664845763655985467, 3.830776090634477882 ) ) ;
#45196 = ADVANCED_FACE ( 'NONE', ( #75749 ), #140283, .F. ) ;
#45195 = FACE_OUTER_BOUND ( 'NONE', #55406, .T. ) ;
#45197 = EDGE_CURVE ( 'NONE', #20616, #32716, #53251, .T. ) ;
#45198 = CARTESIAN_POINT ( 'NONE',  ( 38.79209685856477563, -5.291415217122921177, 3.054999999999999272 ) ) ;
#45199 = EDGE_LOOP ( 'NONE', ( #73053, #98214, #59926, #28155 ) ) ;
#45200 = PRESENTATION_STYLE_ASSIGNMENT (( #100261 ) ) ;
#45201 = ORIENTED_EDGE ( 'NONE', *, *, #70594, .F. ) ;
#45202 = ORIENTED_EDGE ( 'NONE', *, *, #96029, .F. ) ;
#45203 = DIRECTION ( 'NONE',  ( -1.000000000000000000, -0.000000000000000000, -0.000000000000000000 ) ) ;
#45204 = EDGE_CURVE ( 'NONE', #49135, #115415, #85891, .T. ) ;
#45205 = LINE ( 'NONE', #25544, #26879 ) ;
#45206 = PLANE ( 'NONE',  #42101 ) ;
#45207 = LINE ( 'NONE', #133616, #48741 ) ;
#45208 = ORIENTED_EDGE ( 'NONE', *, *, #114345, .T. ) ;
#45209 = EDGE_CURVE ( 'NONE', #94410, #102769, #108318, .T. ) ;
#45210 = CARTESIAN_POINT ( 'NONE',  ( -11.96912906347995964, 22.22500000000000142, 13.69883763336573956 ) ) ;
#45211 = EDGE_LOOP ( 'NONE', ( #34619, #17767, #16126, #94499 ) ) ;
#45212 = DIRECTION ( 'NONE',  ( -0.3543493200069162685, -0.000000000000000000, -0.9351131265310288487 ) ) ;
#45213 = ADVANCED_FACE ( 'NONE', ( #86634 ), #132293, .F. ) ;
#45214 = CARTESIAN_POINT ( 'NONE',  ( 34.92499999999998295, -13.27521306008087265, -8.452357796116183764 ) ) ;
#45215 = CARTESIAN_POINT ( 'NONE',  ( 21.70710678118638270, -18.74070752338409562, 5.000000000000000000 ) ) ;
#45216 = DIRECTION ( 'NONE',  ( 0.7071067811865487940, 0.7071067811865463515, 0.000000000000000000 ) ) ;
#45217 = DIRECTION ( 'NONE',  ( -0.7071067811865487940, 0.7071067811865463515, -0.000000000000000000 ) ) ;
#45218 = CARTESIAN_POINT ( 'NONE',  ( 24.39999999999999858, -1.600000000000055600, -28.92500000000001492 ) ) ;
#45219 = AXIS2_PLACEMENT_3D ( 'NONE', #19305, #104881, #5549 ) ;
#45220 = EDGE_LOOP ( 'NONE', ( #39815, #50237, #26015, #74769 ) ) ;
#45221 = EDGE_CURVE ( 'NONE', #111354, #41615, #21356, .T. ) ;
#45222 = DIRECTION ( 'NONE',  ( 0.7071067811865486830, -0.7071067811865464625, -0.000000000000000000 ) ) ;
#45223 = CARTESIAN_POINT ( 'NONE',  ( 56.20376352523144448, 6.109999999999998543, 1.122388791418548911E-15 ) ) ;
#45224 = MECHANICAL_DESIGN_GEOMETRIC_PRESENTATION_REPRESENTATION (  '', ( #96072 ), #135442 ) ;
#45225 = DIRECTION ( 'NONE',  ( -1.000000000000000000, -1.224606353822377258E-16, -0.000000000000000000 ) ) ;
#45226 = CARTESIAN_POINT ( 'NONE',  ( -36.12147316337124892, -20.24070752338407786, 7.412974875817872622 ) ) ;
#45227 = CARTESIAN_POINT ( 'NONE',  ( 3.707106781186518152, -0.7407075233842788098, 5.000000000000000000 ) ) ;
#45228 = ORIENTED_EDGE ( 'NONE', *, *, #22518, .T. ) ;
#45229 = FACE_OUTER_BOUND ( 'NONE', #71596, .T. ) ;
#45230 = ADVANCED_FACE ( 'NONE', ( #30074 ), #96107, .T. ) ;
#45231 = VERTEX_POINT ( 'NONE', #98896 ) ;
#45232 = VECTOR ( 'NONE', #40664, 1000.000000000000000 ) ;
#45233 = LINE ( 'NONE', #133639, #79298 ) ;
#45234 = EDGE_LOOP ( 'NONE', ( #104902, #20270, #130324, #92052 ) ) ;
#45235 = CARTESIAN_POINT ( 'NONE',  ( 36.18398860626899705, 28.73617430169812437, 5.000000000000000000 ) ) ;
#45236 = CARTESIAN_POINT ( 'NONE',  ( -1.499999999999990896, 6.277155672890267546, -3.510561720658938345 ) ) ;
#45237 = DIRECTION ( 'NONE',  ( -0.7071067811865486830, 0.7071067811865464625, 0.000000000000000000 ) ) ;
#45238 = FACE_BOUND ( 'NONE', #62926, .T. ) ;
#45239 = LINE ( 'NONE', #88728, #34120 ) ;
#45240 = CARTESIAN_POINT ( 'NONE',  ( -1.828169399223509517, -8.240707523384196875, 4.000000000000000000 ) ) ;
#45241 = CARTESIAN_POINT ( 'NONE',  ( -6.005480084712508493, 28.92564299267933947, 4.000000000000000000 ) ) ;
#45242 = CARTESIAN_POINT ( 'NONE',  ( -6.489213562373093325, -27.52281430457059841, 5.000000000000000000 ) ) ;
#45244 = ORIENTED_EDGE ( 'NONE', *, *, #1344, .T. ) ;
#45243 = LINE ( 'NONE', #13974, #71287 ) ;
#45245 = LINE ( 'NONE', #2375, #37043 ) ;
#45246 = AXIS2_PLACEMENT_3D ( 'NONE', #93473, #72479, #5715 ) ;
#45247 = EDGE_LOOP ( 'NONE', ( #70137, #140532, #25537, #51567 ) ) ;
#45248 = EDGE_CURVE ( 'NONE', #142234, #13538, #24310, .T. ) ;
#45250 = ADVANCED_FACE ( 'NONE', ( #63471 ), #8989, .F. ) ;
#45249 = AXIS2_PLACEMENT_3D ( 'NONE', #52548, #65620, #54716 ) ;
#45252 = ORIENTED_EDGE ( 'NONE', *, *, #71492, .F. ) ;
#45251 = VECTOR ( 'NONE', #7129, 1000.000000000000000 ) ;
#45253 = CARTESIAN_POINT ( 'NONE',  ( 74.72459685856478018, -1.637169565754160949, 6.109999999999997655 ) ) ;
#45254 = ORIENTED_EDGE ( 'NONE', *, *, #12537, .F. ) ;
#45255 = LINE ( 'NONE', #55392, #140218 ) ;
#45256 = AXIS2_PLACEMENT_3D ( 'NONE', #62197, #128172, #17247 ) ;
#45257 = LINE ( 'NONE', #91578, #31 ) ;
#45258 = AXIS2_PLACEMENT_3D ( 'NONE', #18739, #93475, #28223 ) ;
#45259 = VERTEX_POINT ( 'NONE', #118513 ) ;
#45260 = DIRECTION ( 'NONE',  ( 0.7071067811865486830, -0.7071067811865464625, -0.000000000000000000 ) ) ;
#45261 = CARTESIAN_POINT ( 'NONE',  ( 34.92499999999998295, -15.18334561358938650, 4.500000000000000888 ) ) ;
#45262 = LINE ( 'NONE', #89432, #27562 ) ;
#45263 = CARTESIAN_POINT ( 'NONE',  ( -24.55388970886357569, 5.485012786255876627, 4.000000000000000000 ) ) ;
#45264 = FACE_OUTER_BOUND ( 'NONE', #122544, .T. ) ;
#45266 = DIRECTION ( 'NONE',  ( 1.000000000000000000, 0.000000000000000000, 0.000000000000000000 ) ) ;
#45265 = FACE_OUTER_BOUND ( 'NONE', #124709, .T. ) ;
#45267 = FACE_OUTER_BOUND ( 'NONE', #143342, .T. ) ;
#45268 = LINE ( 'NONE', #13282, #2185 ) ;
#45269 = ORIENTED_EDGE ( 'NONE', *, *, #75218, .F. ) ;
#45270 = ORIENTED_EDGE ( 'NONE', *, *, #134671, .T. ) ;
#45271 = CARTESIAN_POINT ( 'NONE',  ( 0.005480084712502889671, 28.92564299267938210, 4.000000000000000000 ) ) ;
#45272 =( NAMED_UNIT ( * ) SI_UNIT ( $, .STERADIAN. ) SOLID_ANGLE_UNIT ( ) );
#45273 = ORIENTED_EDGE ( 'NONE', *, *, #93574, .F. ) ;
#45274 = VERTEX_POINT ( 'NONE', #32980 ) ;
#45275 = ORIENTED_EDGE ( 'NONE', *, *, #79206, .F. ) ;
#45276 = CARTESIAN_POINT ( 'NONE',  ( 25.37543019189810067, -5.291415217122920289, -3.055000000000001492 ) ) ;
#45277 = ORIENTED_EDGE ( 'NONE', *, *, #124002, .T. ) ;
#45278 = CARTESIAN_POINT ( 'NONE',  ( -4.954842266633313841, -21.74070752338406720, 21.72585301388583545 ) ) ;
#45279 = CARTESIAN_POINT ( 'NONE',  ( -8.994519915287490619, 28.92564299267944250, 4.000000000000000000 ) ) ;
#45280 = CARTESIAN_POINT ( 'NONE',  ( 31.39997294953710849, 4.461849672132297329, -4.461849672132302658 ) ) ;
#45281 = DIRECTION ( 'NONE',  ( 0.000000000000000000, -1.000000000000000000, 0.000000000000000000 ) ) ;
#45282 = ORIENTED_EDGE ( 'NONE', *, *, #120883, .F. ) ;
#45283 = FACE_OUTER_BOUND ( 'NONE', #29644, .T. ) ;
#45285 = EDGE_CURVE ( 'NONE', #63651, #60942, #41678, .T. ) ;
#45284 = DIRECTION ( 'NONE',  ( -0.7071067811865486830, -0.7071067811865464625, 0.000000000000000000 ) ) ;
#45286 = CARTESIAN_POINT ( 'NONE',  ( -42.48921356237308800, -27.52281430457085065, 5.000000000000000000 ) ) ;
#45288 = EDGE_LOOP ( 'NONE', ( #113363, #26446, #49355, #34148 ) ) ;
#45287 = CARTESIAN_POINT ( 'NONE',  ( 5.999999999999963585, 20.70535890316561733, 1.956823837851902725 ) ) ;
#45289 = EDGE_LOOP ( 'NONE', ( #86805, #27282, #112791, #102263 ) ) ;
#45290 = DIRECTION ( 'NONE',  ( 0.6830127018922180770, -0.6830127018922204085, -0.2588190451025213501 ) ) ;
#45291 = CARTESIAN_POINT ( 'NONE',  ( -6.707013264292997157, -21.74070752338405654, 4.999753212805220670 ) ) ;
#45292 = DIRECTION ( 'NONE',  ( 1.000000000000000000, 0.000000000000000000, 0.000000000000000000 ) ) ;
#45293 = EDGE_LOOP ( 'NONE', ( #52535, #47046, #39990, #16077 ) ) ;
#45294 = DIRECTION ( 'NONE',  ( -0.000000000000000000, -0.3543493200069152693, 0.9351131265310292928 ) ) ;
#45295 = FACE_OUTER_BOUND ( 'NONE', #58846, .T. ) ;
#45296 = EDGE_LOOP ( 'NONE', ( #104481, #99434, #68240, #71179 ) ) ;
#45297 = ADVANCED_FACE ( 'NONE', ( #117769 ), #96727, .T. ) ;
#45298 = CARTESIAN_POINT ( 'NONE',  ( 18.48921356237309510, -27.52281430457068367, 5.000000000000000000 ) ) ;
#45299 = LINE ( 'NONE', #2438, #30163 ) ;
#45300 = CARTESIAN_POINT ( 'NONE',  ( 11.56505274454301357, -2.500000000000000444, 3.061616997868384127E-16 ) ) ;
#45301 = LINE ( 'NONE', #2441, #32370 ) ;
#45302 = DIRECTION ( 'NONE',  ( 0.000000000000000000, 1.000000000000000000, -0.000000000000000000 ) ) ;
#45303 = PLANE ( 'NONE',  #97723 ) ;
#45304 = ADVANCED_FACE ( 'NONE', ( #106921 ), #62741, .T. ) ;
#45305 = DIRECTION ( 'NONE',  ( 0.000000000000000000, -1.000000000000000000, 0.000000000000000000 ) ) ;
#45306 = LINE ( 'NONE', #11905, #115457 ) ;
#45307 = EDGE_CURVE ( 'NONE', #18576, #17742, #130128, .T. ) ;
#45309 = EDGE_LOOP ( 'NONE', ( #135620, #37231, #32717, #94170 ) ) ;
#45308 = EDGE_CURVE ( 'NONE', #17086, #119805, #31523, .T. ) ;
#45310 = ORIENTED_EDGE ( 'NONE', *, *, #121060, .F. ) ;
#45311 =( NAMED_UNIT ( * ) PLANE_ANGLE_UNIT ( ) SI_UNIT ( $, .RADIAN. ) );
#45312 = CARTESIAN_POINT ( 'NONE',  ( 0.2997448713915885632, -27.71228299555206220, 4.000000000000000000 ) ) ;
#45313 = ADVANCED_FACE ( 'NONE', ( #67007 ), #35113, .F. ) ;
#45314 = EDGE_CURVE ( 'NONE', #124953, #142228, #112645, .T. ) ;
#45315 = AXIS2_PLACEMENT_3D ( 'NONE', #124323, #36591, #93129 ) ;
#45316 = CARTESIAN_POINT ( 'NONE',  ( 42.48921356237308800, -27.52281430457085065, 5.000000000000000000 ) ) ;
#45317 = VERTEX_POINT ( 'NONE', #68466 ) ;
#45318 = LINE ( 'NONE', #124976, #32251 ) ;
#45319 = DIRECTION ( 'NONE',  ( 0.7071067811865487940, -0.7071067811865463515, 0.000000000000000000 ) ) ;
#45320 = PLANE ( 'NONE',  #21257 ) ;
#45321 = EDGE_LOOP ( 'NONE', ( #5267, #8891, #2598, #17004 ) ) ;
#45322 = EDGE_CURVE ( 'NONE', #34296, #90987, #55422, .T. ) ;
#45323 = PRESENTATION_STYLE_ASSIGNMENT (( #89497 ) ) ;
#45324 = DIRECTION ( 'NONE',  ( -0.7071067811865486830, -0.7071067811865464625, 0.000000000000000000 ) ) ;
#45325 = CARTESIAN_POINT ( 'NONE',  ( 21.00548008471250938, 28.92564299267923644, 4.000000000000000000 ) ) ;
#45326 = DIRECTION ( 'NONE',  ( -0.000000000000000000, -0.3543493200069152693, 0.9351131265310292928 ) ) ;
#45327 = CARTESIAN_POINT ( 'NONE',  ( 54.30793019189810167, -6.109999999999999432, 1.637169565754158507 ) ) ;
#45328 = CARTESIAN_POINT ( 'NONE',  ( 27.66846741159839596, -18.74070752338408852, 20.73178291233847759 ) ) ;
#45329 = ADVANCED_FACE ( 'NONE', ( #35841 ), #1696, .T. ) ;
#45330 = CARTESIAN_POINT ( 'NONE',  ( -36.70679250724052167, 20.25929247661551358, 20.83292124670823142 ) ) ;
#45331 = VECTOR ( 'NONE', #32473, 1000.000000000000227 ) ;
#45332 = SURFACE_STYLE_FILL_AREA ( #111240 ) ;
#45333 = DIRECTION ( 'NONE',  ( 0.7071067811865487940, 0.7071067811865463515, 0.000000000000000000 ) ) ;
#45334 = ORIENTED_EDGE ( 'NONE', *, *, #130924, .F. ) ;
#45335 = DIRECTION ( 'NONE',  ( -0.7071067811865487940, 8.659560562354918067E-17, -0.7071067811865463515 ) ) ;
#45336 = VERTEX_POINT ( 'NONE', #46737 ) ;
#45337 = LINE ( 'NONE', #34421, #126477 ) ;
#45338 = EDGE_CURVE ( 'NONE', #139251, #32532, #13307, .T. ) ;
#45339 = LINE ( 'NONE', #89515, #115540 ) ;
#45340 = CARTESIAN_POINT ( 'NONE',  ( -12.20000000000000284, -40.42999999999999261, -39.50000000000000000 ) ) ;
#45341 = CARTESIAN_POINT ( 'NONE',  ( -6.328169399223488867, -15.74070752338412049, 4.000000000000000000 ) ) ;
#45342 = LINE ( 'NONE', #22791, #83452 ) ;
#45343 = FACE_OUTER_BOUND ( 'NONE', #50844, .T. ) ;
#45344 = ORIENTED_EDGE ( 'NONE', *, *, #65059, .F. ) ;
#45345 = ORIENTED_EDGE ( 'NONE', *, *, #139762, .T. ) ;
#45346 = CARTESIAN_POINT ( 'NONE',  ( 22.49999999999984368, 21.43112307739195899, 4.000000000000000000 ) ) ;
#45347 = CARTESIAN_POINT ( 'NONE',  ( 27.70710678118635428, -9.740707523384186217, 5.000000000000000000 ) ) ;
#45348 = EDGE_CURVE ( 'NONE', #47525, #67739, #80059, .T. ) ;
#45349 = PLANE ( 'NONE',  #126121 ) ;
#45350 = VECTOR ( 'NONE', #112735, 999.9999999999998863 ) ;
#45351 = CARTESIAN_POINT ( 'NONE',  ( 32.99999999999976552, -18.03360074219755660, 5.000000000000000000 ) ) ;
#45352 = CARTESIAN_POINT ( 'NONE',  ( 74.16252705046288440, 7.949999999999998401, 1.460391307983218338E-15 ) ) ;
#45353 = CARTESIAN_POINT ( 'NONE',  ( -34.92500000000001137, -10.29806943317888290, 4.500000000000000888 ) ) ;
#45354 = VECTOR ( 'NONE', #101130, 1000.000000000000227 ) ;
#45355 = CARTESIAN_POINT ( 'NONE',  ( -24.29974487139158867, -27.71228299555223273, 4.000000000000000000 ) ) ;
#45356 = VERTEX_POINT ( 'NONE', #24220 ) ;
#45357 = CARTESIAN_POINT ( 'NONE',  ( 73.18749999999995737, -5.819803920172573086, 5.819803920172572198 ) ) ;
#45358 = AXIS2_PLACEMENT_3D ( 'NONE', #132253, #77164, #111909 ) ;
#45359 = CARTESIAN_POINT ( 'NONE',  ( 1.369266385878517678, 5.729711685171558773E-16, 4.607329295533711289 ) ) ;
#45360 = DIRECTION ( 'NONE',  ( 0.7071067811865487940, 0.7071067811865463515, 0.000000000000000000 ) ) ;
#45361 = CARTESIAN_POINT ( 'NONE',  ( -1.499999999999982236, 1.087461875839230707, 4.000000000000000000 ) ) ;
#45362 = EDGE_CURVE ( 'NONE', #62795, #61349, #57578, .T. ) ;
#45363 = EDGE_LOOP ( 'NONE', ( #126870, #4460, #113928, #109288 ) ) ;
#45364 = CARTESIAN_POINT ( 'NONE',  ( -13.11017322888201697, -22.22500000000000142, 4.785647885939352975 ) ) ;
#45365 = EDGE_CURVE ( 'NONE', #95876, #141613, #14023, .T. ) ;
#45366 = CARTESIAN_POINT ( 'NONE',  ( 8.500000000000000000, 2.055000000000001492, 0.000000000000000000 ) ) ;
#45367 = CARTESIAN_POINT ( 'NONE',  ( 65.77126352523144703, 4.472830434245839371, 4.472830434245842035 ) ) ;
#45368 = ADVANCED_FACE ( 'NONE', ( #58324 ), #77197, .F. ) ;
#45369 = ORIENTED_EDGE ( 'NONE', *, *, #141059, .F. ) ;
#45370 = ORIENTED_EDGE ( 'NONE', *, *, #1841, .T. ) ;
#45371 = DIRECTION ( 'NONE',  ( -1.000000000000000000, -0.000000000000000000, -0.000000000000000000 ) ) ;
#45372 = EDGE_CURVE ( 'NONE', #129322, #58187, #102505, .T. ) ;
#45373 = CARTESIAN_POINT ( 'NONE',  ( -8.207106781186476852, -20.24070752338407075, 5.000000000000000000 ) ) ;
#45374 = CARTESIAN_POINT ( 'NONE',  ( 25.97159235450331849, 9.902892378096218942E-16, 0.000000000000000000 ) ) ;
#45375 = CARTESIAN_POINT ( 'NONE',  ( -32.99999999999977263, -5.527737879153217015, -7.983877177622296095 ) ) ;
#45376 = PLANE ( 'NONE',  #76686 ) ;
#45378 = ORIENTED_EDGE ( 'NONE', *, *, #796, .T. ) ;
#45377 = CARTESIAN_POINT ( 'NONE',  ( 34.47516574401890921, -8.971932658884092859, 4.998110765256834398 ) ) ;
#45379 = DIRECTION ( 'NONE',  ( -1.000000000000000000, -1.224606353822377258E-16, -0.000000000000000000 ) ) ;
#45380 = DIRECTION ( 'NONE',  ( -1.000000000000000000, -1.224606353822377258E-16, -0.000000000000000000 ) ) ;
#45381 = LINE ( 'NONE', #60537, #14715 ) ;
#45382 = EDGE_LOOP ( 'NONE', ( #47256, #139651, #54873, #112587 ) ) ;
#45383 = ORIENTED_EDGE ( 'NONE', *, *, #79569, .F. ) ;
#45384 = CARTESIAN_POINT ( 'NONE',  ( 63.72959685856477563, -6.110000000000000320, -1.637169565754161393 ) ) ;
#45385 = ORIENTED_EDGE ( 'NONE', *, *, #135183, .T. ) ;
#45386 = ADVANCED_FACE ( 'NONE', ( #124235 ), #24912, .F. ) ;
#45387 = CARTESIAN_POINT ( 'NONE',  ( 0.000000000000000000, 0.000000000000000000, 10.00000000000000000 ) ) ;
#45388 = DIRECTION ( 'NONE',  ( 0.000000000000000000, 0.000000000000000000, -1.000000000000000000 ) ) ;
#45389 = CARTESIAN_POINT ( 'NONE',  ( 4.171830600776436526, -5.240707523384232402, 4.000000000000000000 ) ) ;
#45390 = DIRECTION ( 'NONE',  ( -0.7071067811865486830, 0.7071067811865464625, 0.000000000000000000 ) ) ;
#45391 = DIRECTION ( 'NONE',  ( 0.7071067811865487940, -0.7071067811865463515, 0.000000000000000000 ) ) ;
#45392 = ORIENTED_EDGE ( 'NONE', *, *, #42451, .F. ) ;
#45393 = VERTEX_POINT ( 'NONE', #100353 ) ;
#45394 = DIRECTION ( 'NONE',  ( -0.7071067811865486830, -0.7071067811865464625, 0.000000000000000000 ) ) ;
#45396 = ADVANCED_FACE ( 'NONE', ( #110477 ), #79354, .F. ) ;
#45395 = CARTESIAN_POINT ( 'NONE',  ( -31.92499999999997584, 0.000000000000000000, -37.00000000000000000 ) ) ;
#45397 = ORIENTED_EDGE ( 'NONE', *, *, #19721, .F. ) ;
#45398 = LINE ( 'NONE', #80865, #106862 ) ;
#45399 = CARTESIAN_POINT ( 'NONE',  ( 24.48921356237309510, -27.52281430457072631, 5.000000000000000000 ) ) ;
#45400 = FACE_OUTER_BOUND ( 'NONE', #18903, .T. ) ;
#45401 =( BOUNDED_CURVE ( )  B_SPLINE_CURVE ( 3, ( #86745, #109904, #54140, #65741 ),
 .UNSPECIFIED., .F., .T. ) 
 B_SPLINE_CURVE_WITH_KNOTS ( ( 4, 4 ),
 ( 1.964434688349488756, 3.503810798801452187 ),
 .UNSPECIFIED. ) 
 CURVE ( )  GEOMETRIC_REPRESENTATION_ITEM ( )  RATIONAL_B_SPLINE_CURVE ( ( 1.000000000000000000, 0.8120851936182280628, 0.8120851936182280628, 1.000000000000000000 ) ) 
 REPRESENTATION_ITEM ( '' )  );
#45402 = ORIENTED_EDGE ( 'NONE', *, *, #35365, .T. ) ;
#45403 = EDGE_CURVE ( 'NONE', #13716, #82359, #1004, .T. ) ;
#45404 = FACE_BOUND ( 'NONE', #119233, .T. ) ;
#45405 = DIRECTION ( 'NONE',  ( -0.3543493200069163240, -0.000000000000000000, 0.9351131265310288487 ) ) ;
#45406 = DIRECTION ( 'NONE',  ( 1.000000000000000000, 0.000000000000000000, 0.000000000000000000 ) ) ;
#45407 = CARTESIAN_POINT ( 'NONE',  ( 38.99451991528749062, 28.92564299267965211, 4.000000000000000000 ) ) ;
#45408 = DIRECTION ( 'NONE',  ( -0.7071067811865486830, -0.7071067811865464625, 0.000000000000000000 ) ) ;
#45409 = CARTESIAN_POINT ( 'NONE',  ( -20.29298673570681544, -21.74070752338406720, 4.999753212805217117 ) ) ;
#45410 = DIRECTION ( 'NONE',  ( -5.370136480751025050E-27, -0.8105404501096011849, -0.5856826604366268674 ) ) ;
#45412 = ORIENTED_EDGE ( 'NONE', *, *, #138260, .F. ) ;
#45411 = VECTOR ( 'NONE', #138179, 1000.000000000000000 ) ;
#45413 = EDGE_CURVE ( 'NONE', #47758, #126555, #121369, .T. ) ;
#45414 = VERTEX_POINT ( 'NONE', #11145 ) ;
#45415 = CARTESIAN_POINT ( 'NONE',  ( 105.4954301918981230, 5.291415217122916737, 3.055000000000001936 ) ) ;
#45416 = ORIENTED_EDGE ( 'NONE', *, *, #38912, .T. ) ;
#45417 = CIRCLE ( 'NONE', #33811, 2.500000000000000888 ) ;
#45418 = PRESENTATION_STYLE_ASSIGNMENT (( #51454 ) ) ;
#45419 = ORIENTED_EDGE ( 'NONE', *, *, #116709, .F. ) ;
#45420 = CARTESIAN_POINT ( 'NONE',  ( -23.20710678118638981, 18.75929247661553134, 5.000000000000000000 ) ) ;
#45421 = EDGE_CURVE ( 'NONE', #68681, #123983, #44579, .T. ) ;
#45422 = CARTESIAN_POINT ( 'NONE',  ( 3.545806282870439308, 5.278424836066143655, -3.047499999999997655 ) ) ;
#45424 = EDGE_CURVE ( 'NONE', #36667, #90206, #33683, .T. ) ;
#45423 = CARTESIAN_POINT ( 'NONE',  ( -29.29289321881324426, -0.7407075233842805861, 5.000000000000000000 ) ) ;
#45425 = VERTEX_POINT ( 'NONE', #90168 ) ;
#45426 = LINE ( 'NONE', #13444, #122357 ) ;
#45427 = DIRECTION ( 'NONE',  ( 1.000000000000000000, 0.000000000000000000, 0.000000000000000000 ) ) ;
#45428 = LINE ( 'NONE', #78745, #105579 ) ;
#45429 = AXIS2_PLACEMENT_3D ( 'NONE', #43007, #119116, #97335 ) ;
#45430 = CYLINDRICAL_SURFACE ( 'NONE', #124542, 5.999999999999998224 ) ;
#45431 = DIRECTION ( 'NONE',  ( -0.7071067811865486830, -0.7071067811865464625, 0.000000000000000000 ) ) ;
#45432 = DIRECTION ( 'NONE',  ( -0.000000000000000000, 0.000000000000000000, 1.000000000000000000 ) ) ;
#45433 = EDGE_LOOP ( 'NONE', ( #20651, #52885, #142082, #5577 ) ) ;
#45434 = DIRECTION ( 'NONE',  ( 0.5735764363510444941, 0.8191520442889929088, 0.000000000000000000 ) ) ;
#45435 = DIRECTION ( 'NONE',  ( 0.7071067811865487940, 0.7071067811865463515, 0.000000000000000000 ) ) ;
#45436 = VERTEX_POINT ( 'NONE', #116923 ) ;
#45437 = ORIENTED_EDGE ( 'NONE', *, *, #137379, .F. ) ;
#45438 = EDGE_CURVE ( 'NONE', #6138, #131532, #60440, .T. ) ;
#45439 = ORIENTED_EDGE ( 'NONE', *, *, #67785, .T. ) ;
#45440 = CARTESIAN_POINT ( 'NONE',  ( 54.83376352523143282, 6.110000000000001208, 1.122388791418549305E-15 ) ) ;
#45441 = ORIENTED_EDGE ( 'NONE', *, *, #15169, .T. ) ;
#45442 = VECTOR ( 'NONE', #37331, 1000.000000000000227 ) ;
#45443 = LINE ( 'NONE', #108481, #60561 ) ;
#45444 = PRESENTATION_LAYER_ASSIGNMENT (  '', '', ( #84740 ) ) ;
#45445 = CARTESIAN_POINT ( 'NONE',  ( 3.691639616203772789, 6.094999999999988205, -1.633150327867694651 ) ) ;
#45446 = CARTESIAN_POINT ( 'NONE',  ( 91.00043019189810423, -3.055000000000002380, 5.291415217122920289 ) ) ;
#45447 = SURFACE_SIDE_STYLE ('',( #56343 ) ) ;
#45448 = ORIENTED_EDGE ( 'NONE', *, *, #128837, .F. ) ;
#45449 = VECTOR ( 'NONE', #116817, 1000.000000000000227 ) ;
#45450 = ORIENTED_EDGE ( 'NONE', *, *, #125407, .F. ) ;
#45451 = DIRECTION ( 'NONE',  ( 1.000000000000000000, -0.000000000000000000, 0.000000000000000000 ) ) ;
#45452 = VECTOR ( 'NONE', #87030, 1000.000000000000000 ) ;
#45453 = CARTESIAN_POINT ( 'NONE',  ( 27.18398860626900060, 28.73617430169806042, 5.000000000000000000 ) ) ;
#45454 = ORIENTED_EDGE ( 'NONE', *, *, #29816, .F. ) ;
#45455 =( NAMED_UNIT ( * ) SI_UNIT ( $, .STERADIAN. ) SOLID_ANGLE_UNIT ( ) );
#45456 = DIRECTION ( 'NONE',  ( 0.7071067811865487940, 0.7071067811865463515, -0.000000000000000000 ) ) ;
#45457 = LINE ( 'NONE', #22216, #45149 ) ;
#45458 = ORIENTED_EDGE ( 'NONE', *, *, #120231, .T. ) ;
#45459 = CARTESIAN_POINT ( 'NONE',  ( 15.18398860626900237, 28.73617430169797871, 5.000000000000000000 ) ) ;
#45460 = VERTEX_POINT ( 'NONE', #93034 ) ;
#45461 = ORIENTED_EDGE ( 'NONE', *, *, #24186, .T. ) ;
#45462 = EDGE_LOOP ( 'NONE', ( #119272, #135019, #80609, #112207 ) ) ;
#45463 = EDGE_CURVE ( 'NONE', #91901, #91730, #37228, .T. ) ;
#45464 = CARTESIAN_POINT ( 'NONE',  ( 36.83652871126526662, 15.75929247661555799, 9.299976744543005935 ) ) ;
#45465 = DIRECTION ( 'NONE',  ( -0.7071067811865487940, 0.7071067811865463515, -0.000000000000000000 ) ) ;
#45466 = LINE ( 'NONE', #67193, #64843 ) ;
#45468 = ADVANCED_FACE ( 'NONE', ( #106017 ), #71302, .T. ) ;
#45467 = EDGE_CURVE ( 'NONE', #63778, #40456, #59035, .T. ) ;
#45469 = ADVANCED_FACE ( 'NONE', ( #114067 ), #123877, .T. ) ;
#45470 = DIRECTION ( 'NONE',  ( -0.000000000000000000, 0.000000000000000000, 1.000000000000000000 ) ) ;
#45471 = ORIENTED_EDGE ( 'NONE', *, *, #47305, .T. ) ;
#45472 = CARTESIAN_POINT ( 'NONE',  ( 28.82816939922333432, -20.24070752338407431, 4.000000000000000000 ) ) ;
#45473 = EDGE_CURVE ( 'NONE', #17685, #37393, #29026, .T. ) ;
#45474 = EDGE_CURVE ( 'NONE', #35947, #59015, #15430, .T. ) ;
#45475 = CARTESIAN_POINT ( 'NONE',  ( 9.457903141435219041, 6.871911579029515771, 3.967499999999989146 ) ) ;
#45476 = CARTESIAN_POINT ( 'NONE',  ( -3.717577386425651831, -21.73023691814492153, 5.000000000000000888 ) ) ;
#45477 = ADVANCED_FACE ( 'NONE', ( #105328 ), #27771, .T. ) ;
#45478 = CARTESIAN_POINT ( 'NONE',  ( -23.48860328114998453, 7.166961737892989071, 4.667035327419722712 ) ) ;
#45479 = CARTESIAN_POINT ( 'NONE',  ( -14.20710678118644665, -2.240707523384257716, 5.000000000000000000 ) ) ;
#45480 = ORIENTED_EDGE ( 'NONE', *, *, #241, .F. ) ;
#45481 = ORIENTED_EDGE ( 'NONE', *, *, #43307, .F. ) ;
#45482 = EDGE_CURVE ( 'NONE', #74460, #20468, #137979, .T. ) ;
#45483 = EDGE_LOOP ( 'NONE', ( #13245, #11015, #31659, #33871 ) ) ;
#45484 = CARTESIAN_POINT ( 'NONE',  ( 20.41666666666667140, 5.278424836066147208, 3.047499999999990550 ) ) ;
#45485 = CARTESIAN_POINT ( 'NONE',  ( 58.31249999999998579, 5.819803920172571310, 5.819803920172576639 ) ) ;
#45486 = VECTOR ( 'NONE', #128765, 1000.000000000000227 ) ;
#45487 = EDGE_CURVE ( 'NONE', #65559, #20866, #138700, .T. ) ;
#45488 = DIRECTION ( 'NONE',  ( -0.6830127018922181881, 0.6830127018922202975, -0.2588190451025214056 ) ) ;
#45489 = DIRECTION ( 'NONE',  ( 0.7071067811865487940, -0.7071067811865463515, 0.000000000000000000 ) ) ;
#45490 = CARTESIAN_POINT ( 'NONE',  ( 8.124863741626466407, 8.711972394638584305, -3.792219164446597013 ) ) ;
#45491 = ADVANCED_FACE ( 'NONE', ( #36515 ), #5282, .T. ) ;
#45492 = LINE ( 'NONE', #78812, #108505 ) ;
#45493 = DIRECTION ( 'NONE',  ( -0.7071067811865487940, 0.7071067811865463515, -0.000000000000000000 ) ) ;
#45494 = FACE_OUTER_BOUND ( 'NONE', #86329, .T. ) ;
#45495 = DIRECTION ( 'NONE',  ( -0.7071067811865486830, -0.7071067811865464625, 0.000000000000000000 ) ) ;
#45496 = ORIENTED_EDGE ( 'NONE', *, *, #112737, .F. ) ;
#45497 = DIRECTION ( 'NONE',  ( -0.5735764363510503783, -0.8191520442889886899, 0.000000000000000000 ) ) ;
#45498 = VECTOR ( 'NONE', #65676, 999.9999999999998863 ) ;
#45499 = ORIENTED_EDGE ( 'NONE', *, *, #72582, .F. ) ;
#45500 = CARTESIAN_POINT ( 'NONE',  ( 16.99919035942976109, -0.8850635513006737121, -35.72698641301105482 ) ) ;
#45501 = EDGE_LOOP ( 'NONE', ( #140326, #31748, #109171, #36768 ) ) ;
#45502 = EDGE_CURVE ( 'NONE', #57842, #19888, #116215, .T. ) ;
#45503 = CARTESIAN_POINT ( 'NONE',  ( 17.25413961620377279, 3.047499999999993214, -5.278424836066146320 ) ) ;
#45505 = ORIENTED_EDGE ( 'NONE', *, *, #109920, .F. ) ;
#45504 = CARTESIAN_POINT ( 'NONE',  ( 2.588385094051668833, 22.22500000000000497, 4.777194822843813249 ) ) ;
#45506 = FACE_OUTER_BOUND ( 'NONE', #122523, .T. ) ;
#45507 = PLANE ( 'NONE',  #21736 ) ;
#45508 = ORIENTED_EDGE ( 'NONE', *, *, #31211, .F. ) ;
#45509 = ORIENTED_EDGE ( 'NONE', *, *, #71165, .T. ) ;
#45510 = DIRECTION ( 'NONE',  ( -0.6830127018922180770, -0.6830127018922204085, -0.2588190451025213501 ) ) ;
#45511 = VERTEX_POINT ( 'NONE', #16146 ) ;
#45512 = ADVANCED_FACE ( 'NONE', ( #38661 ), #48834, .T. ) ;
#45513 = LINE ( 'NONE', #78842, #56628 ) ;
#45514 = CIRCLE ( 'NONE', #96350, 2.500000000000000888 ) ;
#45515 = CARTESIAN_POINT ( 'NONE',  ( 104.0583603837962272, -7.949999999999997513, -2.130196079827425759 ) ) ;
#45516 = CARTESIAN_POINT ( 'NONE',  ( -72.18398860626899705, 28.73617430169837661, 5.000000000000000000 ) ) ;
#45517 = CARTESIAN_POINT ( 'NONE',  ( 25.39999999999999858, -16.48000000000005016, 12.69999999999954454 ) ) ;
#45518 = EDGE_LOOP ( 'NONE', ( #72040, #95000, #61316, #96930 ) ) ;
#45519 = VECTOR ( 'NONE', #80342, 1000.000000000000227 ) ;
#45520 = PLANE ( 'NONE',  #79218 ) ;
#45521 = CARTESIAN_POINT ( 'NONE',  ( 24.29974487139158867, -27.71228299555223273, 4.000000000000000000 ) ) ;
#45522 = LINE ( 'NONE', #3382, #80848 ) ;
#45523 = CARTESIAN_POINT ( 'NONE',  ( 17.20833333333333570, 3.047499999999997655, 5.278424836066143655 ) ) ;
#45524 = CARTESIAN_POINT ( 'NONE',  ( 22.29123647476855652, -9.717572351234235426E-16, -7.934999999999990727 ) ) ;
#45525 = CARTESIAN_POINT ( 'NONE',  ( -48.29974487139158867, -27.71228299555239971, 4.000000000000000000 ) ) ;
#45526 = DIRECTION ( 'NONE',  ( -0.3543493200069162685, -0.000000000000000000, -0.9351131265310288487 ) ) ;
#45527 = ORIENTED_EDGE ( 'NONE', *, *, #5245, .F. ) ;
#45528 = VERTEX_POINT ( 'NONE', #124941 ) ;
#45529 = CARTESIAN_POINT ( 'NONE',  ( 34.92499999999998295, 15.58119340046983758, 2.482413320905456633 ) ) ;
#45530 = EDGE_CURVE ( 'NONE', #118158, #81879, #61177, .T. ) ;
#45531 = ORIENTED_EDGE ( 'NONE', *, *, #126232, .F. ) ;
#45532 = VECTOR ( 'NONE', #22182, 999.9999999999998863 ) ;
#45533 = CARTESIAN_POINT ( 'NONE',  ( 90.70876352523143282, -7.482591942790329030E-16, 6.110000000000001208 ) ) ;
#45534 = EDGE_CURVE ( 'NONE', #142960, #42538, #26358, .T. ) ;
#45535 = DIRECTION ( 'NONE',  ( -0.7071067811865487940, 0.7071067811865463515, 0.000000000000000000 ) ) ;
#45536 = CARTESIAN_POINT ( 'NONE',  ( -7.828169399223478209, 0.7592924766157120864, 4.000000000000000000 ) ) ;
#45537 = FACE_OUTER_BOUND ( 'NONE', #67666, .T. ) ;
#45538 = FACE_OUTER_BOUND ( 'NONE', #143378, .T. ) ;
#45539 = ORIENTED_EDGE ( 'NONE', *, *, #88420, .T. ) ;
#45540 =( NAMED_UNIT ( * ) SI_UNIT ( $, .STERADIAN. ) SOLID_ANGLE_UNIT ( ) );
#45541 = DIRECTION ( 'NONE',  ( -0.7071067811865487940, 0.7071067811865463515, 0.000000000000000000 ) ) ;
#45542 = EDGE_CURVE ( 'NONE', #11127, #116312, #53077, .T. ) ;
#45543 = DIRECTION ( 'NONE',  ( 0.000000000000000000, -1.000000000000000000, 0.000000000000000000 ) ) ;
#45544 = AXIS2_PLACEMENT_3D ( 'NONE', #44692, #52653, #55533 ) ;
#45545 = CARTESIAN_POINT ( 'NONE',  ( 1.499999999999990896, 22.01701374228155927, 2.453858888625627621 ) ) ;
#45546 = DIRECTION ( 'NONE',  ( -0.000000000000000000, 0.000000000000000000, 1.000000000000000000 ) ) ;
#45548 = EDGE_LOOP ( 'NONE', ( #44884, #95530, #36299 ) ) ;
#45547 = DIRECTION ( 'NONE',  ( 0.000000000000000000, -1.000000000000000000, -1.734723475976807686E-15 ) ) ;
#45549 = CARTESIAN_POINT ( 'NONE',  ( -54.18398860626899705, 28.73617430169825226, 5.000000000000000000 ) ) ;
#45550 = PLANE ( 'NONE',  #141926 ) ;
#45551 = DIRECTION ( 'NONE',  ( 0.7071067811865487940, -0.7071067811865463515, 0.000000000000000000 ) ) ;
#45552 = ADVANCED_FACE ( 'NONE', ( #85707 ), #42958, .T. ) ;
#45553 = VECTOR ( 'NONE', #17865, 999.9999999999998863 ) ;
#45554 = CARTESIAN_POINT ( 'NONE',  ( 39.18398860626899705, 28.73617430169814568, 5.000000000000000000 ) ) ;
#45555 = AXIS2_PLACEMENT_3D ( 'NONE', #137918, #70553, #135088 ) ;
#45556 = EDGE_LOOP ( 'NONE', ( #17106, #100205, #69141, #142626 ) ) ;
#45557 = EDGE_LOOP ( 'NONE', ( #31399, #105204, #38714, #60340, #101373 ) ) ;
#45558 = ORIENTED_EDGE ( 'NONE', *, *, #133692, .T. ) ;
#45559 = VECTOR ( 'NONE', #112401, 1000.000000000000000 ) ;
#45560 = CARTESIAN_POINT ( 'NONE',  ( 96.39626352523144703, 4.472830434245840259, -4.472830434245839371 ) ) ;
#45561 = ORIENTED_EDGE ( 'NONE', *, *, #36282, .F. ) ;
#45562 = EDGE_CURVE ( 'NONE', #11291, #125242, #32061, .T. ) ;
#45563 = CARTESIAN_POINT ( 'NONE',  ( 9.299744871391588674, -27.71228299555212971, 4.000000000000000000 ) ) ;
#45564 = LINE ( 'NONE', #132573, #126663 ) ;
#45566 = VECTOR ( 'NONE', #107549, 1000.000000000000000 ) ;
#45565 = PLANE ( 'NONE',  #64259 ) ;
#45567 = CARTESIAN_POINT ( 'NONE',  ( -17.20710678118642889, 18.75929247661552779, 5.000000000000000000 ) ) ;
#45568 = ORIENTED_EDGE ( 'NONE', *, *, #14906, .T. ) ;
#45569 = LINE ( 'NONE', #110746, #37486 ) ;
#45570 = CARTESIAN_POINT ( 'NONE',  ( 11.62000000000000099, 9.521314400968980422E-16, 0.000000000000000000 ) ) ;
#45571 = CARTESIAN_POINT ( 'NONE',  ( 19.49999999999986500, 14.14708470758592895, -0.5283514160167009921 ) ) ;
#45572 = CARTESIAN_POINT ( 'NONE',  ( 90.62043019189810877, 3.055000000000001936, -5.291415217122916737 ) ) ;
#45573 = ORIENTED_EDGE ( 'NONE', *, *, #82015, .F. ) ;
#45574 = EDGE_CURVE ( 'NONE', #39797, #57666, #29901, .T. ) ;
#45575 = CARTESIAN_POINT ( 'NONE',  ( 42.18398860626899705, 28.73617430169816700, 5.000000000000000000 ) ) ;
#45576 = FACE_OUTER_BOUND ( 'NONE', #114251, .T. ) ;
#45577 = VERTEX_POINT ( 'NONE', #64697 ) ;
#45578 = VERTEX_POINT ( 'NONE', #41497 ) ;
#45579 = EDGE_CURVE ( 'NONE', #58696, #645, #131380, .T. ) ;
#45580 = DIRECTION ( 'NONE',  ( 1.000000000000000000, 0.000000000000000000, 0.000000000000000000 ) ) ;
#45581 = CARTESIAN_POINT ( 'NONE',  ( 21.21290314143522338, 3.967499999999992699, -6.871911579029513994 ) ) ;
#45582 = LINE ( 'NONE', #133984, #18757 ) ;
#45583 = CARTESIAN_POINT ( 'NONE',  ( 162.5049720716601200, 26.96999999999993847, 34.75200654934010913 ) ) ;
#45584 = CARTESIAN_POINT ( 'NONE',  ( -16.49999999999987566, 13.46639925780212010, 5.000000000000000000 ) ) ;
#45585 = DIRECTION ( 'NONE',  ( 0.000000000000000000, 0.000000000000000000, -1.000000000000000000 ) ) ;
#45586 = ADVANCED_FACE ( 'NONE', ( #76293 ), #128531, .F. ) ;
#45587 = ORIENTED_EDGE ( 'NONE', *, *, #39228, .T. ) ;
#45588 = ORIENTED_EDGE ( 'NONE', *, *, #44198, .F. ) ;
#45589 = PLANE ( 'NONE',  #57337 ) ;
#45590 = VERTEX_POINT ( 'NONE', #63302 ) ;
#45591 = ORIENTED_EDGE ( 'NONE', *, *, #105987, .F. ) ;
#45592 = VECTOR ( 'NONE', #48554, 1000.000000000000000 ) ;
#45593 = ADVANCED_FACE ( 'NONE', ( #7426 ), #120449, .F. ) ;
#45595 = ADVANCED_FACE ( 'NONE', ( #53836 ), #129951, .F. ) ;
#45594 = LINE ( 'NONE', #12203, #40473 ) ;
#45596 = VERTEX_POINT ( 'NONE', #109612 ) ;
#45597 = CARTESIAN_POINT ( 'NONE',  ( 55.93336038379622011, 2.130196079827431532, -7.949999999999996625 ) ) ;
#45598 = CARTESIAN_POINT ( 'NONE',  ( -15.18398860626900237, 28.73617430169797871, 5.000000000000000000 ) ) ;
#45599 = VECTOR ( 'NONE', #82079, 1000.000000000000000 ) ;
#45600 = CARTESIAN_POINT ( 'NONE',  ( 1.499999999999994449, 13.56627193232215056, -10.57019076586068351 ) ) ;
#45601 = CARTESIAN_POINT ( 'NONE',  ( 17.67183060077635304, 11.25929247661560950, 4.000000000000000000 ) ) ;
#45602 = EDGE_LOOP ( 'NONE', ( #62768, #126009, #43986, #10858 ) ) ;
#45603 = CARTESIAN_POINT ( 'NONE',  ( -42.48921356237308800, -27.52281430457085065, 5.000000000000000000 ) ) ;
#45605 = ORIENTED_EDGE ( 'NONE', *, *, #78762, .F. ) ;
#45604 = CIRCLE ( 'NONE', #73330, 4.000000000000000000 ) ;
#45606 = DIRECTION ( 'NONE',  ( -0.6830127018922181881, 0.6830127018922202975, -0.2588190451025214056 ) ) ;
#45607 = ORIENTED_EDGE ( 'NONE', *, *, #88392, .T. ) ;
#45608 = DIRECTION ( 'NONE',  ( -0.7071067811865486830, -0.7071067811865464625, 0.000000000000000000 ) ) ;
#45609 = EDGE_CURVE ( 'NONE', #114228, #81908, #119058, .T. ) ;
#45610 = ORIENTED_EDGE ( 'NONE', *, *, #13763, .F. ) ;
#45611 = CARTESIAN_POINT ( 'NONE',  ( -45.48921356237309510, -27.52281430457087197, 5.000000000000000000 ) ) ;
#45612 = ORIENTED_EDGE ( 'NONE', *, *, #57881, .T. ) ;
#45613 = ORIENTED_EDGE ( 'NONE', *, *, #54848, .T. ) ;
#45614 = VERTEX_POINT ( 'NONE', #107472 ) ;
#45615 = STYLED_ITEM ( 'NONE', ( #44366 ), #106840 ) ;
#45616 = CARTESIAN_POINT ( 'NONE',  ( 8.538396446294241215, -9.740707523384180888, 17.74957260769612688 ) ) ;
#45617 = DIRECTION ( 'NONE',  ( 0.3543493200069162685, -0.000000000000000000, -0.9351131265310288487 ) ) ;
#45618 = CARTESIAN_POINT ( 'NONE',  ( 6.183988606268994381, 28.73617430169791476, 5.000000000000000000 ) ) ;
#45619 = VECTOR ( 'NONE', #106871, 999.9999999999998863 ) ;
#45620 = CARTESIAN_POINT ( 'NONE',  ( 116.6670968585647756, -3.055000000000000160, -5.291415217122921177 ) ) ;
#45621 = DIRECTION ( 'NONE',  ( -0.000000000000000000, 0.000000000000000000, 1.000000000000000000 ) ) ;
#45622 = LINE ( 'NONE', #134035, #87569 ) ;
#45623 = CARTESIAN_POINT ( 'NONE',  ( 2.700255128608413990, -27.71228299555204089, 4.000000000000000000 ) ) ;
#45624 = VERTEX_POINT ( 'NONE', #139434 ) ;
#45625 = CARTESIAN_POINT ( 'NONE',  ( 12.29974487139158512, -27.71228299555214747, 4.000000000000000000 ) ) ;
#45626 = DIRECTION ( 'NONE',  ( 0.7071067811865487940, 0.7071067811865463515, 0.000000000000000000 ) ) ;
#45627 = DIRECTION ( 'NONE',  ( -0.000000000000000000, 0.000000000000000000, 1.000000000000000000 ) ) ;
#45628 = VERTEX_POINT ( 'NONE', #74142 ) ;
#45629 = ORIENTED_EDGE ( 'NONE', *, *, #46855, .F. ) ;
#45630 = EDGE_CURVE ( 'NONE', #137150, #20442, #10290, .T. ) ;
#45631 = CARTESIAN_POINT ( 'NONE',  ( -10.59167451900992418, -0.7407075233842735917, 14.76736230305378328 ) ) ;
#45632 = ORIENTED_EDGE ( 'NONE', *, *, #13588, .F. ) ;
#45633 = ORIENTED_EDGE ( 'NONE', *, *, #52250, .F. ) ;
#45634 = DIRECTION ( 'NONE',  ( 0.7071067811865486830, -0.7071067811865464625, -0.000000000000000000 ) ) ;
#45635 = CARTESIAN_POINT ( 'NONE',  ( 29.99999999999979039, -12.41253812416062985, 4.000000000000000000 ) ) ;
#45636 = DIRECTION ( 'NONE',  ( -0.000000000000000000, 0.3543493200069153248, 0.9351131265310292928 ) ) ;
#45637 = LINE ( 'NONE', #122436, #2399 ) ;
#45638 = ORIENTED_EDGE ( 'NONE', *, *, #24812, .F. ) ;
#45639 = DIRECTION ( 'NONE',  ( -0.7071067811865486830, -0.7071067811865464625, 0.000000000000000000 ) ) ;
#45640 = ORIENTED_EDGE ( 'NONE', *, *, #24705, .T. ) ;
#45641 = VECTOR ( 'NONE', #32179, 1000.000000000000000 ) ;
#45643 = DIRECTION ( 'NONE',  ( -0.7071067811865487940, 0.7071067811865463515, -0.000000000000000000 ) ) ;
#45642 = VECTOR ( 'NONE', #141473, 1000.000000000000000 ) ;
#45645 = EDGE_CURVE ( 'NONE', #138468, #41591, #84333, .T. ) ;
#45644 = VECTOR ( 'NONE', #17160, 1000.000000000000000 ) ;
#45646 = CARTESIAN_POINT ( 'NONE',  ( 15.52540314143522160, 2.126176841940962348, 7.934999999999989839 ) ) ;
#45647 = ORIENTED_EDGE ( 'NONE', *, *, #103919, .F. ) ;
#45648 = CARTESIAN_POINT ( 'NONE',  ( 82.74543019189812298, -5.291415217122919401, -3.055000000000000604 ) ) ;
#45649 = EDGE_CURVE ( 'NONE', #81493, #116320, #42247, .T. ) ;
#45650 = CARTESIAN_POINT ( 'NONE',  ( -24.32816939922335209, -9.740707523384187994, 4.000000000000000000 ) ) ;
#45651 = CARTESIAN_POINT ( 'NONE',  ( 2.700255128608413990, -27.71228299555204089, 4.000000000000000000 ) ) ;
#45652 = EDGE_LOOP ( 'NONE', ( #105752, #77221, #95662, #134899, #134801, #70470 ) ) ;
#45653 = VECTOR ( 'NONE', #36036, 999.9999999999998863 ) ;
#45654 = ORIENTED_EDGE ( 'NONE', *, *, #134174, .F. ) ;
#45655 = EDGE_CURVE ( 'NONE', #142129, #39099, #106741, .T. ) ;
#45656 = VERTEX_POINT ( 'NONE', #8136 ) ;
#45657 = CARTESIAN_POINT ( 'NONE',  ( 11.67183060077639034, 8.259292476615637923, 4.000000000000000000 ) ) ;
#45658 = PLANE ( 'NONE',  #9212 ) ;
#45659 = DIRECTION ( 'NONE',  ( 0.000000000000000000, -1.000000000000000000, 0.000000000000000000 ) ) ;
#45660 = VECTOR ( 'NONE', #135749, 1000.000000000000000 ) ;
#45661 = CARTESIAN_POINT ( 'NONE',  ( -21.18398860626899349, 28.73617430169802134, 5.000000000000000000 ) ) ;
#45662 = EDGE_CURVE ( 'NONE', #106288, #42560, #86458, .T. ) ;
#45663 = FACE_OUTER_BOUND ( 'NONE', #115166, .T. ) ;
#45664 = VERTEX_POINT ( 'NONE', #75577 ) ;
#45665 = DIRECTION ( 'NONE',  ( -1.000000000000000000, -1.224606353822377258E-16, -0.000000000000000000 ) ) ;
#45666 = ADVANCED_FACE ( 'NONE', ( #129214 ), #118337, .F. ) ;
#45667 = DIRECTION ( 'NONE',  ( 1.000000000000000000, 0.000000000000000000, 0.000000000000000000 ) ) ;
#45668 = DIRECTION ( 'NONE',  ( 1.734723475976806848E-16, -1.000000000000000000, 0.000000000000000000 ) ) ;
#45669 = ORIENTED_EDGE ( 'NONE', *, *, #70549, .F. ) ;
#45670 = LINE ( 'NONE', #11541, #113744 ) ;
#45671 = DIRECTION ( 'NONE',  ( 0.000000000000000000, -1.000000000000000000, 0.000000000000000000 ) ) ;
#45672 = VERTEX_POINT ( 'NONE', #44398 ) ;
#45673 = EDGE_CURVE ( 'NONE', #103418, #57341, #66139, .T. ) ;
#45675 = EDGE_LOOP ( 'NONE', ( #56305, #51589, #114979, #56302 ) ) ;
#45674 = DIRECTION ( 'NONE',  ( 0.6830127018922180770, -0.6830127018922204085, -0.2588190451025213501 ) ) ;
#45676 = VERTEX_POINT ( 'NONE', #99429 ) ;
#45677 = EDGE_CURVE ( 'NONE', #109576, #15478, #24746, .T. ) ;
#45678 = LINE ( 'NONE', #110164, #84061 ) ;
#45680 = AXIS2_PLACEMENT_3D ( 'NONE', #13464, #104042, #136693 ) ;
#45679 = LINE ( 'NONE', #43503, #80826 ) ;
#45681 = VERTEX_POINT ( 'NONE', #13845 ) ;
#45682 = EDGE_CURVE ( 'NONE', #14544, #41659, #21890, .T. ) ;
#45683 = CARTESIAN_POINT ( 'NONE',  ( 9.183988606268997046, 28.73617430169793607, 5.000000000000000000 ) ) ;
#45684 = LINE ( 'NONE', #114459, #143431 ) ;
#45685 = VECTOR ( 'NONE', #66256, 999.9999999999998863 ) ;
#45686 = CARTESIAN_POINT ( 'NONE',  ( 11.81601139373100651, 28.73617430169779041, 5.000000000000000000 ) ) ;
#45687 = DIRECTION ( 'NONE',  ( 0.7071067811865487940, -0.7071067811865463515, -0.000000000000000000 ) ) ;
#45688 = CARTESIAN_POINT ( 'NONE',  ( 34.92499999999998295, 5.718490437204210686, 4.759050581649325373 ) ) ;
#45689 = LINE ( 'NONE', #66012, #97685 ) ;
#45690 = DIRECTION ( 'NONE',  ( -0.000000000000000000, 0.3543493200069153248, 0.9351131265310292928 ) ) ;
#45691 = DIRECTION ( 'NONE',  ( 0.7071067811865486830, -0.7071067811865464625, -0.000000000000000000 ) ) ;
#45692 = CARTESIAN_POINT ( 'NONE',  ( 24.91623647476855652, -7.934999999999990727, 4.858786175617117713E-16 ) ) ;
#45694 = CONICAL_SURFACE ( 'NONE', #64193, 2.500000000000000888, 0.9599310885968822538 ) ;
#45693 = CARTESIAN_POINT ( 'NONE',  ( 2.749569808101886004, 3.967499999999998916, 6.871911579029510442 ) ) ;
#45695 = DIRECTION ( 'NONE',  ( -0.000000000000000000, 0.000000000000000000, 1.000000000000000000 ) ) ;
#45696 = CARTESIAN_POINT ( 'NONE',  ( 109.6458333333333286, 2.130196079827431976, -7.949999999999998401 ) ) ;
#45697 = FACE_OUTER_BOUND ( 'NONE', #54491, .T. ) ;
#45698 = VERTEX_POINT ( 'NONE', #68992 ) ;
#45699 = ORIENTED_EDGE ( 'NONE', *, *, #96121, .F. ) ;
#45700 = CARTESIAN_POINT ( 'NONE',  ( 106.0000000000000000, 0.000000000000000000, -7.950000000000000178 ) ) ;
#45701 = EDGE_LOOP ( 'NONE', ( #53530, #33993, #80741, #138084 ) ) ;
#45702 = ORIENTED_EDGE ( 'NONE', *, *, #138003, .F. ) ;
#45703 = ORIENTED_EDGE ( 'NONE', *, *, #31052, .T. ) ;
#45704 = EDGE_CURVE ( 'NONE', #130345, #61667, #100184, .T. ) ;
#45705 = PLANE ( 'NONE',  #119725 ) ;
#45706 = DIRECTION ( 'NONE',  ( 0.6830127018922181881, 0.6830127018922202975, -0.2588190451025214056 ) ) ;
#45707 = DIRECTION ( 'NONE',  ( 0.7071067811865487940, -0.7071067811865463515, 0.000000000000000000 ) ) ;
#45708 = ORIENTED_EDGE ( 'NONE', *, *, #20213, .F. ) ;
#45709 = CARTESIAN_POINT ( 'NONE',  ( -33.48921356237309510, -27.52281430457078670, 5.000000000000000000 ) ) ;
#45710 = DIRECTION ( 'NONE',  ( -0.3543493200069162685, -0.000000000000000000, -0.9351131265310288487 ) ) ;
#45712 = VECTOR ( 'NONE', #49866, 1000.000000000000114 ) ;
#45711 = DIRECTION ( 'NONE',  ( -0.000000000000000000, 0.000000000000000000, 1.000000000000000000 ) ) ;
#45713 = CARTESIAN_POINT ( 'NONE',  ( -7.499999999999951150, 1.030536316426505117, -5.498701923753780640 ) ) ;
#45714 = ORIENTED_EDGE ( 'NONE', *, *, #99183, .F. ) ;
#45715 = DIRECTION ( 'NONE',  ( -0.7071067811865486830, -0.7071067811865464625, 0.000000000000000000 ) ) ;
#45716 = DIRECTION ( 'NONE',  ( 0.7071067811865486830, -0.7071067811865464625, -0.000000000000000000 ) ) ;
#45717 = DIRECTION ( 'NONE',  ( -0.000000000000000000, 0.3543493200069153248, 0.9351131265310292928 ) ) ;
#45718 = CARTESIAN_POINT ( 'NONE',  ( 4.898587196589412829E-16, -8.616843969807042924, -4.000000000000000000 ) ) ;
#45719 = CYLINDRICAL_SURFACE ( 'NONE', #73075, 2.500000000000000444 ) ;
#45720 = LINE ( 'NONE', #57310, #33085 ) ;
#45721 = DIRECTION ( 'NONE',  ( 0.7071067811865486830, -0.7071067811865464625, -0.000000000000000000 ) ) ;
#45722 = CARTESIAN_POINT ( 'NONE',  ( 5.007369047664765205, 22.22500000000000142, -10.13186738250296592 ) ) ;
#45723 = EDGE_CURVE ( 'NONE', #123521, #81380, #45816, .T. ) ;
#45724 = DIRECTION ( 'NONE',  ( 0.000000000000000000, -0.3543493200069153248, -0.9351131265310291818 ) ) ;
#45725 = ORIENTED_EDGE ( 'NONE', *, *, #62000, .T. ) ;
#45726 = ORIENTED_EDGE ( 'NONE', *, *, #94664, .T. ) ;
#45727 = CARTESIAN_POINT ( 'NONE',  ( 118.7087635252314328, -7.482591942790329030E-16, 6.110000000000001208 ) ) ;
#45728 = CIRCLE ( 'NONE', #73435, 1.000000000000000888 ) ;
#45729 = AXIS2_PLACEMENT_3D ( 'NONE', #84055, #128253, #73168 ) ;
#45730 = ORIENTED_EDGE ( 'NONE', *, *, #5304, .F. ) ;
#45731 = ADVANCED_FACE ( 'NONE', ( #46559 ), #68305, .F. ) ;
#45732 = CARTESIAN_POINT ( 'NONE',  ( 100.6041666666666572, 2.130196079827384459, 7.950000000000025047 ) ) ;
#45733 = CARTESIAN_POINT ( 'NONE',  ( 34.49999999999976552, -13.91253812416061386, 4.000000000000000000 ) ) ;
#45734 = CARTESIAN_POINT ( 'NONE',  ( -45.18398860626900415, 28.73617430169818832, 5.000000000000000000 ) ) ;
#45735 = DIRECTION ( 'NONE',  ( 0.7071067811865487940, 0.7071067811865463515, 0.000000000000000000 ) ) ;
#45736 = CARTESIAN_POINT ( 'NONE',  ( 114.6829301918980946, -1.637169565754158951, -6.109999999999998543 ) ) ;
#45737 = ORIENTED_EDGE ( 'NONE', *, *, #130130, .T. ) ;
#45738 = EDGE_CURVE ( 'NONE', #28591, #123227, #134975, .T. ) ;
#45739 = ORIENTED_EDGE ( 'NONE', *, *, #3217, .F. ) ;
#45740 = LINE ( 'NONE', #102252, #45559 ) ;
#45741 = ORIENTED_EDGE ( 'NONE', *, *, #58155, .F. ) ;
#45742 = VERTEX_POINT ( 'NONE', #1533 ) ;
#45743 = VECTOR ( 'NONE', #25032, 1000.000000000000227 ) ;
#45744 = CARTESIAN_POINT ( 'NONE',  ( 35.29209685856476852, -5.291415217122921177, 3.054999999999999272 ) ) ;
#45745 = EDGE_CURVE ( 'NONE', #11327, #94854, #101584, .T. ) ;
#45746 = VERTEX_POINT ( 'NONE', #79176 ) ;
#45747 = CARTESIAN_POINT ( 'NONE',  ( 0.000000000000000000, -21.72500000000000142, 4.500000000000000888 ) ) ;
#45748 = EDGE_CURVE ( 'NONE', #140981, #64204, #132888, .T. ) ;
#45749 = APPLICATION_CONTEXT ( 'automotive_design' ) ;
#45750 = CARTESIAN_POINT ( 'NONE',  ( 3.712903141435219379, 3.967499999999992699, -6.871911579029513994 ) ) ;
#45751 = VECTOR ( 'NONE', #90514, 999.9999999999998863 ) ;
#45752 = VECTOR ( 'NONE', #76787, 1000.000000000000000 ) ;
#45753 = AXIS2_PLACEMENT_3D ( 'NONE', #30555, #50165, #28411 ) ;
#45754 = CARTESIAN_POINT ( 'NONE',  ( 28.05793019189811233, 6.110000000000000320, -1.637169565754156064 ) ) ;
#45755 = ORIENTED_EDGE ( 'NONE', *, *, #34171, .F. ) ;
#45756 = LINE ( 'NONE', #20379, #89585 ) ;
#45757 = ORIENTED_EDGE ( 'NONE', *, *, #35692, .F. ) ;
#45758 = ORIENTED_EDGE ( 'NONE', *, *, #32380, .F. ) ;
#45759 = AXIS2_PLACEMENT_3D ( 'NONE', #86735, #64258, #108423 ) ;
#45760 = ORIENTED_EDGE ( 'NONE', *, *, #116995, .F. ) ;
#45761 = CYLINDRICAL_SURFACE ( 'NONE', #61410, 1.000000000000000888 ) ;
#45762 = DIRECTION ( 'NONE',  ( -1.000000000000000000, -1.192622389734054877E-16, 0.000000000000000000 ) ) ;
#45763 = ADVANCED_FACE ( 'NONE', ( #77721 ), #90747, .F. ) ;
#45764 = ORIENTED_EDGE ( 'NONE', *, *, #83500, .T. ) ;
#45765 = DIRECTION ( 'NONE',  ( 0.7071067811865487940, 0.7071067811865463515, 0.000000000000000000 ) ) ;
#45766 = EDGE_CURVE ( 'NONE', #108133, #39160, #24045, .T. ) ;
#45767 = DIRECTION ( 'NONE',  ( -0.7071067811865487940, 0.7071067811865463515, -0.000000000000000000 ) ) ;
#45768 = SURFACE_SIDE_STYLE ('',( #132048 ) ) ;
#45769 = CARTESIAN_POINT ( 'NONE',  ( -29.99999999999979039, 10.55218569542906515, 5.000000000000000000 ) ) ;
#45770 = EDGE_CURVE ( 'NONE', #95348, #2907, #45122, .T. ) ;
#45771 = FACE_BOUND ( 'NONE', #31703, .T. ) ;
#45772 = EDGE_LOOP ( 'NONE', ( #91944, #71207, #25325, #124038 ) ) ;
#45773 = CARTESIAN_POINT ( 'NONE',  ( 0.4368010322082955810, -12.74070752338415247, 9.898150129686374754 ) ) ;
#45774 = CARTESIAN_POINT ( 'NONE',  ( -48.18398860626899705, 28.73617430169820608, 5.000000000000000000 ) ) ;
#45775 = DIRECTION ( 'NONE',  ( 0.000000000000000000, -1.000000000000000000, 0.000000000000000000 ) ) ;
#45777 = EDGE_CURVE ( 'NONE', #131756, #141782, #33520, .T. ) ;
#45776 = PLANE ( 'NONE',  #60128 ) ;
#45778 = ORIENTED_EDGE ( 'NONE', *, *, #80473, .T. ) ;
#45779 = DIRECTION ( 'NONE',  ( 0.7071067811865487940, 0.7071067811865463515, -0.000000000000000000 ) ) ;
#45780 = ORIENTED_EDGE ( 'NONE', *, *, #36466, .T. ) ;
#45781 = VECTOR ( 'NONE', #101760, 1000.000000000000000 ) ;
#45782 = EDGE_LOOP ( 'NONE', ( #127325, #71299, #64164, #16160 ) ) ;
#45783 = ORIENTED_EDGE ( 'NONE', *, *, #71746, .T. ) ;
#45784 = CARTESIAN_POINT ( 'NONE',  ( 48.32876352523145158, 0.000000000000000000, -6.109999999999998543 ) ) ;
#45785 = AXIS2_PLACEMENT_3D ( 'NONE', #4924, #28162, #136200 ) ;
#45786 = ORIENTED_EDGE ( 'NONE', *, *, #128627, .F. ) ;
#45787 = CARTESIAN_POINT ( 'NONE',  ( -42.18398860626899705, 28.73617430169816700, 5.000000000000000000 ) ) ;
#45788 = DIRECTION ( 'NONE',  ( 1.369518533665900312E-16, -1.000000000000000000, 0.000000000000000000 ) ) ;
#45789 = EDGE_LOOP ( 'NONE', ( #43456, #118962, #59201, #107713 ) ) ;
#45790 = EDGE_CURVE ( 'NONE', #69258, #129048, #66837, .T. ) ;
#45791 =( BOUNDED_CURVE ( )  B_SPLINE_CURVE ( 2, ( #124227, #1688, #13298, #48826, #103181, #79348, #123547, #27049, #113331, #37218, #24211, #114749, #124934 ),
 .UNSPECIFIED., .F., .F. ) 
 B_SPLINE_CURVE_WITH_KNOTS ( ( 3, 2, 2, 2, 2, 2, 3 ),
 ( 0.8166666666666666519, 0.8194444444444444198, 0.8222222222222221877, 0.8249999999999999556, 0.8277777777777777235, 0.8305555555555556024, 0.8333333333333333703 ),
 .UNSPECIFIED. ) 
 CURVE ( )  GEOMETRIC_REPRESENTATION_ITEM ( )  RATIONAL_B_SPLINE_CURVE ( ( 1.000000000000000000, 0.9659258262890683122, 1.000000000000000000, 0.9659258262890683122, 1.000000000000000000, 0.9659258262890683122, 1.000000000000000000, 0.9659258262890683122, 1.000000000000000000, 0.9659258262890683122, 1.000000000000000000, 0.9659258262890683122, 1.000000000000000000 ) ) 
 REPRESENTATION_ITEM ( '' )  );
#45792 = LINE ( 'NONE', #68969, #59780 ) ;
#45793 = CARTESIAN_POINT ( 'NONE',  ( 27.51665438641025219, 22.22500000000000142, 4.500000000000000888 ) ) ;
#45794 = CARTESIAN_POINT ( 'NONE',  ( 11.51078643762690490, -27.52281430457047406, 5.000000000000000000 ) ) ;
#45795 = ORIENTED_EDGE ( 'NONE', *, *, #141042, .T. ) ;
#45796 = ORIENTED_EDGE ( 'NONE', *, *, #135121, .F. ) ;
#45797 = VERTEX_POINT ( 'NONE', #121196 ) ;
#45798 = ORIENTED_EDGE ( 'NONE', *, *, #134438, .F. ) ;
#45799 = CARTESIAN_POINT ( 'NONE',  ( 24.00548008471250938, 28.92564299267921513, 4.000000000000000000 ) ) ;
#45800 = VERTEX_POINT ( 'NONE', #34210 ) ;
#45801 = ORIENTED_EDGE ( 'NONE', *, *, #921, .T. ) ;
#45802 =( LENGTH_UNIT ( ) NAMED_UNIT ( * ) SI_UNIT ( .MILLI., .METRE. ) );
#45803 = LINE ( 'NONE', #100865, #43946 ) ;
#45804 = VERTEX_POINT ( 'NONE', #22570 ) ;
#45805 = CARTESIAN_POINT ( 'NONE',  ( -6.489213562373093325, -27.52281430457059841, 5.000000000000000000 ) ) ;
#45806 = DIRECTION ( 'NONE',  ( -0.7071067811865486830, -0.7071067811865464625, 0.000000000000000000 ) ) ;
#45807 = CARTESIAN_POINT ( 'NONE',  ( 26.60873647476855552, -5.808823158059033709, 5.808823158059035485 ) ) ;
#45808 = EDGE_CURVE ( 'NONE', #48333, #54912, #10982, .T. ) ;
#45809 = FILL_AREA_STYLE ('',( #12428 ) ) ;
#45810 = ORIENTED_EDGE ( 'NONE', *, *, #33335, .T. ) ;
#45811 = CARTESIAN_POINT ( 'NONE',  ( 113.0787635252314516, -7.482591942790327058E-16, 6.109999999999999432 ) ) ;
#45812 = VECTOR ( 'NONE', #136672, 1000.000000000000000 ) ;
#45813 = EDGE_CURVE ( 'NONE', #89147, #29105, #56718, .T. ) ;
#45814 = CARTESIAN_POINT ( 'NONE',  ( 3.489213562373097322, -27.52281430457057709, 5.000000000000000000 ) ) ;
#45815 = CARTESIAN_POINT ( 'NONE',  ( 26.99999999999981526, -6.033600742197678279, 5.000000000000000000 ) ) ;
#45816 = LINE ( 'NONE', #23296, #70401 ) ;
#45818 = VERTEX_POINT ( 'NONE', #100879 ) ;
#45817 = DIRECTION ( 'NONE',  ( -0.7071067811865487940, 0.7071067811865463515, -0.000000000000000000 ) ) ;
#45819 = LINE ( 'NONE', #68308, #13785 ) ;
#45820 = EDGE_LOOP ( 'NONE', ( #101466, #143115, #60997, #89371 ) ) ;
#45821 = LINE ( 'NONE', #55990, #105233 ) ;
#45822 = DIRECTION ( 'NONE',  ( -0.7071067811865486830, 0.7071067811865464625, 0.000000000000000000 ) ) ;
#45823 = ADVANCED_FACE ( 'NONE', ( #111770 ), #50091, .F. ) ;
#45824 = EDGE_CURVE ( 'NONE', #19198, #2249, #49399, .T. ) ;
#45825 = CARTESIAN_POINT ( 'NONE',  ( 1.500000000000000000, 0.000000000000000000, 0.000000000000000000 ) ) ;
#45826 = ORIENTED_EDGE ( 'NONE', *, *, #69367, .F. ) ;
#45827 = PLANE ( 'NONE',  #18123 ) ;
#45828 = VECTOR ( 'NONE', #48722, 999.9999999999998863 ) ;
#45829 = LINE ( 'NONE', #99441, #14110 ) ;
#45830 = LINE ( 'NONE', #77034, #56036 ) ;
#45831 = ORIENTED_EDGE ( 'NONE', *, *, #23726, .F. ) ;
#45832 = VECTOR ( 'NONE', #39569, 999.9999999999998863 ) ;
#45833 = DIRECTION ( 'NONE',  ( -0.000000000000000000, 0.3543493200069153248, 0.9351131265310292928 ) ) ;
#45834 = ORIENTED_EDGE ( 'NONE', *, *, #128356, .F. ) ;
#45835 = CIRCLE ( 'NONE', #101370, 6.094999999999989093 ) ;
#45836 = ADVANCED_FACE ( 'NONE', ( #16726 ), #61004, .F. ) ;
#45837 = CARTESIAN_POINT ( 'NONE',  ( 36.48921356237310221, -27.52281430457080802, 5.000000000000000000 ) ) ;
#45839 = ORIENTED_EDGE ( 'NONE', *, *, #103346, .F. ) ;
#45838 = CARTESIAN_POINT ( 'NONE',  ( -17.99999999999986855, -22.06887692260758271, 4.000000000000000000 ) ) ;
#45840 = EDGE_CURVE ( 'NONE', #142336, #21645, #124776, .T. ) ;
#45841 = EDGE_LOOP ( 'NONE', ( #104120, #30803, #37032, #80737 ) ) ;
#45842 = CARTESIAN_POINT ( 'NONE',  ( -8.534745106696862769E-17, 0.000000000000000000, 0.000000000000000000 ) ) ;
#45843 = LINE ( 'NONE', #66161, #119987 ) ;
#45844 = VECTOR ( 'NONE', #135805, 1000.000000000000000 ) ;
#45845 = ORIENTED_EDGE ( 'NONE', *, *, #16833, .F. ) ;
#45846 = VECTOR ( 'NONE', #93536, 1000.000000000000000 ) ;
#45847 = ADVANCED_FACE ( 'NONE', ( #47968 ), #116022, .T. ) ;
#45848 = DIRECTION ( 'NONE',  ( -0.7071067811865487940, 0.7071067811865463515, -0.000000000000000000 ) ) ;
#45849 = CARTESIAN_POINT ( 'NONE',  ( -12.79289321881336861, -5.240707523384230626, 5.000000000000000000 ) ) ;
#45850 = ORIENTED_EDGE ( 'NONE', *, *, #116671, .T. ) ;
#45851 = LINE ( 'NONE', #89329, #48957 ) ;
#45852 = CARTESIAN_POINT ( 'NONE',  ( 34.49999999999976552, 7.464255608400424791, 4.994342998332163219 ) ) ;
#45853 = DIRECTION ( 'NONE',  ( 0.7071067811865487940, 0.7071067811865463515, 0.000000000000000000 ) ) ;
#45854 = ADVANCED_FACE ( 'NONE', ( #80582 ), #84355, .T. ) ;
#45855 = PLANE ( 'NONE',  #77148 ) ;
#45856 = CARTESIAN_POINT ( 'NONE',  ( -34.60428828362105236, 22.19175015946030882, 4.000000000000000000 ) ) ;
#45857 = CARTESIAN_POINT ( 'NONE',  ( 0.000000000000000000, 0.000000000000000000, 0.000000000000000000 ) ) ;
#45858 = VERTEX_POINT ( 'NONE', #136360 ) ;
#45859 = ORIENTED_EDGE ( 'NONE', *, *, #46794, .F. ) ;
#45860 = ORIENTED_EDGE ( 'NONE', *, *, #115687, .F. ) ;
#45861 = CARTESIAN_POINT ( 'NONE',  ( -30.29974487139158867, -27.71228299555227537, 4.000000000000000000 ) ) ;
#45862 = ORIENTED_EDGE ( 'NONE', *, *, #85471, .F. ) ;
#45863 = ORIENTED_EDGE ( 'NONE', *, *, #115572, .F. ) ;
#45864 = ORIENTED_EDGE ( 'NONE', *, *, #120732, .T. ) ;
#45865 = EDGE_CURVE ( 'NONE', #104944, #47327, #83431, .T. ) ;
#45866 = DIRECTION ( 'NONE',  ( -0.3543493200069162685, -0.000000000000000000, -0.9351131265310288487 ) ) ;
#45867 = CARTESIAN_POINT ( 'NONE',  ( -33.48921356237309510, -27.52281430457078670, 5.000000000000000000 ) ) ;
#45868 = ORIENTED_EDGE ( 'NONE', *, *, #80379, .T. ) ;
#45869 = CARTESIAN_POINT ( 'NONE',  ( 15.18079593298623564, -2.055000000000000160, 2.789133085058097101E-16 ) ) ;
#45870 = DIRECTION ( 'NONE',  ( -0.000000000000000000, -0.3543493200069152693, 0.9351131265310292928 ) ) ;
#45871 = PLANE ( 'NONE',  #122741 ) ;
#45872 = CARTESIAN_POINT ( 'NONE',  ( 19.49999999999987210, 21.05218569542895679, 5.000000000000000000 ) ) ;
#45873 = CARTESIAN_POINT ( 'NONE',  ( 117.5420968585647756, 5.291415217122923842, -3.054999999999996163 ) ) ;
#45874 = ORIENTED_EDGE ( 'NONE', *, *, #75552, .F. ) ;
#45875 = EDGE_CURVE ( 'NONE', #45317, #22333, #38493, .T. ) ;
#45876 = LINE ( 'NONE', #133585, #55781 ) ;
#45877 = CARTESIAN_POINT ( 'NONE',  ( 14.29298673570684919, -21.74070752338406365, 4.999753212805221558 ) ) ;
#45878 = VECTOR ( 'NONE', #29693, 1000.000000000000000 ) ;
#45879 = CARTESIAN_POINT ( 'NONE',  ( 12.66846741159848655, -18.74070752338408852, 20.73178291233844206 ) ) ;
#45880 = CARTESIAN_POINT ( 'NONE',  ( 1.274578247585341995, 1.447108250109749417, 6.668332787597689659 ) ) ;
#45881 = DIRECTION ( 'NONE',  ( 0.7071067811865487940, 0.7071067811865463515, 0.000000000000000000 ) ) ;
#45882 = LINE ( 'NONE', #133591, #23721 ) ;
#45883 = DIRECTION ( 'NONE',  ( -0.6830127018922180770, -0.6830127018922204085, -0.2588190451025213501 ) ) ;
#45884 = CARTESIAN_POINT ( 'NONE',  ( 45.14169371712955581, -2.130196079827424871, -7.949999999999999289 ) ) ;
#45885 = ADVANCED_FACE ( 'NONE', ( #27590 ), #104438, .F. ) ;
#45886 = CARTESIAN_POINT ( 'NONE',  ( 12.48921356237309155, -27.52281430457064104, 5.000000000000000000 ) ) ;
#45887 = CARTESIAN_POINT ( 'NONE',  ( 48.18398860626899705, 28.73617430169820608, 5.000000000000000000 ) ) ;
#45888 = ORIENTED_EDGE ( 'NONE', *, *, #108913, .F. ) ;
#45889 = ORIENTED_EDGE ( 'NONE', *, *, #78473, .F. ) ;
#45890 = CARTESIAN_POINT ( 'NONE',  ( 46.35416666666666430, -2.130196079827425315, -7.950000000000001066 ) ) ;
#45891 = CARTESIAN_POINT ( 'NONE',  ( -34.49999999999975842, -10.53574439159939757, 4.994342998332166772 ) ) ;
#45892 = ORIENTED_EDGE ( 'NONE', *, *, #49283, .F. ) ;
#45893 = CARTESIAN_POINT ( 'NONE',  ( 24.18398860626899705, 28.73617430169804265, 5.000000000000000000 ) ) ;
#45895 = AXIS2_PLACEMENT_3D ( 'NONE', #58364, #122849, #79396 ) ;
#45894 = CARTESIAN_POINT ( 'NONE',  ( -2.700255128608413990, -27.71228299555204089, 4.000000000000000000 ) ) ;
#45896 = CARTESIAN_POINT ( 'NONE',  ( 41.56293019189811133, 1.637169565754157174, 6.110000000000002984 ) ) ;
#45897 = ORIENTED_EDGE ( 'NONE', *, *, #1571, .T. ) ;
#45898 = CARTESIAN_POINT ( 'NONE',  ( 16.82816939922340183, -20.24070752338408852, 4.000000000000000000 ) ) ;
#45899 = ORIENTED_EDGE ( 'NONE', *, *, #109914, .F. ) ;
#45900 = CARTESIAN_POINT ( 'NONE',  ( 36.48921356237310221, -27.52281430457080802, 5.000000000000000000 ) ) ;
#45901 = PLANE ( 'NONE',  #100871 ) ;
#45902 = CARTESIAN_POINT ( 'NONE',  ( 10.73493329717942224, 12.75929247661558286, 18.34774599283953833 ) ) ;
#45903 = FACE_OUTER_BOUND ( 'NONE', #118897, .T. ) ;
#45904 = ORIENTED_EDGE ( 'NONE', *, *, #13836, .F. ) ;
#45905 = PLANE ( 'NONE',  #53484 ) ;
#45906 = EDGE_CURVE ( 'NONE', #100067, #116077, #138518, .T. ) ;
#45907 = ORIENTED_EDGE ( 'NONE', *, *, #29937, .T. ) ;
#45908 = CARTESIAN_POINT ( 'NONE',  ( 40.03752705046288440, -9.735942053221456900E-16, 7.949999999999998401 ) ) ;
#45909 = FACE_OUTER_BOUND ( 'NONE', #131081, .T. ) ;
#45910 = DIRECTION ( 'NONE',  ( -0.7071067811865486830, -0.7071067811865464625, 0.000000000000000000 ) ) ;
#45911 = FACE_OUTER_BOUND ( 'NONE', #111371, .T. ) ;
#45912 = LINE ( 'NONE', #90096, #115704 ) ;
#45913 = CARTESIAN_POINT ( 'NONE',  ( 33.29974487139158867, -27.71228299555229313, 4.000000000000000000 ) ) ;
#45914 = EDGE_LOOP ( 'NONE', ( #43527, #128009, #1470, #32141 ) ) ;
#45915 = VECTOR ( 'NONE', #4498, 1000.000000000000000 ) ;
#45916 = LINE ( 'NONE', #87970, #124035 ) ;
#45917 = CARTESIAN_POINT ( 'NONE',  ( 59.55793019189812298, 6.110000000000000320, -1.637169565754156064 ) ) ;
#45918 = MANIFOLD_SOLID_BREP ( 'Mirror1', #23189 ) ;
#45919 = CARTESIAN_POINT ( 'NONE',  ( 32.99451991528749062, 28.92564299267960948, 4.000000000000000000 ) ) ;
#45920 = LINE ( 'NONE', #90103, #43149 ) ;
#45922 = ORIENTED_EDGE ( 'NONE', *, *, #96316, .F. ) ;
#45921 = CARTESIAN_POINT ( 'NONE',  ( -62.99451991528749772, 28.92564299267982264, 4.000000000000000000 ) ) ;
#45923 = ORIENTED_EDGE ( 'NONE', *, *, #74281, .F. ) ;
#45924 = CARTESIAN_POINT ( 'NONE',  ( 1.554198618961949441, -0.3999999999999997446, -2.412907390626681359 ) ) ;
#45925 = ORIENTED_EDGE ( 'NONE', *, *, #56811, .T. ) ;
#45926 = CARTESIAN_POINT ( 'NONE',  ( 34.92500000000001137, 22.27000000000000668, -7.752744394707098863 ) ) ;
#45927 = EDGE_LOOP ( 'NONE', ( #78348, #73859, #77452, #10717 ) ) ;
#45928 = DIRECTION ( 'NONE',  ( 1.192622389734054877E-16, -1.000000000000000000, 0.000000000000000000 ) ) ;
#45929 = CARTESIAN_POINT ( 'NONE',  ( -24.18398860626899705, 28.73617430169804265, 5.000000000000000000 ) ) ;
#45930 = CARTESIAN_POINT ( 'NONE',  ( 34.92382263987068569, 21.75929247661549937, 4.252424926123345550 ) ) ;
#45931 = STYLED_ITEM ( 'NONE', ( #126375 ), #125643 ) ;
#45932 = CARTESIAN_POINT ( 'NONE',  ( 0.7307956238753654521, 0.3999999999999995226, 2.467792535850613866 ) ) ;
#45933 = VECTOR ( 'NONE', #40074, 1000.000000000000000 ) ;
#45934 = EDGE_CURVE ( 'NONE', #9641, #16, #48655, .T. ) ;
#45935 = FACE_BOUND ( 'NONE', #124543, .T. ) ;
#45936 = LINE ( 'NONE', #79309, #47989 ) ;
#45937 = CARTESIAN_POINT ( 'NONE',  ( 39.18398860626899705, 28.73617430169814568, 5.000000000000000000 ) ) ;
#45939 = ADVANCED_FACE ( 'NONE', ( #82030 ), #126213, .F. ) ;
#45938 = DIRECTION ( 'NONE',  ( -0.7071067811865487940, 0.7071067811865463515, 0.000000000000000000 ) ) ;
#45940 = LINE ( 'NONE', #88732, #133685 ) ;
#45942 = EDGE_LOOP ( 'NONE', ( #23180, #48254, #70109, #54846 ) ) ;
#45941 = FACE_OUTER_BOUND ( 'NONE', #86823, .T. ) ;
#45943 = VECTOR ( 'NONE', #81271, 1000.000000000000000 ) ;
#45944 = CIRCLE ( 'NONE', #129206, 4.582731094065999322 ) ;
#45945 = PLANE ( 'NONE',  #69579 ) ;
#45946 = ORIENTED_EDGE ( 'NONE', *, *, #44329, .T. ) ;
#45947 = ORIENTED_EDGE ( 'NONE', *, *, #12926, .F. ) ;
#45948 = CARTESIAN_POINT ( 'NONE',  ( 75.59959685856478018, -6.109999999999997655, -1.637169565754160283 ) ) ;
#45949 = ORIENTED_EDGE ( 'NONE', *, *, #54951, .F. ) ;
#45950 = CARTESIAN_POINT ( 'NONE',  ( -27.48921356237309155, -27.52281430457074762, 5.000000000000000000 ) ) ;
#45951 =( BOUNDED_CURVE ( )  B_SPLINE_CURVE ( 3, ( #107289, #7961, #96388, #140626 ),
 .UNSPECIFIED., .F., .T. ) 
 B_SPLINE_CURVE_WITH_KNOTS ( ( 4, 4 ),
 ( 1.964434688349487867, 3.503810798801452187 ),
 .UNSPECIFIED. ) 
 CURVE ( )  GEOMETRIC_REPRESENTATION_ITEM ( )  RATIONAL_B_SPLINE_CURVE ( ( 1.000000000000000000, 0.8120851936182279518, 0.8120851936182279518, 1.000000000000000000 ) ) 
 REPRESENTATION_ITEM ( '' )  );
#45952 = EDGE_CURVE ( 'NONE', #17180, #81879, #139965, .T. ) ;
#45953 = CARTESIAN_POINT ( 'NONE',  ( -30.18398860626900060, 28.73617430169808173, 5.000000000000000000 ) ) ;
#45954 = VERTEX_POINT ( 'NONE', #95713 ) ;
#45955 = DIRECTION ( 'NONE',  ( 0.6830127018922180770, -0.6830127018922204085, -0.2588190451025213501 ) ) ;
#45956 = VECTOR ( 'NONE', #96582, 1000.000000000000000 ) ;
#45957 = ADVANCED_FACE ( 'NONE', ( #84167 ), #52895, .F. ) ;
#45958 = DIRECTION ( 'NONE',  ( -0.000000000000000000, -0.3543493200069152693, 0.9351131265310292928 ) ) ;
#45959 = VECTOR ( 'NONE', #25140, 1000.000000000000227 ) ;
#45960 = DIRECTION ( 'NONE',  ( -0.000000000000000000, 0.000000000000000000, 1.000000000000000000 ) ) ;
#45961 = CARTESIAN_POINT ( 'NONE',  ( 1.592112687295236917, 0.3999999999999995226, 2.358007167714498475 ) ) ;
#45963 = DIRECTION ( 'NONE',  ( -0.6830127018922180770, -0.6830127018922204085, -0.2588190451025213501 ) ) ;
#45962 = CARTESIAN_POINT ( 'NONE',  ( -11.29289321881337038, 2.259292476615690770, 5.000000000000000000 ) ) ;
#45964 = DIRECTION ( 'NONE',  ( 0.7071067811865487940, 0.7071067811865463515, 0.000000000000000000 ) ) ;
#45965 = CARTESIAN_POINT ( 'NONE',  ( -30.18398860626900060, 28.73617430169808173, 5.000000000000000000 ) ) ;
#45966 = VERTEX_POINT ( 'NONE', #20278 ) ;
#45967 = VECTOR ( 'NONE', #86695, 1000.000000000000000 ) ;
#45968 = EDGE_CURVE ( 'NONE', #100698, #107938, #29038, .T. ) ;
#45969 = ORIENTED_EDGE ( 'NONE', *, *, #5579, .F. ) ;
#45970 = LINE ( 'NONE', #55407, #47302 ) ;
#45971 = FACE_OUTER_BOUND ( 'NONE', #69733, .T. ) ;
#45972 = ORIENTED_EDGE ( 'NONE', *, *, #122528, .F. ) ;
#45973 = VECTOR ( 'NONE', #96586, 1000.000000000000000 ) ;
#45974 = EDGE_LOOP ( 'NONE', ( #45397, #105567, #25291, #44763 ) ) ;
#45975 = CIRCLE ( 'NONE', #89914, 2.500000000000000888 ) ;
#45976 = VERTEX_POINT ( 'NONE', #42074 ) ;
#45977 = CARTESIAN_POINT ( 'NONE',  ( 25.52126352523142927, -4.472830434245838482, -4.472830434245840259 ) ) ;
#45978 = ORIENTED_EDGE ( 'NONE', *, *, #4183, .T. ) ;
#45979 = CARTESIAN_POINT ( 'NONE',  ( 59.99451991528749772, 28.92564299267980132, 4.000000000000000000 ) ) ;
#45980 =( BOUNDED_CURVE ( )  B_SPLINE_CURVE ( 3, ( #89298, #111767, #134972, #35671 ),
 .UNSPECIFIED., .F., .T. ) 
 B_SPLINE_CURVE_WITH_KNOTS ( ( 4, 4 ),
 ( 1.208578181583240374, 1.359146454359417167 ),
 .UNSPECIFIED. ) 
 CURVE ( )  GEOMETRIC_REPRESENTATION_ITEM ( )  RATIONAL_B_SPLINE_CURVE ( ( 1.000000000000000000, 0.9981116584018959736, 0.9981116584018959736, 1.000000000000000000 ) ) 
 REPRESENTATION_ITEM ( '' )  );
#45981 = CARTESIAN_POINT ( 'NONE',  ( 0.5045698081018860082, 6.871911579029510442, -3.967499999999998916 ) ) ;
#45982 = LINE ( 'NONE', #134410, #58862 ) ;
#45983 = VERTEX_POINT ( 'NONE', #53658 ) ;
#45984 = CARTESIAN_POINT ( 'NONE',  ( -25.49999999999982236, -17.91344420646044711, 1.358650452708403567 ) ) ;
#45985 = ADVANCED_FACE ( 'NONE', ( #97099 ), #98196, .T. ) ;
#45986 = CARTESIAN_POINT ( 'NONE',  ( 26.99999999999981171, -8.731860332648819778, -2.120594902707474638 ) ) ;
#45987 = DIRECTION ( 'NONE',  ( -0.6830127018922180770, -0.6830127018922204085, -0.2588190451025213501 ) ) ;
#45988 = VECTOR ( 'NONE', #100694, 1000.000000000000227 ) ;
#45990 = ORIENTED_EDGE ( 'NONE', *, *, #60366, .F. ) ;
#45989 = PLANE ( 'NONE',  #79499 ) ;
#45991 = ORIENTED_EDGE ( 'NONE', *, *, #102283, .F. ) ;
#45992 = CARTESIAN_POINT ( 'NONE',  ( -15.29974487139158867, -27.71228299555216879, 4.000000000000000000 ) ) ;
#45993 = CARTESIAN_POINT ( 'NONE',  ( 27.70710678118635428, -0.7407075233842701500, 5.000000000000000000 ) ) ;
#45995 = EDGE_CURVE ( 'NONE', #74781, #141351, #62398, .T. ) ;
#45994 = COLOUR_RGB ( '', 0.72549020, 0.75294118, 0.79215686) ;
#45996 = EDGE_CURVE ( 'NONE', #126491, #59163, #112171, .T. ) ;
#45997 = PLANE ( 'NONE',  #74925 ) ;
#45998 = EDGE_LOOP ( 'NONE', ( #134977, #117753, #19425, #103752 ) ) ;
#45999 = CARTESIAN_POINT ( 'NONE',  ( 0.000000000000000000, 0.000000000000000000, 5.000000000000000000 ) ) ;
#46000 = CARTESIAN_POINT ( 'NONE',  ( -3.707106781186518152, 17.25929247661554911, 5.000000000000000000 ) ) ;
#46001 = CARTESIAN_POINT ( 'NONE',  ( 1.249915061292911078, -0.4000000000000004108, 2.317232259782045389 ) ) ;
#46002 = CARTESIAN_POINT ( 'NONE',  ( -39.29974487139159578, -27.71228299555233576, 4.000000000000000000 ) ) ;
#46003 = LINE ( 'NONE', #24234, #36914 ) ;
#46004 = EDGE_CURVE ( 'NONE', #52143, #95691, #7245, .T. ) ;
#46005 = CARTESIAN_POINT ( 'NONE',  ( 57.48921356237308800, -27.52281430457095368, 5.000000000000000000 ) ) ;
#46006 = PLANE ( 'NONE',  #67758 ) ;
#46007 = DIRECTION ( 'NONE',  ( -0.3543493200069162685, -0.000000000000000000, -0.9351131265310288487 ) ) ;
#46008 = EDGE_CURVE ( 'NONE', #130559, #75959, #75143, .T. ) ;
#46009 = DIRECTION ( 'NONE',  ( -0.000000000000000000, -1.000000000000000000, -0.000000000000000000 ) ) ;
#46010 = ORIENTED_EDGE ( 'NONE', *, *, #44690, .F. ) ;
#46011 = EDGE_CURVE ( 'NONE', #45672, #132598, #41322, .T. ) ;
#46012 = EDGE_LOOP ( 'NONE', ( #88172, #116868, #127477, #71038 ) ) ;
#46013 = LINE ( 'NONE', #124968, #73409 ) ;
#46014 = PLANE ( 'NONE',  #12298 ) ;
#46015 = DIRECTION ( 'NONE',  ( 0.6830127018922181881, 0.6830127018922202975, -0.2588190451025214056 ) ) ;
#46016 = EDGE_CURVE ( 'NONE', #76475, #72349, #26473, .T. ) ;
#46017 = ORIENTED_EDGE ( 'NONE', *, *, #57302, .F. ) ;
#46018 = CARTESIAN_POINT ( 'NONE',  ( 7.966599676569728672, 6.759292476615653023, 12.28218704918523940 ) ) ;
#46019 = FACE_OUTER_BOUND ( 'NONE', #71014, .T. ) ;
#46020 = EDGE_CURVE ( 'NONE', #41843, #92431, #107987, .T. ) ;
#46021 = DIRECTION ( 'NONE',  ( 0.7071067811865487940, 0.7071067811865463515, 0.000000000000000000 ) ) ;
#46022 = ORIENTED_EDGE ( 'NONE', *, *, #61238, .T. ) ;
#46023 = PLANE ( 'NONE',  #156 ) ;
#46024 = UNCERTAINTY_MEASURE_WITH_UNIT (LENGTH_MEASURE( 1.000000000000000082E-05 ), #138273, 'distance_accuracy_value', 'NONE');
#46025 = CARTESIAN_POINT ( 'NONE',  ( -65.99451991528749772, 28.92564299267984396, 4.000000000000000000 ) ) ;
#46026 = EDGE_CURVE ( 'NONE', #74278, #113076, #17435, .T. ) ;
#46027 = CARTESIAN_POINT ( 'NONE',  ( -5.207106781186502609, 9.759292476615618384, 5.000000000000000000 ) ) ;
#46028 = CARTESIAN_POINT ( 'NONE',  ( 56.49543019189812298, 5.291415217122917625, 3.055000000000002380 ) ) ;
#46029 = PLANE ( 'NONE',  #4685 ) ;
#46030 = CARTESIAN_POINT ( 'NONE',  ( -8.510786437626906675, -27.52281430457049183, 5.000000000000000000 ) ) ;
#46031 = VECTOR ( 'NONE', #106569, 1000.000000000000000 ) ;
#46032 = DIRECTION ( 'NONE',  ( -1.000000000000000000, -1.224606353822377258E-16, -0.000000000000000000 ) ) ;
#46033 = VERTEX_POINT ( 'NONE', #84843 ) ;
#46034 = DIRECTION ( 'NONE',  ( -1.000000000000000000, -1.224606353822377258E-16, -0.000000000000000000 ) ) ;
#46035 = ORIENTED_EDGE ( 'NONE', *, *, #106820, .F. ) ;
#46036 = ADVANCED_FACE ( 'NONE', ( #7971 ), #105851, .F. ) ;
#46037 = DIRECTION ( 'NONE',  ( 0.3543493200069163240, -0.000000000000000000, 0.9351131265310288487 ) ) ;
#46038 = CIRCLE ( 'NONE', #101472, 2.337566348077130929 ) ;
#46039 = VECTOR ( 'NONE', #115654, 1000.000000000000000 ) ;
#46040 = VECTOR ( 'NONE', #93521, 1000.000000000000000 ) ;
#46041 = CARTESIAN_POINT ( 'NONE',  ( -42.18398860626899705, 28.73617430169816700, 5.000000000000000000 ) ) ;
#46042 = LINE ( 'NONE', #122130, #81315 ) ;
#46043 = AXIS2_PLACEMENT_3D ( 'NONE', #79841, #14536, #103647 ) ;
#46044 = CARTESIAN_POINT ( 'NONE',  ( -24.51665438641027706, 22.22500000000000142, 4.500000000000000888 ) ) ;
#46045 = DIRECTION ( 'NONE',  ( -0.7071067811865486830, -0.7071067811865464625, -0.000000000000000000 ) ) ;
#46046 = LINE ( 'NONE', #33043, #1379 ) ;
#46047 = EDGE_LOOP ( 'NONE', ( #112397, #49809, #61956, #2330, #94452 ) ) ;
#46048 = ORIENTED_EDGE ( 'NONE', *, *, #75371, .T. ) ;
#46049 = DIRECTION ( 'NONE',  ( -0.6830127018922180770, -0.6830127018922204085, -0.2588190451025213501 ) ) ;
#46050 = CARTESIAN_POINT ( 'NONE',  ( 4.184256412735922304, 4.202752102959690472E-16, 0.000000000000000000 ) ) ;
#46051 = UNCERTAINTY_MEASURE_WITH_UNIT (LENGTH_MEASURE( 1.000000000000000082E-05 ), #123452, 'distance_accuracy_value', 'NONE');
#46052 = COLOUR_RGB ( '', 0.08235294, 0.09019608, 0.10196078) ;
#46053 = AXIS2_PLACEMENT_3D ( 'NONE', #82961, #80833, #4603 ) ;
#46054 = CARTESIAN_POINT ( 'NONE',  ( 24.32816939922335564, 20.25929247661551003, 4.000000000000000000 ) ) ;
#46056 = EDGE_CURVE ( 'NONE', #73841, #99786, #81260, .T. ) ;
#46055 = DIRECTION ( 'NONE',  ( -0.7071067811865486830, -0.7071067811865464625, 0.000000000000000000 ) ) ;
#46057 = CARTESIAN_POINT ( 'NONE',  ( 78.68336038379622721, -2.130196079827426203, 7.949999999999997513 ) ) ;
#46059 = EDGE_CURVE ( 'NONE', #89491, #50573, #74710, .T. ) ;
#46058 = DIRECTION ( 'NONE',  ( -1.000000000000000000, -0.000000000000000000, -0.000000000000000000 ) ) ;
#46060 = CARTESIAN_POINT ( 'NONE',  ( -69.18398860626899705, 28.73617430169835529, 5.000000000000000000 ) ) ;
#46061 = ORIENTED_EDGE ( 'NONE', *, *, #121354, .T. ) ;
#46062 = CARTESIAN_POINT ( 'NONE',  ( 75.37500000000000000, 7.950000000000000178, 1.460391307983218535E-15 ) ) ;
#46063 = DIRECTION ( 'NONE',  ( 0.7071067811865486830, -0.7071067811865464625, -0.000000000000000000 ) ) ;
#46064 = DIRECTION ( 'NONE',  ( 0.3543493200069162685, -0.000000000000000000, -0.9351131265310288487 ) ) ;
#46065 = CARTESIAN_POINT ( 'NONE',  ( 152.4000000000000057, 7.919999999999947526, 19.12499999999998224 ) ) ;
#46066 = VECTOR ( 'NONE', #59409, 1000.000000000000000 ) ;
#46067 = VERTEX_POINT ( 'NONE', #128365 ) ;
#46068 = ADVANCED_FACE ( 'NONE', ( #18857 ), #52211, .T. ) ;
#46069 = CARTESIAN_POINT ( 'NONE',  ( 12.18398860626900060, 28.73617430169795739, 5.000000000000000000 ) ) ;
#46070 = VECTOR ( 'NONE', #43902, 1000.000000000000000 ) ;
#46071 = CARTESIAN_POINT ( 'NONE',  ( 25.39999999999999858, 1.126161369193133366, -16.41140641659140798 ) ) ;
#46072 = CARTESIAN_POINT ( 'NONE',  ( 70.43793019189810423, -6.110000000000001208, 1.637169565754158951 ) ) ;
#46074 = EDGE_LOOP ( 'NONE', ( #132471, #44408, #115853, #10137 ) ) ;
#46073 = VECTOR ( 'NONE', #124815, 999.9999999999998863 ) ;
#46075 = ORIENTED_EDGE ( 'NONE', *, *, #110888, .T. ) ;
#46076 = VECTOR ( 'NONE', #90446, 1000.000000000000000 ) ;
#46077 = AXIS2_PLACEMENT_3D ( 'NONE', #57087, #101269, #120130 ) ;
#46078 = FACE_OUTER_BOUND ( 'NONE', #49066, .T. ) ;
#46079 = VECTOR ( 'NONE', #51183, 1000.000000000000000 ) ;
#46080 = FACE_OUTER_BOUND ( 'NONE', #76813, .T. ) ;
#46081 = LINE ( 'NONE', #34465, #7071 ) ;
#46083 = ORIENTED_EDGE ( 'NONE', *, *, #135014, .F. ) ;
#46082 = DIRECTION ( 'NONE',  ( 0.6830127018922180770, -0.6830127018922204085, -0.2588190451025213501 ) ) ;
#46084 = CARTESIAN_POINT ( 'NONE',  ( -5.510786437626906675, -27.52281430457051314, 5.000000000000000000 ) ) ;
#46085 = DIRECTION ( 'NONE',  ( -0.6830127018922181881, 0.6830127018922202975, -0.2588190451025214056 ) ) ;
#46086 = CARTESIAN_POINT ( 'NONE',  ( 7.139999999999985469, -39.92999999999999972, -40.00000000000000000 ) ) ;
#46087 = CIRCLE ( 'NONE', #129346, 2.055000000000001048 ) ;
#46088 = CARTESIAN_POINT ( 'NONE',  ( 0.000000000000000000, 0.000000000000000000, 5.000000000000000000 ) ) ;
#46089 = COLOUR_RGB ( '', 0.66274510, 0.83137255, 0.94901961) ;
#46090 = ORIENTED_EDGE ( 'NONE', *, *, #115441, .F. ) ;
#46091 = ORIENTED_EDGE ( 'NONE', *, *, #25553, .T. ) ;
#46092 = CARTESIAN_POINT ( 'NONE',  ( 54.39626352523144703, 4.472830434245840259, -4.472830434245839371 ) ) ;
#46093 = ORIENTED_EDGE ( 'NONE', *, *, #109447, .F. ) ;
#46094 = DIRECTION ( 'NONE',  ( -1.000000000000000000, -1.224606353822377258E-16, -0.000000000000000000 ) ) ;
#46095 = LINE ( 'NONE', #133109, #48058 ) ;
#46096 = CARTESIAN_POINT ( 'NONE',  ( 13.49159235450332162, 9.902892378096218942E-16, 0.000000000000000000 ) ) ;
#46097 = CARTESIAN_POINT ( 'NONE',  ( 54.66666666666667140, 6.884901960086285300, 3.975000000000003642 ) ) ;
#46098 = ORIENTED_EDGE ( 'NONE', *, *, #90683, .F. ) ;
#46099 = EDGE_LOOP ( 'NONE', ( #101787, #22161, #62448, #2019, #5922 ) ) ;
#46100 = VECTOR ( 'NONE', #41699, 1000.000000000000000 ) ;
#46101 = LINE ( 'NONE', #1115, #125544 ) ;
#46102 = CARTESIAN_POINT ( 'NONE',  ( -16.85442536677114589, -0.3105974261732821762, -34.40776350357948132 ) ) ;
#46103 = ORIENTED_EDGE ( 'NONE', *, *, #20596, .T. ) ;
#46104 = FACE_OUTER_BOUND ( 'NONE', #40056, .T. ) ;
#46105 = DIRECTION ( 'NONE',  ( -0.000000000000000000, 1.000000000000000000, -0.000000000000000000 ) ) ;
#46106 = CARTESIAN_POINT ( 'NONE',  ( -57.18398860626899705, 28.73617430169827358, 5.000000000000000000 ) ) ;
#46107 = EDGE_LOOP ( 'NONE', ( #141532, #111516, #138566, #136525 ) ) ;
#46108 = EDGE_CURVE ( 'NONE', #16056, #9912, #19580, .T. ) ;
#46109 = ADVANCED_FACE ( 'NONE', ( #123739 ), #57064, .F. ) ;
#46110 = FACE_BOUND ( 'NONE', #87476, .T. ) ;
#46111 = CARTESIAN_POINT ( 'NONE',  ( 13.10966639810773948, 3.759292476615678336, 4.164048746910661514 ) ) ;
#46112 = CARTESIAN_POINT ( 'NONE',  ( -2.206660635421508143, 21.75929247661549937, 4.998822639870708073 ) ) ;
#46113 = DIRECTION ( 'NONE',  ( -0.3543493200069162685, -0.000000000000000000, -0.9351131265310288487 ) ) ;
#46114 = CARTESIAN_POINT ( 'NONE',  ( -20.20003122016824548, 8.259292476615634371, 16.85664084051845890 ) ) ;
#46115 = EDGE_CURVE ( 'NONE', #25446, #137546, #59212, .T. ) ;
#46116 = EDGE_CURVE ( 'NONE', #22881, #18685, #4012, .T. ) ;
#46117 = DIRECTION ( 'NONE',  ( -0.6830127018922180770, -0.6830127018922204085, -0.2588190451025213501 ) ) ;
#46118 = CARTESIAN_POINT ( 'NONE',  ( -78.45649007701791788, -49.06047650249247027, 67.89598428144745412 ) ) ;
#46119 = ORIENTED_EDGE ( 'NONE', *, *, #75287, .T. ) ;
#46120 = VERTEX_POINT ( 'NONE', #45472 ) ;
#46121 = CARTESIAN_POINT ( 'NONE',  ( 102.5787635252314658, -7.482591942790325086E-16, 6.109999999999998543 ) ) ;
#46122 = VERTEX_POINT ( 'NONE', #12788 ) ;
#46123 = EDGE_CURVE ( 'NONE', #89522, #74016, #35312, .T. ) ;
#46124 = DIRECTION ( 'NONE',  ( 0.7071067811865486830, -0.7071067811865464625, -0.000000000000000000 ) ) ;
#46125 = VERTEX_POINT ( 'NONE', #113533 ) ;
#46126 = CARTESIAN_POINT ( 'NONE',  ( 78.48921356237309510, -27.52281430457109934, 5.000000000000000000 ) ) ;
#46127 = DIRECTION ( 'NONE',  ( -0.000000000000000000, 0.000000000000000000, 1.000000000000000000 ) ) ;
#46128 = ADVANCED_FACE ( 'NONE', ( #58517 ), #70508, .T. ) ;
#46129 = CARTESIAN_POINT ( 'NONE',  ( -36.29974487139159578, -27.71228299555231445, 4.000000000000000000 ) ) ;
#46130 = VERTEX_POINT ( 'NONE', #3336 ) ;
#46131 = FACE_OUTER_BOUND ( 'NONE', #47130, .T. ) ;
#46132 = CYLINDRICAL_SURFACE ( 'NONE', #17209, 3.378199999999994319 ) ;
#46133 = DIRECTION ( 'NONE',  ( -0.6830127018922181881, 0.6830127018922202975, -0.2588190451025214056 ) ) ;
#46134 = PLANE ( 'NONE',  #103615 ) ;
#46136 = DIRECTION ( 'NONE',  ( 0.7071067811865487940, 0.7071067811865463515, -0.000000000000000000 ) ) ;
#46135 = CARTESIAN_POINT ( 'NONE',  ( -2.700255128608413990, -27.71228299555204089, 4.000000000000000000 ) ) ;
#46137 = DIRECTION ( 'NONE',  ( -0.7071067811865487940, 0.7071067811865463515, 0.000000000000000000 ) ) ;
#46138 = VECTOR ( 'NONE', #58064, 1000.000000000000000 ) ;
#46140 = EDGE_CURVE ( 'NONE', #119913, #102340, #111394, .T. ) ;
#46139 = CIRCLE ( 'NONE', #127122, 0.5000000000000000000 ) ;
#46141 = AXIS2_PLACEMENT_3D ( 'NONE', #23518, #135177, #90203 ) ;
#46142 = CARTESIAN_POINT ( 'NONE',  ( -34.92500000000001137, 20.82781275693358225, 4.470553524000292711 ) ) ;
#46143 = AXIS2_PLACEMENT_3D ( 'NONE', #20002, #109169, #77298 ) ;
#46144 = ORIENTED_EDGE ( 'NONE', *, *, #73202, .T. ) ;
#46145 = CARTESIAN_POINT ( 'NONE',  ( 6.005480084712508493, 28.92564299267933947, 4.000000000000000000 ) ) ;
#46146 = CARTESIAN_POINT ( 'NONE',  ( 26.99999999999981881, -19.06887692260762179, 4.000000000000000000 ) ) ;
#46147 = VECTOR ( 'NONE', #57191, 1000.000000000000000 ) ;
#46148 = ORIENTED_EDGE ( 'NONE', *, *, #29379, .T. ) ;
#46149 = ORIENTED_EDGE ( 'NONE', *, *, #16970, .T. ) ;
#46150 = ORIENTED_EDGE ( 'NONE', *, *, #14587, .T. ) ;
#46151 = CARTESIAN_POINT ( 'NONE',  ( 51.04209685856476852, 5.291415217122923842, -3.054999999999996163 ) ) ;
#46152 = ADVANCED_FACE ( 'NONE', ( #134615 ), #101239, .T. ) ;
#46153 = EDGE_CURVE ( 'NONE', #10128, #143125, #102691, .T. ) ;
#46154 = ORIENTED_EDGE ( 'NONE', *, *, #71240, .F. ) ;
#46155 = COLOUR_RGB ( '', 0.72549020, 0.75294118, 0.79215686) ;
#46156 = CARTESIAN_POINT ( 'NONE',  ( -23.99999999999983302, -13.39766691384885000, -10.96608748226460328 ) ) ;
#46157 = CARTESIAN_POINT ( 'NONE',  ( 5.004139616203772789, -3.047499999999994547, 5.278424836066145431 ) ) ;
#46158 = CARTESIAN_POINT ( 'NONE',  ( 89.25043019189810423, 3.055000000000002824, -5.291415217122919401 ) ) ;
#46159 = CARTESIAN_POINT ( 'NONE',  ( 45.29974487139158867, -27.71228299555237840, 4.000000000000000000 ) ) ;
#46160 = ORIENTED_EDGE ( 'NONE', *, *, #70029, .F. ) ;
#46161 = MANIFOLD_SOLID_BREP ( 'ThdSchPat', #16243 ) ;
#46162 = DIRECTION ( 'NONE',  ( -0.7071067811865487940, 0.7071067811865463515, 0.000000000000000000 ) ) ;
#46163 = EDGE_CURVE ( 'NONE', #136547, #74950, #136011, .T. ) ;
#46164 = ORIENTED_EDGE ( 'NONE', *, *, #6811, .T. ) ;
#46165 = CARTESIAN_POINT ( 'NONE',  ( -0.1839886062690032631, 28.73617430169787568, 5.000000000000000000 ) ) ;
#46166 = COLOUR_RGB ( '', 0.31764706, 0.68627451, 0.89019608) ;
#46167 = AXIS2_PLACEMENT_3D ( 'NONE', #87349, #9771, #109074 ) ;
#46168 = CARTESIAN_POINT ( 'NONE',  ( -21.70666784232957980, -22.22500000000000142, -0.008920181745145777663 ) ) ;
#46169 = ORIENTED_EDGE ( 'NONE', *, *, #37550, .F. ) ;
#46170 =( NAMED_UNIT ( * ) PLANE_ANGLE_UNIT ( ) SI_UNIT ( $, .RADIAN. ) );
#46171 = LINE ( 'NONE', #79537, #101401 ) ;
#46173 = ADVANCED_FACE ( 'NONE', ( #80940 ), #25824, .T. ) ;
#46172 = LINE ( 'NONE', #65797, #75244 ) ;
#46174 = VERTEX_POINT ( 'NONE', #89652 ) ;
#46175 = PRESENTATION_LAYER_ASSIGNMENT (  '', '', ( #131834 ) ) ;
#46176 = DIRECTION ( 'NONE',  ( -0.7071067811865486830, -0.7071067811865464625, 0.000000000000000000 ) ) ;
#46177 = ORIENTED_EDGE ( 'NONE', *, *, #75185, .T. ) ;
#46178 = EDGE_CURVE ( 'NONE', #110261, #64365, #34572, .T. ) ;
#46179 = ORIENTED_EDGE ( 'NONE', *, *, #55144, .F. ) ;
#46180 = VERTEX_POINT ( 'NONE', #94635 ) ;
#46181 = VECTOR ( 'NONE', #120748, 1000.000000000000000 ) ;
#46183 = EDGE_CURVE ( 'NONE', #117925, #102633, #26544, .T. ) ;
#46182 = VECTOR ( 'NONE', #33739, 1000.000000000000000 ) ;
#46184 = CARTESIAN_POINT ( 'NONE',  ( 28.00000000000002487, -52.14999999999999147, -59.92499999999979821 ) ) ;
#46185 = VECTOR ( 'NONE', #42108, 999.9999999999998863 ) ;
#46186 = LINE ( 'NONE', #13483, #116506 ) ;
#46187 = CARTESIAN_POINT ( 'NONE',  ( -5.999999999999954703, -12.03360074219762055, 5.000000000000000000 ) ) ;
#46188 = CARTESIAN_POINT ( 'NONE',  ( -15.18398860626900237, 28.73617430169797871, 5.000000000000000000 ) ) ;
#46189 = ORIENTED_EDGE ( 'NONE', *, *, #105298, .T. ) ;
#46190 = CIRCLE ( 'NONE', #11453, 2.500000000000000444 ) ;
#46191 = AXIS2_PLACEMENT_3D ( 'NONE', #40308, #128711, #29387 ) ;
#46192 = SURFACE_SIDE_STYLE ('',( #133881 ) ) ;
#46193 = CARTESIAN_POINT ( 'NONE',  ( 23.89540314143522437, 2.126176841940962348, 7.934999999999989839 ) ) ;
#46194 = DIRECTION ( 'NONE',  ( -0.000000000000000000, 0.3543493200069153248, 0.9351131265310292928 ) ) ;
#46195 = DIRECTION ( 'NONE',  ( -0.7071067811865487940, 0.7071067811865463515, 0.000000000000000000 ) ) ;
#46196 = ADVANCED_FACE ( 'NONE', ( #140303 ), #15612, .F. ) ;
#46197 = CARTESIAN_POINT ( 'NONE',  ( 34.92499999999998295, 0.8561230773924017878, 4.000000000000000000 ) ) ;
#46198 = ORIENTED_EDGE ( 'NONE', *, *, #17130, .T. ) ;
#46199 = VERTEX_POINT ( 'NONE', #51886 ) ;
#46200 = ORIENTED_EDGE ( 'NONE', *, *, #74441, .F. ) ;
#46201 = CARTESIAN_POINT ( 'NONE',  ( -14.99999999999989697, 10.55218569542906337, 5.000000000000000000 ) ) ;
#46202 = CARTESIAN_POINT ( 'NONE',  ( -4.823340898400238608, 5.259292476615665457, 15.86257073897099090 ) ) ;
#46203 = UNCERTAINTY_MEASURE_WITH_UNIT (LENGTH_MEASURE( 1.000000000000000082E-05 ), #135310, 'distance_accuracy_value', 'NONE');
#46204 = VECTOR ( 'NONE', #98058, 1000.000000000000000 ) ;
#46205 = DIRECTION ( 'NONE',  ( 0.000000000000000000, 0.000000000000000000, 1.000000000000000000 ) ) ;
#46206 = EDGE_CURVE ( 'NONE', #75908, #54158, #116411, .T. ) ;
#46207 = SURFACE_STYLE_USAGE ( .BOTH. , #1893 ) ;
#46208 = LINE ( 'NONE', #90382, #121854 ) ;
#46209 = DIRECTION ( 'NONE',  ( 0.7071067811865487940, -0.7071067811865463515, 0.000000000000000000 ) ) ;
#46210 = CARTESIAN_POINT ( 'NONE',  ( -23.99999999999982947, -11.35517001088074629, -1.126524801160163625 ) ) ;
#46211 = DIRECTION ( 'NONE',  ( -0.6830127018922180770, -0.6830127018922204085, -0.2588190451025213501 ) ) ;
#46212 = CARTESIAN_POINT ( 'NONE',  ( 2.671830600776444076, 11.25929247661560240, 4.000000000000000000 ) ) ;
#46213 = CARTESIAN_POINT ( 'NONE',  ( 0.000000000000000000, 0.000000000000000000, 5.000000000000000000 ) ) ;
#46214 = ORIENTED_EDGE ( 'NONE', *, *, #79413, .T. ) ;
#46215 = ORIENTED_EDGE ( 'NONE', *, *, #11625, .F. ) ;
#46216 = CARTESIAN_POINT ( 'NONE',  ( 17.98330628287043709, 6.094999999999991758, 1.633150327867686880 ) ) ;
#46218 = VERTEX_POINT ( 'NONE', #83074 ) ;
#46217 = DIRECTION ( 'NONE',  ( -0.000000000000000000, 0.3543493200069153248, 0.9351131265310292928 ) ) ;
#46219 = CARTESIAN_POINT ( 'NONE',  ( -10.49999999999992184, 8.900465351122141655, -2.516491619111488554 ) ) ;
#46220 = ORIENTED_EDGE ( 'NONE', *, *, #57288, .F. ) ;
#46221 = DIRECTION ( 'NONE',  ( 0.000000000000000000, -1.000000000000000000, 0.000000000000000000 ) ) ;
#46222 = ORIENTED_EDGE ( 'NONE', *, *, #58516, .T. ) ;
#46223 = LINE ( 'NONE', #46962, #130035 ) ;
#46224 = UNCERTAINTY_MEASURE_WITH_UNIT (LENGTH_MEASURE( 1.000000000000000082E-05 ), #48368, 'distance_accuracy_value', 'NONE');
#46225 = EDGE_LOOP ( 'NONE', ( #69595, #34215, #129658, #107537 ) ) ;
#46226 = LINE ( 'NONE', #110007, #107768 ) ;
#46227 = EDGE_CURVE ( 'NONE', #111700, #11445, #5475, .T. ) ;
#46228 = CARTESIAN_POINT ( 'NONE',  ( 98.66252705046289861, 7.949999999999998401, 1.460391307983218338E-15 ) ) ;
#46229 = CYLINDRICAL_SURFACE ( 'NONE', #62490, 2.500000000000000444 ) ;
#46230 = DIRECTION ( 'NONE',  ( -0.7071067811865487940, 0.7071067811865463515, -0.000000000000000000 ) ) ;
#46231 = EDGE_LOOP ( 'NONE', ( #114437, #76832, #47183, #111697 ) ) ;
#46232 = LINE ( 'NONE', #89013, #72295 ) ;
#46233 = CARTESIAN_POINT ( 'NONE',  ( 21.48921356237309155, -27.52281430457070499, 5.000000000000000000 ) ) ;
#46234 = FACE_OUTER_BOUND ( 'NONE', #138245, .T. ) ;
#46235 = CARTESIAN_POINT ( 'NONE',  ( 10.64583333333333215, -1.633150327867689988, 6.094999999999989981 ) ) ;
#46236 = DIRECTION ( 'NONE',  ( -0.7071067811865486830, 0.7071067811865464625, 0.000000000000000000 ) ) ;
#46237 = CARTESIAN_POINT ( 'NONE',  ( -45.29974487139158867, -27.71228299555237840, 4.000000000000000000 ) ) ;
#46238 = DIRECTION ( 'NONE',  ( -0.000000000000000000, 0.3543493200069153248, 0.9351131265310292928 ) ) ;
#46239 = ORIENTED_EDGE ( 'NONE', *, *, #85026, .T. ) ;
#46240 = EDGE_CURVE ( 'NONE', #110472, #77537, #117797, .T. ) ;
#46241 = CARTESIAN_POINT ( 'NONE',  ( -15.48921356237309510, -27.52281430457066236, 5.000000000000000000 ) ) ;
#46242 = ORIENTED_EDGE ( 'NONE', *, *, #14888, .T. ) ;
#46243 = CARTESIAN_POINT ( 'NONE',  ( 97.12543019189810423, 5.291415217122919401, 3.055000000000002824 ) ) ;
#46244 = CARTESIAN_POINT ( 'NONE',  ( 14.99999999999988809, -5.527737879153178824, -7.983877177622407117 ) ) ;
#46245 = FILL_AREA_STYLE_COLOUR ( '', #41363 ) ;
#46246 = CIRCLE ( 'NONE', #115594, 1.898649999999993065 ) ;
#46247 = DIRECTION ( 'NONE',  ( 0.6830127018922181881, 0.6830127018922202975, -0.2588190451025214056 ) ) ;
#46248 = CARTESIAN_POINT ( 'NONE',  ( 123.5545056966553688, -44.02090675800832287, -34.92500000000512728 ) ) ;
#46249 = ORIENTED_EDGE ( 'NONE', *, *, #6146, .F. ) ;
#46250 = VECTOR ( 'NONE', #105812, 999.9999999999998863 ) ;
#46251 = AXIS2_PLACEMENT_3D ( 'NONE', #82372, #70790, #37434 ) ;
#46252 = AXIS2_PLACEMENT_3D ( 'NONE', #16633, #100975, #115928 ) ;
#46253 = FACE_OUTER_BOUND ( 'NONE', #50302, .T. ) ;
#46254 = CARTESIAN_POINT ( 'NONE',  ( -34.92500000000001137, -13.19990548397266394, 4.759050581649336920 ) ) ;
#46255 =( BOUNDED_CURVE ( )  B_SPLINE_CURVE ( 3, ( #14622, #56021, #58176, #78464 ),
 .UNSPECIFIED., .F., .T. ) 
 B_SPLINE_CURVE_WITH_KNOTS ( ( 4, 4 ),
 ( 5.106027341939300968, 6.645403452391245303 ),
 .UNSPECIFIED. ) 
 CURVE ( )  GEOMETRIC_REPRESENTATION_ITEM ( )  RATIONAL_B_SPLINE_CURVE ( ( 1.000000000000000000, 0.8120851936182325037, 0.8120851936182325037, 1.000000000000000000 ) ) 
 REPRESENTATION_ITEM ( '' )  );
#46256 = VECTOR ( 'NONE', #110620, 1000.000000000000000 ) ;
#46257 = CARTESIAN_POINT ( 'NONE',  ( -21.18398860626899349, 28.73617430169802134, 5.000000000000000000 ) ) ;
#46258 = ORIENTED_EDGE ( 'NONE', *, *, #57731, .T. ) ;
#46259 = LINE ( 'NONE', #80306, #83298 ) ;
#46260 = SURFACE_STYLE_USAGE ( .BOTH. , #55689 ) ;
#46262 = VERTEX_POINT ( 'NONE', #72950 ) ;
#46261 = PLANE ( 'NONE',  #109945 ) ;
#46263 = PLANE ( 'NONE',  #110787 ) ;
#46264 = DIRECTION ( 'NONE',  ( 0.7071067811865487940, 0.7071067811865463515, 0.000000000000000000 ) ) ;
#46265 = DIRECTION ( 'NONE',  ( -0.7071067811865486830, 0.7071067811865464625, 0.000000000000000000 ) ) ;
#46266 = DIRECTION ( 'NONE',  ( 1.000000000000000000, 0.000000000000000000, 0.000000000000000000 ) ) ;
#46267 = VECTOR ( 'NONE', #47835, 1000.000000000000114 ) ;
#46268 = DIRECTION ( 'NONE',  ( 0.7071067811865487940, 0.7071067811865463515, -0.000000000000000000 ) ) ;
#46269 = ORIENTED_EDGE ( 'NONE', *, *, #36277, .T. ) ;
#46270 = ORIENTED_EDGE ( 'NONE', *, *, #125350, .T. ) ;
#46271 = ORIENTED_EDGE ( 'NONE', *, *, #5329, .F. ) ;
#46272 = CARTESIAN_POINT ( 'NONE',  ( 85.89626352523144703, 4.472830434245840259, -4.472830434245839371 ) ) ;
#46273 = AXIS2_PLACEMENT_3D ( 'NONE', #108167, #20461, #64710 ) ;
#46274 = ORIENTED_EDGE ( 'NONE', *, *, #134343, .F. ) ;
#46275 = PLANE ( 'NONE',  #99524 ) ;
#46276 = LINE ( 'NONE', #123822, #78065 ) ;
#46277 = VECTOR ( 'NONE', #13894, 1000.000000000000000 ) ;
#46278 = VECTOR ( 'NONE', #23997, 999.9999999999998863 ) ;
#46279 = CARTESIAN_POINT ( 'NONE',  ( 2.816011393730999401, 28.73617430169785436, 5.000000000000000000 ) ) ;
#46280 = CARTESIAN_POINT ( 'NONE',  ( -12.48921356237309155, -27.52281430457064104, 5.000000000000000000 ) ) ;
#46281 = EDGE_LOOP ( 'NONE', ( #5608, #109065, #67490, #58886 ) ) ;
#46282 = LINE ( 'NONE', #12880, #90780 ) ;
#46283 = CARTESIAN_POINT ( 'NONE',  ( -51.18398860626899705, 28.73617430169823095, 5.000000000000000000 ) ) ;
#46284 = DIRECTION ( 'NONE',  ( -0.7071067811865486830, -0.7071067811865464625, 0.000000000000000000 ) ) ;
#46285 = PRESENTATION_LAYER_ASSIGNMENT (  '', '', ( #4466 ) ) ;
#46286 = CARTESIAN_POINT ( 'NONE',  ( 84.93293019189812298, 1.637169565754156508, 6.110000000000000320 ) ) ;
#46287 = ORIENTED_EDGE ( 'NONE', *, *, #49325, .F. ) ;
#46288 = CARTESIAN_POINT ( 'NONE',  ( -30.70710678118632941, 17.25929247661554200, 5.000000000000000000 ) ) ;
#46289 = ADVANCED_FACE ( 'NONE', ( #84514 ), #95360, .F. ) ;
#46290 = CARTESIAN_POINT ( 'NONE',  ( 4.499999999999976019, 3.073033219394630144, -6.593910359670959842 ) ) ;
#46291 = VECTOR ( 'NONE', #81357, 999.9999999999998863 ) ;
#46292 = VECTOR ( 'NONE', #101286, 999.9999999999998863 ) ;
#46293 = VERTEX_POINT ( 'NONE', #126549 ) ;
#46294 = ORIENTED_EDGE ( 'NONE', *, *, #96324, .T. ) ;
#46295 = LINE ( 'NONE', #23041, #116252 ) ;
#46296 = EDGE_CURVE ( 'NONE', #26483, #60374, #96063, .T. ) ;
#46297 = ADVANCED_FACE ( 'NONE', ( #50449 ), #106211, .T. ) ;
#46298 = AXIS2_PLACEMENT_3D ( 'NONE', #45096, #91420, #23269 ) ;
#46299 = CARTESIAN_POINT ( 'NONE',  ( 25.39999999999999147, -6.329169252561944070, -1.258656420499090878 ) ) ;
#46300 = AXIS2_PLACEMENT_3D ( 'NONE', #95952, #43026, #75650 ) ;
#46301 = DIRECTION ( 'NONE',  ( 0.7071067811865486830, -0.7071067811865464625, -0.000000000000000000 ) ) ;
#46302 = CARTESIAN_POINT ( 'NONE',  ( 20.51078643762690490, -27.52281430457041012, 5.000000000000000000 ) ) ;
#46303 = EDGE_CURVE ( 'NONE', #26872, #114249, #29384, .T. ) ;
#46304 = EDGE_CURVE ( 'NONE', #7608, #31464, #117100, .T. ) ;
#46305 = DIRECTION ( 'NONE',  ( 0.7071067811865487940, 0.7071067811865463515, 0.000000000000000000 ) ) ;
#46306 = SURFACE_STYLE_FILL_AREA ( #102077 ) ;
#46307 = VERTEX_POINT ( 'NONE', #138895 ) ;
#46308 = ORIENTED_EDGE ( 'NONE', *, *, #54508, .F. ) ;
#46310 = EDGE_CURVE ( 'NONE', #130435, #49722, #104070, .T. ) ;
#46309 = CARTESIAN_POINT ( 'NONE',  ( -34.49999999999976552, 6.431123077392124188, 4.000000000000000000 ) ) ;
#46311 = ORIENTED_EDGE ( 'NONE', *, *, #68444, .T. ) ;
#46312 = VERTEX_POINT ( 'NONE', #6886 ) ;
#46313 = VECTOR ( 'NONE', #48503, 1000.000000000000000 ) ;
#46314 = EDGE_CURVE ( 'NONE', #137089, #34213, #38851, .T. ) ;
#46315 = ADVANCED_FACE ( 'NONE', ( #40306 ), #49755, .F. ) ;
#46316 = DIRECTION ( 'NONE',  ( -1.000000000000000000, -1.224606353822377258E-16, -0.000000000000000000 ) ) ;
#46317 = ORIENTED_EDGE ( 'NONE', *, *, #105398, .T. ) ;
#46318 = CARTESIAN_POINT ( 'NONE',  ( 29.20666063542132207, 21.75929247661549581, 4.998822639870703632 ) ) ;
#46319 = LINE ( 'NONE', #90501, #47288 ) ;
#46320 = CARTESIAN_POINT ( 'NONE',  ( 21.18398860626899349, 28.73617430169802134, 5.000000000000000000 ) ) ;
#46321 = LINE ( 'NONE', #103486, #39186 ) ;
#46322 = VECTOR ( 'NONE', #22731, 1000.000000000000000 ) ;
#46323 = DIRECTION ( 'NONE',  ( 1.000000000000000000, 0.000000000000000000, 0.000000000000000000 ) ) ;
#46324 = ORIENTED_EDGE ( 'NONE', *, *, #41351, .T. ) ;
#46325 = ADVANCED_FACE ( 'NONE', ( #82367 ), #127272, .F. ) ;
#46326 = DIRECTION ( 'NONE',  ( 0.000000000000000000, 0.000000000000000000, 1.000000000000000000 ) ) ;
#46327 = ORIENTED_EDGE ( 'NONE', *, *, #23886, .F. ) ;
#46328 = DIRECTION ( 'NONE',  ( -1.000000000000000000, -0.000000000000000000, -0.000000000000000000 ) ) ;
#46329 = EDGE_LOOP ( 'NONE', ( #78763, #123280, #67829, #108258 ) ) ;
#46330 = CARTESIAN_POINT ( 'NONE',  ( -68.99451991528748351, 28.92564299267986172, 4.000000000000000000 ) ) ;
#46331 = ORIENTED_EDGE ( 'NONE', *, *, #72048, .T. ) ;
#46332 = DIRECTION ( 'NONE',  ( -0.7071067811865486830, -0.7071067811865464625, 0.000000000000000000 ) ) ;
#46333 = ORIENTED_EDGE ( 'NONE', *, *, #3423, .T. ) ;
#46334 = ORIENTED_EDGE ( 'NONE', *, *, #142492, .T. ) ;
#46335 = EDGE_CURVE ( 'NONE', #41303, #79450, #62762, .T. ) ;
#46336 = EDGE_LOOP ( 'NONE', ( #113144, #141709, #141025, #52355 ) ) ;
#46337 = LINE ( 'NONE', #57206, #111418 ) ;
#46338 = CARTESIAN_POINT ( 'NONE',  ( 23.00840764549667483, 9.139736423841732040E-16, 0.000000000000000000 ) ) ;
#46339 = CARTESIAN_POINT ( 'NONE',  ( -1.828169399223516400, -17.24070752338410628, 4.000000000000000000 ) ) ;
#46340 = CARTESIAN_POINT ( 'NONE',  ( 121.9170968585647756, 3.054999999999998828, 5.291415217122922066 ) ) ;
#46341 = CARTESIAN_POINT ( 'NONE',  ( 8.816011393731004731, 28.73617430169781173, 5.000000000000000000 ) ) ;
#46342 = CARTESIAN_POINT ( 'NONE',  ( -29.20710678118634362, -8.240707523384196875, 5.000000000000000000 ) ) ;
#46343 = CARTESIAN_POINT ( 'NONE',  ( 17.06332250466817158, -2.500000000000000000, 3.061616997868383634E-16 ) ) ;
#46344 = EDGE_CURVE ( 'NONE', #104397, #48470, #125875, .T. ) ;
#46345 = CARTESIAN_POINT ( 'NONE',  ( -54.18398860626899705, 28.73617430169825226, 5.000000000000000000 ) ) ;
#46347 = EDGE_CURVE ( 'NONE', #43368, #112625, #77222, .T. ) ;
#46346 = CARTESIAN_POINT ( 'NONE',  ( -4.499999999999972466, 8.900465351122148761, -2.516491619111501876 ) ) ;
#46349 = ORIENTED_EDGE ( 'NONE', *, *, #79772, .F. ) ;
#46348 = AXIS2_PLACEMENT_3D ( 'NONE', #61515, #62210, #39014 ) ;
#46350 = FILL_AREA_STYLE_COLOUR ( '', #29536 ) ;
#46351 = LINE ( 'NONE', #68803, #15181 ) ;
#46352 = DIRECTION ( 'NONE',  ( -0.000000000000000000, 0.000000000000000000, 1.000000000000000000 ) ) ;
#46353 = VERTEX_POINT ( 'NONE', #19238 ) ;
#46354 = EDGE_CURVE ( 'NONE', #143094, #78582, #20649, .T. ) ;
#46355 = ORIENTED_EDGE ( 'NONE', *, *, #80544, .T. ) ;
#46356 = CARTESIAN_POINT ( 'NONE',  ( -12.70000000000000284, -40.42999999999999261, -40.00000000000000000 ) ) ;
#46357 = CIRCLE ( 'NONE', #87910, 2.500000000000000444 ) ;
#46358 = CIRCLE ( 'NONE', #129703, 2.055000000000000604 ) ;
#46359 = ORIENTED_EDGE ( 'NONE', *, *, #90193, .F. ) ;
#46360 = AXIS2_PLACEMENT_3D ( 'NONE', #26891, #64520, #97868 ) ;
#46361 = EDGE_CURVE ( 'NONE', #34231, #105496, #9017, .T. ) ;
#46362 = EDGE_CURVE ( 'NONE', #41654, #19820, #119938, .T. ) ;
#46363 = AXIS2_PLACEMENT_3D ( 'NONE', #119894, #98186, #121345 ) ;
#46364 = LINE ( 'NONE', #67379, #30628 ) ;
#46365 = CARTESIAN_POINT ( 'NONE',  ( 8.816011393731004731, 28.73617430169781173, 5.000000000000000000 ) ) ;
#46366 = CARTESIAN_POINT ( 'NONE',  ( -34.92500000000001137, 22.22500000000000142, 4.000000000000000000 ) ) ;
#46367 = CARTESIAN_POINT ( 'NONE',  ( -19.27928215921719612, -2.789594763390444321, 4.000000000000000000 ) ) ;
#46368 = ORIENTED_EDGE ( 'NONE', *, *, #77243, .F. ) ;
#46369 = CARTESIAN_POINT ( 'NONE',  ( 11.93159235450332112, 9.902892378096218942E-16, 0.000000000000000000 ) ) ;
#46371 = ORIENTED_EDGE ( 'NONE', *, *, #125635, .F. ) ;
#46370 = VECTOR ( 'NONE', #83491, 1000.000000000000000 ) ;
#46372 = EDGE_CURVE ( 'NONE', #123433, #138081, #143152, .T. ) ;
#46373 = DIRECTION ( 'NONE',  ( 0.7071067811865486830, -0.7071067811865464625, -0.000000000000000000 ) ) ;
#46374 = CARTESIAN_POINT ( 'NONE',  ( 19.31706980810189123, -2.126176841940956130, 7.934999999999991616 ) ) ;
#46375 = ORIENTED_EDGE ( 'NONE', *, *, #117103, .F. ) ;
#46376 = CARTESIAN_POINT ( 'NONE',  ( 81.28709685856478018, 3.054999999999997939, 5.291415217122920289 ) ) ;
#46377 = CARTESIAN_POINT ( 'NONE',  ( 36.48921356237310221, -27.52281430457080802, 5.000000000000000000 ) ) ;
#46378 = EDGE_CURVE ( 'NONE', #126185, #35333, #140999, .T. ) ;
#46379 = CARTESIAN_POINT ( 'NONE',  ( -28.49999999999979750, 7.087461875839173864, 4.000000000000000000 ) ) ;
#46380 = VERTEX_POINT ( 'NONE', #32265 ) ;
#46381 = ORIENTED_EDGE ( 'NONE', *, *, #106117, .F. ) ;
#46382 = EDGE_LOOP ( 'NONE', ( #59414, #107361, #93535, #108544 ) ) ;
#46384 = VECTOR ( 'NONE', #8500, 1000.000000000000000 ) ;
#46383 = DIRECTION ( 'NONE',  ( 0.3543493200069162685, -0.000000000000000000, -0.9351131265310288487 ) ) ;
#46385 = LINE ( 'NONE', #79737, #94926 ) ;
#46386 = PLANE ( 'NONE',  #999 ) ;
#46387 = CARTESIAN_POINT ( 'NONE',  ( -6.792893218813405021, 15.75929247661555976, 5.000000000000000000 ) ) ;
#46388 = VERTEX_POINT ( 'NONE', #129414 ) ;
#46389 = CARTESIAN_POINT ( 'NONE',  ( 26.99999999999981526, 10.93112307739207267, 4.000000000000000000 ) ) ;
#46390 = VECTOR ( 'NONE', #141816, 999.9999999999998863 ) ;
#46391 = SURFACE_SIDE_STYLE ('',( #57255 ) ) ;
#46392 = FACE_OUTER_BOUND ( 'NONE', #39001, .T. ) ;
#46393 = MECHANICAL_DESIGN_GEOMETRIC_PRESENTATION_REPRESENTATION (  '', ( #53263 ), #65213 ) ;
#46394 = EDGE_LOOP ( 'NONE', ( #63649, #58260, #138176 ) ) ;
#46396 = VECTOR ( 'NONE', #31246, 1000.000000000000000 ) ;
#46395 = LINE ( 'NONE', #91986, #93374 ) ;
#46397 = EDGE_LOOP ( 'NONE', ( #87787, #120754, #69977, #76981 ) ) ;
#46400 = EDGE_CURVE ( 'NONE', #26635, #54672, #43148, .T. ) ;
#46399 = ORIENTED_EDGE ( 'NONE', *, *, #103297, .F. ) ;
#46398 = DIRECTION ( 'NONE',  ( -0.7071067811865486830, -0.7071067811865464625, 0.000000000000000000 ) ) ;
#46401 = ORIENTED_EDGE ( 'NONE', *, *, #104688, .T. ) ;
#46402 = AXIS2_PLACEMENT_3D ( 'NONE', #28716, #40318, #72960 ) ;
#46403 = DIRECTION ( 'NONE',  ( 1.000000000000000000, 0.000000000000000000, 0.000000000000000000 ) ) ;
#46404 = LINE ( 'NONE', #134093, #66945 ) ;
#46405 = EDGE_LOOP ( 'NONE', ( #27483, #16455, #58656, #37289 ) ) ;
#46406 = PRESENTATION_STYLE_ASSIGNMENT (( #57268 ) ) ;
#46407 = UNCERTAINTY_MEASURE_WITH_UNIT (LENGTH_MEASURE( 1.000000000000000082E-05 ), #4278, 'distance_accuracy_value', 'NONE');
#46408 = DIRECTION ( 'NONE',  ( -0.7071067811865486830, 0.7071067811865464625, 0.000000000000000000 ) ) ;
#46409 = CARTESIAN_POINT ( 'NONE',  ( 156.1499999999997783, -49.14999999999999147, -62.92499999999978400 ) ) ;
#46410 = EDGE_CURVE ( 'NONE', #98498, #60519, #64902, .T. ) ;
#46411 = FACE_OUTER_BOUND ( 'NONE', #37389, .T. ) ;
#46412 = VECTOR ( 'NONE', #83750, 1000.000000000000000 ) ;
#46413 = CARTESIAN_POINT ( 'NONE',  ( -25.39999999999996305, 0.000000000000000000, 2.500000000000000000 ) ) ;
#46414 = PLANE ( 'NONE',  #9482 ) ;
#46415 = DIRECTION ( 'NONE',  ( -0.7071067811865486830, 0.7071067811865464625, 0.000000000000000000 ) ) ;
#46416 = CARTESIAN_POINT ( 'NONE',  ( -36.48921356237310221, -27.52281430457080802, 5.000000000000000000 ) ) ;
#46417 = DIRECTION ( 'NONE',  ( 0.000000000000000000, -1.000000000000000000, -5.559056632600920815E-15 ) ) ;
#46419 = AXIS2_PLACEMENT_3D ( 'NONE', #135200, #38710, #46789 ) ;
#46418 = CARTESIAN_POINT ( 'NONE',  ( 20.83290314143522082, -3.967499999999994476, 6.871911579029513106 ) ) ;
#46420 = DIRECTION ( 'NONE',  ( 0.000000000000000000, 0.000000000000000000, 1.000000000000000000 ) ) ;
#46421 = DIRECTION ( 'NONE',  ( -0.7071067811865486830, -0.7071067811865464625, -0.000000000000000000 ) ) ;
#46422 = FACE_OUTER_BOUND ( 'NONE', #4159, .T. ) ;
#46423 = DIRECTION ( 'NONE',  ( -0.7071067811865487940, 0.7071067811865463515, -0.000000000000000000 ) ) ;
#46424 = ORIENTED_EDGE ( 'NONE', *, *, #128438, .F. ) ;
#46425 = ADVANCED_FACE ( 'NONE', ( #19934 ), #63368, .T. ) ;
#46426 = ORIENTED_EDGE ( 'NONE', *, *, #43472, .T. ) ;
#46427 = CARTESIAN_POINT ( 'NONE',  ( 96.37500000000000000, 7.950000000000000178, 1.460391307983218535E-15 ) ) ;
#46428 = EDGE_CURVE ( 'NONE', #138304, #113129, #75776, .T. ) ;
#46429 = ORIENTED_EDGE ( 'NONE', *, *, #66462, .F. ) ;
#46430 = ORIENTED_EDGE ( 'NONE', *, *, #125123, .F. ) ;
#46431 = ORIENTED_EDGE ( 'NONE', *, *, #88335, .T. ) ;
#46432 = CARTESIAN_POINT ( 'NONE',  ( 34.42499999999998295, -6.022814304570537125, 5.000000000000000000 ) ) ;
#46433 = PLANE ( 'NONE',  #76471 ) ;
#46434 = VECTOR ( 'NONE', #82524, 999.9999999999998863 ) ;
#46435 = CARTESIAN_POINT ( 'NONE',  ( 13.61855308952199195, 9.051029200191091917, 2.893811631854878996 ) ) ;
#46436 = ORIENTED_EDGE ( 'NONE', *, *, #69032, .F. ) ;
#46437 = DIRECTION ( 'NONE',  ( -0.7071067811865486830, -0.7071067811865464625, 0.000000000000000000 ) ) ;
#46438 = CARTESIAN_POINT ( 'NONE',  ( 23.99999999999983302, 7.007997736742463957, -8.085015511992057924 ) ) ;
#46439 = CARTESIAN_POINT ( 'NONE',  ( -16.92580874392868040, 8.754106587137664874, 4.662926800793050219 ) ) ;
#46440 = DIRECTION ( 'NONE',  ( 0.7071067811865487940, -0.7071067811865463515, 0.000000000000000000 ) ) ;
#46441 = EDGE_CURVE ( 'NONE', #136084, #110261, #63493, .T. ) ;
#46442 = CARTESIAN_POINT ( 'NONE',  ( 20.51078643762690490, -27.52281430457041012, 5.000000000000000000 ) ) ;
#46443 = DIRECTION ( 'NONE',  ( -0.3543493200069162685, -0.000000000000000000, -0.9351131265310288487 ) ) ;
#46444 = DIRECTION ( 'NONE',  ( -0.7071067811865487940, 0.7071067811865463515, 0.000000000000000000 ) ) ;
#46445 = LINE ( 'NONE', #58762, #89205 ) ;
#46446 = VECTOR ( 'NONE', #89519, 1000.000000000000000 ) ;
#46447 = CARTESIAN_POINT ( 'NONE',  ( 21.61838490601983409, -2.240707523384257716, 13.37739548510234400 ) ) ;
#46448 = CARTESIAN_POINT ( 'NONE',  ( 30.48921356237309510, -27.52281430457076894, 5.000000000000000000 ) ) ;
#46449 = CLOSED_SHELL ( 'NONE', ( #43817, #124202, #81158, #121822, #73485, #95849 ) ) ;
#46450 = CARTESIAN_POINT ( 'NONE',  ( 26.45376352523144803, -6.109999999999998543, -3.741295971395162543E-16 ) ) ;
#46451 = DIRECTION ( 'NONE',  ( 0.000000000000000000, -1.000000000000000000, 0.000000000000000000 ) ) ;
#46452 = ORIENTED_EDGE ( 'NONE', *, *, #73533, .T. ) ;
#46453 = ORIENTED_EDGE ( 'NONE', *, *, #94565, .T. ) ;
#46454 = CARTESIAN_POINT ( 'NONE',  ( 109.0837635252314470, -6.110000000000001208, -3.741295971395164515E-16 ) ) ;
#46455 = EDGE_LOOP ( 'NONE', ( #93738, #136765, #82072 ) ) ;
#46456 = DIRECTION ( 'NONE',  ( -0.6830127018922181881, 0.6830127018922202975, -0.2588190451025214056 ) ) ;
#46457 = VECTOR ( 'NONE', #110272, 1000.000000000000000 ) ;
#46458 = CARTESIAN_POINT ( 'NONE',  ( 0.000000000000000000, 0.000000000000000000, 5.000000000000000000 ) ) ;
#46459 = DIRECTION ( 'NONE',  ( -0.7071067811865486830, -0.7071067811865464625, 0.000000000000000000 ) ) ;
#46460 = VECTOR ( 'NONE', #98517, 1000.000000000000227 ) ;
#46461 = AXIS2_PLACEMENT_3D ( 'NONE', #48054, #105269, #93690 ) ;
#46462 = CARTESIAN_POINT ( 'NONE',  ( 110.0162635252314374, -4.472830434245839371, 4.472830434245839371 ) ) ;
#46463 = EDGE_CURVE ( 'NONE', #74571, #114684, #78159, .T. ) ;
#46464 = VERTEX_POINT ( 'NONE', #98237 ) ;
#46465 = EDGE_CURVE ( 'NONE', #118785, #16702, #81892, .T. ) ;
#46466 = ORIENTED_EDGE ( 'NONE', *, *, #68927, .F. ) ;
#46467 = CARTESIAN_POINT ( 'NONE',  ( 8.968407645496675684, 2.500000000000000888, 3.061616997868383141E-16 ) ) ;
#46468 = EDGE_CURVE ( 'NONE', #75609, #124219, #99635, .T. ) ;
#46469 = VECTOR ( 'NONE', #138195, 1000.000000000000000 ) ;
#46470 = VECTOR ( 'NONE', #136193, 1000.000000000000000 ) ;
#46471 = LINE ( 'NONE', #78344, #73266 ) ;
#46472 = AXIS2_PLACEMENT_3D ( 'NONE', #78773, #120821, #66475 ) ;
#46473 = ORIENTED_EDGE ( 'NONE', *, *, #103877, .T. ) ;
#46474 = VERTEX_POINT ( 'NONE', #110500 ) ;
#46475 = ORIENTED_EDGE ( 'NONE', *, *, #137310, .F. ) ;
#46476 = DIRECTION ( 'NONE',  ( -0.000000000000000000, -0.3543493200069152693, 0.9351131265310292928 ) ) ;
#46477 = EDGE_CURVE ( 'NONE', #64566, #57564, #11171, .T. ) ;
#46478 = CARTESIAN_POINT ( 'NONE',  ( 33.79289321881321939, -8.240707523384195099, 5.000000000000000000 ) ) ;
#46479 = CIRCLE ( 'NONE', #90405, 1.000000000000000888 ) ;
#46480 = EDGE_CURVE ( 'NONE', #63651, #122408, #40994, .T. ) ;
#46481 = EDGE_CURVE ( 'NONE', #100660, #116780, #52571, .T. ) ;
#46482 = CARTESIAN_POINT ( 'NONE',  ( 32.87043019189811588, -3.055000000000001492, 5.291415217122917625 ) ) ;
#46483 = EDGE_CURVE ( 'NONE', #96125, #35696, #30851, .T. ) ;
#46484 = VERTEX_POINT ( 'NONE', #90945 ) ;
#46485 = ORIENTED_EDGE ( 'NONE', *, *, #30257, .T. ) ;
#46487 = EDGE_CURVE ( 'NONE', #47828, #63098, #69929, .T. ) ;
#46486 = DIRECTION ( 'NONE',  ( 0.7071067811865487940, -0.7071067811865463515, 0.000000000000000000 ) ) ;
#46488 = ORIENTED_EDGE ( 'NONE', *, *, #9114, .T. ) ;
#46489 = EDGE_LOOP ( 'NONE', ( #50905, #78752, #103519, #55474 ) ) ;
#46490 = CIRCLE ( 'NONE', #62705, 0.5000000000000000000 ) ;
#46491 = VERTEX_POINT ( 'NONE', #80775 ) ;
#46492 = EDGE_CURVE ( 'NONE', #83424, #106324, #113367, .T. ) ;
#46493 = PLANE ( 'NONE',  #19327 ) ;
#46494 = VECTOR ( 'NONE', #55728, 1000.000000000000227 ) ;
#46495 = EDGE_CURVE ( 'NONE', #15784, #121472, #46763, .T. ) ;
#46497 = DIRECTION ( 'NONE',  ( 0.000000000000000000, 0.000000000000000000, -1.000000000000000000 ) ) ;
#46496 = AXIS2_PLACEMENT_3D ( 'NONE', #60217, #73233, #49359 ) ;
#46498 = CARTESIAN_POINT ( 'NONE',  ( 9.748407645496676821, 9.139736423841732040E-16, 0.000000000000000000 ) ) ;
#46499 = ORIENTED_EDGE ( 'NONE', *, *, #41397, .F. ) ;
#46500 = DIRECTION ( 'NONE',  ( -0.6830127018922181881, 0.6830127018922202975, -0.2588190451025214056 ) ) ;
#46501 = EDGE_CURVE ( 'NONE', #131882, #53582, #101066, .T. ) ;
#46502 = AXIS2_PLACEMENT_3D ( 'NONE', #101648, #90052, #92187 ) ;
#46503 = FACE_OUTER_BOUND ( 'NONE', #121053, .T. ) ;
#46504 = VECTOR ( 'NONE', #129252, 999.9999999999998863 ) ;
#46505 = EDGE_CURVE ( 'NONE', #80270, #112794, #79381, .T. ) ;
#46506 = FACE_BOUND ( 'NONE', #73482, .T. ) ;
#46507 = VERTEX_POINT ( 'NONE', #134442 ) ;
#46508 = EDGE_CURVE ( 'NONE', #133473, #97018, #80082, .T. ) ;
#46509 = DIRECTION ( 'NONE',  ( -0.000000000000000000, 0.000000000000000000, 1.000000000000000000 ) ) ;
#46510 = CARTESIAN_POINT ( 'NONE',  ( 12.29974487139158512, -27.71228299555214747, 4.000000000000000000 ) ) ;
#46511 = VECTOR ( 'NONE', #74177, 1000.000000000000000 ) ;
#46512 = DIRECTION ( 'NONE',  ( 0.000000000000000000, -1.000000000000000000, 0.000000000000000000 ) ) ;
#46513 = LINE ( 'NONE', #66088, #50907 ) ;
#46514 = ORIENTED_EDGE ( 'NONE', *, *, #88380, .T. ) ;
#46515 = DIRECTION ( 'NONE',  ( 0.6830127018922180770, -0.6830127018922204085, -0.2588190451025213501 ) ) ;
#46516 = ORIENTED_EDGE ( 'NONE', *, *, #9560, .T. ) ;
#46517 = VERTEX_POINT ( 'NONE', #133029 ) ;
#46518 = ADVANCED_FACE ( 'NONE', ( #59058 ), #1721, .T. ) ;
#46519 = ORIENTED_EDGE ( 'NONE', *, *, #81818, .F. ) ;
#46520 = CARTESIAN_POINT ( 'NONE',  ( 51.24543019189811588, -5.291415217122918513, -3.055000000000000160 ) ) ;
#46521 = ORIENTED_EDGE ( 'NONE', *, *, #15910, .T. ) ;
#46522 = AXIS2_PLACEMENT_3D ( 'NONE', #19786, #64731, #9607 ) ;
#46523 = DIRECTION ( 'NONE',  ( -0.7071067811865486830, -0.7071067811865464625, -0.000000000000000000 ) ) ;
#46524 = PLANE ( 'NONE',  #100639 ) ;
#46525 = ORIENTED_EDGE ( 'NONE', *, *, #140228, .F. ) ;
#46526 = LINE ( 'NONE', #70422, #103787 ) ;
#46528 = CARTESIAN_POINT ( 'NONE',  ( -66.29974487139159578, -27.71228299555252406, 4.000000000000000000 ) ) ;
#46527 = AXIS2_PLACEMENT_3D ( 'NONE', #70336, #136971, #102923 ) ;
#46529 = SURFACE_STYLE_FILL_AREA ( #66 ) ;
#46530 = CARTESIAN_POINT ( 'NONE',  ( 11.99999999999992362, -3.485240976185064010, -4.108735105802371557 ) ) ;
#46531 = PLANE ( 'NONE',  #43636 ) ;
#46532 = CARTESIAN_POINT ( 'NONE',  ( 1.499999999999996225, 3.052185695429134871, 5.000000000000000000 ) ) ;
#46533 = VERTEX_POINT ( 'NONE', #24933 ) ;
#46534 = ADVANCED_FACE ( 'NONE', ( #57605 ), #46014, .T. ) ;
#46535 = VERTEX_POINT ( 'NONE', #122104 ) ;
#46536 = EDGE_LOOP ( 'NONE', ( #57134, #102186, #78199, #56232 ) ) ;
#46537 = VECTOR ( 'NONE', #133184, 1000.000000000000227 ) ;
#46538 = VERTEX_POINT ( 'NONE', #135856 ) ;
#46539 = CARTESIAN_POINT ( 'NONE',  ( -5.700255128608413102, -27.71228299555201957, 4.000000000000000000 ) ) ;
#46540 = EDGE_LOOP ( 'NONE', ( #121553, #14847, #62291, #44921 ) ) ;
#46541 = EDGE_LOOP ( 'NONE', ( #119703, #95727, #33322, #116391 ) ) ;
#46542 = DIRECTION ( 'NONE',  ( -0.6830127018922180770, -0.6830127018922204085, -0.2588190451025213501 ) ) ;
#46543 = DIRECTION ( 'NONE',  ( 0.7071067811865486830, -0.7071067811865464625, -0.000000000000000000 ) ) ;
#46544 = VERTEX_POINT ( 'NONE', #112668 ) ;
#46545 = DIRECTION ( 'NONE',  ( 0.7071067811865487940, 0.7071067811865463515, 0.000000000000000000 ) ) ;
#46546 = AXIS2_PLACEMENT_3D ( 'NONE', #84384, #107525, #32115 ) ;
#46547 = VECTOR ( 'NONE', #22413, 1000.000000000000227 ) ;
#46548 = EDGE_CURVE ( 'NONE', #141894, #36014, #142004, .T. ) ;
#46549 = DIRECTION ( 'NONE',  ( 0.3543493200069163240, 0.000000000000000000, 0.9351131265310288487 ) ) ;
#46550 = CARTESIAN_POINT ( 'NONE',  ( 25.44206980810188412, 7.934999999999993392, 2.126176841940951689 ) ) ;
#46551 = CARTESIAN_POINT ( 'NONE',  ( 7.499999999999952927, -7.912538124160680475, 4.000000000000000000 ) ) ;
#46552 = EDGE_LOOP ( 'NONE', ( #132522, #75659, #9379, #83802, #139733 ) ) ;
#46554 = CARTESIAN_POINT ( 'NONE',  ( 42.29974487139158157, -27.71228299555235708, 4.000000000000000000 ) ) ;
#46553 = CARTESIAN_POINT ( 'NONE',  ( 112.9329301918981230, 1.637169565754156730, 6.110000000000001208 ) ) ;
#46556 = EDGE_CURVE ( 'NONE', #114516, #105099, #124258, .T. ) ;
#46555 = PLANE ( 'NONE',  #111505 ) ;
#46557 = CARTESIAN_POINT ( 'NONE',  ( 12.52400138585440459, 22.03583458319438648, 4.979811245910089390 ) ) ;
#46558 = ORIENTED_EDGE ( 'NONE', *, *, #92997, .F. ) ;
#46559 = FACE_OUTER_BOUND ( 'NONE', #1348, .T. ) ;
#46561 = VERTEX_POINT ( 'NONE', #135171 ) ;
#46560 = CARTESIAN_POINT ( 'NONE',  ( -17.92867102513379862, 9.037728232668255757, 5.000000000000000000 ) ) ;
#46562 = FACE_OUTER_BOUND ( 'NONE', #96310, .T. ) ;
#46563 = VERTEX_POINT ( 'NONE', #47468 ) ;
#46564 = CARTESIAN_POINT ( 'NONE',  ( -19.93032425809868258, -22.22500000000000142, -0.6820431690203968556 ) ) ;
#46565 = VECTOR ( 'NONE', #116019, 1000.000000000000000 ) ;
#46566 = LINE ( 'NONE', #124782, #86367 ) ;
#46567 = CARTESIAN_POINT ( 'NONE',  ( 121.1666666666666714, 6.884901960086285300, 3.975000000000003642 ) ) ;
#46568 = ORIENTED_EDGE ( 'NONE', *, *, #64101, .T. ) ;
#46569 = AXIS2_PLACEMENT_3D ( 'NONE', #91073, #57729, #10604 ) ;
#46570 = PLANE ( 'NONE',  #113048 ) ;
#46571 = EDGE_CURVE ( 'NONE', #134283, #82053, #22761, .T. ) ;
#46572 = PLANE ( 'NONE',  #139158 ) ;
#46573 = CARTESIAN_POINT ( 'NONE',  ( 5.999999999999958256, -12.03360074219761877, 5.000000000000000000 ) ) ;
#46574 = ORIENTED_EDGE ( 'NONE', *, *, #72425, .F. ) ;
#46575 = AXIS2_PLACEMENT_3D ( 'NONE', #25639, #125694, #137278 ) ;
#46576 = VECTOR ( 'NONE', #40848, 999.9999999999998863 ) ;
#46577 = AXIS2_PLACEMENT_3D ( 'NONE', #21024, #143529, #74000 ) ;
#46578 = VECTOR ( 'NONE', #12177, 1000.000000000000000 ) ;
#46579 = DIRECTION ( 'NONE',  ( -0.7071067811865487940, 0.7071067811865463515, 0.000000000000000000 ) ) ;
#46581 = EDGE_LOOP ( 'NONE', ( #70200, #135411, #27574, #46609 ) ) ;
#46580 = PRESENTATION_LAYER_ASSIGNMENT (  '', '', ( #109003 ) ) ;
#46582 = FACE_OUTER_BOUND ( 'NONE', #102354, .T. ) ;
#46585 = EDGE_CURVE ( 'NONE', #77789, #128763, #14784, .T. ) ;
#46584 = VERTEX_POINT ( 'NONE', #23513 ) ;
#46583 = DIRECTION ( 'NONE',  ( -0.6830127018922180770, -0.6830127018922204085, -0.2588190451025213501 ) ) ;
#46586 = VERTEX_POINT ( 'NONE', #88800 ) ;
#46587 = CARTESIAN_POINT ( 'NONE',  ( 14.99999999999989519, 19.93112307739198386, 4.000000000000000000 ) ) ;
#46588 = VECTOR ( 'NONE', #143220, 1000.000000000000000 ) ;
#46589 = DIRECTION ( 'NONE',  ( -0.000000000000000000, 0.3543493200069153248, 0.9351131265310292928 ) ) ;
#46590 = ORIENTED_EDGE ( 'NONE', *, *, #68063, .T. ) ;
#46591 = CARTESIAN_POINT ( 'NONE',  ( -16.49999999999987921, -4.912538124160701791, 4.000000000000000000 ) ) ;
#46592 = ORIENTED_EDGE ( 'NONE', *, *, #1009, .T. ) ;
#46593 = AXIS2_PLACEMENT_3D ( 'NONE', #89410, #46680, #12550 ) ;
#46594 = DIRECTION ( 'NONE',  ( -0.7071067811865486830, -0.7071067811865464625, -0.000000000000000000 ) ) ;
#46595 = DIRECTION ( 'NONE',  ( -0.7071067811865487940, 0.7071067811865463515, 0.000000000000000000 ) ) ;
#46596 = LINE ( 'NONE', #34974, #42416 ) ;
#46597 = VECTOR ( 'NONE', #62961, 1000.000000000000000 ) ;
#46598 = LINE ( 'NONE', #69760, #102685 ) ;
#46599 = LINE ( 'NONE', #111805, #6594 ) ;
#46600 = CARTESIAN_POINT ( 'NONE',  ( 31.63753812416075917, 22.22500000000000142, 4.000000000000000000 ) ) ;
#46601 = ORIENTED_EDGE ( 'NONE', *, *, #110254, .T. ) ;
#46602 = CIRCLE ( 'NONE', #92899, 3.000000000000002665 ) ;
#46603 = ORIENTED_EDGE ( 'NONE', *, *, #89851, .T. ) ;
#46604 = ORIENTED_EDGE ( 'NONE', *, *, #83521, .F. ) ;
#46605 = CARTESIAN_POINT ( 'NONE',  ( 123.9375000000000142, 5.819803920172573974, -5.819803920172572198 ) ) ;
#46606 = VECTOR ( 'NONE', #100439, 1000.000000000000227 ) ;
#46607 = EDGE_CURVE ( 'NONE', #18811, #21087, #67037, .T. ) ;
#46608 = ORIENTED_EDGE ( 'NONE', *, *, #2889, .T. ) ;
#46609 = ORIENTED_EDGE ( 'NONE', *, *, #16222, .F. ) ;
#46610 = VECTOR ( 'NONE', #4142, 1000.000000000000114 ) ;
#46611 = ORIENTED_EDGE ( 'NONE', *, *, #47306, .T. ) ;
#46612 = CARTESIAN_POINT ( 'NONE',  ( 0.9370758337544541350, -5.958929145428653484, -3.977263664294321099 ) ) ;
#46613 = CARTESIAN_POINT ( 'NONE',  ( 23.28242261357416254, -21.73023691814493574, 5.000000000000000888 ) ) ;
#46614 = VECTOR ( 'NONE', #82068, 1000.000000000000000 ) ;
#46615 = ORIENTED_EDGE ( 'NONE', *, *, #37435, .F. ) ;
#46616 = CARTESIAN_POINT ( 'NONE',  ( -30.18398860626900060, 28.73617430169808173, 5.000000000000000000 ) ) ;
#46617 = CARTESIAN_POINT ( 'NONE',  ( 0.000000000000000000, 0.000000000000000000, 9.407735506486140764 ) ) ;
#46618 = DIRECTION ( 'NONE',  ( -0.7071067811865487940, 0.7071067811865463515, -0.000000000000000000 ) ) ;
#46619 = CARTESIAN_POINT ( 'NONE',  ( -26.89452376399129818, 22.22500000000000142, 8.043047640789337649 ) ) ;
#46620 = CARTESIAN_POINT ( 'NONE',  ( 125.2712635252314470, 4.472830434245839371, 4.472830434245842035 ) ) ;
#46621 = VECTOR ( 'NONE', #70486, 1000.000000000000227 ) ;
#46622 = ORIENTED_EDGE ( 'NONE', *, *, #24228, .F. ) ;
#46623 = EDGE_CURVE ( 'NONE', #117264, #103756, #56198, .T. ) ;
#46624 = DIRECTION ( 'NONE',  ( 0.7071067811865486830, -0.7071067811865464625, -0.000000000000000000 ) ) ;
#46625 = CARTESIAN_POINT ( 'NONE',  ( 104.9333603837962272, 2.130196079827431532, -7.949999999999996625 ) ) ;
#46626 = FACE_OUTER_BOUND ( 'NONE', #112292, .T. ) ;
#46627 = CARTESIAN_POINT ( 'NONE',  ( 0.3243279295976794208, 5.567135860803324121, -5.437310639911629551 ) ) ;
#46628 = CARTESIAN_POINT ( 'NONE',  ( 1.499999999999991340, -19.91253812416055169, 4.000000000000000000 ) ) ;
#46629 = CARTESIAN_POINT ( 'NONE',  ( 3.005480084712505828, 28.92564299267936079, 4.000000000000000000 ) ) ;
#46630 = CARTESIAN_POINT ( 'NONE',  ( 12.48921356237309155, -27.52281430457064104, 5.000000000000000000 ) ) ;
#46631 = PRODUCT_DEFINITION ( 'UNKNOWN', '', #93384, #135774 ) ;
#46632 = CARTESIAN_POINT ( 'NONE',  ( 48.49586038379622011, -3.974999999999998312, -6.884901960086286188 ) ) ;
#46633 = CARTESIAN_POINT ( 'NONE',  ( 17.67183060077634593, -21.74070752338406010, 4.000000000000000000 ) ) ;
#46634 = LINE ( 'NONE', #111084, #57759 ) ;
#46635 = AXIS2_PLACEMENT_3D ( 'NONE', #20033, #31654, #8415 ) ;
#46636 = ORIENTED_EDGE ( 'NONE', *, *, #41495, .F. ) ;
#46637 = ORIENTED_EDGE ( 'NONE', *, *, #54130, .T. ) ;
#46638 = CARTESIAN_POINT ( 'NONE',  ( 44.60416666666665719, 2.130196079827422206, 7.950000000000001954 ) ) ;
#46639 = ORIENTED_EDGE ( 'NONE', *, *, #56028, .F. ) ;
#46640 = LINE ( 'NONE', #132908, #124906 ) ;
#46641 = ORIENTED_EDGE ( 'NONE', *, *, #92626, .T. ) ;
#46642 = CIRCLE ( 'NONE', #74438, 2.055000000000001048 ) ;
#46643 = DIRECTION ( 'NONE',  ( 0.6830127018922180770, -0.6830127018922204085, -0.2588190451025213501 ) ) ;
#46644 = CARTESIAN_POINT ( 'NONE',  ( 0.000000000000000000, 0.000000000000000000, 5.000000000000000000 ) ) ;
#46645 = CARTESIAN_POINT ( 'NONE',  ( 40.68793019189811133, 6.110000000000002984, -1.637169565754156730 ) ) ;
#46646 = ORIENTED_EDGE ( 'NONE', *, *, #98653, .F. ) ;
#46647 = LINE ( 'NONE', #26973, #36320 ) ;
#46648 = ORIENTED_EDGE ( 'NONE', *, *, #11572, .F. ) ;
#46649 = CIRCLE ( 'NONE', #65138, 5.968999999999998529 ) ;
#46650 = CARTESIAN_POINT ( 'NONE',  ( 5.999999999999967137, 14.58746187583909837, 4.000000000000000000 ) ) ;
#46651 = DIRECTION ( 'NONE',  ( 0.7071067811865487940, 0.7071067811865463515, 0.000000000000000000 ) ) ;
#46652 = FACE_OUTER_BOUND ( 'NONE', #114053, .T. ) ;
#46653 = FACE_OUTER_BOUND ( 'NONE', #101493, .T. ) ;
#46654 = ORIENTED_EDGE ( 'NONE', *, *, #88000, .F. ) ;
#46655 = DIRECTION ( 'NONE',  ( -0.3543493200069162685, -0.000000000000000000, -0.9351131265310288487 ) ) ;
#46656 = EDGE_LOOP ( 'NONE', ( #143449, #65984, #79151, #77401 ) ) ;
#46657 = CARTESIAN_POINT ( 'NONE',  ( -4.214984197241873787, -3.740707523384244837, 15.76143240460122996 ) ) ;
#46658 = LINE ( 'NONE', #45214, #80930 ) ;
#46659 = CARTESIAN_POINT ( 'NONE',  ( 5.510786437626906675, -27.52281430457051314, 5.000000000000000000 ) ) ;
#46660 = VECTOR ( 'NONE', #94865, 1000.000000000000114 ) ;
#46661 = CARTESIAN_POINT ( 'NONE',  ( 1.353980332882009252, 4.584330080086930965E-16, 0.000000000000000000 ) ) ;
#46662 = EDGE_CURVE ( 'NONE', #124524, #139884, #133723, .T. ) ;
#46663 = DIRECTION ( 'NONE',  ( 0.000000000000000000, -1.000000000000000000, 0.000000000000000000 ) ) ;
#46664 = CARTESIAN_POINT ( 'NONE',  ( 56.05793019189811588, 6.110000000000000320, -1.637169565754156064 ) ) ;
#46665 = EDGE_CURVE ( 'NONE', #46724, #55424, #78624, .T. ) ;
#46666 = MANIFOLD_SOLID_BREP ( 'Boss-Extrude1', #44023 ) ;
#46667 = DIRECTION ( 'NONE',  ( 1.000000000000000000, 1.224606353822377258E-16, 0.000000000000000000 ) ) ;
#46669 = EDGE_CURVE ( 'NONE', #100009, #72242, #16176, .T. ) ;
#46668 = DIRECTION ( 'NONE',  ( 0.7071067811865487940, 0.7071067811865463515, 0.000000000000000000 ) ) ;
#46671 = EDGE_LOOP ( 'NONE', ( #12197, #49791, #5633, #8462 ) ) ;
#46670 = CARTESIAN_POINT ( 'NONE',  ( 34.47516574401890921, 7.490517612115553447, 4.998110765256835286 ) ) ;
#46672 = ORIENTED_EDGE ( 'NONE', *, *, #91892, .F. ) ;
#46673 = DIRECTION ( 'NONE',  ( 0.7071067811865487940, 0.7071067811865463515, -0.000000000000000000 ) ) ;
#46674 = CIRCLE ( 'NONE', #35053, 0.5000000000000004441 ) ;
#46675 = ORIENTED_EDGE ( 'NONE', *, *, #31040, .F. ) ;
#46676 = EDGE_CURVE ( 'NONE', #108717, #44302, #84360, .T. ) ;
#46677 =( BOUNDED_CURVE ( )  B_SPLINE_CURVE ( 3, ( #104243, #8313, #7615, #140296 ),
 .UNSPECIFIED., .F., .F. ) 
 B_SPLINE_CURVE_WITH_KNOTS ( ( 4, 4 ),
 ( 1.208578181583237710, 1.359146454359485334 ),
 .UNSPECIFIED. ) 
 CURVE ( )  GEOMETRIC_REPRESENTATION_ITEM ( )  RATIONAL_B_SPLINE_CURVE ( ( 1.000000000000000000, 0.9981116584018941973, 0.9981116584018941973, 1.000000000000000000 ) ) 
 REPRESENTATION_ITEM ( '' )  );
#46678 = AXIS2_PLACEMENT_3D ( 'NONE', #30810, #75036, #19890 ) ;
#46679 = VECTOR ( 'NONE', #77327, 1000.000000000000000 ) ;
#46680 = DIRECTION ( 'NONE',  ( 0.6830127018922181881, 0.6830127018922202975, -0.2588190451025214056 ) ) ;
#46681 = EDGE_LOOP ( 'NONE', ( #111670, #4990, #121154, #105504 ) ) ;
#46682 = CARTESIAN_POINT ( 'NONE',  ( 23.99999999999984013, -22.06887692260758982, 4.000000000000000000 ) ) ;
#46683 = VECTOR ( 'NONE', #47811, 1000.000000000000000 ) ;
#46684 = VECTOR ( 'NONE', #31049, 1000.000000000000000 ) ;
#46685 = AXIS2_PLACEMENT_3D ( 'NONE', #100877, #47963, #2982 ) ;
#46686 = CARTESIAN_POINT ( 'NONE',  ( -20.99999999999986144, -13.06887692260767686, 4.000000000000000000 ) ) ;
#46687 = ADVANCED_FACE ( 'NONE', ( #49593 ), #4553, .F. ) ;
#46688 = FACE_BOUND ( 'NONE', #66448, .T. ) ;
#46689 = ADVANCED_FACE ( 'NONE', ( #93777 ), #4257, .F. ) ;
#46690 = LINE ( 'NONE', #111140, #20198 ) ;
#46691 = CARTESIAN_POINT ( 'NONE',  ( 20.65000000000000213, 0.000000000000000000, 0.000000000000000000 ) ) ;
#46693 = CARTESIAN_POINT ( 'NONE',  ( 42.48921356237308800, -27.52281430457085065, 5.000000000000000000 ) ) ;
#46692 = VECTOR ( 'NONE', #19826, 1000.000000000000000 ) ;
#46695 = VERTEX_POINT ( 'NONE', #103209 ) ;
#46694 = DIRECTION ( 'NONE',  ( -0.7071067811865487940, 0.7071067811865463515, 0.000000000000000000 ) ) ;
#46696 = VERTEX_POINT ( 'NONE', #137294 ) ;
#46697 = CARTESIAN_POINT ( 'NONE',  ( -8.700255128608413102, -27.71228299555199825, 4.000000000000000000 ) ) ;
#46698 = EDGE_CURVE ( 'NONE', #29986, #29217, #128551, .T. ) ;
#46699 = VERTEX_POINT ( 'NONE', #83645 ) ;
#46700 = EDGE_LOOP ( 'NONE', ( #19061, #32962, #60187, #56815 ) ) ;
#46701 = CARTESIAN_POINT ( 'NONE',  ( 73.55793019189812298, 6.110000000000000320, -1.637169565754156064 ) ) ;
#46702 = ORIENTED_EDGE ( 'NONE', *, *, #10968, .F. ) ;
#46703 = VECTOR ( 'NONE', #92789, 1000.000000000000227 ) ;
#46704 = CARTESIAN_POINT ( 'NONE',  ( 14.99451991528749595, 28.92564299267948513, 4.000000000000000000 ) ) ;
#46705 = EDGE_LOOP ( 'NONE', ( #45889, #23730, #8416, #68878 ) ) ;
#46706 = DIRECTION ( 'NONE',  ( -0.6830127018922180770, -0.6830127018922204085, -0.2588190451025213501 ) ) ;
#46707 = EDGE_CURVE ( 'NONE', #106116, #5533, #27080, .T. ) ;
#46708 = AXIS2_PLACEMENT_3D ( 'NONE', #95650, #28276, #18798 ) ;
#46709 = LINE ( 'NONE', #134385, #24112 ) ;
#46710 = AXIS2_PLACEMENT_3D ( 'NONE', #138980, #139713, #107744 ) ;
#46711 = CARTESIAN_POINT ( 'NONE',  ( -4.499999999999962697, -19.91253812416055524, 4.000000000000000000 ) ) ;
#46712 = CARTESIAN_POINT ( 'NONE',  ( 0.000000000000000000, -4.870000000000014317, -40.00000000000000000 ) ) ;
#46713 = CARTESIAN_POINT ( 'NONE',  ( 0.000000000000000000, 0.000000000000000000, 0.000000000000000000 ) ) ;
#46714 = AXIS2_PLACEMENT_3D ( 'NONE', #61843, #27755, #48820 ) ;
#46715 = CARTESIAN_POINT ( 'NONE',  ( -20.99999999999985079, 10.55218569542906160, 5.000000000000000000 ) ) ;
#46716 = DIRECTION ( 'NONE',  ( -0.7071067811865487940, 0.7071067811865463515, 0.000000000000000000 ) ) ;
#46717 = VERTEX_POINT ( 'NONE', #26389 ) ;
#46718 = EDGE_CURVE ( 'NONE', #56823, #99997, #50283, .T. ) ;
#46719 = ORIENTED_EDGE ( 'NONE', *, *, #78578, .F. ) ;
#46720 = AXIS2_PLACEMENT_3D ( 'NONE', #131793, #42664, #32483 ) ;
#46721 = CARTESIAN_POINT ( 'NONE',  ( 25.00051279177633390, 3.647752439586039230, 4.157751055492739489 ) ) ;
#46722 = CARTESIAN_POINT ( 'NONE',  ( -12.29974487139158512, -27.71228299555214747, 4.000000000000000000 ) ) ;
#46723 = ORIENTED_EDGE ( 'NONE', *, *, #47878, .T. ) ;
#46724 = VERTEX_POINT ( 'NONE', #115480 ) ;
#46725 = ORIENTED_EDGE ( 'NONE', *, *, #73313, .F. ) ;
#46726 = VECTOR ( 'NONE', #107528, 1000.000000000000000 ) ;
#46727 = CARTESIAN_POINT ( 'NONE',  ( 28.72959685856476852, -6.110000000000000320, -1.637169565754161393 ) ) ;
#46728 = ORIENTED_EDGE ( 'NONE', *, *, #23235, .F. ) ;
#46729 = LINE ( 'NONE', #45979, #71764 ) ;
#46730 = EDGE_CURVE ( 'NONE', #143241, #26004, #41361, .T. ) ;
#46731 = CARTESIAN_POINT ( 'NONE',  ( 2.108736474768552860, -5.808823158059033709, 5.808823158059035485 ) ) ;
#46732 = CARTESIAN_POINT ( 'NONE',  ( 14.88812247636860064, 4.294539510182263875, -29.64274772238085021 ) ) ;
#46733 = VERTEX_POINT ( 'NONE', #6007 ) ;
#46734 = DIRECTION ( 'NONE',  ( 0.3543493200069162685, -0.000000000000000000, -0.9351131265310288487 ) ) ;
#46735 = CARTESIAN_POINT ( 'NONE',  ( 119.2250270504628986, 5.819803920172573974, -5.819803920172573086 ) ) ;
#46736 = VECTOR ( 'NONE', #142871, 1000.000000000000000 ) ;
#46737 = CARTESIAN_POINT ( 'NONE',  ( -29.29387692260784348, 22.22500000000000142, 4.000000000000000000 ) ) ;
#46739 = ORIENTED_EDGE ( 'NONE', *, *, #111556, .F. ) ;
#46738 = FACE_OUTER_BOUND ( 'NONE', #44617, .T. ) ;
#46740 = AXIS2_PLACEMENT_3D ( 'NONE', #106588, #140668, #119611 ) ;
#46741 = ORIENTED_EDGE ( 'NONE', *, *, #112507, .F. ) ;
#46742 = DIRECTION ( 'NONE',  ( -0.7071067811865486830, -0.7071067811865464625, 0.000000000000000000 ) ) ;
#46743 = CARTESIAN_POINT ( 'NONE',  ( -6.722814304570563948, -21.72499999999999432, 5.000000000000000000 ) ) ;
#46744 = LINE ( 'NONE', #90925, #56424 ) ;
#46745 = ORIENTED_EDGE ( 'NONE', *, *, #57015, .F. ) ;
#46746 = CYLINDRICAL_SURFACE ( 'NONE', #11099, 2.247899999999996901 ) ;
#46747 = CARTESIAN_POINT ( 'NONE',  ( 57.29974487139158157, -27.71228299555246011, 4.000000000000000000 ) ) ;
#46748 = EDGE_CURVE ( 'NONE', #58598, #142779, #48305, .T. ) ;
#46749 = PRESENTATION_STYLE_ASSIGNMENT (( #101774 ) ) ;
#46750 = DIRECTION ( 'NONE',  ( -0.7071067811865486830, 0.7071067811865464625, 0.000000000000000000 ) ) ;
#46751 = LINE ( 'NONE', #46002, #75054 ) ;
#46752 = VECTOR ( 'NONE', #134988, 1000.000000000000000 ) ;
#46753 = LINE ( 'NONE', #124250, #124975 ) ;
#46754 = DIRECTION ( 'NONE',  ( 0.7071067811865486830, -0.7071067811865464625, -0.000000000000000000 ) ) ;
#46755 = CARTESIAN_POINT ( 'NONE',  ( 21.62913961620377279, 5.278424836066147208, 3.047499999999990550 ) ) ;
#46756 = FACE_OUTER_BOUND ( 'NONE', #95705, .T. ) ;
#46757 = LINE ( 'NONE', #90941, #78467 ) ;
#46759 = ADVANCED_FACE ( 'NONE', ( #95188 ), #82220, .T. ) ;
#46758 = ORIENTED_EDGE ( 'NONE', *, *, #65072, .F. ) ;
#46760 = ORIENTED_EDGE ( 'NONE', *, *, #103276, .F. ) ;
#46761 = CIRCLE ( 'NONE', #123089, 5.968999999999998529 ) ;
#46762 =( LENGTH_UNIT ( ) NAMED_UNIT ( * ) SI_UNIT ( .MILLI., .METRE. ) );
#46763 = LINE ( 'NONE', #2453, #97995 ) ;
#46764 = SURFACE_STYLE_USAGE ( .BOTH. , #1722 ) ;
#46765 = CARTESIAN_POINT ( 'NONE',  ( 66.28752705046289861, 0.000000000000000000, -7.949999999999998401 ) ) ;
#46766 = DIRECTION ( 'NONE',  ( -0.7071067811865487940, 0.7071067811865463515, 0.000000000000000000 ) ) ;
#46767 = FACE_OUTER_BOUND ( 'NONE', #80415, .T. ) ;
#46768 =( NAMED_UNIT ( * ) PLANE_ANGLE_UNIT ( ) SI_UNIT ( $, .RADIAN. ) );
#46769 = VERTEX_POINT ( 'NONE', #15454 ) ;
#46770 = DIRECTION ( 'NONE',  ( -1.000000000000000000, -0.000000000000000000, 0.000000000000000000 ) ) ;
#46771 = DIRECTION ( 'NONE',  ( 0.9843059135695010342, 0.000000000000000000, -0.1764705882352923805 ) ) ;
#46772 = AXIS2_PLACEMENT_3D ( 'NONE', #97497, #139633, #109092 ) ;
#46773 = DIRECTION ( 'NONE',  ( -0.000000000000000000, -1.000000000000000000, -0.000000000000000000 ) ) ;
#46774 = CARTESIAN_POINT ( 'NONE',  ( 53.28709685856478018, 3.054999999999997939, 5.291415217122920289 ) ) ;
#46775 = DIRECTION ( 'NONE',  ( 0.3543493200069162685, -0.000000000000000000, -0.9351131265310288487 ) ) ;
#46776 = COLOUR_RGB ( '', 0.09019608, 0.27058824, 0.51372549) ;
#46777 = VECTOR ( 'NONE', #84963, 1000.000000000000000 ) ;
#46778 = CARTESIAN_POINT ( 'NONE',  ( 24.79289321881328334, 6.759292476615651246, 5.000000000000000000 ) ) ;
#46779 = CARTESIAN_POINT ( 'NONE',  ( 3.722814304570581712, -21.72499999999999432, 5.000000000000000000 ) ) ;
#46780 = ADVANCED_FACE ( 'NONE', ( #126391 ), #82916, .F. ) ;
#46781 = ORIENTED_EDGE ( 'NONE', *, *, #35715, .F. ) ;
#46782 = PLANE ( 'NONE',  #2531 ) ;
#46783 = EDGE_LOOP ( 'NONE', ( #103715, #107681, #23322, #5947 ) ) ;
#46784 = AXIS2_PLACEMENT_3D ( 'NONE', #46069, #135903, #91680 ) ;
#46785 = DIRECTION ( 'NONE',  ( -0.3543493200069162685, -0.000000000000000000, -0.9351131265310288487 ) ) ;
#46786 = MECHANICAL_DESIGN_GEOMETRIC_PRESENTATION_REPRESENTATION (  '', ( #60638 ), #106832 ) ;
#46787 = PLANE ( 'NONE',  #22926 ) ;
#46788 = CARTESIAN_POINT ( 'NONE',  ( 17.39159235450332019, -3.851859888774471706E-31, 2.500000000000001332 ) ) ;
#46789 = DIRECTION ( 'NONE',  ( -0.7071067811865486830, -0.7071067811865464625, 0.000000000000000000 ) ) ;
#46790 = EDGE_CURVE ( 'NONE', #58576, #115135, #8841, .T. ) ;
#46791 = CARTESIAN_POINT ( 'NONE',  ( 5.671830600776434750, 2.259292476615697876, 4.000000000000000000 ) ) ;
#46792 = FACE_OUTER_BOUND ( 'NONE', #96666, .T. ) ;
#46793 = EDGE_LOOP ( 'NONE', ( #2357, #81649, #133678, #128351, #119251 ) ) ;
#46794 = EDGE_CURVE ( 'NONE', #118900, #68320, #19064, .T. ) ;
#46795 = VERTEX_POINT ( 'NONE', #129239 ) ;
#46796 = DIRECTION ( 'NONE',  ( 0.7071067811865487940, 0.7071067811865463515, 0.000000000000000000 ) ) ;
#46797 = CARTESIAN_POINT ( 'NONE',  ( 28.00000000000002487, -57.14999999999999147, -62.92499999999978400 ) ) ;
#46798 = VECTOR ( 'NONE', #49492, 1000.000000000000114 ) ;
#46799 = LINE ( 'NONE', #90979, #54323 ) ;
#46800 = DIRECTION ( 'NONE',  ( -0.7071067811865486830, -0.7071067811865464625, 0.000000000000000000 ) ) ;
#46801 = CARTESIAN_POINT ( 'NONE',  ( 70.66252705046288440, 7.949999999999998401, 1.460391307983218338E-15 ) ) ;
#46802 = DIRECTION ( 'NONE',  ( -0.7071067811865487940, 0.7071067811865463515, 0.000000000000000000 ) ) ;
#46803 = FACE_OUTER_BOUND ( 'NONE', #112788, .T. ) ;
#46804 = EDGE_LOOP ( 'NONE', ( #133901, #97920, #120947, #41587, #17019 ) ) ;
#46805 = CARTESIAN_POINT ( 'NONE',  ( 77.12500000000000000, -7.950000000000000178, -4.867971026610729436E-16 ) ) ;
#46806 = DIRECTION ( 'NONE',  ( 0.7071067811865487940, 0.7071067811865463515, 0.000000000000000000 ) ) ;
#46807 = CARTESIAN_POINT ( 'NONE',  ( -34.45011844616454511, -1.483719188362514041, 5.000000000000000888 ) ) ;
#46808 = CARTESIAN_POINT ( 'NONE',  ( 34.42499999999998295, 22.22500000000000142, 5.000000000000000000 ) ) ;
#46809 = VERTEX_POINT ( 'NONE', #51716 ) ;
#46810 = ADVANCED_FACE ( 'NONE', ( #141573 ), #55252, .T. ) ;
#46811 = VECTOR ( 'NONE', #79510, 1000.000000000000000 ) ;
#46812 = CARTESIAN_POINT ( 'NONE',  ( -24.18398860626899705, 28.73617430169804265, 5.000000000000000000 ) ) ;
#46813 = VECTOR ( 'NONE', #1119, 1000.000000000000000 ) ;
#46814 = DIRECTION ( 'NONE',  ( 0.7071067811865487940, 0.7071067811865463515, 0.000000000000000000 ) ) ;
#46815 = CARTESIAN_POINT ( 'NONE',  ( 68.10459685856474721, 1.637169565754164946, -6.109999999999999432 ) ) ;
#46816 = AXIS2_PLACEMENT_3D ( 'NONE', #18094, #41305, #106542 ) ;
#46817 = LINE ( 'NONE', #80134, #4248 ) ;
#46818 = VERTEX_POINT ( 'NONE', #32088 ) ;
#46819 = ORIENTED_EDGE ( 'NONE', *, *, #53335, .F. ) ;
#46820 = DIRECTION ( 'NONE',  ( -0.000000000000000000, 0.3543493200069153248, 0.9351131265310292928 ) ) ;
#46821 = CARTESIAN_POINT ( 'NONE',  ( 2.999999999999999112, 1.399999999999986366, 20.40202195861970580 ) ) ;
#46822 = DIRECTION ( 'NONE',  ( -0.7071067811865486830, -0.7071067811865464625, -0.000000000000000000 ) ) ;
#46823 = DIRECTION ( 'NONE',  ( -0.7071067811865486830, -0.7071067811865464625, -0.000000000000000000 ) ) ;
#46825 = VERTEX_POINT ( 'NONE', #95908 ) ;
#46824 = PLANE ( 'NONE',  #128586 ) ;
#46826 = CYLINDRICAL_SURFACE ( 'NONE', #2122, 2.500000000000000444 ) ;
#46827 = CARTESIAN_POINT ( 'NONE',  ( 36.18398860626899705, 28.73617430169812437, 5.000000000000000000 ) ) ;
#46828 = DIRECTION ( 'NONE',  ( -0.7071067811865487940, 0.7071067811865463515, -0.000000000000000000 ) ) ;
#46829 = CIRCLE ( 'NONE', #21316, 2.500000000000000888 ) ;
#46830 = VERTEX_POINT ( 'NONE', #53865 ) ;
#46831 = ORIENTED_EDGE ( 'NONE', *, *, #123998, .T. ) ;
#46832 = CARTESIAN_POINT ( 'NONE',  ( 52.35459685856476852, -1.637169565754161615, 6.110000000000000320 ) ) ;
#46833 = ADVANCED_FACE ( 'NONE', ( #142295 ), #76315, .F. ) ;
#46834 = ORIENTED_EDGE ( 'NONE', *, *, #129554, .F. ) ;
#46835 = FACE_OUTER_BOUND ( 'NONE', #136191, .T. ) ;
#46836 = EDGE_CURVE ( 'NONE', #16024, #37562, #129976, .T. ) ;
#46837 = DIRECTION ( 'NONE',  ( 0.6830127018922180770, -0.6830127018922204085, -0.2588190451025213501 ) ) ;
#46838 = FACE_OUTER_BOUND ( 'NONE', #125860, .T. ) ;
#46839 = AXIS2_PLACEMENT_3D ( 'NONE', #118625, #129494, #38936 ) ;
#46840 = DIRECTION ( 'NONE',  ( -0.000000000000000000, 0.000000000000000000, 1.000000000000000000 ) ) ;
#46841 = CARTESIAN_POINT ( 'NONE',  ( 55.10416666666665719, 2.130196079827498146, 7.949999999999958433 ) ) ;
#46842 = EDGE_LOOP ( 'NONE', ( #35606, #33552, #124355, #43609 ) ) ;
#46843 = ORIENTED_EDGE ( 'NONE', *, *, #132405, .T. ) ;
#46844 = AXIS2_PLACEMENT_3D ( 'NONE', #61562, #82569, #39060 ) ;
#46845 = LINE ( 'NONE', #112056, #63058 ) ;
#46846 = CARTESIAN_POINT ( 'NONE',  ( -19.61417773406576259, -0.8225097182635713322, -31.54462512304873911 ) ) ;
#46847 = EDGE_CURVE ( 'NONE', #86268, #76404, #140824, .T. ) ;
#46848 = EDGE_CURVE ( 'NONE', #94406, #119070, #30679, .T. ) ;
#46849 = ORIENTED_EDGE ( 'NONE', *, *, #80188, .T. ) ;
#46850 = FACE_OUTER_BOUND ( 'NONE', #74833, .T. ) ;
#46851 = CARTESIAN_POINT ( 'NONE',  ( 112.8083603837962272, 7.949999999999996625, 2.130196079827431088 ) ) ;
#46852 = CARTESIAN_POINT ( 'NONE',  ( -4.499999999999966249, -11.56887692260769462, 4.000000000000000000 ) ) ;
#46853 = VECTOR ( 'NONE', #88615, 1000.000000000000000 ) ;
#46854 = ORIENTED_EDGE ( 'NONE', *, *, #18454, .T. ) ;
#46855 = EDGE_CURVE ( 'NONE', #68379, #65716, #98062, .T. ) ;
#46856 = FACE_BOUND ( 'NONE', #49445, .T. ) ;
#46857 = EDGE_CURVE ( 'NONE', #123709, #77093, #119774, .T. ) ;
#46858 = DIRECTION ( 'NONE',  ( 0.7071067811865487940, 0.7071067811865463515, -0.000000000000000000 ) ) ;
#46859 = CARTESIAN_POINT ( 'NONE',  ( -15.18398860626900237, 28.73617430169797871, 5.000000000000000000 ) ) ;
#46860 = DIRECTION ( 'NONE',  ( 0.6830127018922180770, -0.6830127018922204085, -0.2588190451025213501 ) ) ;
#46861 = AXIS2_PLACEMENT_3D ( 'NONE', #135384, #36745, #101292 ) ;
#46862 = DIRECTION ( 'NONE',  ( -1.000000000000000000, -1.224606353822377258E-16, -0.000000000000000000 ) ) ;
#46863 =( BOUNDED_CURVE ( )  B_SPLINE_CURVE ( 3, ( #45877, #12494, #132893, #100238 ),
 .UNSPECIFIED., .F., .T. ) 
 B_SPLINE_CURVE_WITH_KNOTS ( ( 4, 4 ),
 ( 5.106027341939290309, 6.645403452391244414 ),
 .UNSPECIFIED. ) 
 CURVE ( )  GEOMETRIC_REPRESENTATION_ITEM ( )  RATIONAL_B_SPLINE_CURVE ( ( 1.000000000000000000, 0.8120851936182302833, 0.8120851936182302833, 1.000000000000000000 ) ) 
 REPRESENTATION_ITEM ( '' )  );
#46864 = DIRECTION ( 'NONE',  ( -1.734723475976806848E-16, 1.000000000000000000, 0.000000000000000000 ) ) ;
#46865 = CARTESIAN_POINT ( 'NONE',  ( 147.9560000000000173, 7.919999999999945750, 19.12499999999998934 ) ) ;
#46866 = EDGE_LOOP ( 'NONE', ( #50322, #107062, #113334, #52438 ) ) ;
#46867 = VERTEX_POINT ( 'NONE', #121220 ) ;
#46868 = CARTESIAN_POINT ( 'NONE',  ( 99.51626352523145158, -4.472830434245838482, 4.472830434245838482 ) ) ;
#46869 = VERTEX_POINT ( 'NONE', #87891 ) ;
#46870 = EDGE_CURVE ( 'NONE', #66621, #50596, #85739, .T. ) ;
#46871 = LINE ( 'NONE', #12735, #62814 ) ;
#46872 = ORIENTED_EDGE ( 'NONE', *, *, #90169, .T. ) ;
#46873 = FACE_OUTER_BOUND ( 'NONE', #122608, .T. ) ;
#46875 = ADVANCED_FACE ( 'NONE', ( #54573 ), #119081, .T. ) ;
#46874 = AXIS2_PLACEMENT_3D ( 'NONE', #33717, #57611, #122111 ) ;
#46876 = VECTOR ( 'NONE', #91286, 1000.000000000000114 ) ;
#46877 = VECTOR ( 'NONE', #85634, 1000.000000000000000 ) ;
#46878 = LINE ( 'NONE', #3289, #64027 ) ;
#46879 = CIRCLE ( 'NONE', #132547, 3.000000000000002665 ) ;
#46880 = DIRECTION ( 'NONE',  ( -0.000000000000000000, -0.3543493200069152693, 0.9351131265310292928 ) ) ;
#46881 = EDGE_LOOP ( 'NONE', ( #51799, #25487, #109725, #124967 ) ) ;
#46882 = CARTESIAN_POINT ( 'NONE',  ( 6.160000000000001030, 9.521314400968980422E-16, 0.000000000000000000 ) ) ;
#46883 = CARTESIAN_POINT ( 'NONE',  ( 8.031592354503320763, 9.902892378096218942E-16, 0.000000000000000000 ) ) ;
#46884 = LINE ( 'NONE', #125089, #119846 ) ;
#46886 = DIRECTION ( 'NONE',  ( 0.7071067811865487940, -0.7071067811865463515, 0.000000000000000000 ) ) ;
#46885 = CARTESIAN_POINT ( 'NONE',  ( -32.95341186370436048, 14.25929247661557042, 18.84478104361335227 ) ) ;
#46887 = CARTESIAN_POINT ( 'NONE',  ( 27.49586038379622721, -3.974999999999998312, -6.884901960086286188 ) ) ;
#46888 = VECTOR ( 'NONE', #69071, 1000.000000000000000 ) ;
#46889 = EDGE_CURVE ( 'NONE', #25969, #63809, #106772, .T. ) ;
#46890 = AXIS2_PLACEMENT_3D ( 'NONE', #41552, #19096, #95941 ) ;
#46891 = AXIS2_PLACEMENT_3D ( 'NONE', #43070, #143071, #97394 ) ;
#46892 = LINE ( 'NONE', #12748, #65307 ) ;
#46893 = VERTEX_POINT ( 'NONE', #64008 ) ;
#46894 = CARTESIAN_POINT ( 'NONE',  ( 87.77083333333331439, -7.949999999999998401, -2.130196079827426203 ) ) ;
#46895 = CARTESIAN_POINT ( 'NONE',  ( -20.99999999999984368, -19.44781430457063465, 5.000000000000000000 ) ) ;
#46896 = ORIENTED_EDGE ( 'NONE', *, *, #124158, .F. ) ;
#46897 = VERTEX_POINT ( 'NONE', #75602 ) ;
#46898 = VERTEX_POINT ( 'NONE', #97303 ) ;
#46899 = EDGE_CURVE ( 'NONE', #54290, #49146, #73764, .T. ) ;
#46900 = CARTESIAN_POINT ( 'NONE',  ( 55.56293019189809712, 1.637169565754157174, 6.110000000000002984 ) ) ;
#46901 = EDGE_CURVE ( 'NONE', #142234, #106369, #7451, .T. ) ;
#46902 = ORIENTED_EDGE ( 'NONE', *, *, #76032, .T. ) ;
#46903 = EDGE_CURVE ( 'NONE', #89022, #68720, #140151, .T. ) ;
#46904 = CARTESIAN_POINT ( 'NONE',  ( 4.129139616203772789, 5.278424836066147208, 3.047499999999990550 ) ) ;
#46905 = CARTESIAN_POINT ( 'NONE',  ( 94.93793019189810423, -6.110000000000001208, 1.637169565754158951 ) ) ;
#46906 = LINE ( 'NONE', #78769, #44894 ) ;
#46907 = ORIENTED_EDGE ( 'NONE', *, *, #63569, .T. ) ;
#46908 = MANIFOLD_SOLID_BREP ( 'Boss-Extrude1', #106478 ) ;
#46909 = PLANE ( 'NONE',  #82700 ) ;
#46910 = ORIENTED_EDGE ( 'NONE', *, *, #90825, .T. ) ;
#46911 = DIRECTION ( 'NONE',  ( 0.6830127018922180770, -0.6830127018922204085, -0.2588190451025213501 ) ) ;
#46912 = VERTEX_POINT ( 'NONE', #24770 ) ;
#46913 = CARTESIAN_POINT ( 'NONE',  ( -12.18398860626900060, 28.73617430169795739, 5.000000000000000000 ) ) ;
#46914 = AXIS2_PLACEMENT_3D ( 'NONE', #20600, #54694, #76449 ) ;
#46915 = DIRECTION ( 'NONE',  ( -0.7071067811865487940, 0.7071067811865463515, 0.000000000000000000 ) ) ;
#46916 = CARTESIAN_POINT ( 'NONE',  ( 125.7662635252314658, 4.472830434245839371, -4.472830434245839371 ) ) ;
#46917 = VERTEX_POINT ( 'NONE', #133550 ) ;
#46918 = FACE_OUTER_BOUND ( 'NONE', #45998, .T. ) ;
#46919 = ORIENTED_EDGE ( 'NONE', *, *, #69792, .T. ) ;
#46920 = VECTOR ( 'NONE', #84660, 1000.000000000000000 ) ;
#46921 = ORIENTED_EDGE ( 'NONE', *, *, #2039, .F. ) ;
#46922 = ORIENTED_EDGE ( 'NONE', *, *, #71691, .F. ) ;
#46923 = DIRECTION ( 'NONE',  ( 0.000000000000000000, -1.000000000000000000, 0.000000000000000000 ) ) ;
#46924 = DIRECTION ( 'NONE',  ( -0.000000000000000000, 0.000000000000000000, 1.000000000000000000 ) ) ;
#46925 = DIRECTION ( 'NONE',  ( -0.000000000000000000, 0.3543493200069153248, 0.9351131265310292928 ) ) ;
#46926 = PLANE ( 'NONE',  #18724 ) ;
#46927 = ORIENTED_EDGE ( 'NONE', *, *, #117739, .T. ) ;
#46928 = CARTESIAN_POINT ( 'NONE',  ( 25.35373647476855297, -5.808823158059035485, -5.808823158059033709 ) ) ;
#46929 = DIRECTION ( 'NONE',  ( -0.3543493200069162685, -0.000000000000000000, -0.9351131265310288487 ) ) ;
#46930 = LINE ( 'NONE', #35315, #78407 ) ;
#46931 = DIRECTION ( 'NONE',  ( 0.6830127018922180770, -0.6830127018922204085, -0.2588190451025213501 ) ) ;
#46932 = EDGE_LOOP ( 'NONE', ( #47696, #21192, #38656 ) ) ;
#46933 = VERTEX_POINT ( 'NONE', #118363 ) ;
#46934 = EDGE_CURVE ( 'NONE', #62052, #137014, #69018, .T. ) ;
#46935 = VECTOR ( 'NONE', #41794, 1000.000000000000227 ) ;
#46936 = ORIENTED_EDGE ( 'NONE', *, *, #123013, .T. ) ;
#46937 = FACE_OUTER_BOUND ( 'NONE', #62010, .T. ) ;
#46938 = AXIS2_PLACEMENT_3D ( 'NONE', #22976, #78848, #12832 ) ;
#46939 = FACE_OUTER_BOUND ( 'NONE', #83269, .T. ) ;
#46940 = DIRECTION ( 'NONE',  ( -0.6830127018922180770, -0.6830127018922204085, -0.2588190451025213501 ) ) ;
#46941 = CARTESIAN_POINT ( 'NONE',  ( 9.176104866590083731, 8.505782047251113198, -4.231528338128802247 ) ) ;
#46942 = CARTESIAN_POINT ( 'NONE',  ( -60.18398860626900415, 28.73617430169829490, 5.000000000000000000 ) ) ;
#46943 = DIRECTION ( 'NONE',  ( 0.7071067811865486830, -0.7071067811865464625, -0.000000000000000000 ) ) ;
#46944 = CARTESIAN_POINT ( 'NONE',  ( 34.92500000000001137, 22.27000000000000668, -7.752744394707098863 ) ) ;
#46945 = CARTESIAN_POINT ( 'NONE',  ( 128.6958184333952602, -52.10373894832327579, 40.45955814675564000 ) ) ;
#46946 = CARTESIAN_POINT ( 'NONE',  ( -7.499999999999947597, 15.43112307739203182, 4.000000000000000000 ) ) ;
#46947 = VERTEX_POINT ( 'NONE', #44423 ) ;
#46948 = AXIS2_PLACEMENT_3D ( 'NONE', #44500, #66935, #45216 ) ;
#46949 = FACE_OUTER_BOUND ( 'NONE', #62168, .T. ) ;
#46950 = VERTEX_POINT ( 'NONE', #91473 ) ;
#46951 = DIRECTION ( 'NONE',  ( -1.000000000000000000, -1.224606353822377258E-16, -0.000000000000000000 ) ) ;
#46953 = ORIENTED_EDGE ( 'NONE', *, *, #116184, .T. ) ;
#46952 = LINE ( 'NONE', #48326, #71910 ) ;
#46954 = EDGE_CURVE ( 'NONE', #60103, #139953, #80604, .T. ) ;
#46955 =( LENGTH_UNIT ( ) NAMED_UNIT ( * ) SI_UNIT ( .MILLI., .METRE. ) );
#46956 = CARTESIAN_POINT ( 'NONE',  ( -23.99999999999983658, -13.44781430457069149, 5.000000000000000000 ) ) ;
#46957 = ORIENTED_EDGE ( 'NONE', *, *, #32683, .F. ) ;
#46958 = EDGE_CURVE ( 'NONE', #51427, #7365, #90019, .T. ) ;
#46959 = CARTESIAN_POINT ( 'NONE',  ( -0.4892135623730947680, -27.52281430457055578, 5.000000000000000000 ) ) ;
#46961 = ORIENTED_EDGE ( 'NONE', *, *, #18551, .F. ) ;
#46960 = VECTOR ( 'NONE', #69612, 1000.000000000000000 ) ;
#46962 = CARTESIAN_POINT ( 'NONE',  ( 21.29974487139158512, -27.71228299555221142, 4.000000000000000000 ) ) ;
#46963 = ORIENTED_EDGE ( 'NONE', *, *, #130439, .T. ) ;
#46964 = EDGE_CURVE ( 'NONE', #43938, #46917, #13158, .T. ) ;
#46965 = CARTESIAN_POINT ( 'NONE',  ( 6.717577386425625185, -21.73023691814492508, 5.000000000000001776 ) ) ;
#46966 = CARTESIAN_POINT ( 'NONE',  ( 100.8500270504628986, -5.819803920172572198, -5.819803920172572198 ) ) ;
#46967 = FACE_OUTER_BOUND ( 'NONE', #97403, .T. ) ;
#46968 = DIRECTION ( 'NONE',  ( 0.7071067811865487940, 0.7071067811865463515, 0.000000000000000000 ) ) ;
#46969 = ORIENTED_EDGE ( 'NONE', *, *, #6187, .F. ) ;
#46970 = ADVANCED_FACE ( 'NONE', ( #13868 ), #121921, .F. ) ;
#46971 = CARTESIAN_POINT ( 'NONE',  ( 75.18398860626899705, 28.73617430169839793, 5.000000000000000000 ) ) ;
#46972 = DIRECTION ( 'NONE',  ( -1.000000000000000000, -0.000000000000000000, -0.000000000000000000 ) ) ;
#46973 = CARTESIAN_POINT ( 'NONE',  ( -57.18398860626899705, 28.73617430169827358, 5.000000000000000000 ) ) ;
#46974 = CARTESIAN_POINT ( 'NONE',  ( 16.33333333333333570, 5.278424836066143655, -3.047499999999997655 ) ) ;
#46975 = CARTESIAN_POINT ( 'NONE',  ( 24.47873647476855652, -5.808823158059033709, 5.808823158059035485 ) ) ;
#46976 = AXIS2_PLACEMENT_3D ( 'NONE', #126228, #25463, #34956 ) ;
#46978 = CARTESIAN_POINT ( 'NONE',  ( 25.39999999999999858, -1.599999999999997202, -17.44999999999996732 ) ) ;
#46977 = VECTOR ( 'NONE', #133979, 1000.000000000000000 ) ;
#46979 = LINE ( 'NONE', #112884, #138145 ) ;
#46980 = VERTEX_POINT ( 'NONE', #34233 ) ;
#46981 = VECTOR ( 'NONE', #37799, 1000.000000000000000 ) ;
#46982 = EDGE_CURVE ( 'NONE', #14592, #78770, #112500, .T. ) ;
#46983 = VECTOR ( 'NONE', #141695, 1000.000000000000000 ) ;
#46984 = CARTESIAN_POINT ( 'NONE',  ( -19.05000000000000071, 3.174999999999997158, 5.000000000000000000 ) ) ;
#46985 = VERTEX_POINT ( 'NONE', #36376 ) ;
#46986 = CARTESIAN_POINT ( 'NONE',  ( 90.41709685856477563, 3.054999999999998828, 5.291415217122922066 ) ) ;
#46987 = CARTESIAN_POINT ( 'NONE',  ( -34.42500000000001137, -21.72500000000000142, 5.000000000000000000 ) ) ;
#46988 = DIRECTION ( 'NONE',  ( 0.3543493200069163240, -0.000000000000000000, -0.9351131265310288487 ) ) ;
#46989 = VECTOR ( 'NONE', #52446, 1000.000000000000000 ) ;
#46991 = CARTESIAN_POINT ( 'NONE',  ( 11.99999999999991651, 1.552185695429147527, 5.000000000000000000 ) ) ;
#46990 = VECTOR ( 'NONE', #112892, 1000.000000000000227 ) ;
#46992 = CARTESIAN_POINT ( 'NONE',  ( 122.6835989386368055, -43.15000000000001990, -34.92499999999998295 ) ) ;
#46993 = ORIENTED_EDGE ( 'NONE', *, *, #28515, .T. ) ;
#46994 = EDGE_CURVE ( 'NONE', #9906, #48450, #11728, .T. ) ;
#46995 = DIRECTION ( 'NONE',  ( -0.6830127018922181881, 0.6830127018922202975, -0.2588190451025214056 ) ) ;
#46996 = DIRECTION ( 'NONE',  ( 0.7071067811865487940, 0.7071067811865463515, 0.000000000000000000 ) ) ;
#46997 = ORIENTED_EDGE ( 'NONE', *, *, #76555, .F. ) ;
#46998 = LINE ( 'NONE', #112208, #124989 ) ;
#46999 = CARTESIAN_POINT ( 'NONE',  ( -45.29974487139158867, -27.71228299555237840, 4.000000000000000000 ) ) ;
#47001 = ORIENTED_EDGE ( 'NONE', *, *, #42956, .T. ) ;
#47000 = DIRECTION ( 'NONE',  ( 1.000000000000000000, 0.000000000000000000, 0.000000000000000000 ) ) ;
#47002 = DIRECTION ( 'NONE',  ( 0.000000000000000000, 0.000000000000000000, 1.000000000000000000 ) ) ;
#47003 = EDGE_CURVE ( 'NONE', #68079, #28957, #45843, .T. ) ;
#47004 = CARTESIAN_POINT ( 'NONE',  ( 102.4541937171295700, 6.884901960086283523, 3.975000000000002753 ) ) ;
#47005 = PLANE ( 'NONE',  #118706 ) ;
#47006 = DIRECTION ( 'NONE',  ( 0.7071067811865487940, 0.7071067811865463515, 0.000000000000000000 ) ) ;
#47007 = PLANE ( 'NONE',  #84046 ) ;
#47008 = ORIENTED_EDGE ( 'NONE', *, *, #132094, .T. ) ;
#47009 = VERTEX_POINT ( 'NONE', #56012 ) ;
#47010 = VERTEX_POINT ( 'NONE', #854 ) ;
#47011 = CARTESIAN_POINT ( 'NONE',  ( 78.89626352523143282, 4.472830434245840259, -4.472830434245839371 ) ) ;
#47012 = ORIENTED_EDGE ( 'NONE', *, *, #34832, .F. ) ;
#47013 = DIRECTION ( 'NONE',  ( 0.6830127018922180770, -0.6830127018922204085, -0.2588190451025213501 ) ) ;
#47014 = EDGE_CURVE ( 'NONE', #78177, #4434, #55277, .T. ) ;
#47015 = DIRECTION ( 'NONE',  ( -1.000000000000000000, -0.000000000000000000, -0.000000000000000000 ) ) ;
#47016 = DIRECTION ( 'NONE',  ( -1.000000000000000000, -1.224606353822377258E-16, -0.000000000000000000 ) ) ;
#47017 = CARTESIAN_POINT ( 'NONE',  ( 5.999999999999956479, 9.631307414974335401, -9.079085613539529476 ) ) ;
#47018 = ORIENTED_EDGE ( 'NONE', *, *, #82658, .T. ) ;
#47019 = CARTESIAN_POINT ( 'NONE',  ( 22.94836012241460566, 22.22500000000000142, 26.93037957019046758 ) ) ;
#47020 = CARTESIAN_POINT ( 'NONE',  ( 18.18398860626898994, 28.73617430169800002, 5.000000000000000000 ) ) ;
#47021 = VECTOR ( 'NONE', #97829, 1000.000000000000000 ) ;
#47022 = EDGE_CURVE ( 'NONE', #51777, #60758, #89321, .T. ) ;
#47023 = EDGE_CURVE ( 'NONE', #62799, #99425, #1554, .T. ) ;
#47024 = CARTESIAN_POINT ( 'NONE',  ( 17.99999999999987566, -13.97847968911258754, -0.1324546996126375054 ) ) ;
#47025 = CARTESIAN_POINT ( 'NONE',  ( 78.37043019189812298, -3.055000000000001492, 5.291415217122917625 ) ) ;
#47026 = ORIENTED_EDGE ( 'NONE', *, *, #8217, .F. ) ;
#47027 = VECTOR ( 'NONE', #73455, 1000.000000000000000 ) ;
#47028 = CARTESIAN_POINT ( 'NONE',  ( -20.27718569542926730, -21.72500000000000853, 5.000000000000000000 ) ) ;
#47030 = AXIS2_PLACEMENT_3D ( 'NONE', #39473, #27856, #104703 ) ;
#47029 = DIRECTION ( 'NONE',  ( 0.7071067811865486830, -0.7071067811865464625, -0.000000000000000000 ) ) ;
#47031 =( GEOMETRIC_REPRESENTATION_CONTEXT ( 3 ) GLOBAL_UNCERTAINTY_ASSIGNED_CONTEXT ( ( #46224 ) ) GLOBAL_UNIT_ASSIGNED_CONTEXT ( ( #48368, #103441, #91195 ) ) REPRESENTATION_CONTEXT ( 'NONE', 'WORKASPACE' ) );
#47032 = EDGE_CURVE ( 'NONE', #51730, #116759, #79202, .T. ) ;
#47033 = VERTEX_POINT ( 'NONE', #2268 ) ;
#47034 = EDGE_LOOP ( 'NONE', ( #44098, #57386, #111419, #56288 ) ) ;
#47035 = CARTESIAN_POINT ( 'NONE',  ( -15.18398860626900237, 28.73617430169797871, 5.000000000000000000 ) ) ;
#47036 = EDGE_CURVE ( 'NONE', #903, #16634, #90773, .T. ) ;
#47037 = ADVANCED_FACE ( 'NONE', ( #61713 ), #114621, .T. ) ;
#47038 = CARTESIAN_POINT ( 'NONE',  ( 15.05159235450332034, 9.902892378096218942E-16, 0.000000000000000000 ) ) ;
#47039 = CARTESIAN_POINT ( 'NONE',  ( 25.29623647476855908, 7.934999999999990727, -1.457635852685135314E-15 ) ) ;
#47040 = DIRECTION ( 'NONE',  ( -0.000000000000000000, 0.000000000000000000, 1.000000000000000000 ) ) ;
#47041 = DIRECTION ( 'NONE',  ( -0.6830127018922180770, -0.6830127018922204085, -0.2588190451025213501 ) ) ;
#47042 = CARTESIAN_POINT ( 'NONE',  ( -11.20710678118646086, -17.24070752338409918, 5.000000000000000000 ) ) ;
#47043 = VECTOR ( 'NONE', #86311, 1000.000000000000000 ) ;
#47044 = CARTESIAN_POINT ( 'NONE',  ( -25.39999999999996305, 0.000000000000000000, 0.000000000000000000 ) ) ;
#47045 = SHAPE_REPRESENTATION_RELATIONSHIP ( 'NONE' , 'NONE' ,  #64389, #15274 ) ;
#47046 = ORIENTED_EDGE ( 'NONE', *, *, #29957, .T. ) ;
#47047 = ORIENTED_EDGE ( 'NONE', *, *, #101716, .F. ) ;
#47048 = EDGE_CURVE ( 'NONE', #51626, #97582, #103732, .T. ) ;
#47049 = CARTESIAN_POINT ( 'NONE',  ( 9.041666666666666075, 3.047499999999993214, -5.278424836066146320 ) ) ;
#47050 = ORIENTED_EDGE ( 'NONE', *, *, #47036, .T. ) ;
#47051 = EDGE_LOOP ( 'NONE', ( #137249, #125521, #121416, #42710 ) ) ;
#47052 = VECTOR ( 'NONE', #24344, 1000.000000000000000 ) ;
#47053 = AXIS2_PLACEMENT_3D ( 'NONE', #69229, #14097, #37301 ) ;
#47054 = EDGE_CURVE ( 'NONE', #70774, #114684, #103940, .T. ) ;
#47055 = DIRECTION ( 'NONE',  ( 0.000000000000000000, -1.000000000000000000, 0.000000000000000000 ) ) ;
#47056 = ORIENTED_EDGE ( 'NONE', *, *, #34695, .T. ) ;
#47057 = DIRECTION ( 'NONE',  ( 0.7071067811865487940, 0.7071067811865463515, -0.000000000000000000 ) ) ;
#47058 = CARTESIAN_POINT ( 'NONE',  ( -26.67183060077628554, -0.7407075233842701500, 4.000000000000000000 ) ) ;
#47059 = CARTESIAN_POINT ( 'NONE',  ( 4.499999999999968914, 13.46639925780212366, 5.000000000000000000 ) ) ;
#47060 = CARTESIAN_POINT ( 'NONE',  ( -0.6431874275173860012, -20.24070752338407786, 21.22881796311212810 ) ) ;
#47061 = VECTOR ( 'NONE', #63588, 1000.000000000000000 ) ;
#47062 = DIRECTION ( 'NONE',  ( -0.000000000000000000, -0.3543493200069152693, 0.9351131265310292928 ) ) ;
#47063 = ORIENTED_EDGE ( 'NONE', *, *, #84917, .T. ) ;
#47064 = DIRECTION ( 'NONE',  ( -1.000000000000000000, -0.000000000000000000, 0.000000000000000000 ) ) ;
#47065 = ORIENTED_EDGE ( 'NONE', *, *, #46903, .F. ) ;
#47066 = CARTESIAN_POINT ( 'NONE',  ( 166.8575281714868481, 26.96999999999994202, -34.92499999999998295 ) ) ;
#47067 = ORIENTED_EDGE ( 'NONE', *, *, #97328, .T. ) ;
#47068 = DIRECTION ( 'NONE',  ( -0.7071067811865487940, 0.7071067811865463515, -0.000000000000000000 ) ) ;
#47069 = ORIENTED_EDGE ( 'NONE', *, *, #46848, .F. ) ;
#47070 = LINE ( 'NONE', #15740, #87521 ) ;
#47071 = ORIENTED_EDGE ( 'NONE', *, *, #87905, .F. ) ;
#47072 = ORIENTED_EDGE ( 'NONE', *, *, #87704, .T. ) ;
#47073 = VECTOR ( 'NONE', #25174, 1000.000000000000227 ) ;
#47074 = ORIENTED_EDGE ( 'NONE', *, *, #8789, .T. ) ;
#47075 = ADVANCED_FACE ( 'NONE', ( #104464 ), #25219, .F. ) ;
#47076 = CARTESIAN_POINT ( 'NONE',  ( 95.20833333333334281, -3.974999999999999201, -6.884901960086287964 ) ) ;
#47077 = ADVANCED_FACE ( 'NONE', ( #103053 ), #59573, .F. ) ;
#47078 = DIRECTION ( 'NONE',  ( 0.000000000000000000, -1.000000000000000000, 0.000000000000000000 ) ) ;
#47079 = CARTESIAN_POINT ( 'NONE',  ( 18.17159235450331778, 9.902892378096218942E-16, 0.000000000000000000 ) ) ;
#47080 = CARTESIAN_POINT ( 'NONE',  ( 118.4170968585647756, 3.054999999999998828, 5.291415217122922066 ) ) ;
#47081 = DIRECTION ( 'NONE',  ( -0.000000000000000000, -0.3543493200069152693, 0.9351131265310292928 ) ) ;
#47082 = EDGE_CURVE ( 'NONE', #63122, #9882, #92881, .T. ) ;
#47083 = DIRECTION ( 'NONE',  ( -0.7071067811865487940, 0.7071067811865463515, 0.000000000000000000 ) ) ;
#47084 = DIRECTION ( 'NONE',  ( 1.000000000000000000, 1.224606353822377258E-16, 0.000000000000000000 ) ) ;
#47085 = CIRCLE ( 'NONE', #14625, 2.500000000000000444 ) ;
#47086 = DIRECTION ( 'NONE',  ( -0.6830127018922180770, -0.6830127018922204085, -0.2588190451025213501 ) ) ;
#47087 = VECTOR ( 'NONE', #114573, 1000.000000000000000 ) ;
#47088 = DIRECTION ( 'NONE',  ( -0.7071067811865486830, -0.7071067811865464625, 0.000000000000000000 ) ) ;
#47089 = EDGE_LOOP ( 'NONE', ( #35034, #46514, #110461, #30525 ) ) ;
#47090 = DIRECTION ( 'NONE',  ( 0.7071067811865486830, -0.7071067811865464625, -0.000000000000000000 ) ) ;
#47091 = ORIENTED_EDGE ( 'NONE', *, *, #45770, .F. ) ;
#47092 = VERTEX_POINT ( 'NONE', #4376 ) ;
#47093 = AXIS2_PLACEMENT_3D ( 'NONE', #65360, #109542, #53760 ) ;
#47094 = LINE ( 'NONE', #81839, #74948 ) ;
#47095 = ORIENTED_EDGE ( 'NONE', *, *, #89679, .T. ) ;
#47096 = CARTESIAN_POINT ( 'NONE',  ( 0.000000000000000000, 0.000000000000000000, 5.000000000000000000 ) ) ;
#47097 = CARTESIAN_POINT ( 'NONE',  ( 11.99999999999992362, 17.96639925780207747, 5.000000000000000000 ) ) ;
#47098 = LINE ( 'NONE', #135490, #85720 ) ;
#47099 = CARTESIAN_POINT ( 'NONE',  ( -42.18398860626899705, 28.73617430169816700, 5.000000000000000000 ) ) ;
#47100 = ORIENTED_EDGE ( 'NONE', *, *, #81387, .F. ) ;
#47101 = DIRECTION ( 'NONE',  ( 0.7071067811865486830, -0.7071067811865464625, -0.000000000000000000 ) ) ;
#47102 = ORIENTED_EDGE ( 'NONE', *, *, #57683, .F. ) ;
#47103 = CARTESIAN_POINT ( 'NONE',  ( 66.29974487139159578, -27.71228299555252406, 4.000000000000000000 ) ) ;
#47104 = VECTOR ( 'NONE', #32097, 1000.000000000000000 ) ;
#47105 = CARTESIAN_POINT ( 'NONE',  ( 26.75456980810189123, -6.871911579029512218, 3.967499999999996252 ) ) ;
#47106 = ORIENTED_EDGE ( 'NONE', *, *, #30946, .T. ) ;
#47107 = DIRECTION ( 'NONE',  ( 0.000000000000000000, 0.000000000000000000, -1.000000000000000000 ) ) ;
#47108 = DIRECTION ( 'NONE',  ( -0.6830127018922181881, 0.6830127018922202975, -0.2588190451025214056 ) ) ;
#47109 = VERTEX_POINT ( 'NONE', #15287 ) ;
#47110 = ORIENTED_EDGE ( 'NONE', *, *, #57932, .F. ) ;
#47111 = EDGE_LOOP ( 'NONE', ( #123933, #78360, #67071, #33783 ) ) ;
#47112 = DIRECTION ( 'NONE',  ( -0.000000000000000000, 0.000000000000000000, 1.000000000000000000 ) ) ;
#47113 = FACE_OUTER_BOUND ( 'NONE', #22283, .T. ) ;
#47114 = LINE ( 'NONE', #92674, #137638 ) ;
#47115 = DIRECTION ( 'NONE',  ( -0.000000000000000000, 0.3543493200069153248, 0.9351131265310292928 ) ) ;
#47116 = ORIENTED_EDGE ( 'NONE', *, *, #48538, .T. ) ;
#47117 = AXIS2_PLACEMENT_3D ( 'NONE', #106187, #104047, #127247 ) ;
#47118 = PLANE ( 'NONE',  #87932 ) ;
#47119 = PRESENTATION_STYLE_ASSIGNMENT (( #2076 ) ) ;
#47120 = VECTOR ( 'NONE', #19915, 1000.000000000000227 ) ;
#47121 = CARTESIAN_POINT ( 'NONE',  ( -21.29974487139158512, -27.71228299555221142, 4.000000000000000000 ) ) ;
#47122 = PLANE ( 'NONE',  #58441 ) ;
#47123 = EDGE_LOOP ( 'NONE', ( #96243, #3156, #2590, #79657 ) ) ;
#47124 = CARTESIAN_POINT ( 'NONE',  ( 21.18398860626899349, 28.73617430169802134, 5.000000000000000000 ) ) ;
#47125 = VERTEX_POINT ( 'NONE', #48677 ) ;
#47126 =( BOUNDED_CURVE ( )  B_SPLINE_CURVE ( 2, ( #15907, #49335, #82651, #40582, #29666, #5764, #94219, #105786, #28980, #60194, #71786, #126839, #73908 ),
 .UNSPECIFIED., .F., .T. ) 
 B_SPLINE_CURVE_WITH_KNOTS ( ( 3, 2, 2, 2, 2, 2, 3 ),
 ( 0.1500000000000000222, 0.1583333333333333537, 0.1666666666666666852, 0.1750000000000000444, 0.1833333333333333759, 0.1916666666666667351, 0.2000000000000000666 ),
 .UNSPECIFIED. ) 
 CURVE ( )  GEOMETRIC_REPRESENTATION_ITEM ( )  RATIONAL_B_SPLINE_CURVE ( ( 0.9999999999999998890, 0.9659258262890684232, 1.000000000000000000, 0.9659258262890683122, 1.000000000000000000, 0.9659258262890683122, 1.000000000000000000, 0.9659258262890683122, 1.000000000000000000, 0.9659258262890683122, 1.000000000000000000, 0.9659258262890680902, 1.000000000000000222 ) ) 
 REPRESENTATION_ITEM ( '' )  );
#47127 = AXIS2_PLACEMENT_3D ( 'NONE', #10474, #120660, #21379 ) ;
#47128 = EDGE_CURVE ( 'NONE', #77035, #90453, #137112, .T. ) ;
#47130 = EDGE_LOOP ( 'NONE', ( #8076, #134449, #112481, #26093 ) ) ;
#47129 = CARTESIAN_POINT ( 'NONE',  ( 60.42123663339243933, -43.84677628530859295, -34.92499999999998295 ) ) ;
#47131 = VERTEX_POINT ( 'NONE', #5123 ) ;
#47132 = EDGE_CURVE ( 'NONE', #14903, #44540, #95002, .T. ) ;
#47133 = ADVANCED_FACE ( 'NONE', ( #37819 ), #58895, .F. ) ;
#47134 = CARTESIAN_POINT ( 'NONE',  ( -21.18398860626899349, 28.73617430169802134, 5.000000000000000000 ) ) ;
#47135 = CARTESIAN_POINT ( 'NONE',  ( 104.2500000000000000, -9.735942053221458872E-16, 7.950000000000000178 ) ) ;
#47136 = ORIENTED_EDGE ( 'NONE', *, *, #53166, .F. ) ;
#47137 = SURFACE_STYLE_USAGE ( .BOTH. , #1392 ) ;
#47138 = ORIENTED_EDGE ( 'NONE', *, *, #44508, .T. ) ;
#47140 = ADVANCED_FACE ( 'NONE', ( #71158 ), #82737, .T. ) ;
#47139 = VECTOR ( 'NONE', #5422, 1000.000000000000000 ) ;
#47141 = ADVANCED_FACE ( 'NONE', ( #29752 ), #87006, .T. ) ;
#47142 = CARTESIAN_POINT ( 'NONE',  ( -13.49999999999990408, -1.912538124160735542, 4.000000000000000000 ) ) ;
#47143 = DIRECTION ( 'NONE',  ( -0.7071067811865487940, 0.7071067811865463515, -0.000000000000000000 ) ) ;
#47144 = LINE ( 'NONE', #79763, #39316 ) ;
#47145 = VECTOR ( 'NONE', #83043, 1000.000000000000000 ) ;
#47146 = DIRECTION ( 'NONE',  ( -2.781805975412905890E-17, 0.3543493200069152693, 0.9351131265310292928 ) ) ;
#47147 = DIRECTION ( 'NONE',  ( 0.000000000000000000, 0.000000000000000000, 1.000000000000000000 ) ) ;
#47148 = EDGE_CURVE ( 'NONE', #139503, #84085, #50692, .T. ) ;
#47149 = CARTESIAN_POINT ( 'NONE',  ( 33.18398860626899705, 28.73617430169810305, 5.000000000000000000 ) ) ;
#47150 = DIRECTION ( 'NONE',  ( -0.7071067811865486830, -0.7071067811865464625, -0.000000000000000000 ) ) ;
#47151 = DIRECTION ( 'NONE',  ( -1.000000000000000000, 2.496005001405478586E-15, 0.000000000000000000 ) ) ;
#47152 = CARTESIAN_POINT ( 'NONE',  ( 23.60373647476854941, 5.808823158059036373, 5.808823158059032821 ) ) ;
#47153 = CARTESIAN_POINT ( 'NONE',  ( -31.43312800248722994, -21.74070752338405654, 6.915939825044148392 ) ) ;
#47154 = DIRECTION ( 'NONE',  ( -1.000000000000000000, 0.000000000000000000, 0.000000000000000000 ) ) ;
#47155 = CARTESIAN_POINT ( 'NONE',  ( 24.56840764549667355, -2.500000000000000888, 0.000000000000000000 ) ) ;
#47156 = DIRECTION ( 'NONE',  ( -0.000000000000000000, 0.000000000000000000, 1.000000000000000000 ) ) ;
#47157 = EDGE_LOOP ( 'NONE', ( #50954, #134592, #2905 ) ) ;
#47158 = ORIENTED_EDGE ( 'NONE', *, *, #122692, .F. ) ;
#47160 = EDGE_CURVE ( 'NONE', #119701, #92286, #129073, .T. ) ;
#47159 = CARTESIAN_POINT ( 'NONE',  ( 95.35416666666665719, -2.130196079827425315, -7.950000000000001066 ) ) ;
#47161 = ORIENTED_EDGE ( 'NONE', *, *, #83173, .T. ) ;
#47162 = ORIENTED_EDGE ( 'NONE', *, *, #103725, .F. ) ;
#47163 = ORIENTED_EDGE ( 'NONE', *, *, #4673, .T. ) ;
#47164 = CARTESIAN_POINT ( 'NONE',  ( 9.183988606268997046, 28.73617430169793607, 5.000000000000000000 ) ) ;
#47165 = PLANE ( 'NONE',  #106414 ) ;
#47166 = CIRCLE ( 'NONE', #130420, 3.999999999999989786 ) ;
#47167 = CARTESIAN_POINT ( 'NONE',  ( 10.32500000000000107, 8.432637487761466488, -4.375000000000001776 ) ) ;
#47168 = EDGE_LOOP ( 'NONE', ( #77137, #27634, #26918 ) ) ;
#47169 = LINE ( 'NONE', #79786, #11544 ) ;
#47170 = LINE ( 'NONE', #91350, #58106 ) ;
#47171 = DIRECTION ( 'NONE',  ( -0.000000000000000000, 0.000000000000000000, 1.000000000000000000 ) ) ;
#47172 = CARTESIAN_POINT ( 'NONE',  ( 29.99999999999979750, -3.033600742197707145, 5.000000000000000000 ) ) ;
#47173 = CARTESIAN_POINT ( 'NONE',  ( 56.99451991528749062, 28.92564299267978001, 4.000000000000000000 ) ) ;
#47174 = CARTESIAN_POINT ( 'NONE',  ( 0.000000000000000000, 0.000000000000000000, 5.000000000000000000 ) ) ;
#47176 = VECTOR ( 'NONE', #125777, 1000.000000000000000 ) ;
#47175 = CARTESIAN_POINT ( 'NONE',  ( -1.499999999999990896, -17.56887692260763956, 4.000000000000000000 ) ) ;
#47177 = EDGE_CURVE ( 'NONE', #39146, #3561, #20298, .T. ) ;
#47178 = DIRECTION ( 'NONE',  ( 0.000000000000000000, -1.000000000000000000, 0.000000000000000000 ) ) ;
#47179 = CARTESIAN_POINT ( 'NONE',  ( 27.79289321881326558, -17.24070752338409918, 5.000000000000000000 ) ) ;
#47180 = CARTESIAN_POINT ( 'NONE',  ( 86.70419371712955581, -6.884901960086285300, -3.975000000000000089 ) ) ;
#47181 = LINE ( 'NONE', #136984, #60773 ) ;
#47182 = ORIENTED_EDGE ( 'NONE', *, *, #85559, .T. ) ;
#47183 = ORIENTED_EDGE ( 'NONE', *, *, #112541, .F. ) ;
#47184 = CARTESIAN_POINT ( 'NONE',  ( 111.4170968585647614, 3.054999999999998828, 5.291415217122922066 ) ) ;
#47185 = AXIS2_PLACEMENT_3D ( 'NONE', #62185, #117936, #70930 ) ;
#47186 = ORIENTED_EDGE ( 'NONE', *, *, #116771, .F. ) ;
#47187 = ADVANCED_FACE ( 'NONE', ( #9401 ), #73998, .T. ) ;
#47188 = CARTESIAN_POINT ( 'NONE',  ( 33.09667064187385677, -2.240707523384257716, 15.26439735382760077 ) ) ;
#47189 = DIRECTION ( 'NONE',  ( -0.3543493200069162685, -0.000000000000000000, -0.9351131265310288487 ) ) ;
#47190 = FACE_OUTER_BOUND ( 'NONE', #70795, .T. ) ;
#47192 = VECTOR ( 'NONE', #34699, 1000.000000000000000 ) ;
#47191 = DIRECTION ( 'NONE',  ( 0.6830127018922180770, -0.6830127018922204085, -0.2588190451025213501 ) ) ;
#47193 = EDGE_CURVE ( 'NONE', #54301, #104648, #53689, .T. ) ;
#47194 = CARTESIAN_POINT ( 'NONE',  ( 103.1620968585647802, -5.291415217122919401, 3.054999999999997939 ) ) ;
#47195 = VERTEX_POINT ( 'NONE', #31916 ) ;
#47196 = EDGE_CURVE ( 'NONE', #70864, #26964, #31213, .T. ) ;
#47197 = ORIENTED_EDGE ( 'NONE', *, *, #95412, .F. ) ;
#47198 = DIRECTION ( 'NONE',  ( -0.000000000000000000, -0.3543493200069152693, 0.9351131265310292928 ) ) ;
#47199 = PRODUCT_DEFINITION_FORMATION_WITH_SPECIFIED_SOURCE ( 'ANY', '', #96739, .NOT_KNOWN. ) ;
#47200 = CARTESIAN_POINT ( 'NONE',  ( -13.82816939922343913, -2.240707523384255939, 4.000000000000000000 ) ) ;
#47201 = ADVANCED_FACE ( 'NONE', ( #54412 ), #95738, .F. ) ;
#47202 = ORIENTED_EDGE ( 'NONE', *, *, #117625, .F. ) ;
#47203 = ORIENTED_EDGE ( 'NONE', *, *, #81225, .F. ) ;
#47204 = VERTEX_POINT ( 'NONE', #19601 ) ;
#47205 = FACE_OUTER_BOUND ( 'NONE', #19722, .T. ) ;
#47206 = CARTESIAN_POINT ( 'NONE',  ( 0.1867277030207833977, 3.637003262229598022, -7.062723959547544617 ) ) ;
#47207 = VECTOR ( 'NONE', #16105, 1000.000000000000000 ) ;
#47208 = TOROIDAL_SURFACE ( 'NONE', #128188, 31.92999999999999261, 3.000000000000000000 ) ;
#47209 = CARTESIAN_POINT ( 'NONE',  ( 34.32876352523143737, 0.000000000000000000, -6.109999999999998543 ) ) ;
#47210 = ORIENTED_EDGE ( 'NONE', *, *, #61555, .F. ) ;
#47211 = EDGE_LOOP ( 'NONE', ( #109626, #10147, #117359, #79530 ) ) ;
#47212 = EDGE_CURVE ( 'NONE', #34241, #121192, #7993, .T. ) ;
#47213 = DIRECTION ( 'NONE',  ( -0.7071067811865486830, 0.7071067811865464625, 0.000000000000000000 ) ) ;
#47214 = ORIENTED_EDGE ( 'NONE', *, *, #45934, .T. ) ;
#47215 = ORIENTED_EDGE ( 'NONE', *, *, #88012, .T. ) ;
#47216 = VECTOR ( 'NONE', #29197, 1000.000000000000000 ) ;
#47217 = CARTESIAN_POINT ( 'NONE',  ( -15.18398860626900237, 28.73617430169797871, 5.000000000000000000 ) ) ;
#47218 = LINE ( 'NONE', #68245, #89213 ) ;
#47219 = DIRECTION ( 'NONE',  ( -0.7071067811865487940, 0.7071067811865463515, 0.000000000000000000 ) ) ;
#47220 = EDGE_CURVE ( 'NONE', #80916, #119727, #73294, .T. ) ;
#47221 = ORIENTED_EDGE ( 'NONE', *, *, #62266, .F. ) ;
#47222 = PRESENTATION_LAYER_ASSIGNMENT (  '', '', ( #109659 ) ) ;
#47223 = DIRECTION ( 'NONE',  ( -1.000000000000000000, 0.000000000000000000, -0.000000000000000000 ) ) ;
#47224 = CARTESIAN_POINT ( 'NONE',  ( -33.48921356237309510, -27.52281430457078670, 5.000000000000000000 ) ) ;
#47225 = CARTESIAN_POINT ( 'NONE',  ( -22.03340032343008659, 6.759292476615653023, 12.28218704918517012 ) ) ;
#47226 = CARTESIAN_POINT ( 'NONE',  ( -3.183988606268992161, 28.73617430169789699, 5.000000000000000000 ) ) ;
#47227 = VECTOR ( 'NONE', #73211, 1000.000000000000000 ) ;
#47228 = ADVANCED_FACE ( 'NONE', ( #97889 ), #8676, .F. ) ;
#47229 = FACE_BOUND ( 'NONE', #74, .T. ) ;
#47230 = ORIENTED_EDGE ( 'NONE', *, *, #26284, .F. ) ;
#47231 = CARTESIAN_POINT ( 'NONE',  ( -32.99999999999977263, 7.007997736742408890, -8.085015511992185822 ) ) ;
#47232 = DIRECTION ( 'NONE',  ( 0.7071067811865486830, -0.7071067811865464625, -0.000000000000000000 ) ) ;
#47233 = VERTEX_POINT ( 'NONE', #119604 ) ;
#47234 = CARTESIAN_POINT ( 'NONE',  ( -34.49999999999975131, -16.53574439159933718, 4.994342998332169437 ) ) ;
#47235 = ORIENTED_EDGE ( 'NONE', *, *, #142685, .T. ) ;
#47236 = EDGE_LOOP ( 'NONE', ( #106188, #30238, #107049, #3670 ) ) ;
#47237 = CIRCLE ( 'NONE', #3181, 3.999999999999989786 ) ;
#47238 = VERTEX_POINT ( 'NONE', #63847 ) ;
#47239 = CIRCLE ( 'NONE', #56544, 2.552699999999928693 ) ;
#47240 = EDGE_CURVE ( 'NONE', #27120, #94114, #142128, .T. ) ;
#47241 = CARTESIAN_POINT ( 'NONE',  ( 38.99543019189812298, 5.291415217122916737, 3.055000000000001936 ) ) ;
#47242 = DIRECTION ( 'NONE',  ( -0.7071067811865486830, -0.7071067811865464625, 0.000000000000000000 ) ) ;
#47244 = ORIENTED_EDGE ( 'NONE', *, *, #107014, .T. ) ;
#47243 = VECTOR ( 'NONE', #70942, 1000.000000000000227 ) ;
#47245 = CARTESIAN_POINT ( 'NONE',  ( 54.18398860626899705, 28.73617430169825226, 5.000000000000000000 ) ) ;
#47246 = DIRECTION ( 'NONE',  ( 0.7071067811865487940, 0.7071067811865463515, 0.000000000000000000 ) ) ;
#47247 = ORIENTED_EDGE ( 'NONE', *, *, #112637, .T. ) ;
#47248 = VECTOR ( 'NONE', #70820, 1000.000000000000000 ) ;
#47249 = ADVANCED_FACE ( 'NONE', ( #129790 ), #62422, .F. ) ;
#47250 =( NAMED_UNIT ( * ) PLANE_ANGLE_UNIT ( ) SI_UNIT ( $, .RADIAN. ) );
#47251 = EDGE_CURVE ( 'NONE', #29429, #36313, #84189, .T. ) ;
#47252 = CYLINDRICAL_SURFACE ( 'NONE', #38652, 3.000000000000000000 ) ;
#47253 = CARTESIAN_POINT ( 'NONE',  ( 1.042387978378689795, -2.055000000000000160, 0.000000000000000000 ) ) ;
#47254 = LINE ( 'NONE', #58842, #45943 ) ;
#47255 = DIRECTION ( 'NONE',  ( -0.7071067811865486830, -0.7071067811865464625, 0.000000000000000000 ) ) ;
#47256 = ORIENTED_EDGE ( 'NONE', *, *, #77225, .T. ) ;
#47257 = ORIENTED_EDGE ( 'NONE', *, *, #66682, .T. ) ;
#47259 = ORIENTED_EDGE ( 'NONE', *, *, #139079, .F. ) ;
#47258 = VECTOR ( 'NONE', #95174, 1000.000000000000227 ) ;
#47260 = ORIENTED_EDGE ( 'NONE', *, *, #21075, .T. ) ;
#47261 = DIRECTION ( 'NONE',  ( -1.000000000000000000, 0.000000000000000000, 0.000000000000000000 ) ) ;
#47262 = ORIENTED_EDGE ( 'NONE', *, *, #50725, .F. ) ;
#47263 = ORIENTED_EDGE ( 'NONE', *, *, #113080, .T. ) ;
#47264 = DIRECTION ( 'NONE',  ( -1.000000000000000000, -1.224606353822377258E-16, -0.000000000000000000 ) ) ;
#47265 = EDGE_CURVE ( 'NONE', #30447, #22650, #18138, .T. ) ;
#47266 = LINE ( 'NONE', #2970, #101880 ) ;
#47267 = ORIENTED_EDGE ( 'NONE', *, *, #112271, .F. ) ;
#47268 = LINE ( 'NONE', #92840, #136711 ) ;
#47269 = VERTEX_POINT ( 'NONE', #51543 ) ;
#47270 = DIRECTION ( 'NONE',  ( 0.7071067811865487940, 0.7071067811865463515, 0.000000000000000000 ) ) ;
#47271 = CARTESIAN_POINT ( 'NONE',  ( 30.54623647476855552, -7.934999999999990727, 4.858786175617117713E-16 ) ) ;
#47272 = AXIS2_PLACEMENT_3D ( 'NONE', #112304, #47786, #125313 ) ;
#47273 = CARTESIAN_POINT ( 'NONE',  ( 2.837903141435219379, -6.871911579029513106, -3.967499999999993587 ) ) ;
#47274 = ORIENTED_EDGE ( 'NONE', *, *, #142492, .F. ) ;
#47276 = LINE ( 'NONE', #91447, #40667 ) ;
#47275 = CARTESIAN_POINT ( 'NONE',  ( 115.1204301918981230, 3.055000000000002380, -5.291415217122917625 ) ) ;
#47277 = LINE ( 'NONE', #124070, #30377 ) ;
#47278 = SURFACE_STYLE_FILL_AREA ( #102337 ) ;
#47279 = ORIENTED_EDGE ( 'NONE', *, *, #84488, .T. ) ;
#47280 =( NAMED_UNIT ( * ) SI_UNIT ( $, .STERADIAN. ) SOLID_ANGLE_UNIT ( ) );
#47282 = EDGE_LOOP ( 'NONE', ( #109730, #30908, #81404, #104787 ) ) ;
#47281 = DIRECTION ( 'NONE',  ( 1.000000000000000000, 0.000000000000000000, 0.000000000000000000 ) ) ;
#47283 = DIRECTION ( 'NONE',  ( -0.000000000000000000, 0.3543493200069153248, 0.9351131265310292928 ) ) ;
#47284 = DIRECTION ( 'NONE',  ( 0.6830127018922180770, -0.6830127018922204085, -0.2588190451025213501 ) ) ;
#47285 = CARTESIAN_POINT ( 'NONE',  ( 26.35681257248245046, -20.24070752338406720, 21.22881796311218849 ) ) ;
#47286 = CYLINDRICAL_SURFACE ( 'NONE', #95540, 0.5000000000000004441 ) ;
#47287 = DIRECTION ( 'NONE',  ( 1.000000000000000000, 0.000000000000000000, 0.000000000000000000 ) ) ;
#47289 = EDGE_LOOP ( 'NONE', ( #62786, #3998, #42147 ) ) ;
#47288 = VECTOR ( 'NONE', #1317, 1000.000000000000227 ) ;
#47290 = FACE_OUTER_BOUND ( 'NONE', #15476, .T. ) ;
#47291 = LINE ( 'NONE', #59561, #34952 ) ;
#47292 = DIRECTION ( 'NONE',  ( 0.7071067811865486830, -0.7071067811865464625, -0.000000000000000000 ) ) ;
#47293 = ORIENTED_EDGE ( 'NONE', *, *, #36660, .T. ) ;
#47294 = CARTESIAN_POINT ( 'NONE',  ( -22.49999999999984013, -4.796895815301037480, -3.611700055028734813 ) ) ;
#47295 = CARTESIAN_POINT ( 'NONE',  ( 14.99999999999989697, -12.03360074219761700, 5.000000000000000000 ) ) ;
#47296 = ORIENTED_EDGE ( 'NONE', *, *, #118936, .F. ) ;
#47298 = ORIENTED_EDGE ( 'NONE', *, *, #34666, .F. ) ;
#47297 = FACE_OUTER_BOUND ( 'NONE', #143450, .T. ) ;
#47299 = EDGE_CURVE ( 'NONE', #86644, #116711, #139985, .T. ) ;
#47300 = ORIENTED_EDGE ( 'NONE', *, *, #67462, .T. ) ;
#47301 = CARTESIAN_POINT ( 'NONE',  ( 8.131392392196376662, 12.20025264268591059, -25.50689499364121815 ) ) ;
#47302 = VECTOR ( 'NONE', #56150, 1000.000000000000000 ) ;
#47303 = ORIENTED_EDGE ( 'NONE', *, *, #125732, .T. ) ;
#47304 = ADVANCED_FACE ( 'NONE', ( #35523 ), #113021, .F. ) ;
#47305 = EDGE_CURVE ( 'NONE', #64792, #33497, #118781, .T. ) ;
#47306 = EDGE_CURVE ( 'NONE', #84441, #74571, #102182, .T. ) ;
#47307 = VECTOR ( 'NONE', #63362, 1000.000000000000000 ) ;
#47308 = DIRECTION ( 'NONE',  ( -0.7071067811865487940, 0.7071067811865463515, 0.000000000000000000 ) ) ;
#47309 = EDGE_CURVE ( 'NONE', #26834, #20276, #46404, .T. ) ;
#47310 = VERTEX_POINT ( 'NONE', #1390 ) ;
#47311 = CARTESIAN_POINT ( 'NONE',  ( 7.600000000000009415, 1.530808498934156811E-16, -1.249999999999971578 ) ) ;
#47312 = EDGE_CURVE ( 'NONE', #129516, #46199, #13696, .T. ) ;
#47313 = DIRECTION ( 'NONE',  ( -0.6830127018922181881, 0.6830127018922202975, -0.2588190451025214056 ) ) ;
#47314 = DIRECTION ( 'NONE',  ( -0.7071067811865486830, -0.7071067811865464625, -0.000000000000000000 ) ) ;
#47315 = DIRECTION ( 'NONE',  ( -0.000000000000000000, 0.000000000000000000, 1.000000000000000000 ) ) ;
#47316 = PLANE ( 'NONE',  #85343 ) ;
#47317 = EDGE_CURVE ( 'NONE', #86570, #87517, #45679, .T. ) ;
#47318 = DIRECTION ( 'NONE',  ( -1.000000000000000000, -3.115803279706882722E-16, 0.000000000000000000 ) ) ;
#47319 = FACE_OUTER_BOUND ( 'NONE', #89521, .T. ) ;
#47320 = ORIENTED_EDGE ( 'NONE', *, *, #121085, .T. ) ;
#47321 = VERTEX_POINT ( 'NONE', #77586 ) ;
#47322 = VERTEX_POINT ( 'NONE', #11551 ) ;
#47324 = ADVANCED_FACE ( 'NONE', ( #90589 ), #55106, .F. ) ;
#47323 = CARTESIAN_POINT ( 'NONE',  ( 119.8541666666666430, -2.130196079827425315, -7.950000000000001066 ) ) ;
#47325 = VERTEX_POINT ( 'NONE', #12990 ) ;
#47326 = VECTOR ( 'NONE', #100559, 1000.000000000000000 ) ;
#47327 = VERTEX_POINT ( 'NONE', #66003 ) ;
#47328 = VERTEX_POINT ( 'NONE', #121753 ) ;
#47329 = CARTESIAN_POINT ( 'NONE',  ( 1.130059519929533574, -4.629186425066019517, -5.239578231266678543 ) ) ;
#47330 = CARTESIAN_POINT ( 'NONE',  ( -1.499999999999982236, -7.912538124160676922, 4.000000000000000000 ) ) ;
#47331 = ORIENTED_EDGE ( 'NONE', *, *, #69726, .F. ) ;
#47332 = CARTESIAN_POINT ( 'NONE',  ( 11.56505274454301357, 4.584330080086930965E-16, 0.000000000000000000 ) ) ;
#47334 = VECTOR ( 'NONE', #85030, 1000.000000000000000 ) ;
#47333 = CARTESIAN_POINT ( 'NONE',  ( 25.39999999999999858, 7.796566843815467607, 1.475727091950665537 ) ) ;
#47335 = EDGE_CURVE ( 'NONE', #23253, #27215, #19704, .T. ) ;
#47336 = CARTESIAN_POINT ( 'NONE',  ( 27.48921356237309155, -27.52281430457074762, 5.000000000000000000 ) ) ;
#47337 = VECTOR ( 'NONE', #70454, 1000.000000000000000 ) ;
#47338 = CARTESIAN_POINT ( 'NONE',  ( 99.53752705046289861, -9.735942053221456900E-16, 7.949999999999998401 ) ) ;
#47339 = CARTESIAN_POINT ( 'NONE',  ( 109.8129301918981042, -1.637169565754159617, -6.110000000000001208 ) ) ;
#47340 = EDGE_LOOP ( 'NONE', ( #129436, #117735, #120086, #58943 ) ) ;
#47341 = CARTESIAN_POINT ( 'NONE',  ( 42.18398860626899705, 28.73617430169816700, 5.000000000000000000 ) ) ;
#47342 = PLANE ( 'NONE',  #79272 ) ;
#47343 = LINE ( 'NONE', #14654, #28834 ) ;
#47344 = ADVANCED_FACE ( 'NONE', ( #21756 ), #22432, .F. ) ;
#47345 = DIRECTION ( 'NONE',  ( 0.7071067811865487940, 0.7071067811865463515, 0.000000000000000000 ) ) ;
#47346 = LINE ( 'NONE', #124841, #43525 ) ;
#47347 = PRESENTATION_LAYER_ASSIGNMENT (  '', '', ( #135371 ) ) ;
#47348 = CARTESIAN_POINT ( 'NONE',  ( 50.97502705046287730, -5.819803920172572198, 5.819803920172572198 ) ) ;
#47349 = CARTESIAN_POINT ( 'NONE',  ( 1.199999999999999956, 0.5999999999999987566, 4.543283425070392845 ) ) ;
#47350 = VECTOR ( 'NONE', #106361, 1000.000000000000000 ) ;
#47351 = LINE ( 'NONE', #26259, #138774 ) ;
#47353 = ORIENTED_EDGE ( 'NONE', *, *, #40526, .T. ) ;
#47352 = B_SPLINE_CURVE_WITH_KNOTS ( 'NONE', 3,
 ( #20683, #137675, #52602, #38347 ),
 .UNSPECIFIED., .F., .F.,
 ( 4, 4 ),
 ( 0.008853860144884173958, 0.009403245473020183098 ),
 .UNSPECIFIED. ) ;
#47354 = ORIENTED_EDGE ( 'NONE', *, *, #11005, .T. ) ;
#47355 = CARTESIAN_POINT ( 'NONE',  ( 36.14583333333332149, 2.130196079827431976, -7.949999999999999289 ) ) ;
#47356 = ORIENTED_EDGE ( 'NONE', *, *, #116834, .T. ) ;
#47357 = ORIENTED_EDGE ( 'NONE', *, *, #130953, .F. ) ;
#47358 = CARTESIAN_POINT ( 'NONE',  ( 19.49999999999986500, 22.22500000000000142, 4.362957392718781691 ) ) ;
#47359 = CARTESIAN_POINT ( 'NONE',  ( 2.510786437626908008, -27.52281430457053446, 5.000000000000000000 ) ) ;
#47360 = VERTEX_POINT ( 'NONE', #23903 ) ;
#47361 = CARTESIAN_POINT ( 'NONE',  ( 0.000000000000000000, 0.000000000000000000, 5.000000000000000000 ) ) ;
#47362 = CARTESIAN_POINT ( 'NONE',  ( -15.18398860626900237, 28.73617430169797871, 5.000000000000000000 ) ) ;
#47363 = CARTESIAN_POINT ( 'NONE',  ( 42.58376352523143993, -6.110000000000001208, -3.741295971395164515E-16 ) ) ;
#47364 = ORIENTED_EDGE ( 'NONE', *, *, #68016, .F. ) ;
#47365 = EDGE_CURVE ( 'NONE', #42167, #15337, #110165, .T. ) ;
#47366 = LINE ( 'NONE', #126292, #6249 ) ;
#47367 = VERTEX_POINT ( 'NONE', #133385 ) ;
#47368 = VECTOR ( 'NONE', #112320, 1000.000000000000000 ) ;
#47369 = CARTESIAN_POINT ( 'NONE',  ( 19.49999999999987210, 16.46639925780209524, 5.000000000000000000 ) ) ;
#47370 = LINE ( 'NONE', #922, #91669 ) ;
#47372 = ADVANCED_FACE ( 'NONE', ( #112337 ), #89847, .T. ) ;
#47371 = DIRECTION ( 'NONE',  ( 1.318980745116185161E-16, -1.000000000000000000, 0.000000000000000000 ) ) ;
#47373 = FACE_OUTER_BOUND ( 'NONE', #10942, .T. ) ;
#47374 = ORIENTED_EDGE ( 'NONE', *, *, #90770, .F. ) ;
#47375 = VERTEX_POINT ( 'NONE', #2090 ) ;
#47376 = DIRECTION ( 'NONE',  ( -0.000000000000000000, 0.000000000000000000, 1.000000000000000000 ) ) ;
#47377 = CARTESIAN_POINT ( 'NONE',  ( 14.52487387214945613, 14.25929247661557575, 9.797011795316668881 ) ) ;
#47378 = CARTESIAN_POINT ( 'NONE',  ( 4.828169399223495084, 9.759292476615614831, 4.000000000000000000 ) ) ;
#47379 = LINE ( 'NONE', #79283, #6939 ) ;
#47380 = DIRECTION ( 'NONE',  ( 0.7071067811865487940, 0.7071067811865463515, -0.000000000000000000 ) ) ;
#47381 = CARTESIAN_POINT ( 'NONE',  ( 61.01626352523143737, -4.472830434245839371, 4.472830434245839371 ) ) ;
#47382 = CARTESIAN_POINT ( 'NONE',  ( 125.1041666666666572, 2.130196079827431532, 7.949999999999996625 ) ) ;
#47383 = EDGE_CURVE ( 'NONE', #102967, #115135, #690, .T. ) ;
#47384 = DIRECTION ( 'NONE',  ( 0.000000000000000000, 0.000000000000000000, 1.000000000000000000 ) ) ;
#47385 = ORIENTED_EDGE ( 'NONE', *, *, #77224, .T. ) ;
#47386 = ORIENTED_EDGE ( 'NONE', *, *, #66725, .T. ) ;
#47387 = DIRECTION ( 'NONE',  ( -1.369518533665900312E-16, 1.000000000000000000, -0.000000000000000000 ) ) ;
#47388 = VERTEX_POINT ( 'NONE', #44986 ) ;
#47389 = AXIS2_PLACEMENT_3D ( 'NONE', #5953, #117570, #63951 ) ;
#47390 = DIRECTION ( 'NONE',  ( -0.7071067811865486830, 0.7071067811865464625, 0.000000000000000000 ) ) ;
#47391 = ORIENTED_EDGE ( 'NONE', *, *, #124617, .F. ) ;
#47392 = SURFACE_STYLE_USAGE ( .BOTH. , #124184 ) ;
#47393 = CARTESIAN_POINT ( 'NONE',  ( 15.29974487139158867, -27.71228299555216879, 4.000000000000000000 ) ) ;
#47394 = CARTESIAN_POINT ( 'NONE',  ( -34.45011844616454511, 22.22499999999999787, 4.231322045536046517 ) ) ;
#47395 = B_SPLINE_CURVE_WITH_KNOTS ( 'NONE', 3,
 ( #127450, #72411, #116580, #17265, #125324, #73105, #61527, #17943, #26715, #83990, #95527, #139793, #114434, #6337, #15102, #70958, #128191, #48467, #92667, #136906, #28869, #117263, #37608, #126050, #115113, #15783, #60079, #104248, #130330, #9948, #54221, #20820, #62942, #96222, #52735, #98408 ),
 .UNSPECIFIED., .F., .F.,
 ( 4, 2, 2, 2, 2, 2, 2, 2, 2, 2, 2, 2, 2, 2, 2, 2, 2, 4 ),
 ( 0.006941909043857026965, 0.007808636908474057142, 0.008675364773091087320, 0.009542092637708117497, 0.01040882050232514767, 0.01127554836694217785, 0.01214227623155920976, 0.01300900409617623821, 0.01387573196079327012, 0.01474245982541030030, 0.01560918769002733048, 0.01647591555464435892, 0.01734264341926139083, 0.01820937128387842274, 0.01907609914849545119, 0.01994282701311247963, 0.02037619094542100079, 0.02080955487772951848 ),
 .UNSPECIFIED. ) ;
#47396 = EDGE_CURVE ( 'NONE', #80017, #11776, #89158, .T. ) ;
#47397 = FACE_BOUND ( 'NONE', #122509, .T. ) ;
#47398 = CARTESIAN_POINT ( 'NONE',  ( 12.48921356237309155, -27.52281430457064104, 5.000000000000000000 ) ) ;
#47399 = ADVANCED_FACE ( 'NONE', ( #23143 ), #67423, .F. ) ;
#47400 = DIRECTION ( 'NONE',  ( 1.000000000000000000, 0.000000000000000000, 0.000000000000000000 ) ) ;
#47401 = ADVANCED_FACE ( 'NONE', ( #71693 ), #135525, .F. ) ;
#47403 = VERTEX_POINT ( 'NONE', #138363 ) ;
#47402 = DIRECTION ( 'NONE',  ( 0.7071067811865486830, -0.7071067811865464625, -0.000000000000000000 ) ) ;
#47404 = VECTOR ( 'NONE', #142254, 1000.000000000000227 ) ;
#47405 = CARTESIAN_POINT ( 'NONE',  ( 30.32816939922331656, -9.740707523384177335, 4.000000000000000000 ) ) ;
#47406 = ORIENTED_EDGE ( 'NONE', *, *, #18175, .F. ) ;
#47407 = ADVANCED_FACE ( 'NONE', ( #113752 ), #126075, .F. ) ;
#47408 = VERTEX_POINT ( 'NONE', #114455 ) ;
#47409 = CARTESIAN_POINT ( 'NONE',  ( 67.57876352523145158, -7.482591942790325086E-16, 6.109999999999998543 ) ) ;
#47410 = ORIENTED_EDGE ( 'NONE', *, *, #53108, .T. ) ;
#47411 = LINE ( 'NONE', #81444, #41798 ) ;
#47412 = CIRCLE ( 'NONE', #82161, 3.000000000000002665 ) ;
#47413 = EDGE_LOOP ( 'NONE', ( #57267, #57269, #42413 ) ) ;
#47414 = SURFACE_STYLE_FILL_AREA ( #59684 ) ;
#47415 = EDGE_CURVE ( 'NONE', #42016, #21974, #14447, .T. ) ;
#47416 = PLANE ( 'NONE',  #95813 ) ;
#47417 = ADVANCED_FACE ( 'NONE', ( #91317 ), #5677, .F. ) ;
#47418 = CARTESIAN_POINT ( 'NONE',  ( 2.207106781186528810, -2.240707523384262601, 5.000000000000000000 ) ) ;
#47419 = AXIS2_PLACEMENT_3D ( 'NONE', #73638, #62776, #19950 ) ;
#47420 = CARTESIAN_POINT ( 'NONE',  ( 5.066132482466838560, -22.22500000000000142, 20.15413504464201822 ) ) ;
#47421 = AXIS2_PLACEMENT_3D ( 'NONE', #69815, #113994, #103796 ) ;
#47422 = DIRECTION ( 'NONE',  ( 0.6830127018922180770, -0.6830127018922204085, -0.2588190451025213501 ) ) ;
#47423 = LINE ( 'NONE', #134390, #74795 ) ;
#47424 = DIRECTION ( 'NONE',  ( 1.000000000000000000, 0.000000000000000000, 0.000000000000000000 ) ) ;
#47425 = ORIENTED_EDGE ( 'NONE', *, *, #67435, .F. ) ;
#47426 = ORIENTED_EDGE ( 'NONE', *, *, #133847, .T. ) ;
#47427 = CARTESIAN_POINT ( 'NONE',  ( -27.79289321881325492, 3.759292476615681888, 5.000000000000000000 ) ) ;
#47428 = CARTESIAN_POINT ( 'NONE',  ( -9.183988606268997046, 28.73617430169793607, 5.000000000000000000 ) ) ;
#47429 = ORIENTED_EDGE ( 'NONE', *, *, #114572, .F. ) ;
#47430 = VERTEX_POINT ( 'NONE', #83271 ) ;
#47431 = ORIENTED_EDGE ( 'NONE', *, *, #105092, .T. ) ;
#47432 = EDGE_CURVE ( 'NONE', #30215, #14419, #26741, .T. ) ;
#47433 = CARTESIAN_POINT ( 'NONE',  ( -34.92500000000001137, -22.22500000000000142, 4.500000000000000888 ) ) ;
#47434 = ORIENTED_EDGE ( 'NONE', *, *, #89668, .T. ) ;
#47435 = CARTESIAN_POINT ( 'NONE',  ( 149.2199999999997999, -3.180000000000061444, 34.92499999999998295 ) ) ;
#47436 = VECTOR ( 'NONE', #103204, 1000.000000000000000 ) ;
#47437 = SURFACE_SIDE_STYLE ('',( #122799 ) ) ;
#47438 = STYLED_ITEM ( 'NONE', ( #45127 ), #44753 ) ;
#47439 = CARTESIAN_POINT ( 'NONE',  ( 31.83747294953710849, 6.094999999999989981, -1.119633336120465690E-15 ) ) ;
#47440 = CIRCLE ( 'NONE', #123781, 1.898649999999993065 ) ;
#47441 = CARTESIAN_POINT ( 'NONE',  ( 2.999999999999983569, 16.93112307739200872, 4.000000000000000000 ) ) ;
#47442 = EDGE_LOOP ( 'NONE', ( #54249, #69766, #38902, #76343 ) ) ;
#47443 = VECTOR ( 'NONE', #78930, 1000.000000000000227 ) ;
#47444 = LINE ( 'NONE', #59715, #124394 ) ;
#47445 = PLANE ( 'NONE',  #53568 ) ;
#47446 = DIRECTION ( 'NONE',  ( 0.7071067811865487940, -0.7071067811865463515, 0.000000000000000000 ) ) ;
#47448 = ORIENTED_EDGE ( 'NONE', *, *, #74587, .F. ) ;
#47447 = LINE ( 'NONE', #48118, #24084 ) ;
#47449 = ORIENTED_EDGE ( 'NONE', *, *, #77395, .T. ) ;
#47450 = CARTESIAN_POINT ( 'NONE',  ( -36.29974487139159578, -27.71228299555231445, 4.000000000000000000 ) ) ;
#47451 = DIRECTION ( 'NONE',  ( -1.000000000000000000, 0.000000000000000000, 0.000000000000000000 ) ) ;
#47452 = DIRECTION ( 'NONE',  ( -0.000000000000000000, 0.3543493200069153248, 0.9351131265310292928 ) ) ;
#47453 = ORIENTED_EDGE ( 'NONE', *, *, #132510, .T. ) ;
#47454 = DIRECTION ( 'NONE',  ( 0.7071067811865487940, 0.7071067811865463515, -0.000000000000000000 ) ) ;
#47455 = CARTESIAN_POINT ( 'NONE',  ( 33.29974487139158867, -27.71228299555229313, 4.000000000000000000 ) ) ;
#47456 = CARTESIAN_POINT ( 'NONE',  ( 27.83333333333332149, -6.884901960086287964, 3.974999999999998312 ) ) ;
#47458 = EDGE_CURVE ( 'NONE', #126408, #48693, #127482, .T. ) ;
#47457 = DIRECTION ( 'NONE',  ( 1.000000000000000000, 0.000000000000000000, 0.000000000000000000 ) ) ;
#47459 = VERTEX_POINT ( 'NONE', #38342 ) ;
#47460 = DIRECTION ( 'NONE',  ( 0.7071067811865487940, 0.7071067811865463515, -0.000000000000000000 ) ) ;
#47461 = CARTESIAN_POINT ( 'NONE',  ( -2.700255128608413990, -27.71228299555204089, 4.000000000000000000 ) ) ;
#47462 = CARTESIAN_POINT ( 'NONE',  ( 20.46247294953710849, -7.464222240803106570E-16, -6.094999999999989981 ) ) ;
#47463 = DIRECTION ( 'NONE',  ( -1.000000000000000000, -1.224606353822377258E-16, -0.000000000000000000 ) ) ;
#47464 = DIRECTION ( 'NONE',  ( -0.7071067811865487940, 0.7071067811865463515, 0.000000000000000000 ) ) ;
#47465 = ORIENTED_EDGE ( 'NONE', *, *, #71853, .F. ) ;
#47466 = ORIENTED_EDGE ( 'NONE', *, *, #61575, .T. ) ;
#47467 = DIRECTION ( 'NONE',  ( -1.000000000000000000, -0.000000000000000000, -0.000000000000000000 ) ) ;
#47468 = CARTESIAN_POINT ( 'NONE',  ( -14.67183060077637080, -9.740707523384180888, 4.000000000000000000 ) ) ;
#47469 = CARTESIAN_POINT ( 'NONE',  ( 5.228736474768552078, 5.808823158059031044, -5.808823158059038150 ) ) ;
#47470 = CARTESIAN_POINT ( 'NONE',  ( 34.92499999999998295, 14.93779483949076159, 7.761394445350724425 ) ) ;
#47471 = EDGE_CURVE ( 'NONE', #141889, #115637, #70987, .T. ) ;
#47472 = DIRECTION ( 'NONE',  ( -0.000000000000000000, -0.000000000000000000, -1.000000000000000000 ) ) ;
#47473 = DIRECTION ( 'NONE',  ( -0.6830127018922181881, 0.6830127018922202975, -0.2588190451025214056 ) ) ;
#47474 = LINE ( 'NONE', #124978, #23627 ) ;
#47475 = EDGE_CURVE ( 'NONE', #91561, #102725, #18846, .T. ) ;
#47476 = EDGE_CURVE ( 'NONE', #33791, #116900, #80436, .T. ) ;
#47477 = VERTEX_POINT ( 'NONE', #15814 ) ;
#47478 = PLANE ( 'NONE',  #118255 ) ;
#47479 = ADVANCED_FACE ( 'NONE', ( #125352 ), #25302, .F. ) ;
#47480 = UNCERTAINTY_MEASURE_WITH_UNIT (LENGTH_MEASURE( 1.000000000000000082E-05 ), #9837, 'distance_accuracy_value', 'NONE');
#47481 = DIRECTION ( 'NONE',  ( 0.7071067811865487940, 0.7071067811865463515, 0.000000000000000000 ) ) ;
#47482 = DIRECTION ( 'NONE',  ( 0.7071067811865487940, -0.7071067811865463515, 0.000000000000000000 ) ) ;
#47483 = ADVANCED_FACE ( 'NONE', ( #58723 ), #4941, .F. ) ;
#47484 = CARTESIAN_POINT ( 'NONE',  ( 51.82876352523144448, 0.000000000000000000, -6.109999999999999432 ) ) ;
#47485 = AXIS2_PLACEMENT_3D ( 'NONE', #34900, #101547, #112446 ) ;
#47486 = CARTESIAN_POINT ( 'NONE',  ( -1.499999999999994449, 3.073033219394623483, -6.593910359670974053 ) ) ;
#47487 = FACE_OUTER_BOUND ( 'NONE', #48949, .T. ) ;
#47488 = ORIENTED_EDGE ( 'NONE', *, *, #12875, .T. ) ;
#47489 = EDGE_CURVE ( 'NONE', #63122, #13922, #82558, .T. ) ;
#47490 = LINE ( 'NONE', #36554, #69758 ) ;
#47491 = VERTEX_POINT ( 'NONE', #107844 ) ;
#47492 = LINE ( 'NONE', #134463, #10760 ) ;
#47493 = LINE ( 'NONE', #113392, #60028 ) ;
#47494 = CARTESIAN_POINT ( 'NONE',  ( 15.18398860626900237, 28.73617430169797871, 5.000000000000000000 ) ) ;
#47495 = EDGE_CURVE ( 'NONE', #36972, #45062, #1999, .T. ) ;
#47496 = LINE ( 'NONE', #91658, #139002 ) ;
#47497 = EDGE_CURVE ( 'NONE', #8014, #138855, #53501, .T. ) ;
#47498 = DIRECTION ( 'NONE',  ( 0.000000000000000000, 1.000000000000000000, 0.000000000000000000 ) ) ;
#47499 = ORIENTED_EDGE ( 'NONE', *, *, #143392, .F. ) ;
#47500 = EDGE_LOOP ( 'NONE', ( #85772, #95415, #123666, #112548 ) ) ;
#47501 = PLANE ( 'NONE',  #76485 ) ;
#47502 = CARTESIAN_POINT ( 'NONE',  ( -29.99451991528749417, 28.92564299267958816, 4.000000000000000000 ) ) ;
#47503 = UNCERTAINTY_MEASURE_WITH_UNIT (LENGTH_MEASURE( 1.000000000000000082E-05 ), #116815, 'distance_accuracy_value', 'NONE');
#47504 = LINE ( 'NONE', #26420, #17236 ) ;
#47505 = EDGE_CURVE ( 'NONE', #98113, #86260, #97708, .T. ) ;
#47506 = CARTESIAN_POINT ( 'NONE',  ( 57.48921356237308800, -27.52281430457095368, 5.000000000000000000 ) ) ;
#47507 = CARTESIAN_POINT ( 'NONE',  ( 77.22502705046287019, 5.819803920172573086, -5.819803920172572198 ) ) ;
#47508 = DIRECTION ( 'NONE',  ( 0.3543493200069162685, -0.000000000000000000, -0.9351131265310288487 ) ) ;
#47509 = AXIS2_PLACEMENT_3D ( 'NONE', #70170, #79626, #24465 ) ;
#47510 = CARTESIAN_POINT ( 'NONE',  ( 19.05000000000000071, 3.174999999999997158, 1.444000000000000394 ) ) ;
#47511 = ORIENTED_EDGE ( 'NONE', *, *, #111962, .T. ) ;
#47512 = CARTESIAN_POINT ( 'NONE',  ( 59.62500000000000000, -7.950000000000000178, -4.867971026610729436E-16 ) ) ;
#47513 = CARTESIAN_POINT ( 'NONE',  ( 2.924914550060625285, 4.584330080086930965E-16, 0.000000000000000000 ) ) ;
#47514 = CIRCLE ( 'NONE', #133164, 2.500000000000000888 ) ;
#47515 = CARTESIAN_POINT ( 'NONE',  ( -21.18398860626899349, 28.73617430169802134, 5.000000000000000000 ) ) ;
#47516 = DIRECTION ( 'NONE',  ( 0.6830127018922181881, 0.6830127018922202975, -0.2588190451025214056 ) ) ;
#47517 = ORIENTED_EDGE ( 'NONE', *, *, #116484, .T. ) ;
#47518 =( BOUNDED_CURVE ( )  B_SPLINE_CURVE ( 3, ( #80337, #11621, #22498, #53762 ),
 .UNSPECIFIED., .F., .F. ) 
 B_SPLINE_CURVE_WITH_KNOTS ( ( 4, 4 ),
 ( 4.350170835173036821, 4.500739107949214279 ),
 .UNSPECIFIED. ) 
 CURVE ( )  GEOMETRIC_REPRESENTATION_ITEM ( )  RATIONAL_B_SPLINE_CURVE ( ( 1.000000000000000000, 0.9981116584018959736, 0.9981116584018959736, 1.000000000000000000 ) ) 
 REPRESENTATION_ITEM ( '' )  );
#47519 = CARTESIAN_POINT ( 'NONE',  ( 28.49999999999980460, -19.91253812416055169, 4.000000000000000000 ) ) ;
#47520 = CIRCLE ( 'NONE', #103040, 2.500000000000000888 ) ;
#47521 = DIRECTION ( 'NONE',  ( 0.000000000000000000, -1.000000000000000000, 0.000000000000000000 ) ) ;
#47522 = CARTESIAN_POINT ( 'NONE',  ( 64.31293019189810423, -1.637169565754159617, -6.110000000000001208 ) ) ;
#47523 = ADVANCED_FACE ( 'NONE', ( #7087 ), #75963, .F. ) ;
#47524 = LINE ( 'NONE', #14108, #15859 ) ;
#47525 = VERTEX_POINT ( 'NONE', #30313 ) ;
#47526 = VERTEX_POINT ( 'NONE', #84696 ) ;
#47527 =( BOUNDED_CURVE ( )  B_SPLINE_CURVE ( 3, ( #71225, #16061, #27683, #104536 ),
 .UNSPECIFIED., .F., .F. ) 
 B_SPLINE_CURVE_WITH_KNOTS ( ( 4, 4 ),
 ( 1.964434688349488090, 3.503810798801450854 ),
 .UNSPECIFIED. ) 
 CURVE ( )  GEOMETRIC_REPRESENTATION_ITEM ( )  RATIONAL_B_SPLINE_CURVE ( ( 1.000000000000000000, 0.8120851936182283959, 0.8120851936182283959, 1.000000000000000000 ) ) 
 REPRESENTATION_ITEM ( '' )  );
#47528 = DIRECTION ( 'NONE',  ( 0.000000000000000000, 1.000000000000000000, 0.000000000000000000 ) ) ;
#47529 = CARTESIAN_POINT ( 'NONE',  ( 39.48921356237310221, -27.52281430457082934, 5.000000000000000000 ) ) ;
#47530 = CARTESIAN_POINT ( 'NONE',  ( -25.49999999999981526, -14.94781430457066840, 5.000000000000000000 ) ) ;
#47531 = CARTESIAN_POINT ( 'NONE',  ( -16.49999999999989342, 9.431123077392092213, 4.000000000000000000 ) ) ;
#47533 = ORIENTED_EDGE ( 'NONE', *, *, #40111, .F. ) ;
#47532 = LINE ( 'NONE', #59117, #107758 ) ;
#47534 = FACE_OUTER_BOUND ( 'NONE', #30858, .T. ) ;
#47535 = CARTESIAN_POINT ( 'NONE',  ( -12.69999999999998153, 0.000000000000000000, 0.000000000000000000 ) ) ;
#47536 = DIRECTION ( 'NONE',  ( -0.000000000000000000, -0.000000000000000000, -1.000000000000000000 ) ) ;
#47537 = CARTESIAN_POINT ( 'NONE',  ( -14.99451991528749595, 28.92564299267948513, 4.000000000000000000 ) ) ;
#47538 = EDGE_LOOP ( 'NONE', ( #76041, #112520, #112474, #124834 ) ) ;
#47539 = EDGE_CURVE ( 'NONE', #4808, #110593, #128899, .T. ) ;
#47540 = AXIS2_PLACEMENT_3D ( 'NONE', #46065, #12676, #54790 ) ;
#47541 = ORIENTED_EDGE ( 'NONE', *, *, #138657, .T. ) ;
#47542 = AXIS2_PLACEMENT_3D ( 'NONE', #40971, #107637, #43826 ) ;
#47543 = AXIS2_PLACEMENT_3D ( 'NONE', #77375, #65056, #99058 ) ;
#47544 = EDGE_LOOP ( 'NONE', ( #55857, #35764, #128636, #86016 ) ) ;
#47545 = AXIS2_PLACEMENT_3D ( 'NONE', #55605, #99798, #470 ) ;
#47546 = DIRECTION ( 'NONE',  ( 1.000000000000000000, 0.000000000000000000, 0.000000000000000000 ) ) ;
#47547 = DIRECTION ( 'NONE',  ( 0.000000000000000000, 0.000000000000000000, 1.000000000000000000 ) ) ;
#47548 = CARTESIAN_POINT ( 'NONE',  ( 9.707106781186471522, 20.25929247661551003, 5.000000000000000000 ) ) ;
#47549 = EDGE_CURVE ( 'NONE', #48100, #58745, #139088, .T. ) ;
#47550 = CARTESIAN_POINT ( 'NONE',  ( 73.28752705046288440, 0.000000000000000000, -7.949999999999998401 ) ) ;
#47551 = CARTESIAN_POINT ( 'NONE',  ( 60.48921356237309510, -27.52281430457097500, 5.000000000000000000 ) ) ;
#47552 = ORIENTED_EDGE ( 'NONE', *, *, #116396, .F. ) ;
#47553 = ORIENTED_EDGE ( 'NONE', *, *, #134919, .F. ) ;
#47554 = DIRECTION ( 'NONE',  ( -0.6830127018922180770, -0.6830127018922204085, -0.2588190451025213501 ) ) ;
#47555 = CARTESIAN_POINT ( 'NONE',  ( -16.67979525387082518, 0.3337821591035555757, -30.81818940114110461 ) ) ;
#47556 = ORIENTED_EDGE ( 'NONE', *, *, #4926, .F. ) ;
#47557 = EDGE_CURVE ( 'NONE', #18761, #118169, #105699, .T. ) ;
#47558 = EDGE_LOOP ( 'NONE', ( #114047, #39078, #105900, #81951 ) ) ;
#47559 = CARTESIAN_POINT ( 'NONE',  ( 21.18398860626899349, 28.73617430169802134, 5.000000000000000000 ) ) ;
#47560 = CARTESIAN_POINT ( 'NONE',  ( 54.18398860626899705, 28.73617430169825226, 5.000000000000000000 ) ) ;
#47561 = ORIENTED_EDGE ( 'NONE', *, *, #112562, .F. ) ;
#47562 = EDGE_CURVE ( 'NONE', #28313, #55124, #39793, .T. ) ;
#47563 = FACE_BOUND ( 'NONE', #98907, .T. ) ;
#47564 = PLANE ( 'NONE',  #82640 ) ;
#47565 = CARTESIAN_POINT ( 'NONE',  ( -8.816011393731004731, 28.73617430169781173, 5.000000000000000000 ) ) ;
#47566 = CARTESIAN_POINT ( 'NONE',  ( 38.28752705046288440, 0.000000000000000000, -7.949999999999998401 ) ) ;
#47567 = LINE ( 'NONE', #91725, #85127 ) ;
#47568 = CARTESIAN_POINT ( 'NONE',  ( 104.8685099229812465, 4.744999999999947704, 0.004999999997858587189 ) ) ;
#47569 = ORIENTED_EDGE ( 'NONE', *, *, #8145, .T. ) ;
#47570 = ORIENTED_EDGE ( 'NONE', *, *, #46008, .T. ) ;
#47571 = CARTESIAN_POINT ( 'NONE',  ( 102.7245968585647802, -1.637169565754160949, 6.109999999999997655 ) ) ;
#47572 = ORIENTED_EDGE ( 'NONE', *, *, #6380, .F. ) ;
#47573 = DIRECTION ( 'NONE',  ( 0.7071067811865486830, -0.7071067811865464625, -0.000000000000000000 ) ) ;
#47574 = FACE_OUTER_BOUND ( 'NONE', #93930, .T. ) ;
#47575 = CARTESIAN_POINT ( 'NONE',  ( 34.92499999999998295, 22.22500000000000142, 4.000000000000000000 ) ) ;
#47576 = CARTESIAN_POINT ( 'NONE',  ( -7.499999999999944933, 18.05218569542898877, 5.000000000000000000 ) ) ;
#47577 = ORIENTED_EDGE ( 'NONE', *, *, #137365, .T. ) ;
#47578 = FACE_OUTER_BOUND ( 'NONE', #119148, .T. ) ;
#47579 = EDGE_CURVE ( 'NONE', #114819, #140054, #7826, .T. ) ;
#47580 = DIRECTION ( 'NONE',  ( -0.7071067811865486830, 0.7071067811865464625, -0.000000000000000000 ) ) ;
#47581 = EDGE_CURVE ( 'NONE', #88391, #91761, #84018, .T. ) ;
#47583 = CARTESIAN_POINT ( 'NONE',  ( 0.000000000000000000, 0.000000000000000000, 0.000000000000000000 ) ) ;
#47582 = CARTESIAN_POINT ( 'NONE',  ( -20.99999999999984368, -22.06887692260758982, 4.000000000000000000 ) ) ;
#47584 = CARTESIAN_POINT ( 'NONE',  ( -14.99999999999989519, 19.93112307739198386, 4.000000000000000000 ) ) ;
#47585 = LINE ( 'NONE', #46142, #9689 ) ;
#47586 = ORIENTED_EDGE ( 'NONE', *, *, #55937, .F. ) ;
#47587 = CARTESIAN_POINT ( 'NONE',  ( 23.99999999999982947, -13.44781430457068261, 5.000000000000000000 ) ) ;
#47588 = DIRECTION ( 'NONE',  ( 0.6830127018922181881, 0.6830127018922202975, -0.2588190451025214056 ) ) ;
#47589 = EDGE_LOOP ( 'NONE', ( #70385, #126737, #73025, #31838, #4853 ) ) ;
#47590 = EDGE_CURVE ( 'NONE', #59910, #135742, #97101, .T. ) ;
#47591 = ORIENTED_EDGE ( 'NONE', *, *, #62674, .F. ) ;
#47592 = ADVANCED_FACE ( 'NONE', ( #41178 ), #52759, .F. ) ;
#47593 = ORIENTED_EDGE ( 'NONE', *, *, #52146, .F. ) ;
#47594 = CARTESIAN_POINT ( 'NONE',  ( 57.16709685856477563, -3.055000000000000160, -5.291415217122921177 ) ) ;
#47595 = ORIENTED_EDGE ( 'NONE', *, *, #128938, .T. ) ;
#47596 = AXIS2_PLACEMENT_3D ( 'NONE', #106273, #63561, #95428 ) ;
#47597 = CARTESIAN_POINT ( 'NONE',  ( 7.337472949537107603, 6.094999999999989981, -1.119633336120465690E-15 ) ) ;
#47598 = CARTESIAN_POINT ( 'NONE',  ( 0.000000000000000000, 21.72500000000000142, 4.500000000000000888 ) ) ;
#47599 = VERTEX_POINT ( 'NONE', #41919 ) ;
#47600 = VECTOR ( 'NONE', #11258, 1000.000000000000000 ) ;
#47601 = LINE ( 'NONE', #27214, #108112 ) ;
#47602 = VERTEX_POINT ( 'NONE', #86129 ) ;
#47603 = DIRECTION ( 'NONE',  ( 0.000000000000000000, -1.000000000000000000, 0.000000000000000000 ) ) ;
#47605 = ORIENTED_EDGE ( 'NONE', *, *, #58443, .T. ) ;
#47604 = LINE ( 'NONE', #91768, #40161 ) ;
#47606 = ORIENTED_EDGE ( 'NONE', *, *, #38469, .F. ) ;
#47607 = EDGE_CURVE ( 'NONE', #100760, #90138, #20128, .T. ) ;
#47608 = PLANE ( 'NONE',  #26024 ) ;
#47609 = CARTESIAN_POINT ( 'NONE',  ( -14.99999999999989519, -8.731860332648849976, -2.120594902707574558 ) ) ;
#47610 = PLANE ( 'NONE',  #96109 ) ;
#47611 = ORIENTED_EDGE ( 'NONE', *, *, #81642, .T. ) ;
#47612 = DIRECTION ( 'NONE',  ( -1.000000000000000000, -0.000000000000000000, -0.000000000000000000 ) ) ;
#47613 = AXIS2_PLACEMENT_3D ( 'NONE', #133228, #44820, #99857 ) ;
#47614 = ORIENTED_EDGE ( 'NONE', *, *, #74973, .F. ) ;
#47615 = ORIENTED_EDGE ( 'NONE', *, *, #65779, .T. ) ;
#47616 = ORIENTED_EDGE ( 'NONE', *, *, #63618, .F. ) ;
#47617 = LINE ( 'NONE', #37416, #109591 ) ;
#47618 = DIRECTION ( 'NONE',  ( -0.7071067811865486830, 0.7071067811865464625, 0.000000000000000000 ) ) ;
#47619 = FACE_OUTER_BOUND ( 'NONE', #3370, .T. ) ;
#47620 = CARTESIAN_POINT ( 'NONE',  ( -60.48921356237309510, -27.52281430457097500, 5.000000000000000000 ) ) ;
#47621 = DIRECTION ( 'NONE',  ( -0.7071067811865487940, 0.7071067811865463515, 0.000000000000000000 ) ) ;
#47622 = ORIENTED_EDGE ( 'NONE', *, *, #65379, .F. ) ;
#47623 = CIRCLE ( 'NONE', #52137, 2.999999999999996003 ) ;
#47624 = CARTESIAN_POINT ( 'NONE',  ( 26.81206980810188512, 7.934999999999993392, 2.126176841940951689 ) ) ;
#47625 = CARTESIAN_POINT ( 'NONE',  ( -5.999999999999951150, -1.447814304570816946, 5.000000000000000000 ) ) ;
#47627 = ADVANCED_FACE ( 'NONE', ( #112176 ), #89000, .F. ) ;
#47626 = VECTOR ( 'NONE', #67097, 1000.000000000000000 ) ;
#47628 = DIRECTION ( 'NONE',  ( -0.3543493200069162685, -0.000000000000000000, -0.9351131265310288487 ) ) ;
#47629 = VECTOR ( 'NONE', #34729, 1000.000000000000000 ) ;
#47630 = LINE ( 'NONE', #125879, #4957 ) ;
#47631 = EDGE_LOOP ( 'NONE', ( #120194, #60421, #24841, #54499 ) ) ;
#47632 = EDGE_CURVE ( 'NONE', #23928, #927, #1916, .T. ) ;
#47633 = ORIENTED_EDGE ( 'NONE', *, *, #109080, .T. ) ;
#47634 = ORIENTED_EDGE ( 'NONE', *, *, #36629, .T. ) ;
#47635 = CARTESIAN_POINT ( 'NONE',  ( 14.28242261357422294, -21.73023691814493219, 5.000000000000000888 ) ) ;
#47636 = FACE_OUTER_BOUND ( 'NONE', #45602, .T. ) ;
#47637 = UNCERTAINTY_MEASURE_WITH_UNIT (LENGTH_MEASURE( 1.000000000000000082E-05 ), #86232, 'distance_accuracy_value', 'NONE');
#47638 = DIRECTION ( 'NONE',  ( -0.6830127018922180770, -0.6830127018922204085, -0.2588190451025213501 ) ) ;
#47639 = AXIS2_PLACEMENT_3D ( 'NONE', #98947, #75801, #142486 ) ;
#47640 = LINE ( 'NONE', #101972, #72879 ) ;
#47641 = PLANE ( 'NONE',  #101430 ) ;
#47642 = EDGE_CURVE ( 'NONE', #3113, #111037, #56400, .T. ) ;
#47644 = EDGE_CURVE ( 'NONE', #98880, #140231, #12115, .T. ) ;
#47643 = CARTESIAN_POINT ( 'NONE',  ( -17.67183060077634948, 17.25929247661553845, 4.000000000000000000 ) ) ;
#47645 = DIRECTION ( 'NONE',  ( 0.5735764363510453823, -0.8191520442889923537, 1.003171929053525486E-16 ) ) ;
#47646 = CARTESIAN_POINT ( 'NONE',  ( -72.29974487139158157, -27.71228299555256669, 4.000000000000000000 ) ) ;
#47647 = CARTESIAN_POINT ( 'NONE',  ( -21.18398860626899349, 28.73617430169802134, 5.000000000000000000 ) ) ;
#47648 = LINE ( 'NONE', #80259, #120643 ) ;
#47649 = DIRECTION ( 'NONE',  ( -1.000000000000000000, -1.224606353822377258E-16, -0.000000000000000000 ) ) ;
#47650 = ORIENTED_EDGE ( 'NONE', *, *, #31902, .T. ) ;
#47651 = CARTESIAN_POINT ( 'NONE',  ( 19.28515664589288292, 1.196650378695334416, -30.59010235425024149 ) ) ;
#47652 = VERTEX_POINT ( 'NONE', #54937 ) ;
#47653 = CARTESIAN_POINT ( 'NONE',  ( -39.48921356237310221, -27.52281430457082934, 5.000000000000000000 ) ) ;
#47655 = ORIENTED_EDGE ( 'NONE', *, *, #235, .T. ) ;
#47654 = CARTESIAN_POINT ( 'NONE',  ( 3.710381658649933634, -9.629649721936179265E-32, 2.500000000000000444 ) ) ;
#47656 = ADVANCED_FACE ( 'NONE', ( #66524 ), #143351, .F. ) ;
#47657 = ADVANCED_FACE ( 'NONE', ( #9980 ), #44057, .F. ) ;
#47658 = DIRECTION ( 'NONE',  ( 0.7071067811865486830, -0.7071067811865464625, -0.000000000000000000 ) ) ;
#47659 = LINE ( 'NONE', #80968, #5565 ) ;
#47660 = VERTEX_POINT ( 'NONE', #11372 ) ;
#47661 = DIRECTION ( 'NONE',  ( -0.7071067811865486830, -0.7071067811865464625, 0.000000000000000000 ) ) ;
#47662 = VERTEX_POINT ( 'NONE', #98428 ) ;
#47663 =( LENGTH_UNIT ( ) NAMED_UNIT ( * ) SI_UNIT ( .MILLI., .METRE. ) );
#47664 = UNCERTAINTY_MEASURE_WITH_UNIT (LENGTH_MEASURE( 1.000000000000000082E-05 ), #127656, 'distance_accuracy_value', 'NONE');
#47665 = EDGE_LOOP ( 'NONE', ( #122681, #41223, #106086, #35778 ) ) ;
#47666 = LINE ( 'NONE', #91826, #133279 ) ;
#47667 = EDGE_CURVE ( 'NONE', #122541, #79346, #10668, .T. ) ;
#47668 = CARTESIAN_POINT ( 'NONE',  ( 104.6416937171295558, -2.130196079827424871, -7.949999999999999289 ) ) ;
#47669 = LINE ( 'NONE', #126589, #81016 ) ;
#47670 = CARTESIAN_POINT ( 'NONE',  ( -33.18398860626899705, 28.73617430169810305, 5.000000000000000000 ) ) ;
#47671 = ORIENTED_EDGE ( 'NONE', *, *, #92785, .T. ) ;
#47672 = DIRECTION ( 'NONE',  ( -0.000000000000000000, -0.3543493200069152138, 0.9351131265310292928 ) ) ;
#47673 = DIRECTION ( 'NONE',  ( -0.7071067811865486830, 0.7071067811865464625, 0.000000000000000000 ) ) ;
#47674 = DIRECTION ( 'NONE',  ( 0.6830127018922180770, -0.6830127018922204085, -0.2588190451025213501 ) ) ;
#47675 = CARTESIAN_POINT ( 'NONE',  ( 20.70833333333333570, 3.047499999999997655, 5.278424836066143655 ) ) ;
#47676 = CARTESIAN_POINT ( 'NONE',  ( 24.91623647476855652, -7.934999999999990727, 4.858786175617117713E-16 ) ) ;
#47677 = ADVANCED_FACE ( 'NONE', ( #65110 ), #32468, .F. ) ;
#47678 = CARTESIAN_POINT ( 'NONE',  ( 9.299744871391588674, -27.71228299555212971, 4.000000000000000000 ) ) ;
#47679 = LINE ( 'NONE', #57114, #101083 ) ;
#47680 = ORIENTED_EDGE ( 'NONE', *, *, #69709, .F. ) ;
#47681 = CARTESIAN_POINT ( 'NONE',  ( 20.81601139373100295, 28.73617430169773002, 5.000000000000000000 ) ) ;
#47682 = ORIENTED_EDGE ( 'NONE', *, *, #116005, .T. ) ;
#47683 = CARTESIAN_POINT ( 'NONE',  ( 94.06293019189809002, 1.637169565754157174, 6.110000000000002984 ) ) ;
#47684 = DIRECTION ( 'NONE',  ( 0.6830127018922181881, 0.6830127018922202975, -0.2588190451025214056 ) ) ;
#47685 = DIRECTION ( 'NONE',  ( 0.7071067811865487940, -0.7071067811865463515, 0.000000000000000000 ) ) ;
#47686 = EDGE_CURVE ( 'NONE', #21546, #129906, #78116, .T. ) ;
#47687 = DIRECTION ( 'NONE',  ( -1.000000000000000000, -1.224606353822377258E-16, -0.000000000000000000 ) ) ;
#47688 = CARTESIAN_POINT ( 'NONE',  ( 124.7734390271410518, -44.54322672567605679, -35.04755940937983638 ) ) ;
#47689 = ORIENTED_EDGE ( 'NONE', *, *, #66863, .T. ) ;
#47690 = CARTESIAN_POINT ( 'NONE',  ( -17.99999999999987210, -21.84840872380826227, 2.849755605029565597 ) ) ;
#47691 = LINE ( 'NONE', #100613, #21061 ) ;
#47692 = VERTEX_POINT ( 'NONE', #120876 ) ;
#47693 = PLANE ( 'NONE',  #6869 ) ;
#47694 = DIRECTION ( 'NONE',  ( 0.7071067811865487940, 0.7071067811865463515, 0.000000000000000000 ) ) ;
#47697 = EDGE_CURVE ( 'NONE', #73610, #9196, #21586, .T. ) ;
#47696 = ORIENTED_EDGE ( 'NONE', *, *, #121359, .F. ) ;
#47695 = CARTESIAN_POINT ( 'NONE',  ( -9.183988606268997046, 28.73617430169793607, 5.000000000000000000 ) ) ;
#47699 = EDGE_CURVE ( 'NONE', #109689, #94631, #111434, .T. ) ;
#47698 = DIRECTION ( 'NONE',  ( -0.3543493200069162685, -0.000000000000000000, -0.9351131265310288487 ) ) ;
#47700 = DIRECTION ( 'NONE',  ( 0.3543493200069162685, -0.000000000000000000, -0.9351131265310288487 ) ) ;
#47701 =( BOUNDED_CURVE ( )  B_SPLINE_CURVE ( 3, ( #52974, #20343, #75475, #74777 ),
 .UNSPECIFIED., .F., .T. ) 
 B_SPLINE_CURVE_WITH_KNOTS ( ( 4, 4 ),
 ( 3.141592653589795336, 4.712388980384686121 ),
 .UNSPECIFIED. ) 
 CURVE ( )  GEOMETRIC_REPRESENTATION_ITEM ( )  RATIONAL_B_SPLINE_CURVE ( ( 1.000000000000000000, 0.8047378541243663808, 0.8047378541243663808, 1.000000000000000000 ) ) 
 REPRESENTATION_ITEM ( '' )  );
#47702 = DIRECTION ( 'NONE',  ( -0.7071067811865486830, -0.7071067811865464625, -0.000000000000000000 ) ) ;
#47703 = VERTEX_POINT ( 'NONE', #137493 ) ;
#47704 = ADVANCED_FACE ( 'NONE', ( #70133 ), #141108, .T. ) ;
#47705 = AXIS2_PLACEMENT_3D ( 'NONE', #17791, #14947, #36704 ) ;
#47706 = ORIENTED_EDGE ( 'NONE', *, *, #119601, .T. ) ;
#47707 = ORIENTED_EDGE ( 'NONE', *, *, #128639, .T. ) ;
#47708 = CARTESIAN_POINT ( 'NONE',  ( 83.41709685856477563, 3.054999999999998828, 5.291415217122922066 ) ) ;
#47709 = EDGE_LOOP ( 'NONE', ( #17248, #81773, #129140, #38124 ) ) ;
#47710 = VECTOR ( 'NONE', #132940, 1000.000000000000000 ) ;
#47711 = DIRECTION ( 'NONE',  ( 1.000000000000000000, -0.000000000000000000, -0.000000000000000000 ) ) ;
#47712 = DIRECTION ( 'NONE',  ( 0.7071067811865487940, 0.7071067811865463515, -0.000000000000000000 ) ) ;
#47713 = PLANE ( 'NONE',  #140603 ) ;
#47714 = FACE_OUTER_BOUND ( 'NONE', #141144, .T. ) ;
#47715 = ORIENTED_EDGE ( 'NONE', *, *, #7625, .F. ) ;
#47716 = CARTESIAN_POINT ( 'NONE',  ( 104.2500000000000000, -9.735942053221458872E-16, 7.950000000000000178 ) ) ;
#47717 = DIRECTION ( 'NONE',  ( -1.000000000000000000, -1.224606353822377258E-16, -0.000000000000000000 ) ) ;
#47718 = LINE ( 'NONE', #23787, #2402 ) ;
#47719 = CARTESIAN_POINT ( 'NONE',  ( 74.72459685856476597, -1.637169565754160949, 6.109999999999997655 ) ) ;
#47720 = ORIENTED_EDGE ( 'NONE', *, *, #94022, .T. ) ;
#47721 = VECTOR ( 'NONE', #14081, 1000.000000000000000 ) ;
#47722 = CARTESIAN_POINT ( 'NONE',  ( -30.18398860626900060, 28.73617430169808173, 5.000000000000000000 ) ) ;
#47723 = DIRECTION ( 'NONE',  ( -0.000000000000000000, 0.3543493200069153248, 0.9351131265310292928 ) ) ;
#47724 = DIRECTION ( 'NONE',  ( 0.7071067811865487940, 0.7071067811865463515, -0.000000000000000000 ) ) ;
#47725 = ORIENTED_EDGE ( 'NONE', *, *, #15532, .F. ) ;
#47726 = VERTEX_POINT ( 'NONE', #27273 ) ;
#47727 = DIRECTION ( 'NONE',  ( 0.3543493200069162685, -0.000000000000000000, -0.9351131265310288487 ) ) ;
#47728 = DIRECTION ( 'NONE',  ( -1.000000000000000000, -1.224606353822377258E-16, -0.000000000000000000 ) ) ;
#47729 = PLANE ( 'NONE',  #69730 ) ;
#47730 = CIRCLE ( 'NONE', #1301, 1.500000000000000000 ) ;
#47731 = LINE ( 'NONE', #1302, #41796 ) ;
#47732 = CARTESIAN_POINT ( 'NONE',  ( 51.48921356237309510, -27.52281430457091460, 5.000000000000000000 ) ) ;
#47733 = FILL_AREA_STYLE ('',( #23803 ) ) ;
#47734 = VECTOR ( 'NONE', #50339, 1000.000000000000000 ) ;
#47735 = ORIENTED_EDGE ( 'NONE', *, *, #141042, .F. ) ;
#47736 = ORIENTED_EDGE ( 'NONE', *, *, #87063, .F. ) ;
#47737 = VECTOR ( 'NONE', #131269, 999.9999999999998863 ) ;
#47738 = LINE ( 'NONE', #91903, #117398 ) ;
#47739 = EDGE_CURVE ( 'NONE', #34380, #63020, #48332, .T. ) ;
#47740 = ORIENTED_EDGE ( 'NONE', *, *, #41251, .F. ) ;
#47741 = VECTOR ( 'NONE', #44635, 999.9999999999998863 ) ;
#47742 = DIRECTION ( 'NONE',  ( 0.6830127018922180770, -0.6830127018922204085, -0.2588190451025213501 ) ) ;
#47743 = ORIENTED_EDGE ( 'NONE', *, *, #102451, .F. ) ;
#47744 = DIRECTION ( 'NONE',  ( 0.7071067811865487940, 0.7071067811865463515, 0.000000000000000000 ) ) ;
#47745 = FACE_OUTER_BOUND ( 'NONE', #43673, .T. ) ;
#47746 = LINE ( 'NONE', #70910, #46147 ) ;
#47747 = DIRECTION ( 'NONE',  ( -0.6830127018922181881, 0.6830127018922202975, -0.2588190451025214056 ) ) ;
#47748 = VERTEX_POINT ( 'NONE', #106794 ) ;
#47749 = LINE ( 'NONE', #76247, #130465 ) ;
#47750 = DIRECTION ( 'NONE',  ( 0.000000000000000000, 1.000000000000000000, 0.000000000000000000 ) ) ;
#47751 = ORIENTED_EDGE ( 'NONE', *, *, #101327, .F. ) ;
#47752 = EDGE_CURVE ( 'NONE', #61225, #82235, #58553, .T. ) ;
#47753 = CARTESIAN_POINT ( 'NONE',  ( -7.828169399223476432, 9.759292476615614831, 4.000000000000000000 ) ) ;
#47754 = ORIENTED_EDGE ( 'NONE', *, *, #11254, .F. ) ;
#47755 = ORIENTED_EDGE ( 'NONE', *, *, #7281, .T. ) ;
#47757 = EDGE_CURVE ( 'NONE', #2221, #134621, #113571, .T. ) ;
#47756 = CARTESIAN_POINT ( 'NONE',  ( 0.3281693992235311108, -9.740707523384182664, 4.000000000000000000 ) ) ;
#47758 = VERTEX_POINT ( 'NONE', #125177 ) ;
#47759 = VERTEX_POINT ( 'NONE', #14268 ) ;
#47760 = DIRECTION ( 'NONE',  ( 0.6830127018922180770, -0.6830127018922204085, -0.2588190451025213501 ) ) ;
#47761 = ORIENTED_EDGE ( 'NONE', *, *, #54570, .F. ) ;
#47762 = LINE ( 'NONE', #93368, #109032 ) ;
#47763 = DIRECTION ( 'NONE',  ( 0.3543493200069162685, -0.000000000000000000, -0.9351131265310288487 ) ) ;
#47764 = CARTESIAN_POINT ( 'NONE',  ( 122.9379301918981042, -6.110000000000001208, 1.637169565754158951 ) ) ;
#47765 = CARTESIAN_POINT ( 'NONE',  ( 4.184256412735922304, 4.202752102959690472E-16, 0.000000000000000000 ) ) ;
#47766 = EDGE_CURVE ( 'NONE', #72201, #92747, #114294, .T. ) ;
#47767 = PLANE ( 'NONE',  #106054 ) ;
#47769 = DIRECTION ( 'NONE',  ( 0.6830127018922180770, -0.6830127018922204085, -0.2588190451025214056 ) ) ;
#47768 = DIRECTION ( 'NONE',  ( 0.000000000000000000, -0.000000000000000000, 1.000000000000000000 ) ) ;
#47770 = CARTESIAN_POINT ( 'NONE',  ( 5.281315875828549444, 4.584330080086930965E-16, 0.000000000000000000 ) ) ;
#47771 = VECTOR ( 'NONE', #120737, 1000.000000000000000 ) ;
#47772 = DIRECTION ( 'NONE',  ( 1.000000000000000000, 0.000000000000000000, 0.000000000000000000 ) ) ;
#47773 = EDGE_CURVE ( 'NONE', #106451, #141686, #122590, .T. ) ;
#47774 = CARTESIAN_POINT ( 'NONE',  ( 3.792893218813436551, -17.24070752338410628, 5.000000000000000000 ) ) ;
#47775 = ORIENTED_EDGE ( 'NONE', *, *, #116149, .F. ) ;
#47776 = PLANE ( 'NONE',  #94335 ) ;
#47777 = DIRECTION ( 'NONE',  ( -0.7071067811865486830, -0.7071067811865464625, -0.000000000000000000 ) ) ;
#47778 = ORIENTED_EDGE ( 'NONE', *, *, #10541, .T. ) ;
#47779 = ORIENTED_EDGE ( 'NONE', *, *, #10089, .T. ) ;
#47780 = AXIS2_PLACEMENT_3D ( 'NONE', #336, #109116, #64205 ) ;
#47781 = PLANE ( 'NONE',  #118882 ) ;
#47782 = EDGE_CURVE ( 'NONE', #51950, #102894, #3367, .T. ) ;
#47783 = ORIENTED_EDGE ( 'NONE', *, *, #78402, .T. ) ;
#47784 = CARTESIAN_POINT ( 'NONE',  ( 26.99999999999981526, -18.03360074219755660, 5.000000000000000000 ) ) ;
#47785 = CARTESIAN_POINT ( 'NONE',  ( -34.92499999999997584, -22.26999999999999247, -37.00000000000000000 ) ) ;
#47786 = DIRECTION ( 'NONE',  ( 1.000000000000000000, 1.224606353822377258E-16, 0.000000000000000000 ) ) ;
#47787 = CARTESIAN_POINT ( 'NONE',  ( 21.15294044719737698, 2.499999999999998224, 3.061616997868380183E-16 ) ) ;
#47788 = ORIENTED_EDGE ( 'NONE', *, *, #4380, .F. ) ;
#47789 = DIRECTION ( 'NONE',  ( 0.7071067811865487940, 0.7071067811865463515, 0.000000000000000000 ) ) ;
#47790 = ORIENTED_EDGE ( 'NONE', *, *, #7824, .F. ) ;
#47791 = CARTESIAN_POINT ( 'NONE',  ( 17.67183060077634948, -15.74070752338412049, 4.000000000000000000 ) ) ;
#47792 = VECTOR ( 'NONE', #93882, 1000.000000000000000 ) ;
#47793 = CARTESIAN_POINT ( 'NONE',  ( 27.04623647476855197, -7.934999999999990727, 4.858786175617117713E-16 ) ) ;
#47794 = CARTESIAN_POINT ( 'NONE',  ( 184.1500000000000057, -14.29000000000013593, 12.69999999999954632 ) ) ;
#47795 = VECTOR ( 'NONE', #138989, 1000.000000000000000 ) ;
#47796 = CARTESIAN_POINT ( 'NONE',  ( 98.95419371712955581, 6.884901960086283523, 3.975000000000002753 ) ) ;
#47797 = ORIENTED_EDGE ( 'NONE', *, *, #121366, .F. ) ;
#47798 = EDGE_CURVE ( 'NONE', #78244, #91252, #91822, .T. ) ;
#47799 = ORIENTED_EDGE ( 'NONE', *, *, #65974, .F. ) ;
#47800 = ORIENTED_EDGE ( 'NONE', *, *, #8204, .T. ) ;
#47801 = DIRECTION ( 'NONE',  ( -1.000000000000000000, 0.000000000000000000, 0.000000000000000000 ) ) ;
#47802 = CARTESIAN_POINT ( 'NONE',  ( 0.000000000000000000, 0.000000000000000000, 0.000000000000000000 ) ) ;
#47803 = LINE ( 'NONE', #134808, #75159 ) ;
#47804 = DIRECTION ( 'NONE',  ( -0.6830127018922181881, 0.6830127018922202975, -0.2588190451025214056 ) ) ;
#47805 = VERTEX_POINT ( 'NONE', #92524 ) ;
#47806 = DIRECTION ( 'NONE',  ( -0.000000000000000000, 0.3543493200069153248, 0.9351131265310292928 ) ) ;
#47807 = EDGE_CURVE ( 'NONE', #15280, #66770, #136047, .T. ) ;
#47808 = EDGE_CURVE ( 'NONE', #131497, #91250, #60684, .T. ) ;
#47809 = PLANE ( 'NONE',  #45785 ) ;
#47810 = AXIS2_PLACEMENT_3D ( 'NONE', #99760, #30966, #132441 ) ;
#47811 = DIRECTION ( 'NONE',  ( -1.000000000000000000, 0.000000000000000000, 0.000000000000000000 ) ) ;
#47812 = PLANE ( 'NONE',  #93154 ) ;
#47813 = ORIENTED_EDGE ( 'NONE', *, *, #96770, .F. ) ;
#47815 = EDGE_CURVE ( 'NONE', #48369, #45681, #136754, .T. ) ;
#47814 = CARTESIAN_POINT ( 'NONE',  ( 1.199999999999999956, 0.5999999999999987566, -4.543283425070392845 ) ) ;
#47816 = EDGE_LOOP ( 'NONE', ( #49832, #78161, #77879, #3957 ) ) ;
#47818 = ORIENTED_EDGE ( 'NONE', *, *, #20794, .T. ) ;
#47817 = CARTESIAN_POINT ( 'NONE',  ( 60.07317433568100995, -45.23984008851914496, -35.04755940938199643 ) ) ;
#47819 = VECTOR ( 'NONE', #31097, 1000.000000000000000 ) ;
#47821 = ORIENTED_EDGE ( 'NONE', *, *, #74982, .F. ) ;
#47820 = ADVANCED_FACE ( 'NONE', ( #37471 ), #36730, .F. ) ;
#47822 = ADVANCED_FACE ( 'NONE', ( #112860 ), #13529, .T. ) ;
#47823 = DIRECTION ( 'NONE',  ( 0.7071067811865487940, -0.7071067811865463515, 0.000000000000000000 ) ) ;
#47824 = DIRECTION ( 'NONE',  ( 0.7071067811865487940, 0.7071067811865463515, 0.000000000000000000 ) ) ;
#47825 = ORIENTED_EDGE ( 'NONE', *, *, #108097, .T. ) ;
#47826 = DIRECTION ( 'NONE',  ( -0.000000000000000000, -0.000000000000000000, -1.000000000000000000 ) ) ;
#47827 = UNCERTAINTY_MEASURE_WITH_UNIT (LENGTH_MEASURE( 1.000000000000000082E-05 ), #12277, 'distance_accuracy_value', 'NONE');
#47828 = VERTEX_POINT ( 'NONE', #81706 ) ;
#47829 = AXIS2_PLACEMENT_3D ( 'NONE', #48929, #49659, #72136 ) ;
#47830 = VECTOR ( 'NONE', #42354, 999.9999999999998863 ) ;
#47831 = DIRECTION ( 'NONE',  ( 0.5735764363510444941, 0.8191520442889929088, 0.000000000000000000 ) ) ;
#47832 = CARTESIAN_POINT ( 'NONE',  ( 10.49999999999992184, 8.900465351122159419, -2.516491619111538292 ) ) ;
#47834 = CARTESIAN_POINT ( 'NONE',  ( 31.55793019189810522, 6.110000000000001208, -1.637169565754156286 ) ) ;
#47833 = VECTOR ( 'NONE', #47886, 999.9999999999998863 ) ;
#47835 = DIRECTION ( 'NONE',  ( -2.781805975412905890E-17, 0.3543493200069152693, 0.9351131265310292928 ) ) ;
#47836 = ADVANCED_FACE ( 'NONE', ( #57809 ), #38185, .F. ) ;
#47837 = CARTESIAN_POINT ( 'NONE',  ( 11.81601139373100651, 28.73617430169779041, 5.000000000000000000 ) ) ;
#47838 = DIRECTION ( 'NONE',  ( -0.7071067811865486830, -0.7071067811865464625, 0.000000000000000000 ) ) ;
#47839 = DIRECTION ( 'NONE',  ( 0.7071067811865486830, -0.7071067811865464625, -0.000000000000000000 ) ) ;
#47840 = CARTESIAN_POINT ( 'NONE',  ( 54.48921356237310221, -27.52281430457093236, 5.000000000000000000 ) ) ;
#47841 = DIRECTION ( 'NONE',  ( 0.6830127018922181881, 0.6830127018922202975, -0.2588190451025214056 ) ) ;
#47842 = CARTESIAN_POINT ( 'NONE',  ( 30.60373647476856007, 5.808823158059036373, 5.808823158059032821 ) ) ;
#47843 = CARTESIAN_POINT ( 'NONE',  ( 0.000000000000000000, -22.26999999999999247, -0.5000000000000004441 ) ) ;
#47844 = DIRECTION ( 'NONE',  ( -0.000000000000000000, -0.3543493200069152693, 0.9351131265310292928 ) ) ;
#47845 = CONICAL_SURFACE ( 'NONE', #124273, 2.055000000000000604, 0.9599310885968764806 ) ;
#47846 = ADVANCED_FACE ( 'NONE', ( #80271 ), #15650, .F. ) ;
#47847 = FACE_OUTER_BOUND ( 'NONE', #127529, .T. ) ;
#47848 = LINE ( 'NONE', #4960, #114827 ) ;
#47849 = EDGE_LOOP ( 'NONE', ( #6182, #138321, #26417, #123037 ) ) ;
#47850 = ORIENTED_EDGE ( 'NONE', *, *, #20646, .F. ) ;
#47851 = CARTESIAN_POINT ( 'NONE',  ( 89.66666666666667140, 6.884901960086285300, 3.975000000000003642 ) ) ;
#47852 = EDGE_LOOP ( 'NONE', ( #44046, #119937, #127545, #30968 ) ) ;
#47853 = ORIENTED_EDGE ( 'NONE', *, *, #3567, .T. ) ;
#47854 = SURFACE_SIDE_STYLE ('',( #137695 ) ) ;
#47855 = CARTESIAN_POINT ( 'NONE',  ( 22.50413961620377634, -3.047499999999994547, 5.278424836066145431 ) ) ;
#47856 = CARTESIAN_POINT ( 'NONE',  ( 14.66377360979165267, 9.483362590305993933, -0.5803357009920233622 ) ) ;
#47857 = VERTEX_POINT ( 'NONE', #93259 ) ;
#47858 = DIRECTION ( 'NONE',  ( 0.000000000000000000, 0.000000000000000000, 1.000000000000000000 ) ) ;
#47859 = PLANE ( 'NONE',  #69585 ) ;
#47860 = DIRECTION ( 'NONE',  ( 0.7071067811865487940, -0.7071067811865463515, 0.000000000000000000 ) ) ;
#47861 = CARTESIAN_POINT ( 'NONE',  ( 126.4318778290302276, 7.022613924927493478, 0.02362404962084689586 ) ) ;
#47862 = DIRECTION ( 'NONE',  ( 0.7071067811865487940, 0.7071067811865463515, 0.000000000000000000 ) ) ;
#47863 = DIRECTION ( 'NONE',  ( -1.000000000000000000, -1.224606353822377258E-16, -0.000000000000000000 ) ) ;
#47864 = EDGE_CURVE ( 'NONE', #51050, #86215, #82401, .T. ) ;
#47865 = DIRECTION ( 'NONE',  ( 0.7071067811865486830, -0.7071067811865464625, -0.000000000000000000 ) ) ;
#47866 = DIRECTION ( 'NONE',  ( -0.7071067811865486830, 0.7071067811865464625, 0.000000000000000000 ) ) ;
#47867 = CARTESIAN_POINT ( 'NONE',  ( 11.99999999999992006, -10.44781430457072346, 5.000000000000000000 ) ) ;
#47868 = CARTESIAN_POINT ( 'NONE',  ( 55.47138350052870948, -49.14501756083438266, 40.36361034346623455 ) ) ;
#47869 = ADVANCED_FACE ( 'NONE', ( #75624 ), #64736, .F. ) ;
#47870 = EDGE_CURVE ( 'NONE', #39265, #126191, #131430, .T. ) ;
#47871 = ORIENTED_EDGE ( 'NONE', *, *, #47632, .F. ) ;
#47872 = EDGE_LOOP ( 'NONE', ( #32994, #139745, #111772, #113215 ) ) ;
#47873 = CARTESIAN_POINT ( 'NONE',  ( 110.2504301918981042, 3.055000000000002824, -5.291415217122919401 ) ) ;
#47874 = ORIENTED_EDGE ( 'NONE', *, *, #33839, .F. ) ;
#47875 = DIRECTION ( 'NONE',  ( -0.7071067811865487940, 0.7071067811865463515, -0.000000000000000000 ) ) ;
#47876 = VECTOR ( 'NONE', #71936, 1000.000000000000000 ) ;
#47877 = ORIENTED_EDGE ( 'NONE', *, *, #69073, .T. ) ;
#47878 = EDGE_CURVE ( 'NONE', #7505, #28061, #42298, .T. ) ;
#47879 = DIRECTION ( 'NONE',  ( -0.000000000000000000, 0.000000000000000000, 1.000000000000000000 ) ) ;
#47880 = CARTESIAN_POINT ( 'NONE',  ( 0.000000000000000000, 0.000000000000000000, 0.000000000000000000 ) ) ;
#47881 = CARTESIAN_POINT ( 'NONE',  ( 105.9329301918981088, 1.637169565754156508, 6.110000000000000320 ) ) ;
#47882 = ORIENTED_EDGE ( 'NONE', *, *, #12340, .T. ) ;
#47883 = ORIENTED_EDGE ( 'NONE', *, *, #21627, .F. ) ;
#47884 = DIRECTION ( 'NONE',  ( -0.7071067811865486830, 0.7071067811865464625, 0.000000000000000000 ) ) ;
#47885 = VECTOR ( 'NONE', #114802, 1000.000000000000000 ) ;
#47886 = DIRECTION ( 'NONE',  ( -0.7071067811865487940, 0.7071067811865463515, -0.000000000000000000 ) ) ;
#47887 = EDGE_LOOP ( 'NONE', ( #142937, #128212, #84520, #118121, #68896, #70012 ) ) ;
#47888 = VERTEX_POINT ( 'NONE', #76334 ) ;
#47889 = VECTOR ( 'NONE', #137927, 1000.000000000000000 ) ;
#47890 = ORIENTED_EDGE ( 'NONE', *, *, #102059, .T. ) ;
#47891 = LINE ( 'NONE', #136281, #88537 ) ;
#47892 = FILL_AREA_STYLE ('',( #69643 ) ) ;
#47893 = AXIS2_PLACEMENT_3D ( 'NONE', #254, #45960, #90144 ) ;
#47894 =( NAMED_UNIT ( * ) SI_UNIT ( $, .STERADIAN. ) SOLID_ANGLE_UNIT ( ) );
#47895 = CYLINDRICAL_SURFACE ( 'NONE', #17727, 2.999999999999999112 ) ;
#47896 = ORIENTED_EDGE ( 'NONE', *, *, #112306, .F. ) ;
#47897 = EDGE_LOOP ( 'NONE', ( #27854, #87508 ) ) ;
#47898 = CARTESIAN_POINT ( 'NONE',  ( -23.99999999999983302, -1.068876922607798985, 4.000000000000000000 ) ) ;
#47900 = EDGE_CURVE ( 'NONE', #771, #15594, #21228, .T. ) ;
#47899 = ORIENTED_EDGE ( 'NONE', *, *, #15024, .T. ) ;
#47901 = ORIENTED_EDGE ( 'NONE', *, *, #3377, .F. ) ;
#47902 = CARTESIAN_POINT ( 'NONE',  ( 30.48921356237309510, -27.52281430457076894, 5.000000000000000000 ) ) ;
#47903 = LINE ( 'NONE', #36290, #112389 ) ;
#47904 = CARTESIAN_POINT ( 'NONE',  ( -3.299744871391591339, -27.71228299555208352, 4.000000000000000000 ) ) ;
#47905 = ORIENTED_EDGE ( 'NONE', *, *, #142999, .T. ) ;
#47906 = CARTESIAN_POINT ( 'NONE',  ( -16.49999999999987566, -14.94781430457067906, 5.000000000000000000 ) ) ;
#47907 = CARTESIAN_POINT ( 'NONE',  ( 13.58990935480160189, 9.759292476615618384, 11.28811694763781937 ) ) ;
#47908 = CARTESIAN_POINT ( 'NONE',  ( 7.499999999999947597, 9.431123077392085108, 4.000000000000000000 ) ) ;
#47909 = PLANE ( 'NONE',  #39738 ) ;
#47910 = EDGE_CURVE ( 'NONE', #22767, #124122, #133626, .T. ) ;
#47912 = FACE_BOUND ( 'NONE', #40057, .T. ) ;
#47911 = VECTOR ( 'NONE', #75164, 1000.000000000000000 ) ;
#47913 = ORIENTED_EDGE ( 'NONE', *, *, #87721, .T. ) ;
#47914 = CARTESIAN_POINT ( 'NONE',  ( 12.48921356237309155, -27.52281430457064104, 5.000000000000000000 ) ) ;
#47915 = EDGE_CURVE ( 'NONE', #45336, #124524, #108923, .T. ) ;
#47916 = CARTESIAN_POINT ( 'NONE',  ( 0.5685132242927012358, -0.4000000000000004108, 2.467792535850613866 ) ) ;
#47917 = CARTESIAN_POINT ( 'NONE',  ( 12.70710678118646619, 11.25929247661560240, 5.000000000000000000 ) ) ;
#47918 = ORIENTED_EDGE ( 'NONE', *, *, #122635, .T. ) ;
#47919 = CARTESIAN_POINT ( 'NONE',  ( 3.792893218813431666, -20.24070752338406720, 5.000000000000000000 ) ) ;
#47920 = ORIENTED_EDGE ( 'NONE', *, *, #49890, .T. ) ;
#47921 = EDGE_LOOP ( 'NONE', ( #88869, #68972, #118736, #36362 ) ) ;
#47922 = VECTOR ( 'NONE', #50534, 999.9999999999998863 ) ;
#47923 = VERTEX_POINT ( 'NONE', #54592 ) ;
#47925 = EDGE_CURVE ( 'NONE', #32684, #63590, #129996, .T. ) ;
#47924 = VECTOR ( 'NONE', #97970, 1000.000000000000000 ) ;
#47926 = ADVANCED_FACE ( 'NONE', ( #98085 ), #87204, .F. ) ;
#47927 = CARTESIAN_POINT ( 'NONE',  ( 42.34959685856478018, 6.109999999999996767, 1.637169565754163836 ) ) ;
#47928 = ORIENTED_EDGE ( 'NONE', *, *, #96361, .F. ) ;
#47929 = FACE_OUTER_BOUND ( 'NONE', #12770, .T. ) ;
#47930 = CARTESIAN_POINT ( 'NONE',  ( 25.39999999999999858, -16.48000000000005016, -34.92499999999998295 ) ) ;
#47931 = CARTESIAN_POINT ( 'NONE',  ( 10.32500000000000107, -8.432637487761466488, -4.375000000000001776 ) ) ;
#47932 = ADVANCED_FACE ( 'NONE', ( #32109 ), #65487, .F. ) ;
#47933 = AXIS2_PLACEMENT_3D ( 'NONE', #65153, #42687, #76003 ) ;
#47934 = VERTEX_POINT ( 'NONE', #66182 ) ;
#47935 = CYLINDRICAL_SURFACE ( 'NONE', #130197, 2.999999999999999112 ) ;
#47936 = AXIS2_PLACEMENT_3D ( 'NONE', #31436, #138777, #42328 ) ;
#47937 = SURFACE_STYLE_USAGE ( .BOTH. , #77864 ) ;
#47938 = EDGE_CURVE ( 'NONE', #124700, #76836, #120499, .T. ) ;
#47939 = DIRECTION ( 'NONE',  ( -0.7071067811865486830, -0.7071067811865464625, -0.000000000000000000 ) ) ;
#47940 = DIRECTION ( 'NONE',  ( 0.5735764363510448272, -0.8191520442889927978, 1.003171929053526103E-16 ) ) ;
#47941 = CARTESIAN_POINT ( 'NONE',  ( -21.32816939922337340, -21.74070752338406720, 4.000000000000000000 ) ) ;
#47942 = EDGE_LOOP ( 'NONE', ( #111170, #65722, #82354, #123616 ) ) ;
#47943 = ORIENTED_EDGE ( 'NONE', *, *, #54761, .F. ) ;
#47944 = ORIENTED_EDGE ( 'NONE', *, *, #18086, .T. ) ;
#47945 = ORIENTED_EDGE ( 'NONE', *, *, #121644, .F. ) ;
#47946 = LINE ( 'NONE', #2965, #88759 ) ;
#47947 = EDGE_CURVE ( 'NONE', #115169, #79668, #109664, .T. ) ;
#47948 = ORIENTED_EDGE ( 'NONE', *, *, #115973, .T. ) ;
#47949 = ORIENTED_EDGE ( 'NONE', *, *, #111587, .F. ) ;
#47950 = DIRECTION ( 'NONE',  ( 0.000000000000000000, 1.000000000000000000, 0.000000000000000000 ) ) ;
#47951 = DIRECTION ( 'NONE',  ( -0.3543493200069162685, -0.000000000000000000, -0.9351131265310288487 ) ) ;
#47952 = EDGE_LOOP ( 'NONE', ( #102106, #118844, #50111, #117548 ) ) ;
#47953 = AXIS2_PLACEMENT_3D ( 'NONE', #70070, #15588, #4700 ) ;
#47954 = LINE ( 'NONE', #113157, #55717 ) ;
#47955 = ADVANCED_FACE ( 'NONE', ( #143009 ), #19087, .T. ) ;
#47956 = EDGE_LOOP ( 'NONE', ( #43861, #13118, #51294, #111569, #101127 ) ) ;
#47957 = CARTESIAN_POINT ( 'NONE',  ( 25.39999999999999858, -30.18000000000009564, -15.92500000000064375 ) ) ;
#47958 = AXIS2_PLACEMENT_3D ( 'NONE', #89566, #122178, #110581 ) ;
#47959 = CARTESIAN_POINT ( 'NONE',  ( 4.733736474768551972, 5.808823158059036373, 5.808823158059032821 ) ) ;
#47960 = ORIENTED_EDGE ( 'NONE', *, *, #134580, .F. ) ;
#47962 = FACE_OUTER_BOUND ( 'NONE', #71264, .T. ) ;
#47961 = CARTESIAN_POINT ( 'NONE',  ( 99.22459685856479439, -1.637169565754161171, 6.109999999999998543 ) ) ;
#47963 = DIRECTION ( 'NONE',  ( -0.000000000000000000, 0.000000000000000000, 1.000000000000000000 ) ) ;
#47964 = CARTESIAN_POINT ( 'NONE',  ( 42.48921356237308800, -27.52281430457085065, 5.000000000000000000 ) ) ;
#47965 = ORIENTED_EDGE ( 'NONE', *, *, #42449, .T. ) ;
#47966 = EDGE_CURVE ( 'NONE', #113044, #53162, #64030, .T. ) ;
#47967 = VERTEX_POINT ( 'NONE', #29947 ) ;
#47968 = FACE_OUTER_BOUND ( 'NONE', #50003, .T. ) ;
#47969 = ORIENTED_EDGE ( 'NONE', *, *, #17787, .T. ) ;
#47970 = AXIS2_PLACEMENT_3D ( 'NONE', #86734, #7707, #43230 ) ;
#47971 = CARTESIAN_POINT ( 'NONE',  ( -26.01844734635654888, 18.75929247661551713, 20.33588619593448854 ) ) ;
#47972 = CARTESIAN_POINT ( 'NONE',  ( 51.48921356237309510, -27.52281430457091460, 5.000000000000000000 ) ) ;
#47973 = FILL_AREA_STYLE_COLOUR ( '', #91172 ) ;
#47974 = ORIENTED_EDGE ( 'NONE', *, *, #31435, .T. ) ;
#47975 = EDGE_CURVE ( 'NONE', #878, #121504, #62503, .T. ) ;
#47976 = EDGE_CURVE ( 'NONE', #117979, #135052, #8178, .T. ) ;
#47977 = VECTOR ( 'NONE', #85762, 1000.000000000000227 ) ;
#47978 = ORIENTED_EDGE ( 'NONE', *, *, #71272, .T. ) ;
#47980 = ADVANCED_FACE ( 'NONE', ( #19791 ), #108198, .T. ) ;
#47979 = CARTESIAN_POINT ( 'NONE',  ( 18.83652871126538386, 15.75929247661555799, 9.299976744542963303 ) ) ;
#47981 = ORIENTED_EDGE ( 'NONE', *, *, #70464, .F. ) ;
#47983 = VERTEX_POINT ( 'NONE', #47330 ) ;
#47982 = DIRECTION ( 'NONE',  ( 0.000000000000000000, 1.000000000000000000, 0.000000000000000000 ) ) ;
#47984 = ORIENTED_EDGE ( 'NONE', *, *, #80069, .F. ) ;
#47985 = CARTESIAN_POINT ( 'NONE',  ( -18.91353603094692204, 2.162493570128502185, -30.33479532556184211 ) ) ;
#47986 = ORIENTED_EDGE ( 'NONE', *, *, #101670, .F. ) ;
#47987 = CARTESIAN_POINT ( 'NONE',  ( 112.1250000000000000, -7.950000000000000178, -4.867971026610729436E-16 ) ) ;
#47988 = DIRECTION ( 'NONE',  ( 0.7071067811865487940, 0.7071067811865463515, -0.000000000000000000 ) ) ;
#47989 = VECTOR ( 'NONE', #123511, 999.9999999999998863 ) ;
#47990 = VERTEX_POINT ( 'NONE', #78478 ) ;
#47991 = EDGE_CURVE ( 'NONE', #103562, #128813, #81026, .T. ) ;
#47992 = LINE ( 'NONE', #77935, #69344 ) ;
#47993 = LINE ( 'NONE', #56750, #88275 ) ;
#47994 = LINE ( 'NONE', #50828, #123063 ) ;
#47995 = LINE ( 'NONE', #80614, #26258 ) ;
#47996 = DIRECTION ( 'NONE',  ( 1.000000000000000000, 0.000000000000000000, 0.000000000000000000 ) ) ;
#47997 = PLANE ( 'NONE',  #20483 ) ;
#47998 = EDGE_CURVE ( 'NONE', #78032, #70129, #85645, .T. ) ;
#47999 = DIRECTION ( 'NONE',  ( 0.6830127018922181881, 0.6830127018922202975, -0.2588190451025214056 ) ) ;
#48000 = DIRECTION ( 'NONE',  ( -0.000000000000000000, -0.000000000000000000, 1.000000000000000000 ) ) ;
#48001 = ORIENTED_EDGE ( 'NONE', *, *, #30400, .F. ) ;
#48002 = ORIENTED_EDGE ( 'NONE', *, *, #105168, .T. ) ;
#48003 = ORIENTED_EDGE ( 'NONE', *, *, #40249, .F. ) ;
#48004 = CARTESIAN_POINT ( 'NONE',  ( 120.8750000000000000, 7.950000000000000178, 1.460391307983218535E-15 ) ) ;
#48005 = ORIENTED_EDGE ( 'NONE', *, *, #47938, .T. ) ;
#48006 = ORIENTED_EDGE ( 'NONE', *, *, #113497, .T. ) ;
#48007 = VERTEX_POINT ( 'NONE', #124827 ) ;
#48008 = FACE_OUTER_BOUND ( 'NONE', #50938, .T. ) ;
#48009 = CARTESIAN_POINT ( 'NONE',  ( -25.39999999999996305, 0.000000000000000000, 0.000000000000000000 ) ) ;
#48010 = ORIENTED_EDGE ( 'NONE', *, *, #102156, .T. ) ;
#48011 = CARTESIAN_POINT ( 'NONE',  ( -6.134995737516187653, 3.759292476615678336, 15.36553568819727644 ) ) ;
#48012 = DIRECTION ( 'NONE',  ( 0.000000000000000000, -1.000000000000000000, 0.000000000000000000 ) ) ;
#48013 = VECTOR ( 'NONE', #20919, 1000.000000000000227 ) ;
#48014 = DIRECTION ( 'NONE',  ( 0.7071067811865487940, 0.7071067811865463515, 0.000000000000000000 ) ) ;
#48015 = CARTESIAN_POINT ( 'NONE',  ( 114.1879301918980900, 6.110000000000002984, -1.637169565754156730 ) ) ;
#48016 = EDGE_LOOP ( 'NONE', ( #25262, #6444, #88765, #137886 ) ) ;
#48017 = DIRECTION ( 'NONE',  ( -1.000000000000000000, -1.224606353822377258E-16, -0.000000000000000000 ) ) ;
#48018 = CARTESIAN_POINT ( 'NONE',  ( 33.18398860626899705, 28.73617430169810305, 5.000000000000000000 ) ) ;
#48019 = CARTESIAN_POINT ( 'NONE',  ( -14.52663903635775533, -5.240707523384225297, 16.25846745537492311 ) ) ;
#48020 = CARTESIAN_POINT ( 'NONE',  ( 0.9173080810154149445, 6.103147713859270240, 3.800379278936838912 ) ) ;
#48021 = VECTOR ( 'NONE', #139550, 1000.000000000000000 ) ;
#48022 = LINE ( 'NONE', #46629, #104744 ) ;
#48023 = DIRECTION ( 'NONE',  ( -0.000000000000000000, 0.3543493200069153248, 0.9351131265310292928 ) ) ;
#48024 = CARTESIAN_POINT ( 'NONE',  ( 41.93336038379621300, 2.130196079827431532, -7.949999999999997513 ) ) ;
#48025 = FACE_OUTER_BOUND ( 'NONE', #24554, .T. ) ;
#48026 = EDGE_CURVE ( 'NONE', #131139, #122126, #11753, .T. ) ;
#48027 = VECTOR ( 'NONE', #739, 1000.000000000000227 ) ;
#48028 = ORIENTED_EDGE ( 'NONE', *, *, #77901, .F. ) ;
#48029 = ORIENTED_EDGE ( 'NONE', *, *, #38165, .T. ) ;
#48030 = CARTESIAN_POINT ( 'NONE',  ( 33.52083333333333570, 7.949999999999999289, 2.130196079827431532 ) ) ;
#48031 = ORIENTED_EDGE ( 'NONE', *, *, #52187, .T. ) ;
#48032 = ORIENTED_EDGE ( 'NONE', *, *, #125803, .T. ) ;
#48033 = FACE_OUTER_BOUND ( 'NONE', #72296, .T. ) ;
#48034 = AXIS2_PLACEMENT_3D ( 'NONE', #22151, #109896, #10558 ) ;
#48035 = ORIENTED_EDGE ( 'NONE', *, *, #93401, .F. ) ;
#48036 = LINE ( 'NONE', #15345, #43259 ) ;
#48037 = FACE_OUTER_BOUND ( 'NONE', #49883, .T. ) ;
#48038 = CARTESIAN_POINT ( 'NONE',  ( 2.510786437626908008, -27.52281430457053446, 5.000000000000000000 ) ) ;
#48039 = CARTESIAN_POINT ( 'NONE',  ( 29.02126352523143282, -4.472830434245839371, -4.472830434245840259 ) ) ;
#48040 = VERTEX_POINT ( 'NONE', #58197 ) ;
#48041 = CARTESIAN_POINT ( 'NONE',  ( 1.249915201643648333, 0.3999999999999995226, 2.317232462839659668 ) ) ;
#48042 = EDGE_LOOP ( 'NONE', ( #40640, #78002, #4914, #30109 ) ) ;
#48043 = LINE ( 'NONE', #3078, #128304 ) ;
#48044 = LINE ( 'NONE', #136447, #63853 ) ;
#48045 = FILL_AREA_STYLE_COLOUR ( '', #97635 ) ;
#48046 = ORIENTED_EDGE ( 'NONE', *, *, #76989, .T. ) ;
#48047 = VERTEX_POINT ( 'NONE', #35723 ) ;
#48048 = DIRECTION ( 'NONE',  ( -0.7071067811865486830, -0.7071067811865464625, 0.000000000000000000 ) ) ;
#48049 = CARTESIAN_POINT ( 'NONE',  ( -9.489213562373095101, -27.52281430457062328, 5.000000000000000000 ) ) ;
#48050 = DIRECTION ( 'NONE',  ( -0.7071067811865487940, 0.7071067811865463515, 0.000000000000000000 ) ) ;
#48051 = AXIS2_PLACEMENT_3D ( 'NONE', #135828, #136520, #2420 ) ;
#48052 = VECTOR ( 'NONE', #28878, 999.9999999999998863 ) ;
#48053 = CARTESIAN_POINT ( 'NONE',  ( 45.41209685856478728, 5.291415217122921177, -3.054999999999994831 ) ) ;
#48054 = CARTESIAN_POINT ( 'NONE',  ( 0.000000000000000000, 0.000000000000000000, 5.000000000000000000 ) ) ;
#48055 = LINE ( 'NONE', #13954, #66334 ) ;
#48056 = ORIENTED_EDGE ( 'NONE', *, *, #7484, .T. ) ;
#48057 = ORIENTED_EDGE ( 'NONE', *, *, #21131, .T. ) ;
#48058 = VECTOR ( 'NONE', #102606, 999.9999999999998863 ) ;
#48059 = LINE ( 'NONE', #36459, #72489 ) ;
#48060 = VERTEX_POINT ( 'NONE', #56038 ) ;
#48061 = DIRECTION ( 'NONE',  ( -0.3543493200069162685, -0.000000000000000000, -0.9351131265310288487 ) ) ;
#48062 = VERTEX_POINT ( 'NONE', #124114 ) ;
#48063 = CARTESIAN_POINT ( 'NONE',  ( 6.299744871391586898, -27.71228299555210484, 4.000000000000000000 ) ) ;
#48064 = EDGE_CURVE ( 'NONE', #25081, #130179, #2292, .T. ) ;
#48065 = CIRCLE ( 'NONE', #140551, 3.000000000000002665 ) ;
#48066 = FACE_BOUND ( 'NONE', #33204, .T. ) ;
#48067 = CARTESIAN_POINT ( 'NONE',  ( -14.99999999999989519, -19.06887692260762179, 4.000000000000000000 ) ) ;
#48068 = EDGE_CURVE ( 'NONE', #61017, #81835, #100229, .T. ) ;
#48069 = EDGE_CURVE ( 'NONE', #50737, #110777, #79943, .T. ) ;
#48070 =( NAMED_UNIT ( * ) SI_UNIT ( $, .STERADIAN. ) SOLID_ANGLE_UNIT ( ) );
#48071 = PLANE ( 'NONE',  #115048 ) ;
#48072 = FACE_BOUND ( 'NONE', #61985, .T. ) ;
#48074 = VERTEX_POINT ( 'NONE', #3718 ) ;
#48073 = DIRECTION ( 'NONE',  ( 0.7071067811865486830, -0.7071067811865464625, -0.000000000000000000 ) ) ;
#48075 = LINE ( 'NONE', #81438, #17033 ) ;
#48076 = ORIENTED_EDGE ( 'NONE', *, *, #6960, .F. ) ;
#48077 = ADVANCED_FACE ( 'NONE', ( #57455 ), #14643, .F. ) ;
#48078 = EDGE_CURVE ( 'NONE', #44266, #20400, #91501, .T. ) ;
#48079 = ORIENTED_EDGE ( 'NONE', *, *, #69380, .F. ) ;
#48080 = CARTESIAN_POINT ( 'NONE',  ( 69.32876352523145158, 0.000000000000000000, -6.109999999999998543 ) ) ;
#48081 = ORIENTED_EDGE ( 'NONE', *, *, #91935, .F. ) ;
#48082 = EDGE_CURVE ( 'NONE', #7189, #19552, #24095, .T. ) ;
#48083 = VECTOR ( 'NONE', #15914, 1000.000000000000227 ) ;
#48084 = DIRECTION ( 'NONE',  ( -0.6830127018922180770, -0.6830127018922204085, -0.2588190451025213501 ) ) ;
#48085 = EDGE_CURVE ( 'NONE', #55021, #59483, #1581, .T. ) ;
#48086 = ORIENTED_EDGE ( 'NONE', *, *, #1693, .T. ) ;
#48087 = EDGE_CURVE ( 'NONE', #50352, #63182, #122670, .T. ) ;
#48088 = DIRECTION ( 'NONE',  ( -0.3543493200069162685, -0.000000000000000000, -0.9351131265310288487 ) ) ;
#48089 = EDGE_CURVE ( 'NONE', #29579, #3561, #43857, .T. ) ;
#48090 = CARTESIAN_POINT ( 'NONE',  ( -17.99999999999986855, 17.58746187583906462, 4.000000000000000000 ) ) ;
#48091 = PLANE ( 'NONE',  #8782 ) ;
#48092 = CARTESIAN_POINT ( 'NONE',  ( -25.99806943317883423, -22.22500000000000142, 4.500000000000000888 ) ) ;
#48093 = CARTESIAN_POINT ( 'NONE',  ( 80.99451991528748351, 28.92564299267994699, 4.000000000000000000 ) ) ;
#48094 = DIRECTION ( 'NONE',  ( -0.6830127018922180770, -0.6830127018922204085, -0.2588190451025213501 ) ) ;
#48095 = EDGE_LOOP ( 'NONE', ( #100862, #87752, #5867, #110794 ) ) ;
#48096 = EDGE_LOOP ( 'NONE', ( #93509, #111681, #77183, #14699 ) ) ;
#48097 = DIRECTION ( 'NONE',  ( 0.000000000000000000, 0.000000000000000000, -1.000000000000000000 ) ) ;
#48099 = CARTESIAN_POINT ( 'NONE',  ( -26.99999999999981171, -15.03360074219758147, 5.000000000000000000 ) ) ;
#48098 = AXIS2_PLACEMENT_3D ( 'NONE', #112293, #69513, #642 ) ;
#48100 = VERTEX_POINT ( 'NONE', #111822 ) ;
#48101 = EDGE_CURVE ( 'NONE', #13228, #70912, #88650, .T. ) ;
#48102 = VERTEX_POINT ( 'NONE', #100925 ) ;
#48104 = ORIENTED_EDGE ( 'NONE', *, *, #18841, .T. ) ;
#48103 = CIRCLE ( 'NONE', #52628, 3.999999999999989786 ) ;
#48105 = LINE ( 'NONE', #94435, #22994 ) ;
#48106 = VERTEX_POINT ( 'NONE', #132881 ) ;
#48107 = LINE ( 'NONE', #48824, #64822 ) ;
#48108 = EDGE_CURVE ( 'NONE', #17123, #41182, #24366, .T. ) ;
#48109 = AXIS2_PLACEMENT_3D ( 'NONE', #100676, #12920, #122400 ) ;
#48110 = AXIS2_PLACEMENT_3D ( 'NONE', #55933, #89943, #1491 ) ;
#48111 =( NAMED_UNIT ( * ) SI_UNIT ( $, .STERADIAN. ) SOLID_ANGLE_UNIT ( ) );
#48112 = CARTESIAN_POINT ( 'NONE',  ( 6.921236474768553748, -9.717572351234235426E-16, -7.934999999999990727 ) ) ;
#48113 = DIRECTION ( 'NONE',  ( 0.6830127018922180770, -0.6830127018922204085, -0.2588190451025213501 ) ) ;
#48114 = ORIENTED_EDGE ( 'NONE', *, *, #66607, .F. ) ;
#48115 = LINE ( 'NONE', #82194, #1718 ) ;
#48116 = CARTESIAN_POINT ( 'NONE',  ( 119.0791937171295700, 3.975000000000002753, -6.884901960086283523 ) ) ;
#48117 = CARTESIAN_POINT ( 'NONE',  ( -13.49999999999990230, -15.29013452822855612, 0.3645803511610036796 ) ) ;
#48119 = ORIENTED_EDGE ( 'NONE', *, *, #92219, .T. ) ;
#48118 = CARTESIAN_POINT ( 'NONE',  ( -34.92500000000001137, -5.405284025385249436, -5.470147491473926316 ) ) ;
#48120 = EDGE_LOOP ( 'NONE', ( #66063, #35550, #65270, #87205, #103104 ) ) ;
#48121 = DIRECTION ( 'NONE',  ( -1.000000000000000000, 0.000000000000000000, 0.000000000000000000 ) ) ;
#48122 = CARTESIAN_POINT ( 'NONE',  ( 18.70710678118641468, -3.740707523384243505, 5.000000000000000000 ) ) ;
#48123 = LINE ( 'NONE', #92305, #109557 ) ;
#48124 = ORIENTED_EDGE ( 'NONE', *, *, #95616, .T. ) ;
#48125 = EDGE_CURVE ( 'NONE', #43222, #135455, #13180, .T. ) ;
#48126 = DIRECTION ( 'NONE',  ( -0.7071067811865486830, 0.7071067811865464625, 0.000000000000000000 ) ) ;
#48127 = EDGE_CURVE ( 'NONE', #58607, #126947, #81354, .T. ) ;
#48128 = DIRECTION ( 'NONE',  ( -0.000000000000000000, 0.3543493200069153248, 0.9351131265310292928 ) ) ;
#48129 = CARTESIAN_POINT ( 'NONE',  ( 125.2500000000000000, -9.735942053221458872E-16, 7.950000000000000178 ) ) ;
#48130 = CARTESIAN_POINT ( 'NONE',  ( -9.299744871391588674, -27.71228299555212971, 4.000000000000000000 ) ) ;
#48131 = ORIENTED_EDGE ( 'NONE', *, *, #6424, .T. ) ;
#48132 = DIRECTION ( 'NONE',  ( 0.7071067811865486830, -0.7071067811865464625, -0.000000000000000000 ) ) ;
#48133 = CARTESIAN_POINT ( 'NONE',  ( -27.18398860626900060, 28.73617430169806042, 5.000000000000000000 ) ) ;
#48134 = ADVANCED_FACE ( 'NONE', ( #128411 ), #29088, .T. ) ;
#48135 = CARTESIAN_POINT ( 'NONE',  ( 6.792893218813414791, 3.759292476615680112, 5.000000000000000000 ) ) ;
#48136 = CARTESIAN_POINT ( 'NONE',  ( 3.710381658649933190, 2.500000000000000888, 0.000000000000000000 ) ) ;
#48137 = PLANE ( 'NONE',  #124813 ) ;
#48138 = ORIENTED_EDGE ( 'NONE', *, *, #90365, .F. ) ;
#48139 = ORIENTED_EDGE ( 'NONE', *, *, #44544, .T. ) ;
#48140 = AXIS2_PLACEMENT_3D ( 'NONE', #3635, #49364, #27549 ) ;
#48141 = DIRECTION ( 'NONE',  ( 0.7071067811865487940, 0.7071067811865463515, -0.000000000000000000 ) ) ;
#48142 = DIRECTION ( 'NONE',  ( -0.000000000000000000, 0.000000000000000000, 1.000000000000000000 ) ) ;
#48143 = CARTESIAN_POINT ( 'NONE',  ( 5.812069808101887780, 7.934999999999993392, 2.126176841940951689 ) ) ;
#48144 = CARTESIAN_POINT ( 'NONE',  ( 66.14169371712955581, -2.130196079827424871, -7.949999999999998401 ) ) ;
#48145 = DIRECTION ( 'NONE',  ( 1.000000000000000000, 0.000000000000000000, 0.000000000000000000 ) ) ;
#48146 = LINE ( 'NONE', #92327, #69120 ) ;
#48147 = CARTESIAN_POINT ( 'NONE',  ( 72.29974487139158157, -27.71228299555256669, 4.000000000000000000 ) ) ;
#48148 = VERTEX_POINT ( 'NONE', #15317 ) ;
#48149 = ADVANCED_FACE ( 'NONE', ( #105899 ), #38541, .F. ) ;
#48150 = CARTESIAN_POINT ( 'NONE',  ( 52.60764783923757903, -49.05583548141700589, 39.86617647058822911 ) ) ;
#48151 = CARTESIAN_POINT ( 'NONE',  ( 14.99999999999989697, 19.55218569542897100, 5.000000000000000000 ) ) ;
#48152 = DIRECTION ( 'NONE',  ( 0.000000000000000000, -1.000000000000000000, 0.000000000000000000 ) ) ;
#48153 = CARTESIAN_POINT ( 'NONE',  ( 47.01626352523143026, -4.472830434245839371, 4.472830434245839371 ) ) ;
#48154 = CARTESIAN_POINT ( 'NONE',  ( -0.7933393645784717618, 21.75929247661549581, 4.998822639870701856 ) ) ;
#48155 = CARTESIAN_POINT ( 'NONE',  ( 2.816011393730999401, 28.73617430169785436, 5.000000000000000000 ) ) ;
#48156 = EDGE_CURVE ( 'NONE', #29361, #40495, #37847, .T. ) ;
#48157 = ORIENTED_EDGE ( 'NONE', *, *, #122596, .F. ) ;
#48158 = DIRECTION ( 'NONE',  ( 0.7071067811865487940, 0.7071067811865463515, -0.000000000000000000 ) ) ;
#48159 = VERTEX_POINT ( 'NONE', #116802 ) ;
#48160 = CARTESIAN_POINT ( 'NONE',  ( 13.82816939922342669, -11.24070752338417201, 4.000000000000000000 ) ) ;
#48161 = DIRECTION ( 'NONE',  ( 0.000000000000000000, 0.000000000000000000, 1.000000000000000000 ) ) ;
#48162 = DIRECTION ( 'NONE',  ( 0.7071067811865487940, 0.7071067811865463515, 0.000000000000000000 ) ) ;
#48163 = PLANE ( 'NONE',  #55599 ) ;
#48164 = EDGE_CURVE ( 'NONE', #85990, #91413, #83480, .T. ) ;
#48165 = FACE_OUTER_BOUND ( 'NONE', #125787, .T. ) ;
#48166 = ORIENTED_EDGE ( 'NONE', *, *, #106727, .F. ) ;
#48167 = EDGE_CURVE ( 'NONE', #42625, #1467, #18167, .T. ) ;
#48168 = CARTESIAN_POINT ( 'NONE',  ( 115.2875270504628986, 0.000000000000000000, -7.949999999999998401 ) ) ;
#48169 = DIRECTION ( 'NONE',  ( 0.000000000000000000, -1.000000000000000000, 0.000000000000000000 ) ) ;
#48170 = DIRECTION ( 'NONE',  ( -0.7071067811865487940, 0.7071067811865463515, 0.000000000000000000 ) ) ;
#48171 = CARTESIAN_POINT ( 'NONE',  ( 21.44840764549667611, 9.139736423841732040E-16, 0.000000000000000000 ) ) ;
#48172 = CARTESIAN_POINT ( 'NONE',  ( 77.80836038379621300, 7.949999999999997513, 2.130196079827431088 ) ) ;
#48173 = LINE ( 'NONE', #138039, #22818 ) ;
#48174 = EDGE_LOOP ( 'NONE', ( #565, #93605, #35278, #128112 ) ) ;
#48175 = EDGE_LOOP ( 'NONE', ( #54940, #27955, #73660, #92306 ) ) ;
#48176 = PRESENTATION_LAYER_ASSIGNMENT (  '', '', ( #115276 ) ) ;
#48177 = CARTESIAN_POINT ( 'NONE',  ( 65.45833333333332860, 3.974999999999997424, 6.884901960086288852 ) ) ;
#48178 = DIRECTION ( 'NONE',  ( 0.6830127018922180770, -0.6830127018922204085, -0.2588190451025213501 ) ) ;
#48179 = DIRECTION ( 'NONE',  ( 0.6830127018922180770, -0.6830127018922204085, -0.2588190451025213501 ) ) ;
#48180 = CARTESIAN_POINT ( 'NONE',  ( 25.65999999999999659, 9.521314400968980422E-16, 0.000000000000000000 ) ) ;
#48181 = ORIENTED_EDGE ( 'NONE', *, *, #28993, .T. ) ;
#48182 = EDGE_CURVE ( 'NONE', #50766, #130550, #48703, .T. ) ;
#48183 = DIRECTION ( 'NONE',  ( -0.7071067811865487940, 0.7071067811865463515, 0.000000000000000000 ) ) ;
#48184 = EDGE_CURVE ( 'NONE', #68957, #136293, #26240, .T. ) ;
#48185 = CYLINDRICAL_SURFACE ( 'NONE', #4942, 2.500000000000000000 ) ;
#48186 = CARTESIAN_POINT ( 'NONE',  ( 52.79209685856476852, -5.291415217122921177, 3.054999999999999272 ) ) ;
#48187 = CARTESIAN_POINT ( 'NONE',  ( 63.48921356237309510, -27.52281430457099631, 5.000000000000000000 ) ) ;
#48188 = ORIENTED_EDGE ( 'NONE', *, *, #25478, .F. ) ;
#48189 = ORIENTED_EDGE ( 'NONE', *, *, #79247, .T. ) ;
#48190 = CARTESIAN_POINT ( 'NONE',  ( -63.18398860626900415, 28.73617430169831621, 5.000000000000000000 ) ) ;
#48191 = CONICAL_SURFACE ( 'NONE', #57526, 2.055000000000001048, 0.9599310885968758145 ) ;
#48192 = CARTESIAN_POINT ( 'NONE',  ( 27.71230993966009137, -21.73547319004781997, 4.999917730833664642 ) ) ;
#48193 = CARTESIAN_POINT ( 'NONE',  ( -8.999999999999937828, 16.55218569542900298, 5.000000000000000000 ) ) ;
#48194 = AXIS2_PLACEMENT_3D ( 'NONE', #126484, #49687, #83007 ) ;
#48195 = LINE ( 'NONE', #81566, #34767 ) ;
#48196 = EDGE_CURVE ( 'NONE', #54208, #36944, #116081, .T. ) ;
#48197 = CARTESIAN_POINT ( 'NONE',  ( 12.71159235450332048, -2.500000000000000444, 3.061616997868384620E-16 ) ) ;
#48198 = ORIENTED_EDGE ( 'NONE', *, *, #83284, .T. ) ;
#48199 = CARTESIAN_POINT ( 'NONE',  ( 42.29974487139158157, -27.71228299555235708, 4.000000000000000000 ) ) ;
#48200 = DIRECTION ( 'NONE',  ( 0.3543493200069162685, -0.000000000000000000, -0.9351131265310288487 ) ) ;
#48201 = FACE_OUTER_BOUND ( 'NONE', #126833, .T. ) ;
#48202 = VECTOR ( 'NONE', #122046, 1000.000000000000000 ) ;
#48203 = DIRECTION ( 'NONE',  ( -0.7071067811865487940, 0.7071067811865463515, -0.000000000000000000 ) ) ;
#48204 = VECTOR ( 'NONE', #143447, 1000.000000000000227 ) ;
#48205 = VERTEX_POINT ( 'NONE', #82764 ) ;
#48206 = EDGE_LOOP ( 'NONE', ( #31557, #63659, #29294, #80543 ) ) ;
#48207 = DIRECTION ( 'NONE',  ( 0.7071067811865487940, 0.7071067811865463515, 0.000000000000000000 ) ) ;
#48208 = DIRECTION ( 'NONE',  ( 0.7071067811865486830, -0.7071067811865464625, -0.000000000000000000 ) ) ;
#48209 = CARTESIAN_POINT ( 'NONE',  ( -63.18398860626900415, 28.73617430169831621, 5.000000000000000000 ) ) ;
#48210 = DIRECTION ( 'NONE',  ( -0.000000000000000000, 0.000000000000000000, 1.000000000000000000 ) ) ;
#48211 = ORIENTED_EDGE ( 'NONE', *, *, #50407, .T. ) ;
#48212 = ORIENTED_EDGE ( 'NONE', *, *, #110907, .T. ) ;
#48213 = CARTESIAN_POINT ( 'NONE',  ( 90.25000000000000000, -9.735942053221458872E-16, 7.950000000000000178 ) ) ;
#48214 = FACE_OUTER_BOUND ( 'NONE', #57221, .T. ) ;
#48215 = VERTEX_POINT ( 'NONE', #60313 ) ;
#48216 = ORIENTED_EDGE ( 'NONE', *, *, #46428, .F. ) ;
#48217 = DIRECTION ( 'NONE',  ( -0.3543493200069162685, -0.000000000000000000, -0.9351131265310288487 ) ) ;
#48218 = DIRECTION ( 'NONE',  ( -0.000000000000000000, 0.000000000000000000, 1.000000000000000000 ) ) ;
#48219 = VECTOR ( 'NONE', #3547, 1000.000000000000000 ) ;
#48220 = VECTOR ( 'NONE', #99456, 1000.000000000000000 ) ;
#48221 = FACE_BOUND ( 'NONE', #8629, .T. ) ;
#48222 = FACE_OUTER_BOUND ( 'NONE', #45382, .T. ) ;
#48223 = EDGE_CURVE ( 'NONE', #44804, #75865, #70504, .T. ) ;
#48224 = DIRECTION ( 'NONE',  ( 1.000000000000000000, 1.224606353822377258E-16, 0.000000000000000000 ) ) ;
#48225 = PLANE ( 'NONE',  #108370 ) ;
#48226 = PLANE ( 'NONE',  #103632 ) ;
#48227 =( NAMED_UNIT ( * ) SI_UNIT ( $, .STERADIAN. ) SOLID_ANGLE_UNIT ( ) );
#48228 = DIRECTION ( 'NONE',  ( -1.000000000000000000, 8.326672684688676518E-17, -2.220446049250313574E-16 ) ) ;
#48229 = VERTEX_POINT ( 'NONE', #82080 ) ;
#48230 = EDGE_CURVE ( 'NONE', #19849, #69925, #39998, .T. ) ;
#48231 = ORIENTED_EDGE ( 'NONE', *, *, #34724, .F. ) ;
#48232 = CARTESIAN_POINT ( 'NONE',  ( 96.01626352523145158, -4.472830434245838482, 4.472830434245838482 ) ) ;
#48233 = ORIENTED_EDGE ( 'NONE', *, *, #14444, .F. ) ;
#48234 = EDGE_CURVE ( 'NONE', #20671, #141363, #26937, .T. ) ;
#48235 = LINE ( 'NONE', #14886, #39636 ) ;
#48236 = EDGE_CURVE ( 'NONE', #142768, #48818, #71185, .T. ) ;
#48237 = LINE ( 'NONE', #39528, #5252 ) ;
#48238 = EDGE_CURVE ( 'NONE', #65454, #35767, #16776, .T. ) ;
#48239 = CIRCLE ( 'NONE', #52777, 2.055000000000000604 ) ;
#48240 = DIRECTION ( 'NONE',  ( 0.7071067811865487940, -0.7071067811865463515, 0.000000000000000000 ) ) ;
#48241 = ORIENTED_EDGE ( 'NONE', *, *, #97815, .T. ) ;
#48242 = DIRECTION ( 'NONE',  ( -0.000000000000000000, 1.000000000000000000, -0.000000000000000000 ) ) ;
#48243 = DIRECTION ( 'NONE',  ( -1.000000000000000000, -0.000000000000000000, -0.000000000000000000 ) ) ;
#48244 = EDGE_CURVE ( 'NONE', #98679, #56501, #104493, .T. ) ;
#48245 = CARTESIAN_POINT ( 'NONE',  ( 25.40000000000000568, 7.827890782510358747, -1.361049978288880302 ) ) ;
#48247 = DIRECTION ( 'NONE',  ( 0.3543493200069162685, -0.000000000000000000, -0.9351131265310288487 ) ) ;
#48246 = DIRECTION ( 'NONE',  ( -1.000000000000000000, -1.224606353822377258E-16, -0.000000000000000000 ) ) ;
#48248 = PLANE ( 'NONE',  #71685 ) ;
#48249 = CARTESIAN_POINT ( 'NONE',  ( 6.852250093007166143, 4.584330080086930965E-16, 0.000000000000000000 ) ) ;
#48250 = ORIENTED_EDGE ( 'NONE', *, *, #63158, .T. ) ;
#48251 = CARTESIAN_POINT ( 'NONE',  ( -9.183988606268997046, 28.73617430169793607, 5.000000000000000000 ) ) ;
#48252 = DIRECTION ( 'NONE',  ( 0.7071067811865486830, -0.7071067811865464625, -0.000000000000000000 ) ) ;
#48253 = EDGE_CURVE ( 'NONE', #53545, #116521, #50843, .T. ) ;
#48254 = ORIENTED_EDGE ( 'NONE', *, *, #131620, .T. ) ;
#48255 = EDGE_LOOP ( 'NONE', ( #9455, #128469, #51490, #119752 ) ) ;
#48256 = ADVANCED_FACE ( 'NONE', ( #139309 ), #84216, .T. ) ;
#48257 = ORIENTED_EDGE ( 'NONE', *, *, #43257, .F. ) ;
#48258 = CARTESIAN_POINT ( 'NONE',  ( 45.50043019189810423, -3.055000000000002380, 5.291415217122920289 ) ) ;
#48259 = EDGE_LOOP ( 'NONE', ( #38663, #129742, #48233, #141291 ) ) ;
#48260 = EDGE_CURVE ( 'NONE', #48333, #31876, #136407, .T. ) ;
#48261 = CARTESIAN_POINT ( 'NONE',  ( 2.962472949537105826, -7.464222240803106570E-16, -6.094999999999989981 ) ) ;
#48262 = CARTESIAN_POINT ( 'NONE',  ( -16.15307943227677612, 1.820290827408419521, -33.22442919644333870 ) ) ;
#48263 = ORIENTED_EDGE ( 'NONE', *, *, #140856, .F. ) ;
#48264 = ORIENTED_EDGE ( 'NONE', *, *, #46508, .F. ) ;
#48265 = LINE ( 'NONE', #92462, #62685 ) ;
#48266 = CARTESIAN_POINT ( 'NONE',  ( 8.999999999999941380, -0.03360074219773377668, 5.000000000000000000 ) ) ;
#48268 = EDGE_LOOP ( 'NONE', ( #43852, #84823, #129479, #68072 ) ) ;
#48267 = CARTESIAN_POINT ( 'NONE',  ( 14.99999999999989164, -21.03360074219752462, 5.000000000000000000 ) ) ;
#48269 = VERTEX_POINT ( 'NONE', #140012 ) ;
#48270 = DIRECTION ( 'NONE',  ( 0.7071067811865487940, 0.7071067811865463515, 0.000000000000000000 ) ) ;
#48271 = DIRECTION ( 'NONE',  ( -0.7071067811865486830, 0.7071067811865464625, 0.000000000000000000 ) ) ;
#48272 = CARTESIAN_POINT ( 'NONE',  ( 126.7870968585647944, 3.054999999999997939, 5.291415217122920289 ) ) ;
#48273 = ORIENTED_EDGE ( 'NONE', *, *, #137601, .T. ) ;
#48274 = CARTESIAN_POINT ( 'NONE',  ( 39.48921356237310221, -27.52281430457082934, 5.000000000000000000 ) ) ;
#48275 = ORIENTED_EDGE ( 'NONE', *, *, #15741, .T. ) ;
#48276 = ORIENTED_EDGE ( 'NONE', *, *, #2710, .F. ) ;
#48277 = EDGE_LOOP ( 'NONE', ( #64621, #48166, #112689, #51561 ) ) ;
#48278 = VERTEX_POINT ( 'NONE', #10176 ) ;
#48279 = EDGE_CURVE ( 'NONE', #39230, #23998, #6861, .T. ) ;
#48280 = CARTESIAN_POINT ( 'NONE',  ( -1.265066702820505373, 12.75929247661558996, 18.34774599283956675 ) ) ;
#48281 = VECTOR ( 'NONE', #20771, 1000.000000000000000 ) ;
#48282 = VECTOR ( 'NONE', #28150, 999.9999999999998863 ) ;
#48283 = TOROIDAL_SURFACE ( 'NONE', #76131, 9.000000000000001776, 3.000000000000000000 ) ;
#48284 = DIRECTION ( 'NONE',  ( 0.7071067811865487940, 0.7071067811865463515, 0.000000000000000000 ) ) ;
#48285 = VECTOR ( 'NONE', #120034, 1000.000000000000227 ) ;
#48286 = DIRECTION ( 'NONE',  ( 1.000000000000000000, 0.000000000000000000, 0.000000000000000000 ) ) ;
#48287 = CARTESIAN_POINT ( 'NONE',  ( -2.999999999999983569, 19.93112307739198386, 4.000000000000000000 ) ) ;
#48288 = VECTOR ( 'NONE', #122274, 999.9999999999998863 ) ;
#48289 = PLANE ( 'NONE',  #37281 ) ;
#48290 = ORIENTED_EDGE ( 'NONE', *, *, #103119, .F. ) ;
#48291 = AXIS2_PLACEMENT_3D ( 'NONE', #81559, #38041, #91001 ) ;
#48292 = DIRECTION ( 'NONE',  ( -0.3543493200069162685, -0.000000000000000000, -0.9351131265310288487 ) ) ;
#48293 = ADVANCED_FACE ( 'NONE', ( #87751 ), #138866, .T. ) ;
#48294 = CARTESIAN_POINT ( 'NONE',  ( 20.24956980810188867, 3.967499999999998916, 6.871911579029510442 ) ) ;
#48295 = CARTESIAN_POINT ( 'NONE',  ( 8.483345613589499123, 22.22500000000000142, 4.500000000000000888 ) ) ;
#48296 = PLANE ( 'NONE',  #39081 ) ;
#48297 = CARTESIAN_POINT ( 'NONE',  ( -5.287690060339683917, -21.73547319004781642, 4.999917730833664642 ) ) ;
#48298 = ORIENTED_EDGE ( 'NONE', *, *, #94078, .T. ) ;
#48299 = ORIENTED_EDGE ( 'NONE', *, *, #64623, .F. ) ;
#48300 = ADVANCED_FACE ( 'NONE', ( #53716 ), #97918, .F. ) ;
#48301 = ORIENTED_EDGE ( 'NONE', *, *, #34068, .T. ) ;
#48302 = DIRECTION ( 'NONE',  ( -8.817971600062199903E-18, 0.3543493200069153248, 0.9351131265310292928 ) ) ;
#48303 = PLANE ( 'NONE',  #81215 ) ;
#48304 = LINE ( 'NONE', #72255, #91638 ) ;
#48305 = CIRCLE ( 'NONE', #57547, 2.500000000000000444 ) ;
#48306 = DIRECTION ( 'NONE',  ( 0.7071067811865486830, -0.7071067811865464625, -0.000000000000000000 ) ) ;
#48307 = CARTESIAN_POINT ( 'NONE',  ( 34.47516574401890210, -11.97193265888406088, 4.998110765256833510 ) ) ;
#48308 = CARTESIAN_POINT ( 'NONE',  ( 15.18398860626900237, 28.73617430169797871, 5.000000000000000000 ) ) ;
#48309 =( BOUNDED_SURFACE ( )  B_SPLINE_SURFACE ( 3, 2, ( 
 ( #107868, #108567, #131802 ),
 ( #131086, #132554, #10010 ),
 ( #98449, #33244, #8535 ),
 ( #43367, #96977, #120912 ),
 ( #77451, #121614, #141230 ),
 ( #41946, #141984, #31774 ),
 ( #31076, #119461, #64396 ),
 ( #97740, #42674, #75991 ),
 ( #120160, #25891, #57833 ),
 ( #1943, #57127, #112202 ),
 ( #44841, #24455, #68021 ),
 ( #12848, #101306, #78145 ),
 ( #102749, #33927, #59272 ),
 ( #2691, #69413, #47688 ),
 ( #123076, #46248, #124488 ),
 ( #90431, #46992, #123800 ) ),
 .UNSPECIFIED., .F., .F., .F. ) 
 B_SPLINE_SURFACE_WITH_KNOTS ( ( 4, 2, 2, 2, 2, 2, 2, 4 ),
 ( 3, 3 ),
 ( 6.460584911619963400, 6.634759501914277990, 6.808934092208593469, 6.983108682502908060, 7.157283272797222651, 7.331457863091538130, 7.505632453385852720, 7.853981633974482790 ),
 ( 0.000000000000000000, 1.000000000000000000 ),
 .UNSPECIFIED. ) 
 GEOMETRIC_REPRESENTATION_ITEM ( )  RATIONAL_B_SPLINE_SURFACE ( (
 ( 1.000000000000000000, 0.7180326832784531543, 1.000000000000000000),
 ( 1.000000000000000000, 0.7250426641246962012, 1.000000000000000000),
 ( 1.000000000000000000, 0.7353122387370452095, 1.000000000000000000),
 ( 1.000000000000000000, 0.7604116155349263106, 1.000000000000000000),
 ( 1.000000000000000000, 0.7752313834059556541, 1.000000000000000000),
 ( 1.000000000000000000, 0.8070860741948175932, 1.000000000000000000),
 ( 1.000000000000000000, 0.8241077986064178074, 1.000000000000000000),
 ( 1.000000000000000000, 0.8581174656083172536, 1.000000000000000000),
 ( 1.000000000000000000, 0.8751006588765014582, 1.000000000000000000),
 ( 1.000000000000000000, 0.9071649184815153699, 1.000000000000000000),
 ( 1.000000000000000000, 0.9222453908327410410, 1.000000000000000000),
 ( 1.000000000000000000, 0.9490805577171569363, 1.000000000000000000),
 ( 1.000000000000000000, 0.9608359430471251628, 1.000000000000000000),
 ( 1.000000000000000000, 0.9896287210067380435, 1.000000000000000000),
 ( 1.000000000000000000, 1.000097732991007682, 1.000000000000000000),
 ( 1.000000000000000000, 1.000000000000000000, 1.000000000000000000) ) ) 
 REPRESENTATION_ITEM ( '' )  SURFACE ( )  );
#48310 = CARTESIAN_POINT ( 'NONE',  ( 11.93159235450332112, 2.500000000000001332, 0.000000000000000000 ) ) ;
#48312 = LINE ( 'NONE', #38869, #90012 ) ;
#48311 = AXIS2_PLACEMENT_3D ( 'NONE', #1758, #23560, #112711 ) ;
#48313 = DIRECTION ( 'NONE',  ( -0.6830127018922181881, 0.6830127018922202975, -0.2588190451025214056 ) ) ;
#48314 = EDGE_CURVE ( 'NONE', #26004, #92199, #29779, .T. ) ;
#48315 = CARTESIAN_POINT ( 'NONE',  ( 29.99999999999978328, 14.58746187583910192, 4.000000000000000000 ) ) ;
#48316 = CARTESIAN_POINT ( 'NONE',  ( -25.43312800248726546, -21.74070752338406365, 6.915939825044133293 ) ) ;
#48317 = EDGE_LOOP ( 'NONE', ( #69182, #138516, #73634, #135546 ) ) ;
#48318 = VECTOR ( 'NONE', #61043, 1000.000000000000000 ) ;
#48319 = FACE_OUTER_BOUND ( 'NONE', #41700, .T. ) ;
#48320 = EDGE_LOOP ( 'NONE', ( #102414, #54137, #82266, #134027 ) ) ;
#48321 = VECTOR ( 'NONE', #81382, 999.9999999999998863 ) ;
#48322 =( BOUNDED_CURVE ( )  B_SPLINE_CURVE ( 3, ( #102458, #47394, #137216, #70564 ),
 .UNSPECIFIED., .F., .T. ) 
 B_SPLINE_CURVE_WITH_KNOTS ( ( 4, 4 ),
 ( 2.356194490192346613, 2.506762762968526292 ),
 .UNSPECIFIED. ) 
 CURVE ( )  GEOMETRIC_REPRESENTATION_ITEM ( )  RATIONAL_B_SPLINE_CURVE ( ( 1.000000000000000000, 0.9981116584018958626, 0.9981116584018958626, 1.000000000000000000 ) ) 
 REPRESENTATION_ITEM ( '' )  );
#48323 = VECTOR ( 'NONE', #133554, 999.9999999999998863 ) ;
#48324 = AXIS2_PLACEMENT_3D ( 'NONE', #640, #12236, #123891 ) ;
#48325 = DIRECTION ( 'NONE',  ( 0.7071067811865486830, -0.7071067811865464625, -0.000000000000000000 ) ) ;
#48327 = ORIENTED_EDGE ( 'NONE', *, *, #34704, .T. ) ;
#48326 = CARTESIAN_POINT ( 'NONE',  ( 2.524873872149526743, 14.25929247661556865, 9.797011795316644012 ) ) ;
#48328 = EDGE_CURVE ( 'NONE', #1167, #35612, #25209, .T. ) ;
#48329 = LINE ( 'NONE', #125902, #2373 ) ;
#48330 = DIRECTION ( 'NONE',  ( -0.7071067811865486830, -0.7071067811865464625, 0.000000000000000000 ) ) ;
#48331 = EDGE_LOOP ( 'NONE', ( #95554, #43989, #30234, #6172 ) ) ;
#48332 = LINE ( 'NONE', #46959, #60126 ) ;
#48333 = VERTEX_POINT ( 'NONE', #19632 ) ;
#48334 = LINE ( 'NONE', #104106, #125483 ) ;
#48335 = ORIENTED_EDGE ( 'NONE', *, *, #92942, .T. ) ;
#48336 = AXIS2_PLACEMENT_3D ( 'NONE', #59510, #29001, #137045 ) ;
#48337 = CARTESIAN_POINT ( 'NONE',  ( -16.83455439249994612, 8.717631302929021331, 5.000000000000000000 ) ) ;
#48338 = CARTESIAN_POINT ( 'NONE',  ( 100.4125270504628986, -7.949999999999998401, -4.867971026610728450E-16 ) ) ;
#48339 = CARTESIAN_POINT ( 'NONE',  ( -13.17183060077637613, -20.24070752338407075, 4.000000000000000000 ) ) ;
#48340 = LINE ( 'NONE', #136764, #34451 ) ;
#48341 = ORIENTED_EDGE ( 'NONE', *, *, #1179, .T. ) ;
#48342 = LINE ( 'NONE', #115692, #19151 ) ;
#48343 = CARTESIAN_POINT ( 'NONE',  ( -42.48921356237308800, -27.52281430457085065, 5.000000000000000000 ) ) ;
#48344 = LINE ( 'NONE', #83120, #97023 ) ;
#48345 = CARTESIAN_POINT ( 'NONE',  ( 19.54166666666666785, 3.047499999999993214, -5.278424836066146320 ) ) ;
#48346 = CARTESIAN_POINT ( 'NONE',  ( -42.29974487139158157, -27.71228299555235708, 4.000000000000000000 ) ) ;
#48347 = VECTOR ( 'NONE', #81667, 1000.000000000000000 ) ;
#48348 =( NAMED_UNIT ( * ) SI_UNIT ( $, .STERADIAN. ) SOLID_ANGLE_UNIT ( ) );
#48349 = ORIENTED_EDGE ( 'NONE', *, *, #14738, .T. ) ;
#48350 = LINE ( 'NONE', #2682, #39709 ) ;
#48351 = ORIENTED_EDGE ( 'NONE', *, *, #26511, .F. ) ;
#48352 = EDGE_CURVE ( 'NONE', #89986, #28308, #63876, .T. ) ;
#48353 = CARTESIAN_POINT ( 'NONE',  ( 93.91709685856477563, 3.054999999999998828, 5.291415217122922066 ) ) ;
#48354 = DIRECTION ( 'NONE',  ( 0.3543493200069162685, -0.000000000000000000, -0.9351131265310288487 ) ) ;
#48355 = DIRECTION ( 'NONE',  ( 0.000000000000000000, 6.938893903907227589E-15, -1.000000000000000000 ) ) ;
#48356 = CARTESIAN_POINT ( 'NONE',  ( 34.92499999999998295, 4.512461875839424152, 4.000000000000000000 ) ) ;
#48357 = VERTEX_POINT ( 'NONE', #21048 ) ;
#48358 = CARTESIAN_POINT ( 'NONE',  ( 7.149738618221213038, -22.22500000000000142, -10.94369129876685420 ) ) ;
#48359 = DIRECTION ( 'NONE',  ( 0.000000000000000000, -1.000000000000000000, 0.000000000000000000 ) ) ;
#48360 = ORIENTED_EDGE ( 'NONE', *, *, #104721, .F. ) ;
#48361 = DIRECTION ( 'NONE',  ( -0.3543493200069163240, 4.681814790819596721E-17, -0.9351131265310288487 ) ) ;
#48362 = EDGE_CURVE ( 'NONE', #59299, #23063, #8702, .T. ) ;
#48363 = CARTESIAN_POINT ( 'NONE',  ( -23.67183060077630685, -21.74070752338406720, 4.000000000000000000 ) ) ;
#48365 = ORIENTED_EDGE ( 'NONE', *, *, #49969, .T. ) ;
#48364 = DIRECTION ( 'NONE',  ( 0.000000000000000000, -1.000000000000000000, 0.000000000000000000 ) ) ;
#48366 = LINE ( 'NONE', #136799, #85345 ) ;
#48367 = FACE_OUTER_BOUND ( 'NONE', #60303, .T. ) ;
#48368 =( LENGTH_UNIT ( ) NAMED_UNIT ( * ) SI_UNIT ( .MILLI., .METRE. ) );
#48369 = VERTEX_POINT ( 'NONE', #52953 ) ;
#48370 = VERTEX_POINT ( 'NONE', #131985 ) ;
#48371 = VERTEX_POINT ( 'NONE', #119630 ) ;
#48372 = CARTESIAN_POINT ( 'NONE',  ( 81.22959685856476142, -6.110000000000000320, -1.637169565754161393 ) ) ;
#48373 = ORIENTED_EDGE ( 'NONE', *, *, #21484, .F. ) ;
#48374 = DIRECTION ( 'NONE',  ( -0.7071067811865486830, 0.7071067811865464625, 0.000000000000000000 ) ) ;
#48375 = CARTESIAN_POINT ( 'NONE',  ( 17.99999999999987921, -6.412538124160682251, 4.000000000000000000 ) ) ;
#48376 = CARTESIAN_POINT ( 'NONE',  ( -21.64790440752752687, 22.22500000000000142, 10.03118784388419016 ) ) ;
#48377 = LINE ( 'NONE', #78897, #140395 ) ;
#48378 = ORIENTED_EDGE ( 'NONE', *, *, #1887, .T. ) ;
#48379 = EDGE_CURVE ( 'NONE', #69904, #122313, #30529, .T. ) ;
#48380 = FACE_OUTER_BOUND ( 'NONE', #34130, .T. ) ;
#48381 = DIRECTION ( 'NONE',  ( -0.7071067811865487940, 0.7071067811865463515, -0.000000000000000000 ) ) ;
#48382 = CARTESIAN_POINT ( 'NONE',  ( 76.91209685856479439, 5.291415217122921177, -3.054999999999994831 ) ) ;
#48383 = ORIENTED_EDGE ( 'NONE', *, *, #89719, .F. ) ;
#48384 = DIRECTION ( 'NONE',  ( -0.7071067811865486830, -0.7071067811865464625, -0.000000000000000000 ) ) ;
#48385 = FACE_OUTER_BOUND ( 'NONE', #62086, .T. ) ;
#48386 = LINE ( 'NONE', #125966, #121081 ) ;
#48387 = AXIS2_PLACEMENT_3D ( 'NONE', #29332, #51831, #40943 ) ;
#48388 = VECTOR ( 'NONE', #65079, 999.9999999999998863 ) ;
#48389 = ORIENTED_EDGE ( 'NONE', *, *, #48464, .F. ) ;
#48390 = ORIENTED_EDGE ( 'NONE', *, *, #95567, .T. ) ;
#48391 = DIRECTION ( 'NONE',  ( -0.7071067811865486830, 0.7071067811865464625, 0.000000000000000000 ) ) ;
#48392 = CARTESIAN_POINT ( 'NONE',  ( 180.5498074873981693, -49.14999999999999147, 40.57313449935463012 ) ) ;
#48393 = DIRECTION ( 'NONE',  ( 0.000000000000000000, -1.000000000000000000, 0.000000000000000000 ) ) ;
#48394 = CIRCLE ( 'NONE', #2093, 2.500000000000000888 ) ;
#48395 = FILL_AREA_STYLE ('',( #4111 ) ) ;
#48396 = DIRECTION ( 'NONE',  ( -0.3543493200069162685, -0.000000000000000000, -0.9351131265310288487 ) ) ;
#48397 = CARTESIAN_POINT ( 'NONE',  ( 3.730677800976857306, -52.14999999999999147, -40.92499999999998295 ) ) ;
#48398 =( NAMED_UNIT ( * ) SI_UNIT ( $, .STERADIAN. ) SOLID_ANGLE_UNIT ( ) );
#48399 = ADVANCED_FACE ( 'NONE', ( #8020 ), #98614, .F. ) ;
#48400 = VERTEX_POINT ( 'NONE', #86339 ) ;
#48401 = VERTEX_POINT ( 'NONE', #63180 ) ;
#48402 = ADVANCED_FACE ( 'NONE', ( #121080 ), #107353, .F. ) ;
#48403 = CARTESIAN_POINT ( 'NONE',  ( -25.39999999999996305, 0.000000000000000000, 2.500000000000000000 ) ) ;
#48404 = ORIENTED_EDGE ( 'NONE', *, *, #94870, .T. ) ;
#48405 = MECHANICAL_DESIGN_GEOMETRIC_PRESENTATION_REPRESENTATION (  '', ( #141012 ), #69233 ) ;
#48406 = AXIS2_PLACEMENT_3D ( 'NONE', #18361, #48355, #139509 ) ;
#48407 = ADVANCED_FACE ( 'NONE', ( #96442 ), #142156, .T. ) ;
#48408 = EDGE_CURVE ( 'NONE', #24590, #31006, #94636, .T. ) ;
#48409 = VECTOR ( 'NONE', #37865, 1000.000000000000000 ) ;
#48410 = FACE_OUTER_BOUND ( 'NONE', #134784, .T. ) ;
#48411 = ORIENTED_EDGE ( 'NONE', *, *, #36069, .F. ) ;
#48412 = DIRECTION ( 'NONE',  ( 0.7071067811865487940, 0.7071067811865463515, 0.000000000000000000 ) ) ;
#48413 = CARTESIAN_POINT ( 'NONE',  ( 1.499999999999990896, -15.29013452822854546, 0.3645803511610392622 ) ) ;
#48414 = CARTESIAN_POINT ( 'NONE',  ( 31.49999999999978684, 1.087461875839228931, 4.000000000000000000 ) ) ;
#48415 = AXIS2_PLACEMENT_3D ( 'NONE', #46084, #6071, #59804 ) ;
#48416 = FACE_OUTER_BOUND ( 'NONE', #64412, .T. ) ;
#48417 = ORIENTED_EDGE ( 'NONE', *, *, #37689, .T. ) ;
#48418 = VECTOR ( 'NONE', #17125, 1000.000000000000227 ) ;
#48419 = CARTESIAN_POINT ( 'NONE',  ( 60.48921356237309510, -27.52281430457097500, 5.000000000000000000 ) ) ;
#48420 = DIRECTION ( 'NONE',  ( -1.000000000000000000, -0.000000000000000000, -0.000000000000000000 ) ) ;
#48421 = VECTOR ( 'NONE', #36035, 999.9999999999998863 ) ;
#48422 = EDGE_CURVE ( 'NONE', #139534, #134437, #20763, .T. ) ;
#48423 = EDGE_LOOP ( 'NONE', ( #112054, #114393, #53768, #82450 ) ) ;
#48424 = PLANE ( 'NONE',  #22598 ) ;
#48425 = ORIENTED_EDGE ( 'NONE', *, *, #23362, .T. ) ;
#48426 = EDGE_CURVE ( 'NONE', #61464, #131664, #110894, .T. ) ;
#48427 = VERTEX_POINT ( 'NONE', #36238 ) ;
#48428 = CARTESIAN_POINT ( 'NONE',  ( 8.207106781186485733, 15.75929247661555976, 5.000000000000000000 ) ) ;
#48429 = VERTEX_POINT ( 'NONE', #78311 ) ;
#48430 = ORIENTED_EDGE ( 'NONE', *, *, #102207, .F. ) ;
#48432 = VECTOR ( 'NONE', #86704, 1000.000000000000000 ) ;
#48431 = CARTESIAN_POINT ( 'NONE',  ( 71.02126352523144703, -4.472830434245838482, -4.472830434245840259 ) ) ;
#48433 = ORIENTED_EDGE ( 'NONE', *, *, #1606, .T. ) ;
#48434 =( GEOMETRIC_REPRESENTATION_CONTEXT ( 3 ) GLOBAL_UNCERTAINTY_ASSIGNED_CONTEXT ( ( #78119 ) ) GLOBAL_UNIT_ASSIGNED_CONTEXT ( ( #138510, #115272, #82024 ) ) REPRESENTATION_CONTEXT ( 'NONE', 'WORKASPACE' ) );
#48435 = EDGE_CURVE ( 'NONE', #82006, #96223, #76361, .T. ) ;
#48436 = LINE ( 'NONE', #112971, #85865 ) ;
#48437 = LINE ( 'NONE', #81085, #102766 ) ;
#48438 = CARTESIAN_POINT ( 'NONE',  ( 108.7920968585647756, -5.291415217122921177, 3.054999999999999272 ) ) ;
#48439 = CARTESIAN_POINT ( 'NONE',  ( -4.499999999999962697, -5.568876922607757685, 4.000000000000000000 ) ) ;
#48440 = CARTESIAN_POINT ( 'NONE',  ( -1.180000000000000382, 6.391994993740215847, 6.750000000000000888 ) ) ;
#48442 = FACE_OUTER_BOUND ( 'NONE', #54509, .T. ) ;
#48441 = PLANE ( 'NONE',  #54875 ) ;
#48443 = ADVANCED_FACE ( 'NONE', ( #79783 ), #47165, .F. ) ;
#48444 = CARTESIAN_POINT ( 'NONE',  ( 28.17183060077627133, -14.24070752338414003, 4.000000000000000000 ) ) ;
#48445 = CARTESIAN_POINT ( 'NONE',  ( 34.92499999999998295, 1.077975372831902590, 13.01339814852642540 ) ) ;
#48446 = SURFACE_STYLE_USAGE ( .BOTH. , #60797 ) ;
#48447 = EDGE_LOOP ( 'NONE', ( #83343, #711, #31533, #93510 ) ) ;
#48448 = CARTESIAN_POINT ( 'NONE',  ( 3.299744871391591339, -27.71228299555208352, 4.000000000000000000 ) ) ;
#48449 = CARTESIAN_POINT ( 'NONE',  ( 50.99451991528749062, 28.92564299267973738, 4.000000000000000000 ) ) ;
#48450 = VERTEX_POINT ( 'NONE', #1420 ) ;
#48451 = ORIENTED_EDGE ( 'NONE', *, *, #119882, .T. ) ;
#48452 = ADVANCED_FACE ( 'NONE', ( #123260 ), #11579, .F. ) ;
#48453 = CARTESIAN_POINT ( 'NONE',  ( -8.999999999999936051, 15.45873954670184780, -0.03131636524291922519 ) ) ;
#48454 = VERTEX_POINT ( 'NONE', #88482 ) ;
#48455 = PLANE ( 'NONE',  #83840 ) ;
#48456 = LINE ( 'NONE', #93388, #8450 ) ;
#48457 = DIRECTION ( 'NONE',  ( 0.7071067811865487940, 0.7071067811865463515, 0.000000000000000000 ) ) ;
#48458 = DIRECTION ( 'NONE',  ( 0.7071067811865487940, 0.7071067811865463515, -0.000000000000000000 ) ) ;
#48459 = ORIENTED_EDGE ( 'NONE', *, *, #106433, .F. ) ;
#48460 = ADVANCED_FACE ( 'NONE', ( #123964 ), #46433, .F. ) ;
#48461 = FACE_OUTER_BOUND ( 'NONE', #107837, .T. ) ;
#48462 = EDGE_LOOP ( 'NONE', ( #17132, #114644, #20490, #114127 ) ) ;
#48463 = CARTESIAN_POINT ( 'NONE',  ( -22.42819999999999681, 3.174999999999997602, 0.000000000000000000 ) ) ;
#48464 = EDGE_CURVE ( 'NONE', #12209, #76457, #134859, .T. ) ;
#48465 = CARTESIAN_POINT ( 'NONE',  ( 25.29623647476855908, 7.934999999999990727, -1.457635852685135314E-15 ) ) ;
#48466 = CARTESIAN_POINT ( 'NONE',  ( 0.2997448713915885632, -27.71228299555206220, 4.000000000000000000 ) ) ;
#48467 = CARTESIAN_POINT ( 'NONE',  ( 14.70008083135199684, -9.500037224963584492, -0.2878867768745749234 ) ) ;
#48468 = ORIENTED_EDGE ( 'NONE', *, *, #16648, .F. ) ;
#48469 = ORIENTED_EDGE ( 'NONE', *, *, #67119, .T. ) ;
#48470 = VERTEX_POINT ( 'NONE', #100065 ) ;
#48471 = DIRECTION ( 'NONE',  ( 0.3543493200069162685, -0.000000000000000000, -0.9351131265310288487 ) ) ;
#48472 = CARTESIAN_POINT ( 'NONE',  ( -5.999999999999953815, -21.84840872380825161, 2.849755605029594019 ) ) ;
#48473 = FACE_OUTER_BOUND ( 'NONE', #38644, .T. ) ;
#48474 = DIRECTION ( 'NONE',  ( 0.7071067811865487940, -0.7071067811865463515, 0.000000000000000000 ) ) ;
#48475 = ORIENTED_EDGE ( 'NONE', *, *, #32023, .F. ) ;
#48476 = CARTESIAN_POINT ( 'NONE',  ( -22.82900182742193351, 7.795401085224272109, 5.000000000000000000 ) ) ;
#48477 = DIRECTION ( 'NONE',  ( -1.000000000000000000, -1.224606353822377258E-16, -0.000000000000000000 ) ) ;
#48478 = CARTESIAN_POINT ( 'NONE',  ( -2.999999999999981792, -12.41253812416062985, 4.000000000000000000 ) ) ;
#48479 = EDGE_CURVE ( 'NONE', #135356, #142320, #91345, .T. ) ;
#48480 = LINE ( 'NONE', #68840, #25710 ) ;
#48481 = LINE ( 'NONE', #81869, #127611 ) ;
#48482 = EDGE_LOOP ( 'NONE', ( #40801, #38961 ) ) ;
#48483 = CARTESIAN_POINT ( 'NONE',  ( 23.99451991528749062, 28.92564299267954908, 4.000000000000000000 ) ) ;
#48484 = AXIS2_PLACEMENT_3D ( 'NONE', #136512, #72755, #83600 ) ;
#48485 = AXIS2_PLACEMENT_3D ( 'NONE', #74526, #66497, #98404 ) ;
#48486 = VECTOR ( 'NONE', #90097, 1000.000000000000000 ) ;
#48487 = DIRECTION ( 'NONE',  ( -1.000000000000000000, -0.000000000000000000, -0.000000000000000000 ) ) ;
#48488 = VERTEX_POINT ( 'NONE', #102212 ) ;
#48489 = VECTOR ( 'NONE', #62164, 1000.000000000000000 ) ;
#48490 = DIRECTION ( 'NONE',  ( -0.7071067811865486830, 0.7071067811865464625, 0.000000000000000000 ) ) ;
#48492 = ORIENTED_EDGE ( 'NONE', *, *, #21131, .F. ) ;
#48491 = DIRECTION ( 'NONE',  ( -0.000000000000000000, -0.000000000000000000, 1.000000000000000000 ) ) ;
#48493 = ORIENTED_EDGE ( 'NONE', *, *, #142124, .T. ) ;
#48494 = ADVANCED_FACE ( 'NONE', ( #715 ), #134123, .T. ) ;
#48495 = DIRECTION ( 'NONE',  ( 0.000000000000000000, 0.000000000000000000, 1.000000000000000000 ) ) ;
#48496 = CARTESIAN_POINT ( 'NONE',  ( -11.99999999999991651, 4.965500833774314948, -4.007596771432631044 ) ) ;
#48497 = DIRECTION ( 'NONE',  ( -0.7071067811865486830, 0.7071067811865464625, 0.000000000000000000 ) ) ;
#48498 = ORIENTED_EDGE ( 'NONE', *, *, #3250, .F. ) ;
#48499 = CARTESIAN_POINT ( 'NONE',  ( 9.524999999999995026, -4.870000000000013429, -40.00000000000000000 ) ) ;
#48500 = AXIS2_PLACEMENT_3D ( 'NONE', #45686, #123945, #121761 ) ;
#48501 = ORIENTED_EDGE ( 'NONE', *, *, #25668, .T. ) ;
#48502 = LINE ( 'NONE', #92704, #10401 ) ;
#48503 = DIRECTION ( 'NONE',  ( -0.000000000000000000, -0.3543493200069152693, 0.9351131265310292928 ) ) ;
#48504 = CARTESIAN_POINT ( 'NONE',  ( 128.2666937171295274, -7.949999999999999289, 2.130196079827424427 ) ) ;
#48505 = LINE ( 'NONE', #50645, #136457 ) ;
#48506 = CIRCLE ( 'NONE', #122583, 2.500000000000000888 ) ;
#48507 = CARTESIAN_POINT ( 'NONE',  ( 47.91252705046289151, -7.949999999999998401, -4.867971026610728450E-16 ) ) ;
#48508 = DIRECTION ( 'NONE',  ( 0.7071067811865486830, -0.7071067811865464625, -0.000000000000000000 ) ) ;
#48509 = DIRECTION ( 'NONE',  ( -1.000000000000000000, -0.000000000000000000, -0.000000000000000000 ) ) ;
#48510 = CARTESIAN_POINT ( 'NONE',  ( -22.17183060077631396, -5.240707523384232402, 4.000000000000000000 ) ) ;
#48511 = CARTESIAN_POINT ( 'NONE',  ( 32.06206980810188867, -7.934999999999991616, -2.126176841940955242 ) ) ;
#48513 = VECTOR ( 'NONE', #140168, 1000.000000000000000 ) ;
#48512 = DIRECTION ( 'NONE',  ( 0.000000000000000000, -1.000000000000000000, 0.000000000000000000 ) ) ;
#48514 = LINE ( 'NONE', #62259, #36719 ) ;
#48515 = VECTOR ( 'NONE', #90186, 1000.000000000000000 ) ;
#48516 = LINE ( 'NONE', #126091, #42013 ) ;
#48517 = DIRECTION ( 'NONE',  ( -0.000000000000000000, 0.3543493200069153248, 0.9351131265310292928 ) ) ;
#48518 = VERTEX_POINT ( 'NONE', #2867 ) ;
#48519 = ORIENTED_EDGE ( 'NONE', *, *, #126966, .T. ) ;
#48520 = CARTESIAN_POINT ( 'NONE',  ( 91.27083333333334281, -7.949999999999999289, -2.130196079827426203 ) ) ;
#48521 = VECTOR ( 'NONE', #48361, 1000.000000000000227 ) ;
#48522 = ORIENTED_EDGE ( 'NONE', *, *, #120441, .F. ) ;
#48523 = ORIENTED_EDGE ( 'NONE', *, *, #118015, .F. ) ;
#48524 = EDGE_CURVE ( 'NONE', #10002, #86852, #34810, .T. ) ;
#48525 = DIRECTION ( 'NONE',  ( 0.000000000000000000, 1.000000000000000000, -0.000000000000000000 ) ) ;
#48526 = CARTESIAN_POINT ( 'NONE',  ( 22.64997294953709783, -4.461849672132299105, 4.461849672132299993 ) ) ;
#48527 = CARTESIAN_POINT ( 'NONE',  ( 14.11343486808858216, 9.243406610528717593, -2.206469626207758772 ) ) ;
#48528 = VERTEX_POINT ( 'NONE', #110194 ) ;
#48529 = AXIS2_PLACEMENT_3D ( 'NONE', #96651, #20537, #85101 ) ;
#48530 = CARTESIAN_POINT ( 'NONE',  ( -30.09843580608217550, 11.25929247661560595, 10.79108189686400010 ) ) ;
#48531 = VECTOR ( 'NONE', #57457, 1000.000000000000227 ) ;
#48532 = CARTESIAN_POINT ( 'NONE',  ( 7.139999999999956160, -35.56014942880460694, -11.72188031596273206 ) ) ;
#48533 = VECTOR ( 'NONE', #119955, 1000.000000000000000 ) ;
#48534 = CARTESIAN_POINT ( 'NONE',  ( 23.99999999999983302, -18.03360074219755660, 5.000000000000000000 ) ) ;
#48535 = CARTESIAN_POINT ( 'NONE',  ( 126.4955769715163996, 6.892355196946173379, 1.023687185015854428 ) ) ;
#48536 = EDGE_CURVE ( 'NONE', #99466, #70483, #99309, .T. ) ;
#48538 = EDGE_CURVE ( 'NONE', #98566, #18405, #143552, .T. ) ;
#48537 = AXIS2_PLACEMENT_3D ( 'NONE', #18957, #94367, #44305 ) ;
#48539 = CARTESIAN_POINT ( 'NONE',  ( 5.229957205422025801, 21.73644205237997795, 5.000000000000000888 ) ) ;
#48540 = CARTESIAN_POINT ( 'NONE',  ( 34.92499999999998295, -2.038703271653913962, -4.194424194487909929 ) ) ;
#48541 = CARTESIAN_POINT ( 'NONE',  ( 0.000000000000000000, 0.000000000000000000, 5.000000000000000000 ) ) ;
#48542 = VECTOR ( 'NONE', #89535, 999.9999999999998863 ) ;
#48543 = CARTESIAN_POINT ( 'NONE',  ( 34.92499999999998295, 22.22500000000000142, 4.000000000000000000 ) ) ;
#48544 = CARTESIAN_POINT ( 'NONE',  ( 15.72281430457048934, -21.72500000000000497, 5.000000000000000000 ) ) ;
#48545 = CARTESIAN_POINT ( 'NONE',  ( 9.489213562373095101, -27.52281430457062328, 5.000000000000000000 ) ) ;
#48546 = LINE ( 'NONE', #14487, #52239 ) ;
#48547 = CARTESIAN_POINT ( 'NONE',  ( 55.57593013779205648, -49.04047092356913851, 39.41690992498946855 ) ) ;
#48548 = ORIENTED_EDGE ( 'NONE', *, *, #27709, .F. ) ;
#48549 = ORIENTED_EDGE ( 'NONE', *, *, #30927, .T. ) ;
#48551 = ADVANCED_FACE ( 'NONE', ( #89188 ), #133413, .F. ) ;
#48550 = CARTESIAN_POINT ( 'NONE',  ( 112.4379301918981184, -6.110000000000001208, 1.637169565754158951 ) ) ;
#48552 = ORIENTED_EDGE ( 'NONE', *, *, #29580, .T. ) ;
#48553 = EDGE_CURVE ( 'NONE', #66785, #32778, #67454, .T. ) ;
#48554 = DIRECTION ( 'NONE',  ( -0.7071067811865486830, -0.7071067811865464625, 0.000000000000000000 ) ) ;
#48555 = VECTOR ( 'NONE', #47143, 999.9999999999998863 ) ;
#48556 = SURFACE_STYLE_USAGE ( .BOTH. , #81937 ) ;
#48557 = ORIENTED_EDGE ( 'NONE', *, *, #132967, .F. ) ;
#48558 = EDGE_CURVE ( 'NONE', #18419, #31469, #60138, .T. ) ;
#48559 = DIRECTION ( 'NONE',  ( 0.7071067811865486830, 0.7071067811865463515, 0.000000000000000000 ) ) ;
#48560 = DIRECTION ( 'NONE',  ( 0.000000000000000000, -1.000000000000000000, 0.000000000000000000 ) ) ;
#48561 = CARTESIAN_POINT ( 'NONE',  ( 106.6620968585647802, -5.291415217122919401, 3.054999999999997939 ) ) ;
#48562 = ORIENTED_EDGE ( 'NONE', *, *, #23009, .F. ) ;
#48563 = ORIENTED_EDGE ( 'NONE', *, *, #42043, .F. ) ;
#48564 = FACE_OUTER_BOUND ( 'NONE', #7612, .T. ) ;
#48565 = DIRECTION ( 'NONE',  ( 0.3543493200069162685, -0.000000000000000000, -0.9351131265310288487 ) ) ;
#48566 = LINE ( 'NONE', #69370, #66338 ) ;
#48567 = EDGE_LOOP ( 'NONE', ( #1925, #56712, #48079, #89821 ) ) ;
#48568 = ORIENTED_EDGE ( 'NONE', *, *, #137035, .F. ) ;
#48569 = ORIENTED_EDGE ( 'NONE', *, *, #13335, .F. ) ;
#48570 = DIRECTION ( 'NONE',  ( 0.000000000000000000, 0.000000000000000000, -1.000000000000000000 ) ) ;
#48571 = CARTESIAN_POINT ( 'NONE',  ( 3.421236474768552860, -9.717572351234235426E-16, -7.934999999999990727 ) ) ;
#48572 = ADVANCED_FACE ( 'NONE', ( #27460 ), #94856, .F. ) ;
#48573 =( NAMED_UNIT ( * ) SI_UNIT ( $, .STERADIAN. ) SOLID_ANGLE_UNIT ( ) );
#48574 = EDGE_CURVE ( 'NONE', #11869, #135832, #126779, .T. ) ;
#48575 =( NAMED_UNIT ( * ) PLANE_ANGLE_UNIT ( ) SI_UNIT ( $, .RADIAN. ) );
#48576 = ORIENTED_EDGE ( 'NONE', *, *, #91613, .F. ) ;
#48577 = VERTEX_POINT ( 'NONE', #82584 ) ;
#48578 = EDGE_CURVE ( 'NONE', #15499, #7366, #14472, .T. ) ;
#48579 = LINE ( 'NONE', #14519, #121964 ) ;
#48580 = ORIENTED_EDGE ( 'NONE', *, *, #104007, .T. ) ;
#48581 = ORIENTED_EDGE ( 'NONE', *, *, #19671, .T. ) ;
#48582 = EDGE_CURVE ( 'NONE', #95370, #56470, #137696, .T. ) ;
#48583 = EDGE_CURVE ( 'NONE', #137404, #49688, #124297, .T. ) ;
#48584 = FACE_OUTER_BOUND ( 'NONE', #139394, .T. ) ;
#48585 = DIRECTION ( 'NONE',  ( 0.7071067811865487940, 0.7071067811865463515, 0.000000000000000000 ) ) ;
#48586 = VERTEX_POINT ( 'NONE', #104304 ) ;
#48587 = CARTESIAN_POINT ( 'NONE',  ( 15.83652871126539630, 15.75929247661555443, 9.299976744542956197 ) ) ;
#48588 = AXIS2_PLACEMENT_3D ( 'NONE', #89392, #20541, #132935 ) ;
#48589 = DIRECTION ( 'NONE',  ( 0.000000000000000000, 0.000000000000000000, -1.000000000000000000 ) ) ;
#48590 = AXIS2_PLACEMENT_3D ( 'NONE', #1521, #87854, #21167 ) ;
#48591 = CIRCLE ( 'NONE', #4540, 2.999999999999999112 ) ;
#48592 =( GEOMETRIC_REPRESENTATION_CONTEXT ( 3 ) GLOBAL_UNCERTAINTY_ASSIGNED_CONTEXT ( ( #91150 ) ) GLOBAL_UNIT_ASSIGNED_CONTEXT ( ( #71137, #136363, #138520 ) ) REPRESENTATION_CONTEXT ( 'NONE', 'WORKASPACE' ) );
#48593 = CARTESIAN_POINT ( 'NONE',  ( 32.29289321881323360, 5.259292476615672562, 5.000000000000000000 ) ) ;
#48594 = VECTOR ( 'NONE', #77175, 1000.000000000000227 ) ;
#48595 = DIRECTION ( 'NONE',  ( -0.7071067811865486830, -0.7071067811865464625, 0.000000000000000000 ) ) ;
#48596 = FACE_BOUND ( 'NONE', #62968, .T. ) ;
#48597 = EDGE_CURVE ( 'NONE', #91814, #10831, #39823, .T. ) ;
#48598 = ORIENTED_EDGE ( 'NONE', *, *, #41251, .T. ) ;
#48599 = CARTESIAN_POINT ( 'NONE',  ( 54.18398860626899705, 28.73617430169825226, 5.000000000000000000 ) ) ;
#48600 = CARTESIAN_POINT ( 'NONE',  ( 0.7307956238753654521, -0.4000000000000004108, 2.467792535850613866 ) ) ;
#48601 = CARTESIAN_POINT ( 'NONE',  ( 8.999999999999937828, -1.068876922607798985, 4.000000000000000000 ) ) ;
#48602 = EDGE_CURVE ( 'NONE', #87366, #128057, #103595, .T. ) ;
#48603 = ORIENTED_EDGE ( 'NONE', *, *, #79518, .F. ) ;
#48604 = DIRECTION ( 'NONE',  ( -0.7071067811865487940, 0.7071067811865463515, 0.000000000000000000 ) ) ;
#48605 = ORIENTED_EDGE ( 'NONE', *, *, #120053, .T. ) ;
#48606 = ORIENTED_EDGE ( 'NONE', *, *, #133674, .F. ) ;
#48607 = VECTOR ( 'NONE', #96106, 1000.000000000000000 ) ;
#48608 = ORIENTED_EDGE ( 'NONE', *, *, #14480, .T. ) ;
#48609 = CARTESIAN_POINT ( 'NONE',  ( 35.05793019189810877, 6.110000000000000320, -1.637169565754156064 ) ) ;
#48610 = ORIENTED_EDGE ( 'NONE', *, *, #108588, .F. ) ;
#48611 = EDGE_CURVE ( 'NONE', #84395, #80606, #71018, .T. ) ;
#48612 = DIRECTION ( 'NONE',  ( -0.000000000000000000, -0.000000000000000000, 1.000000000000000000 ) ) ;
#48613 = LINE ( 'NONE', #137046, #143275 ) ;
#48614 = DIRECTION ( 'NONE',  ( -0.7071067811865487940, 0.7071067811865463515, 0.000000000000000000 ) ) ;
#48615 = EDGE_LOOP ( 'NONE', ( #21037, #137139, #15225, #28020 ) ) ;
#48616 = CARTESIAN_POINT ( 'NONE',  ( 19.77149322861323455, 20.25929247661551003, 7.808871592221815483 ) ) ;
#48617 = PLANE ( 'NONE',  #122196 ) ;
#48618 = AXIS2_PLACEMENT_3D ( 'NONE', #44448, #43698, #130734 ) ;
#48619 = EDGE_CURVE ( 'NONE', #22222, #4418, #69598, .T. ) ;
#48620 =( LENGTH_UNIT ( ) NAMED_UNIT ( * ) SI_UNIT ( .MILLI., .METRE. ) );
#48621 = VECTOR ( 'NONE', #22830, 1000.000000000000000 ) ;
#48622 = CARTESIAN_POINT ( 'NONE',  ( -34.92500000000001137, -8.993876922607963564, 4.000000000000000000 ) ) ;
#48623 = DIRECTION ( 'NONE',  ( 0.6830127018922180770, -0.6830127018922204085, -0.2588190451025213501 ) ) ;
#48624 = CARTESIAN_POINT ( 'NONE',  ( -59.99451991528749772, 28.92564299267980132, 4.000000000000000000 ) ) ;
#48625 = CARTESIAN_POINT ( 'NONE',  ( 0.000000000000000000, 0.000000000000000000, 5.000000000000000000 ) ) ;
#48626 = ORIENTED_EDGE ( 'NONE', *, *, #68513, .T. ) ;
#48627 = EDGE_LOOP ( 'NONE', ( #71342, #54399, #76871, #27204 ) ) ;
#48629 = ORIENTED_EDGE ( 'NONE', *, *, #1429, .F. ) ;
#48628 = EDGE_CURVE ( 'NONE', #121707, #139204, #5705, .T. ) ;
#48630 = ORIENTED_EDGE ( 'NONE', *, *, #101202, .T. ) ;
#48631 = CARTESIAN_POINT ( 'NONE',  ( 1.499999999999980460, -12.08601207473289740, -10.46905243149095099 ) ) ;
#48632 = EDGE_LOOP ( 'NONE', ( #82048, #71863, #73460, #31241 ) ) ;
#48633 = VECTOR ( 'NONE', #718, 1000.000000000000000 ) ;
#48634 = EDGE_LOOP ( 'NONE', ( #88561, #12520, #122921, #20553 ) ) ;
#48635 = CARTESIAN_POINT ( 'NONE',  ( 10.17183060077640810, -5.240707523384230626, 4.000000000000000000 ) ) ;
#48636 = CARTESIAN_POINT ( 'NONE',  ( 78.18398860626899705, 28.73617430169841924, 5.000000000000000000 ) ) ;
#48637 = VECTOR ( 'NONE', #70425, 999.9999999999998863 ) ;
#48638 = LINE ( 'NONE', #115264, #143471 ) ;
#48639 = ORIENTED_EDGE ( 'NONE', *, *, #37793, .F. ) ;
#48640 = VECTOR ( 'NONE', #126616, 1000.000000000000000 ) ;
#48641 = EDGE_CURVE ( 'NONE', #5100, #113749, #94154, .T. ) ;
#48642 = CARTESIAN_POINT ( 'NONE',  ( 12.71159235450332048, 9.902892378096218942E-16, 0.000000000000000000 ) ) ;
#48643 = ORIENTED_EDGE ( 'NONE', *, *, #74583, .T. ) ;
#48644 = CARTESIAN_POINT ( 'NONE',  ( 25.99806943317883068, -22.22500000000000142, 4.500000000000000888 ) ) ;
#48645 = EDGE_CURVE ( 'NONE', #22290, #132198, #138390, .T. ) ;
#48646 = DIRECTION ( 'NONE',  ( -1.000000000000000000, -1.224606353822377258E-16, -0.000000000000000000 ) ) ;
#48647 = AXIS2_PLACEMENT_3D ( 'NONE', #66970, #89421, #233 ) ;
#48648 = CARTESIAN_POINT ( 'NONE',  ( -0.8079301918981138808, -7.934999999999991616, -2.126176841940955242 ) ) ;
#48649 = VERTEX_POINT ( 'NONE', #72466 ) ;
#48650 = CARTESIAN_POINT ( 'NONE',  ( 97.18293019189810877, -1.637169565754159173, -6.109999999999999432 ) ) ;
#48651 = LINE ( 'NONE', #95708, #125390 ) ;
#48652 = DIRECTION ( 'NONE',  ( 0.3543493200069162685, -0.000000000000000000, -0.9351131265310288487 ) ) ;
#48653 = ORIENTED_EDGE ( 'NONE', *, *, #10640, .F. ) ;
#48654 = ORIENTED_EDGE ( 'NONE', *, *, #34468, .F. ) ;
#48655 = LINE ( 'NONE', #37794, #7823 ) ;
#48656 = VECTOR ( 'NONE', #18171, 1000.000000000000000 ) ;
#48657 = ORIENTED_EDGE ( 'NONE', *, *, #66430, .T. ) ;
#48658 = SURFACE_STYLE_USAGE ( .BOTH. , #50093 ) ;
#48659 = DIRECTION ( 'NONE',  ( -0.7071067811865486830, -0.7071067811865464625, 0.000000000000000000 ) ) ;
#48660 = DIRECTION ( 'NONE',  ( 0.000000000000000000, -1.000000000000000000, 0.000000000000000000 ) ) ;
#48661 = EDGE_CURVE ( 'NONE', #75984, #70943, #127510, .T. ) ;
#48662 = DIRECTION ( 'NONE',  ( 1.000000000000000000, 0.000000000000000000, 0.000000000000000000 ) ) ;
#48663 = CARTESIAN_POINT ( 'NONE',  ( 183.7102003651264681, -49.08473565290606189, -39.91868829876866442 ) ) ;
#48664 = EDGE_LOOP ( 'NONE', ( #84180, #98132, #117533, #15746 ) ) ;
#48665 = PLANE ( 'NONE',  #59990 ) ;
#48666 = DIRECTION ( 'NONE',  ( -1.000000000000000000, -8.718663809566799855E-16, 0.000000000000000000 ) ) ;
#48667 = CARTESIAN_POINT ( 'NONE',  ( 27.99999999999999645, 2.055000000000001492, 2.789133085058098087E-16 ) ) ;
#48668 = ORIENTED_EDGE ( 'NONE', *, *, #15992, .F. ) ;
#48669 = SPHERICAL_SURFACE ( 'NONE', #58237, 0.5000000000000000000 ) ;
#48670 = VECTOR ( 'NONE', #87857, 1000.000000000000000 ) ;
#48671 = CARTESIAN_POINT ( 'NONE',  ( -25.39999999999996305, 0.000000000000000000, 0.000000000000000000 ) ) ;
#48672 = EDGE_LOOP ( 'NONE', ( #64887, #114217, #115850, #66502 ) ) ;
#48674 = ORIENTED_EDGE ( 'NONE', *, *, #106291, .F. ) ;
#48673 = LINE ( 'NONE', #3688, #99581 ) ;
#48675 = VERTEX_POINT ( 'NONE', #17316 ) ;
#48676 = LINE ( 'NONE', #104462, #105107 ) ;
#48677 = CARTESIAN_POINT ( 'NONE',  ( -23.99999999999982592, 8.966399257802171618, 5.000000000000000000 ) ) ;
#48679 = ORIENTED_EDGE ( 'NONE', *, *, #77611, .T. ) ;
#48678 = MECHANICAL_DESIGN_GEOMETRIC_PRESENTATION_REPRESENTATION (  '', ( #13869 ), #13976 ) ;
#48680 = DIRECTION ( 'NONE',  ( -1.000000000000000000, -1.224606353822377258E-16, -0.000000000000000000 ) ) ;
#48681 = CARTESIAN_POINT ( 'NONE',  ( 2.999999999999999112, -4.600000000000094680, 34.92499999999996874 ) ) ;
#48682 = DIRECTION ( 'NONE',  ( 0.6830127018922181881, 0.6830127018922202975, -0.2588190451025214056 ) ) ;
#48683 = ORIENTED_EDGE ( 'NONE', *, *, #113914, .T. ) ;
#48684 = LINE ( 'NONE', #104471, #124898 ) ;
#48685 = PLANE ( 'NONE',  #62834 ) ;
#48686 = EDGE_CURVE ( 'NONE', #26613, #19532, #92726, .T. ) ;
#48687 = CARTESIAN_POINT ( 'NONE',  ( 2.479166666666666963, 6.094999999999988205, -1.633150327867694651 ) ) ;
#48688 = FACE_OUTER_BOUND ( 'NONE', #84844, .T. ) ;
#48689 = DIRECTION ( 'NONE',  ( -1.000000000000000000, -0.000000000000000000, -0.000000000000000000 ) ) ;
#48690 = CARTESIAN_POINT ( 'NONE',  ( -8.292893218813398803, 11.25929247661560062, 5.000000000000000000 ) ) ;
#48691 = CARTESIAN_POINT ( 'NONE',  ( -31.92499999999997584, -7.730000000000015525, 3.180000000000000160 ) ) ;
#48692 = CARTESIAN_POINT ( 'NONE',  ( 34.92499999999998295, -8.143876922607498514, 4.000000000000000000 ) ) ;
#48693 = VERTEX_POINT ( 'NONE', #26069 ) ;
#48694 = EDGE_LOOP ( 'NONE', ( #129640, #31374, #3134, #24622 ) ) ;
#48695 = VERTEX_POINT ( 'NONE', #70331 ) ;
#48696 = VECTOR ( 'NONE', #38953, 999.9999999999998863 ) ;
#48697 = CARTESIAN_POINT ( 'NONE',  ( 123.3541666666666572, -2.130196079827425315, -7.950000000000001066 ) ) ;
#48698 = VECTOR ( 'NONE', #36011, 1000.000000000000000 ) ;
#48699 = VERTEX_POINT ( 'NONE', #73157 ) ;
#48700 = VERTEX_POINT ( 'NONE', #97736 ) ;
#48701 = ORIENTED_EDGE ( 'NONE', *, *, #48238, .T. ) ;
#48702 = CARTESIAN_POINT ( 'NONE',  ( -25.39999999999996305, 0.000000000000000000, 0.000000000000000000 ) ) ;
#48703 = LINE ( 'NONE', #61058, #67146 ) ;
#48704 = VECTOR ( 'NONE', #90932, 1000.000000000000227 ) ;
#48705 = VECTOR ( 'NONE', #66689, 1000.000000000000227 ) ;
#48706 = ORIENTED_EDGE ( 'NONE', *, *, #73020, .T. ) ;
#48707 = DIRECTION ( 'NONE',  ( 0.000000000000000000, 1.000000000000000000, 0.000000000000000000 ) ) ;
#48708 = VECTOR ( 'NONE', #133499, 1000.000000000000000 ) ;
#48709 = LINE ( 'NONE', #103764, #87977 ) ;
#48710 = FACE_OUTER_BOUND ( 'NONE', #98873, .T. ) ;
#48711 = CARTESIAN_POINT ( 'NONE',  ( 117.1045968585647898, 1.637169565754164946, -6.109999999999999432 ) ) ;
#48712 = EDGE_CURVE ( 'NONE', #51714, #94334, #107867, .T. ) ;
#48713 = VERTEX_POINT ( 'NONE', #41205 ) ;
#48714 = CARTESIAN_POINT ( 'NONE',  ( -28.49999999999981171, -20.56887692260760048, 4.000000000000000000 ) ) ;
#48715 = LINE ( 'NONE', #49460, #123323 ) ;
#48716 = ADVANCED_FACE ( 'NONE', ( #128934 ), #141229, .F. ) ;
#48717 = CARTESIAN_POINT ( 'NONE',  ( -30.71757738642547508, -21.73023691814492508, 5.000000000000000888 ) ) ;
#48718 = AXIS2_PLACEMENT_3D ( 'NONE', #77617, #66722, #130563 ) ;
#48719 = CARTESIAN_POINT ( 'NONE',  ( -2.671830600776449405, -21.74070752338406010, 4.000000000000000000 ) ) ;
#48720 = SURFACE_STYLE_FILL_AREA ( #69055 ) ;
#48721 = CARTESIAN_POINT ( 'NONE',  ( -63.48921356237309510, -27.52281430457099631, 5.000000000000000000 ) ) ;
#48722 = DIRECTION ( 'NONE',  ( 0.7071067811865487940, 0.7071067811865463515, 0.000000000000000000 ) ) ;
#48723 = EDGE_CURVE ( 'NONE', #123895, #13745, #19461, .T. ) ;
#48724 = CARTESIAN_POINT ( 'NONE',  ( 34.35002705046288440, -5.819803920172572198, -5.819803920172572198 ) ) ;
#48725 = CARTESIAN_POINT ( 'NONE',  ( -7.140000000000001457, -35.13237070076360169, 17.62370837922860289 ) ) ;
#48726 = DIRECTION ( 'NONE',  ( 0.7071067811865487940, 0.7071067811865463515, -0.000000000000000000 ) ) ;
#48727 = ORIENTED_EDGE ( 'NONE', *, *, #8257, .T. ) ;
#48728 = ORIENTED_EDGE ( 'NONE', *, *, #112526, .T. ) ;
#48729 = CARTESIAN_POINT ( 'NONE',  ( 36.87499999999999289, 7.950000000000000178, 1.460391307983218535E-15 ) ) ;
#48730 = ORIENTED_EDGE ( 'NONE', *, *, #78222, .T. ) ;
#48731 = ORIENTED_EDGE ( 'NONE', *, *, #38317, .F. ) ;
#48732 = EDGE_CURVE ( 'NONE', #108968, #73204, #106426, .T. ) ;
#48733 = PLANE ( 'NONE',  #22824 ) ;
#48734 = VECTOR ( 'NONE', #55132, 1000.000000000000000 ) ;
#48735 = CARTESIAN_POINT ( 'NONE',  ( 2.924914550060625729, -2.500000000000000000, 3.061616997868383634E-16 ) ) ;
#48736 = EDGE_LOOP ( 'NONE', ( #130087, #42317, #67761, #72834 ) ) ;
#48737 = CARTESIAN_POINT ( 'NONE',  ( 12.19999999999999574, -27.55040120718572894, 16.07347811296898854 ) ) ;
#48738 = DIRECTION ( 'NONE',  ( -0.000000000000000000, 0.000000000000000000, 1.000000000000000000 ) ) ;
#48739 = EDGE_CURVE ( 'NONE', #96885, #21343, #31772, .T. ) ;
#48740 = CARTESIAN_POINT ( 'NONE',  ( 20.99999999999985789, -9.033600742197645417, 5.000000000000000000 ) ) ;
#48741 = VECTOR ( 'NONE', #3758, 1000.000000000000000 ) ;
#48742 = VECTOR ( 'NONE', #58288, 1000.000000000000000 ) ;
#48743 = CARTESIAN_POINT ( 'NONE',  ( 26.39626352523143282, 4.472830434245840259, -4.472830434245839371 ) ) ;
#48744 = VERTEX_POINT ( 'NONE', #117322 ) ;
#48745 = CIRCLE ( 'NONE', #120496, 2.500000000000000444 ) ;
#48746 = CARTESIAN_POINT ( 'NONE',  ( -11.99999999999993427, -16.02097659208073566, -11.96015758381206417 ) ) ;
#48747 = ORIENTED_EDGE ( 'NONE', *, *, #72922, .T. ) ;
#48748 = PLANE ( 'NONE',  #75135 ) ;
#48749 = ADVANCED_FACE ( 'NONE', ( #29607 ), #30338, .T. ) ;
#48750 = VECTOR ( 'NONE', #40162, 1000.000000000000227 ) ;
#48751 = DIRECTION ( 'NONE',  ( 0.3543493200069162685, -0.000000000000000000, -0.9351131265310288487 ) ) ;
#48752 = PLANE ( 'NONE',  #78859 ) ;
#48753 = ORIENTED_EDGE ( 'NONE', *, *, #65120, .T. ) ;
#48754 = ORIENTED_EDGE ( 'NONE', *, *, #77919, .F. ) ;
#48755 = LINE ( 'NONE', #126300, #9969 ) ;
#48756 = CARTESIAN_POINT ( 'NONE',  ( 34.92499999999998295, 21.72500000000000142, 4.165035510187005130 ) ) ;
#48757 = CARTESIAN_POINT ( 'NONE',  ( 26.99999999999980815, 12.25461709320623349, -10.07315571508691043 ) ) ;
#48758 = ADVANCED_FACE ( 'NONE', ( #118019 ), #51394, .F. ) ;
#48759 = LINE ( 'NONE', #125614, #32454 ) ;
#48760 = ADVANCED_FACE ( 'NONE', ( #84722 ), #18723, .F. ) ;
#48761 = MECHANICAL_DESIGN_GEOMETRIC_PRESENTATION_REPRESENTATION (  '', ( #34898 ), #58098 ) ;
#48762 = CARTESIAN_POINT ( 'NONE',  ( 44.39126352523143737, -4.472830434245839371, -4.472830434245839371 ) ) ;
#48763 = EDGE_LOOP ( 'NONE', ( #124374, #42838, #139439, #31603 ) ) ;
#48764 = DIRECTION ( 'NONE',  ( -0.7071067811865486830, -0.7071067811865464625, -0.000000000000000000 ) ) ;
#48765 = EDGE_CURVE ( 'NONE', #46218, #33856, #123874, .T. ) ;
#48766 = LINE ( 'NONE', #92969, #117519 ) ;
#48767 = EDGE_LOOP ( 'NONE', ( #47707, #55899, #39126 ) ) ;
#48768 = ORIENTED_EDGE ( 'NONE', *, *, #17937, .F. ) ;
#48769 = AXIS2_PLACEMENT_3D ( 'NONE', #106432, #50667, #139123 ) ;
#48770 = CARTESIAN_POINT ( 'NONE',  ( -31.00193056682077497, -22.22500000000000142, 4.500000000000000888 ) ) ;
#48771 = VERTEX_POINT ( 'NONE', #137658 ) ;
#48772 = EDGE_CURVE ( 'NONE', #103277, #24958, #4931, .T. ) ;
#48773 = EDGE_CURVE ( 'NONE', #27078, #94753, #104267, .T. ) ;
#48774 = DIRECTION ( 'NONE',  ( 0.6830127018922181881, 0.6830127018922202975, -0.2588190451025214056 ) ) ;
#48775 = ORIENTED_EDGE ( 'NONE', *, *, #74636, .T. ) ;
#48776 = LINE ( 'NONE', #92242, #72419 ) ;
#48777 = LINE ( 'NONE', #92983, #73424 ) ;
#48778 = AXIS2_PLACEMENT_3D ( 'NONE', #97085, #107969, #63810 ) ;
#48779 = EDGE_CURVE ( 'NONE', #125681, #105597, #54878, .T. ) ;
#48780 = CARTESIAN_POINT ( 'NONE',  ( 11.81601139373100651, 28.73617430169779041, 5.000000000000000000 ) ) ;
#48781 = FACE_BOUND ( 'NONE', #25738, .T. ) ;
#48782 = EDGE_CURVE ( 'NONE', #34187, #47131, #136923, .T. ) ;
#48783 = CARTESIAN_POINT ( 'NONE',  ( 7.603431928946386087, -14.24070752338413648, 19.24067776001727736 ) ) ;
#48784 = DIRECTION ( 'NONE',  ( -1.000000000000000000, -3.115803279706882722E-16, 0.000000000000000000 ) ) ;
#48785 = CARTESIAN_POINT ( 'NONE',  ( 34.45011844616451668, 10.51628081163738671, 5.000000000000000888 ) ) ;
#48787 = ORIENTED_EDGE ( 'NONE', *, *, #14029, .T. ) ;
#48786 = DIRECTION ( 'NONE',  ( -0.7071067811865487940, 0.7071067811865463515, 0.000000000000000000 ) ) ;
#48788 = VECTOR ( 'NONE', #72820, 1000.000000000000000 ) ;
#48789 = VECTOR ( 'NONE', #105855, 1000.000000000000000 ) ;
#48790 = CARTESIAN_POINT ( 'NONE',  ( 14.99451991528749595, 28.92564299267948513, 4.000000000000000000 ) ) ;
#48791 = VERTEX_POINT ( 'NONE', #37631 ) ;
#48792 = EDGE_LOOP ( 'NONE', ( #27543, #18055, #118043, #19666 ) ) ;
#48793 = CARTESIAN_POINT ( 'NONE',  ( 64.22459685856478018, -1.637169565754160949, 6.109999999999997655 ) ) ;
#48794 = EDGE_LOOP ( 'NONE', ( #83403, #94409, #125553, #11205 ) ) ;
#48795 = ADVANCED_FACE ( 'NONE', ( #70974 ), #128206, .F. ) ;
#48796 = CARTESIAN_POINT ( 'NONE',  ( 8.816011393731004731, 28.73617430169781173, 5.000000000000000000 ) ) ;
#48797 = CYLINDRICAL_SURFACE ( 'NONE', #49644, 0.5000000000000004441 ) ;
#48798 = ORIENTED_EDGE ( 'NONE', *, *, #40194, .T. ) ;
#48799 = PLANE ( 'NONE',  #134764 ) ;
#48801 = EDGE_CURVE ( 'NONE', #138040, #99796, #106388, .T. ) ;
#48800 = VECTOR ( 'NONE', #133049, 1000.000000000000000 ) ;
#48802 = AXIS2_PLACEMENT_3D ( 'NONE', #131872, #87644, #21678 ) ;
#48803 = VECTOR ( 'NONE', #132216, 999.9999999999998863 ) ;
#48804 = CARTESIAN_POINT ( 'NONE',  ( 34.83333333333332860, -6.884901960086287964, 3.974999999999998312 ) ) ;
#48805 = FACE_OUTER_BOUND ( 'NONE', #110090, .T. ) ;
#48806 = FACE_OUTER_BOUND ( 'NONE', #69800, .T. ) ;
#48807 = CARTESIAN_POINT ( 'NONE',  ( -23.99451991528749062, 28.92564299267954908, 4.000000000000000000 ) ) ;
#48808 = SURFACE_STYLE_FILL_AREA ( #16124 ) ;
#48809 = ORIENTED_EDGE ( 'NONE', *, *, #57731, .F. ) ;
#48810 = VECTOR ( 'NONE', #105861, 1000.000000000000000 ) ;
#48811 = AXIS2_PLACEMENT_3D ( 'NONE', #59934, #96096, #128052 ) ;
#48812 = VECTOR ( 'NONE', #84676, 1000.000000000000000 ) ;
#48813 = ORIENTED_EDGE ( 'NONE', *, *, #74258, .F. ) ;
#48814 = VECTOR ( 'NONE', #43863, 1000.000000000000000 ) ;
#48815 = DIRECTION ( 'NONE',  ( 0.7071067811865487940, 0.7071067811865463515, 0.000000000000000000 ) ) ;
#48816 = ORIENTED_EDGE ( 'NONE', *, *, #108630, .F. ) ;
#48817 = VECTOR ( 'NONE', #133693, 1000.000000000000000 ) ;
#48818 = VERTEX_POINT ( 'NONE', #95548 ) ;
#48819 = ORIENTED_EDGE ( 'NONE', *, *, #126081, .T. ) ;
#48820 = DIRECTION ( 'NONE',  ( 0.7071067811865487940, -0.7071067811865463515, 0.000000000000000000 ) ) ;
#48821 = CARTESIAN_POINT ( 'NONE',  ( 29.58333333333332149, 6.884901960086290629, -3.974999999999994316 ) ) ;
#48822 = ORIENTED_EDGE ( 'NONE', *, *, #57480, .F. ) ;
#48823 = VECTOR ( 'NONE', #77456, 1000.000000000000000 ) ;
#48824 = CARTESIAN_POINT ( 'NONE',  ( 9.836528711265433600, 15.75929247661555976, 9.299976744542940210 ) ) ;
#48825 = EDGE_CURVE ( 'NONE', #138000, #78104, #60094, .T. ) ;
#48826 = CARTESIAN_POINT ( 'NONE',  ( 43.10002705046289861, 5.819803920172570422, 5.819803920172575751 ) ) ;
#48827 = CARTESIAN_POINT ( 'NONE',  ( 6.775403141435218934, -2.126176841940958351, -7.934999999999989839 ) ) ;
#48828 = CARTESIAN_POINT ( 'NONE',  ( -3.874853806907633924, -14.24070752338413826, 9.401115078912665624 ) ) ;
#48829 = ORIENTED_EDGE ( 'NONE', *, *, #135002, .F. ) ;
#48830 = VECTOR ( 'NONE', #111705, 1000.000000000000227 ) ;
#48831 = DIRECTION ( 'NONE',  ( -0.000000000000000000, -0.3543493200069152693, 0.9351131265310292928 ) ) ;
#48832 = CARTESIAN_POINT ( 'NONE',  ( -22.49999999999984013, -4.533600742197690714, 5.000000000000000000 ) ) ;
#48833 = CIRCLE ( 'NONE', #9460, 2.055000000000001048 ) ;
#48834 = PLANE ( 'NONE',  #21819 ) ;
#48836 = ORIENTED_EDGE ( 'NONE', *, *, #25662, .T. ) ;
#48835 = FACE_OUTER_BOUND ( 'NONE', #17395, .T. ) ;
#48837 = CARTESIAN_POINT ( 'NONE',  ( 9.591592354503321260, 9.902892378096218942E-16, 0.000000000000000000 ) ) ;
#48838 = ORIENTED_EDGE ( 'NONE', *, *, #51388, .T. ) ;
#48839 = DIRECTION ( 'NONE',  ( 0.000000000000000000, -1.000000000000000000, 0.000000000000000000 ) ) ;
#48840 = CARTESIAN_POINT ( 'NONE',  ( 38.99451991528749062, 28.92564299267965211, 4.000000000000000000 ) ) ;
#48841 = CARTESIAN_POINT ( 'NONE',  ( 4.828169399223503078, 18.75929247661552424, 4.000000000000000000 ) ) ;
#48842 = ORIENTED_EDGE ( 'NONE', *, *, #131571, .F. ) ;
#48843 = VECTOR ( 'NONE', #10406, 1000.000000000000227 ) ;
#48844 = VECTOR ( 'NONE', #95256, 1000.000000000000227 ) ;
#48846 = CARTESIAN_POINT ( 'NONE',  ( 0.000000000000000000, 0.000000000000000000, 5.000000000000000000 ) ) ;
#48845 = VECTOR ( 'NONE', #100073, 999.9999999999998863 ) ;
#48847 = DIRECTION ( 'NONE',  ( 0.7071067811865487940, 0.7071067811865463515, -0.000000000000000000 ) ) ;
#48848 = LINE ( 'NONE', #37243, #74545 ) ;
#48849 = ORIENTED_EDGE ( 'NONE', *, *, #85299, .F. ) ;
#48850 = DIRECTION ( 'NONE',  ( -0.000000000000000000, -0.3543493200069153248, -0.9351131265310291818 ) ) ;
#48851 = CONICAL_SURFACE ( 'NONE', #62721, 2.055000000000001048, 0.9599310885968758145 ) ;
#48852 = LINE ( 'NONE', #93052, #49370 ) ;
#48853 = CARTESIAN_POINT ( 'NONE',  ( 8.066639616203772789, 1.633150327867685103, 6.094999999999992646 ) ) ;
#48854 = CARTESIAN_POINT ( 'NONE',  ( 0.000000000000000000, 0.000000000000000000, 5.000000000000000000 ) ) ;
#48855 = DIRECTION ( 'NONE',  ( 0.7071067811865487940, 0.7071067811865463515, 0.000000000000000000 ) ) ;
#48856 = ORIENTED_EDGE ( 'NONE', *, *, #21860, .F. ) ;
#48857 = AXIS2_PLACEMENT_3D ( 'NONE', #38000, #103913, #82228 ) ;
#48858 = ORIENTED_EDGE ( 'NONE', *, *, #115815, .T. ) ;
#48859 = CARTESIAN_POINT ( 'NONE',  ( 26.43999999999999773, 2.055000000000001492, 2.516649172247811554E-16 ) ) ;
#48860 = CARTESIAN_POINT ( 'NONE',  ( 6.687069808101886892, -2.126176841940956130, 7.934999999999991616 ) ) ;
#48861 = CARTESIAN_POINT ( 'NONE',  ( -34.92500000000001137, -3.183345613589545486, 4.500000000000000888 ) ) ;
#48862 = VECTOR ( 'NONE', #140164, 1000.000000000000000 ) ;
#48863 = CARTESIAN_POINT ( 'NONE',  ( -0.1839886062690032631, 28.73617430169787568, 5.000000000000000000 ) ) ;
#48864 = DIRECTION ( 'NONE',  ( 0.6830127018922181881, 0.6830127018922202975, -0.2588190451025214056 ) ) ;
#48865 = DIRECTION ( 'NONE',  ( -0.7071067811865486830, -0.7071067811865464625, -0.000000000000000000 ) ) ;
#48866 = EDGE_LOOP ( 'NONE', ( #114617, #118246, #9651, #29712 ) ) ;
#48867 = CARTESIAN_POINT ( 'NONE',  ( 21.18398860626899349, 28.73617430169802134, 5.000000000000000000 ) ) ;
#48868 = VECTOR ( 'NONE', #127339, 1000.000000000000000 ) ;
#48869 = LINE ( 'NONE', #3193, #12167 ) ;
#48870 = AXIS2_PLACEMENT_3D ( 'NONE', #31905, #63135, #130523 ) ;
#48871 = LINE ( 'NONE', #25665, #11152 ) ;
#48872 = CARTESIAN_POINT ( 'NONE',  ( 43.95376352523145158, -6.109999999999999432, -3.741295971395163529E-16 ) ) ;
#48873 = PLANE ( 'NONE',  #25543 ) ;
#48874 = VERTEX_POINT ( 'NONE', #92687 ) ;
#48875 = LINE ( 'NONE', #80788, #136689 ) ;
#48876 = ORIENTED_EDGE ( 'NONE', *, *, #25974, .F. ) ;
#48877 = EDGE_CURVE ( 'NONE', #106116, #74581, #105690, .T. ) ;
#48878 = ORIENTED_EDGE ( 'NONE', *, *, #40578, .F. ) ;
#48879 = VECTOR ( 'NONE', #134612, 1000.000000000000227 ) ;
#48880 = LINE ( 'NONE', #83669, #47885 ) ;
#48881 = CARTESIAN_POINT ( 'NONE',  ( -18.18398860626898994, 28.73617430169800002, 5.000000000000000000 ) ) ;
#48882 = CARTESIAN_POINT ( 'NONE',  ( 25.39999999999999858, 7.464222240803104598E-16, -6.094999999999989093 ) ) ;
#48883 = EDGE_CURVE ( 'NONE', #24156, #48700, #115129, .T. ) ;
#48884 = DIRECTION ( 'NONE',  ( 0.7071067811865487940, -0.7071067811865463515, 0.000000000000000000 ) ) ;
#48885 = DIRECTION ( 'NONE',  ( -0.000000000000000000, 0.000000000000000000, 1.000000000000000000 ) ) ;
#48886 = EDGE_CURVE ( 'NONE', #84890, #42322, #4193, .T. ) ;
#48887 = EDGE_CURVE ( 'NONE', #133571, #30937, #115846, .T. ) ;
#48888 = EDGE_LOOP ( 'NONE', ( #127696, #42435, #105177, #86595 ) ) ;
#48889 = DIRECTION ( 'NONE',  ( -1.000000000000000000, -0.000000000000000000, -0.000000000000000000 ) ) ;
#48890 = CARTESIAN_POINT ( 'NONE',  ( -13.82816939922342492, 18.75929247661553489, 4.000000000000000000 ) ) ;
#48891 = UNCERTAINTY_MEASURE_WITH_UNIT (LENGTH_MEASURE( 1.000000000000000082E-05 ), #35470, 'distance_accuracy_value', 'NONE');
#48892 = CIRCLE ( 'NONE', #129901, 2.500000000000000888 ) ;
#48893 = DIRECTION ( 'NONE',  ( -0.000000000000000000, 0.000000000000000000, 1.000000000000000000 ) ) ;
#48894 = FACE_OUTER_BOUND ( 'NONE', #3449, .T. ) ;
#48895 = CARTESIAN_POINT ( 'NONE',  ( 6.628407645496676714, 9.139736423841732040E-16, 0.000000000000000000 ) ) ;
#48896 = EDGE_CURVE ( 'NONE', #22343, #40695, #127470, .T. ) ;
#48898 = EDGE_CURVE ( 'NONE', #37768, #109138, #39782, .T. ) ;
#48897 = CARTESIAN_POINT ( 'NONE',  ( 69.05836038379621300, -7.949999999999997513, -2.130196079827425759 ) ) ;
#48899 = LINE ( 'NONE', #93103, #36921 ) ;
#48900 = ORIENTED_EDGE ( 'NONE', *, *, #76566, .F. ) ;
#48901 = ORIENTED_EDGE ( 'NONE', *, *, #121425, .F. ) ;
#48902 = CARTESIAN_POINT ( 'NONE',  ( 68.37499999999998579, 7.950000000000000178, 1.460391307983218535E-15 ) ) ;
#48903 = PLANE ( 'NONE',  #132711 ) ;
#48904 = EDGE_CURVE ( 'NONE', #90251, #138592, #57966, .T. ) ;
#48905 = PLANE ( 'NONE',  #115650 ) ;
#48906 = DIRECTION ( 'NONE',  ( 1.000000000000000000, 0.000000000000000000, 0.000000000000000000 ) ) ;
#48907 = ORIENTED_EDGE ( 'NONE', *, *, #74431, .F. ) ;
#48908 = CONICAL_SURFACE ( 'NONE', #127536, 2.055000000000001048, 0.9599310885968758145 ) ;
#48909 = CARTESIAN_POINT ( 'NONE',  ( 33.22916666666665719, 7.950000000000001954, -2.130196079827421762 ) ) ;
#48910 = VECTOR ( 'NONE', #41656, 999.9999999999998863 ) ;
#48911 = EDGE_CURVE ( 'NONE', #47009, #29818, #116597, .T. ) ;
#48912 = AXIS2_PLACEMENT_3D ( 'NONE', #28076, #61459, #138266 ) ;
#48913 = CARTESIAN_POINT ( 'NONE',  ( 6.938893903907228378E-15, 5.587461875839191627, 4.000000000000000000 ) ) ;
#48914 = CARTESIAN_POINT ( 'NONE',  ( 55.85459685856475431, -1.637169565754161615, 6.110000000000000320 ) ) ;
#48915 = FACE_OUTER_BOUND ( 'NONE', #29157, .T. ) ;
#48916 = ORIENTED_EDGE ( 'NONE', *, *, #30250, .F. ) ;
#48918 = ORIENTED_EDGE ( 'NONE', *, *, #104030, .F. ) ;
#48917 = AXIS2_PLACEMENT_3D ( 'NONE', #107998, #29735, #119592 ) ;
#48919 = AXIS2_PLACEMENT_3D ( 'NONE', #85058, #110356, #11032 ) ;
#48920 = VECTOR ( 'NONE', #83454, 1000.000000000000000 ) ;
#48921 = AXIS2_PLACEMENT_3D ( 'NONE', #71757, #41233, #17344 ) ;
#48922 = CARTESIAN_POINT ( 'NONE',  ( 11.51078643762690490, -27.52281430457047406, 5.000000000000000000 ) ) ;
#48923 = DIRECTION ( 'NONE',  ( 0.7071067811865486830, -0.7071067811865464625, -0.000000000000000000 ) ) ;
#48924 = CARTESIAN_POINT ( 'NONE',  ( 26.12840764549667583, 9.139736423841732040E-16, 0.000000000000000000 ) ) ;
#48925 = LINE ( 'NONE', #93128, #34984 ) ;
#48927 = ORIENTED_EDGE ( 'NONE', *, *, #120926, .T. ) ;
#48926 = DIRECTION ( 'NONE',  ( 0.7071067811865486830, -0.7071067811865464625, -0.000000000000000000 ) ) ;
#48928 = DIRECTION ( 'NONE',  ( 0.000000000000000000, 0.000000000000000000, 1.000000000000000000 ) ) ;
#48929 = CARTESIAN_POINT ( 'NONE',  ( -20.81601139373100295, 28.73617430169773002, 5.000000000000000000 ) ) ;
#48930 = LINE ( 'NONE', #82977, #33287 ) ;
#48931 = AXIS2_PLACEMENT_3D ( 'NONE', #74969, #75662, #108966 ) ;
#48932 = EDGE_CURVE ( 'NONE', #75514, #110346, #76694, .T. ) ;
#48933 = ORIENTED_EDGE ( 'NONE', *, *, #132574, .T. ) ;
#48934 = ORIENTED_EDGE ( 'NONE', *, *, #101446, .F. ) ;
#48935 = VECTOR ( 'NONE', #71428, 1000.000000000000114 ) ;
#48936 = FACE_OUTER_BOUND ( 'NONE', #49292, .T. ) ;
#48937 = CARTESIAN_POINT ( 'NONE',  ( 14.99451991528749595, 28.92564299267948513, 4.000000000000000000 ) ) ;
#48938 = EDGE_CURVE ( 'NONE', #84739, #105871, #75951, .T. ) ;
#48939 = FACE_OUTER_BOUND ( 'NONE', #120152, .T. ) ;
#48940 = CARTESIAN_POINT ( 'NONE',  ( 72.70419371712955581, -6.884901960086285300, -3.975000000000000089 ) ) ;
#48941 = EDGE_LOOP ( 'NONE', ( #123439, #117648, #10632, #25356 ) ) ;
#48942 = ORIENTED_EDGE ( 'NONE', *, *, #80247, .F. ) ;
#48943 = CARTESIAN_POINT ( 'NONE',  ( 17.81601139373099940, 28.73617430169775133, 5.000000000000000000 ) ) ;
#48944 = CARTESIAN_POINT ( 'NONE',  ( 16.76840764549667639, 9.139736423841732040E-16, 0.000000000000000000 ) ) ;
#48945 = AXIS2_PLACEMENT_3D ( 'NONE', #75696, #79306, #45237 ) ;
#48946 = EDGE_CURVE ( 'NONE', #106292, #43835, #32453, .T. ) ;
#48947 = ORIENTED_EDGE ( 'NONE', *, *, #23256, .T. ) ;
#48948 = VECTOR ( 'NONE', #23033, 1000.000000000000000 ) ;
#48950 = EDGE_CURVE ( 'NONE', #49613, #9752, #107137, .T. ) ;
#48949 = EDGE_LOOP ( 'NONE', ( #118290, #50161, #100569, #103047, #84961, #126722 ) ) ;
#48951 = AXIS2_PLACEMENT_3D ( 'NONE', #77365, #98373, #133159 ) ;
#48952 = LINE ( 'NONE', #82297, #52537 ) ;
#48953 = FACE_OUTER_BOUND ( 'NONE', #116648, .T. ) ;
#48954 = AXIS2_PLACEMENT_3D ( 'NONE', #36064, #136064, #1933 ) ;
#48955 = EDGE_CURVE ( 'NONE', #108205, #14902, #131049, .T. ) ;
#48956 = FACE_BOUND ( 'NONE', #135735, .T. ) ;
#48957 = VECTOR ( 'NONE', #69755, 1000.000000000000227 ) ;
#48958 = DIRECTION ( 'NONE',  ( -0.000000000000000000, 0.000000000000000000, 1.000000000000000000 ) ) ;
#48959 = CARTESIAN_POINT ( 'NONE',  ( -34.92500000000001137, -3.425372908132398475, 14.71988515618267357 ) ) ;
#48960 = CARTESIAN_POINT ( 'NONE',  ( -18.48921356237309510, -27.52281430457068367, 5.000000000000000000 ) ) ;
#48961 = PLANE ( 'NONE',  #73656 ) ;
#48962 = EDGE_CURVE ( 'NONE', #112402, #105677, #9967, .T. ) ;
#48963 = CARTESIAN_POINT ( 'NONE',  ( -60.18398860626900415, 28.73617430169829490, 5.000000000000000000 ) ) ;
#48964 = SHAPE_DEFINITION_REPRESENTATION ( #77995, #69070 ) ;
#48965 = ORIENTED_EDGE ( 'NONE', *, *, #38682, .T. ) ;
#48966 = ORIENTED_EDGE ( 'NONE', *, *, #89146, .T. ) ;
#48967 = CARTESIAN_POINT ( 'NONE',  ( 98.49543019189812298, 5.291415217122916737, 3.055000000000001936 ) ) ;
#48968 = VERTEX_POINT ( 'NONE', #54236 ) ;
#48969 = EDGE_CURVE ( 'NONE', #104746, #103339, #37127, .T. ) ;
#48970 = DIRECTION ( 'NONE',  ( 1.734723475976806848E-16, -1.000000000000000000, 0.000000000000000000 ) ) ;
#48971 =( GEOMETRIC_REPRESENTATION_CONTEXT ( 3 ) GLOBAL_UNCERTAINTY_ASSIGNED_CONTEXT ( ( #39050 ) ) GLOBAL_UNIT_ASSIGNED_CONTEXT ( ( #19662, #7335, #107382 ) ) REPRESENTATION_CONTEXT ( 'NONE', 'WORKASPACE' ) );
#48972 = CARTESIAN_POINT ( 'NONE',  ( 30.48921356237309510, -27.52281430457076894, 5.000000000000000000 ) ) ;
#48973 = DIRECTION ( 'NONE',  ( -0.7071067811865487940, 0.7071067811865463515, 0.000000000000000000 ) ) ;
#48974 = DIRECTION ( 'NONE',  ( -0.000000000000000000, -0.3543493200069153248, -0.9351131265310291818 ) ) ;
#48975 = EDGE_LOOP ( 'NONE', ( #98345, #12061, #69951, #55153 ) ) ;
#48976 = CARTESIAN_POINT ( 'NONE',  ( 33.83652871126528794, 15.75929247661555443, 9.299976744542998830 ) ) ;
#48977 = DIRECTION ( 'NONE',  ( -1.000000000000000000, -0.000000000000000000, -0.000000000000000000 ) ) ;
#48978 = DIRECTION ( 'NONE',  ( 0.7071067811865487940, 0.7071067811865463515, -0.000000000000000000 ) ) ;
#48980 = CARTESIAN_POINT ( 'NONE',  ( 18.29974487139159223, -27.71228299555219010, 4.000000000000000000 ) ) ;
#48979 = CARTESIAN_POINT ( 'NONE',  ( -8.292893218813398803, 2.259292476615692546, 5.000000000000000000 ) ) ;
#48981 = CARTESIAN_POINT ( 'NONE',  ( -11.99999999999992006, 5.587461875839191627, 4.000000000000000000 ) ) ;
#48982 = VECTOR ( 'NONE', #51884, 1000.000000000000000 ) ;
#48983 = CARTESIAN_POINT ( 'NONE',  ( -26.99999999999981171, -22.06887692260758982, 4.000000000000000000 ) ) ;
#48984 = ORIENTED_EDGE ( 'NONE', *, *, #51783, .T. ) ;
#48985 = DIRECTION ( 'NONE',  ( 0.6830127018922181881, 0.6830127018922202975, -0.2588190451025214056 ) ) ;
#48986 = CARTESIAN_POINT ( 'NONE',  ( -5.816011393731002066, 28.73617430169783304, 5.000000000000000000 ) ) ;
#48987 = ORIENTED_EDGE ( 'NONE', *, *, #56983, .T. ) ;
#48988 = ADVANCED_FACE ( 'NONE', ( #140480 ), #141188, .F. ) ;
#48989 = ORIENTED_EDGE ( 'NONE', *, *, #15685, .F. ) ;
#48990 = ORIENTED_EDGE ( 'NONE', *, *, #21382, .F. ) ;
#48991 = CARTESIAN_POINT ( 'NONE',  ( 42.14626352523143993, -4.472830434245840259, 4.472830434245838482 ) ) ;
#48992 = ORIENTED_EDGE ( 'NONE', *, *, #104573, .F. ) ;
#48993 = ADVANCED_FACE ( 'NONE', ( #98420 ), #131768, .F. ) ;
#48994 = CARTESIAN_POINT ( 'NONE',  ( 12.14997294953710849, -4.461849672132299105, 4.461849672132299993 ) ) ;
#48995 = CARTESIAN_POINT ( 'NONE',  ( -13.33265045070550237, 6.437115738644505925, -28.78119739759756968 ) ) ;
#48996 = ORIENTED_EDGE ( 'NONE', *, *, #106370, .T. ) ;
#48997 = LINE ( 'NONE', #102669, #27112 ) ;
#48998 = ORIENTED_EDGE ( 'NONE', *, *, #108330, .T. ) ;
#48999 = PLANE ( 'NONE',  #39617 ) ;
#49000 = CARTESIAN_POINT ( 'NONE',  ( 18.79653912142945060, 2.499999999999998224, 3.061616997868380183E-16 ) ) ;
#49001 = VECTOR ( 'NONE', #106217, 999.9999999999998863 ) ;
#49002 = VECTOR ( 'NONE', #50612, 999.9999999999998863 ) ;
#49004 = VERTEX_POINT ( 'NONE', #107834 ) ;
#49003 = CARTESIAN_POINT ( 'NONE',  ( -12.08491323193754141, -12.74070752338414891, 18.74364270924351317 ) ) ;
#49005 = ORIENTED_EDGE ( 'NONE', *, *, #79583, .F. ) ;
#49006 = EDGE_CURVE ( 'NONE', #81784, #93258, #132515, .T. ) ;
#49007 = FACE_OUTER_BOUND ( 'NONE', #57773, .T. ) ;
#49008 = FACE_OUTER_BOUND ( 'NONE', #62960, .T. ) ;
#49009 = AXIS2_PLACEMENT_3D ( 'NONE', #40789, #84991, #129193 ) ;
#49011 = VERTEX_POINT ( 'NONE', #41170 ) ;
#49010 = AXIS2_PLACEMENT_3D ( 'NONE', #142391, #75005, #130079 ) ;
#49012 = EDGE_CURVE ( 'NONE', #109349, #129328, #125193, .T. ) ;
#49013 = DIRECTION ( 'NONE',  ( -0.000000000000000000, 0.3543493200069153248, 0.9351131265310292928 ) ) ;
#49014 = ORIENTED_EDGE ( 'NONE', *, *, #124383, .T. ) ;
#49015 = VERTEX_POINT ( 'NONE', #54926 ) ;
#49016 = ORIENTED_EDGE ( 'NONE', *, *, #114527, .F. ) ;
#49017 = EDGE_LOOP ( 'NONE', ( #29624, #27190, #137940, #46637, #131158 ) ) ;
#49018 = CARTESIAN_POINT ( 'NONE',  ( -17.99999999999986855, -6.108550654416975867, -3.114665004255009695 ) ) ;
#49019 = VECTOR ( 'NONE', #99092, 999.9999999999998863 ) ;
#49020 = AXIS2_PLACEMENT_3D ( 'NONE', #109666, #10340, #54594 ) ;
#49021 = VECTOR ( 'NONE', #71695, 1000.000000000000000 ) ;
#49022 = VECTOR ( 'NONE', #56463, 1000.000000000000000 ) ;
#49023 = VECTOR ( 'NONE', #84609, 1000.000000000000000 ) ;
#49024 = LINE ( 'NONE', #71477, #51530 ) ;
#49025 = DIRECTION ( 'NONE',  ( -0.000000000000000000, 0.000000000000000000, 1.000000000000000000 ) ) ;
#49026 = CARTESIAN_POINT ( 'NONE',  ( 29.99999999999979039, 13.55218569542902429, 5.000000000000000000 ) ) ;
#49027 = ADVANCED_FACE ( 'NONE', ( #65834 ), #75262, .F. ) ;
#49028 = DIRECTION ( 'NONE',  ( -0.7071067811865486830, -0.7071067811865464625, 0.000000000000000000 ) ) ;
#49029 = EDGE_LOOP ( 'NONE', ( #17349, #114942, #68398, #65377 ) ) ;
#49030 = DIRECTION ( 'NONE',  ( 0.7071067811865487940, 0.7071067811865463515, -0.000000000000000000 ) ) ;
#49031 = CARTESIAN_POINT ( 'NONE',  ( 18.49956980810188867, -3.967499999999998028, -6.871911579029511330 ) ) ;
#49032 = FACE_OUTER_BOUND ( 'NONE', #131658, .T. ) ;
#49033 = CARTESIAN_POINT ( 'NONE',  ( 19.58200623001875940, 3.821174125832445049E-16, 0.000000000000000000 ) ) ;
#49034 = FACE_OUTER_BOUND ( 'NONE', #109127, .T. ) ;
#49035 = ORIENTED_EDGE ( 'NONE', *, *, #83712, .F. ) ;
#49036 = ORIENTED_EDGE ( 'NONE', *, *, #105482, .F. ) ;
#49037 = ORIENTED_EDGE ( 'NONE', *, *, #40780, .F. ) ;
#49038 = DIRECTION ( 'NONE',  ( 1.000000000000000000, 0.000000000000000000, 0.000000000000000000 ) ) ;
#49039 = CARTESIAN_POINT ( 'NONE',  ( 95.89169371712955581, 2.130196079827421762, 7.950000000000000178 ) ) ;
#49040 = UNCERTAINTY_MEASURE_WITH_UNIT (LENGTH_MEASURE( 1.000000000000000082E-05 ), #95115, 'distance_accuracy_value', 'NONE');
#49041 = DIRECTION ( 'NONE',  ( -0.7071067811865487940, 0.7071067811865463515, -0.000000000000000000 ) ) ;
#49042 = CARTESIAN_POINT ( 'NONE',  ( -34.92500000000001137, 21.72500000000000142, 5.000000000000000000 ) ) ;
#49043 = CARTESIAN_POINT ( 'NONE',  ( -27.79289321881326558, 12.75929247661558996, 5.000000000000000000 ) ) ;
#49044 = CARTESIAN_POINT ( 'NONE',  ( 72.24543019189810877, -5.291415217122919401, -3.055000000000000604 ) ) ;
#49045 = VECTOR ( 'NONE', #110958, 1000.000000000000000 ) ;
#49046 = LINE ( 'NONE', #103381, #51016 ) ;
#49047 = VECTOR ( 'NONE', #66419, 1000.000000000000227 ) ;
#49048 = CARTESIAN_POINT ( 'NONE',  ( 0.000000000000000000, 0.000000000000000000, 0.000000000000000000 ) ) ;
#49049 = DIRECTION ( 'NONE',  ( 0.7071067811865487940, 0.7071067811865463515, 0.000000000000000000 ) ) ;
#49050 = CARTESIAN_POINT ( 'NONE',  ( -48.18398860626899705, 28.73617430169820608, 5.000000000000000000 ) ) ;
#49051 = CIRCLE ( 'NONE', #86085, 2.500000000000000888 ) ;
#49052 = CARTESIAN_POINT ( 'NONE',  ( 5.241399257802002332, 21.72500000000000853, 5.000000000000000000 ) ) ;
#49053 = EDGE_LOOP ( 'NONE', ( #104049, #45146, #4872, #119186 ) ) ;
#49055 = AXIS2_PLACEMENT_3D ( 'NONE', #128429, #61757, #42858 ) ;
#49054 = LINE ( 'NONE', #84541, #89304 ) ;
#49056 = ORIENTED_EDGE ( 'NONE', *, *, #20723, .T. ) ;
#49057 = DIRECTION ( 'NONE',  ( -0.7071067811865486830, -0.7071067811865464625, -0.000000000000000000 ) ) ;
#49059 = EDGE_LOOP ( 'NONE', ( #6241, #36303, #24628, #2088 ) ) ;
#49058 = CARTESIAN_POINT ( 'NONE',  ( -19.77325839282154263, -11.24070752338416845, 18.24660765846978094 ) ) ;
#49060 = DIRECTION ( 'NONE',  ( 1.000000000000000000, 0.000000000000000000, 0.000000000000000000 ) ) ;
#49061 = DIRECTION ( 'NONE',  ( 0.3543493200069162685, -0.000000000000000000, -0.9351131265310288487 ) ) ;
#49063 = ADVANCED_FACE ( 'NONE', ( #33200 ), #52750, .T. ) ;
#49062 = EDGE_CURVE ( 'NONE', #71184, #140269, #30302, .T. ) ;
#49064 = VERTEX_POINT ( 'NONE', #65098 ) ;
#49065 = DIRECTION ( 'NONE',  ( -0.7071067811865486830, 0.7071067811865464625, 0.000000000000000000 ) ) ;
#49066 = EDGE_LOOP ( 'NONE', ( #119730, #77229, #50069, #13595, #47799 ) ) ;
#49067 = DIRECTION ( 'NONE',  ( 0.7071067811865486830, -0.7071067811865464625, -0.000000000000000000 ) ) ;
#49068 = UNCERTAINTY_MEASURE_WITH_UNIT (LENGTH_MEASURE( 1.000000000000000082E-05 ), #46955, 'distance_accuracy_value', 'NONE');
#49069 = ORIENTED_EDGE ( 'NONE', *, *, #14565, .T. ) ;
#49070 = STYLED_ITEM ( 'NONE', ( #105300 ), #25816 ) ;
#49071 = CARTESIAN_POINT ( 'NONE',  ( 5.282422613574296655, -21.73023691814493930, 5.000000000000000888 ) ) ;
#49072 = ADVANCED_FACE ( 'NONE', ( #52062 ), #64362, .F. ) ;
#49074 = EDGE_CURVE ( 'NONE', #79378, #99520, #31036, .T. ) ;
#49073 = CARTESIAN_POINT ( 'NONE',  ( 91.51669371712957002, 7.950000000000001066, -2.130196079827421318 ) ) ;
#49075 = DIRECTION ( 'NONE',  ( 0.7071067811865487940, 0.7071067811865463515, 0.000000000000000000 ) ) ;
#49076 = CARTESIAN_POINT ( 'NONE',  ( 5.691592354503320905, -2.500000000000000444, 3.061616997868384620E-16 ) ) ;
#49078 = EDGE_CURVE ( 'NONE', #35299, #92701, #53490, .T. ) ;
#49077 = ORIENTED_EDGE ( 'NONE', *, *, #124828, .F. ) ;
#49079 = DIRECTION ( 'NONE',  ( -0.6830127018922181881, 0.6830127018922202975, -0.2588190451025214056 ) ) ;
#49080 = EDGE_CURVE ( 'NONE', #49508, #68079, #1902, .T. ) ;
#49081 = FACE_OUTER_BOUND ( 'NONE', #145, .T. ) ;
#49083 = AXIS2_PLACEMENT_3D ( 'NONE', #115029, #37527, #90466 ) ;
#49082 = CARTESIAN_POINT ( 'NONE',  ( 28.00000000000000355, 0.000000000000000000, 6.094999999999989981 ) ) ;
#49084 = SURFACE_SIDE_STYLE ('',( #8873 ) ) ;
#49085 = DIRECTION ( 'NONE',  ( -0.000000000000000000, 0.3543493200069153248, 0.9351131265310292928 ) ) ;
#49086 = EDGE_CURVE ( 'NONE', #55674, #117002, #48833, .T. ) ;
#49087 = ORIENTED_EDGE ( 'NONE', *, *, #110763, .F. ) ;
#49088 = LINE ( 'NONE', #124481, #44484 ) ;
#49090 = VERTEX_POINT ( 'NONE', #46946 ) ;
#49089 = EDGE_CURVE ( 'NONE', #73688, #20599, #79575, .T. ) ;
#49091 = CARTESIAN_POINT ( 'NONE',  ( 84.87543019189810423, -5.291415217122920289, -3.055000000000001492 ) ) ;
#49092 = CARTESIAN_POINT ( 'NONE',  ( -21.18398860626899349, 28.73617430169802134, 5.000000000000000000 ) ) ;
#49094 = CONICAL_SURFACE ( 'NONE', #125446, 2.500000000000000888, 0.9599310885968822538 ) ;
#49093 = LINE ( 'NONE', #49815, #90935 ) ;
#49095 = DIRECTION ( 'NONE',  ( -0.7071067811865486830, 0.7071067811865464625, 0.000000000000000000 ) ) ;
#49096 = ORIENTED_EDGE ( 'NONE', *, *, #81629, .T. ) ;
#49097 = DIRECTION ( 'NONE',  ( -0.7071067811865487940, 0.7071067811865463515, -0.000000000000000000 ) ) ;
#49098 = ADVANCED_FACE ( 'NONE', ( #57797 ), #23708, .F. ) ;
#49099 = PLANE ( 'NONE',  #125284 ) ;
#49100 = CARTESIAN_POINT ( 'NONE',  ( 25.39999999999999858, 0.000000000000000000, 6.094999999999989093 ) ) ;
#49101 = CARTESIAN_POINT ( 'NONE',  ( -54.18398860626899705, 28.73617430169825226, 5.000000000000000000 ) ) ;
#49103 = ORIENTED_EDGE ( 'NONE', *, *, #6187, .T. ) ;
#49102 = DIRECTION ( 'NONE',  ( 0.7071067811865487940, -0.7071067811865463515, 0.000000000000000000 ) ) ;
#49104 = CARTESIAN_POINT ( 'NONE',  ( -15.29974487139158867, -27.71228299555216879, 4.000000000000000000 ) ) ;
#49105 = CARTESIAN_POINT ( 'NONE',  ( 20.99999999999985079, 9.631307414974342507, -9.079085613539490396 ) ) ;
#49106 =( GEOMETRIC_REPRESENTATION_CONTEXT ( 3 ) GLOBAL_UNCERTAINTY_ASSIGNED_CONTEXT ( ( #99673 ) ) GLOBAL_UNIT_ASSIGNED_CONTEXT ( ( #104116, #42311, #60698 ) ) REPRESENTATION_CONTEXT ( 'NONE', 'WORKASPACE' ) );
#49107 =( LENGTH_UNIT ( ) NAMED_UNIT ( * ) SI_UNIT ( .MILLI., .METRE. ) );
#49108 = EDGE_CURVE ( 'NONE', #87414, #103176, #36039, .T. ) ;
#49109 = FILL_AREA_STYLE_COLOUR ( '', #130286 ) ;
#49110 = ORIENTED_EDGE ( 'NONE', *, *, #125128, .T. ) ;
#49111 = VERTEX_POINT ( 'NONE', #88987 ) ;
#49112 = ORIENTED_EDGE ( 'NONE', *, *, #99993, .F. ) ;
#49113 = CARTESIAN_POINT ( 'NONE',  ( 80.50043019189810423, -3.055000000000002380, 5.291415217122920289 ) ) ;
#49114 = EDGE_LOOP ( 'NONE', ( #98127, #106171, #72461, #2914 ) ) ;
#49115 =( NAMED_UNIT ( * ) SI_UNIT ( $, .STERADIAN. ) SOLID_ANGLE_UNIT ( ) );
#49116 = DIRECTION ( 'NONE',  ( 0.000000000000000000, 0.000000000000000000, -1.000000000000000000 ) ) ;
#49117 = CARTESIAN_POINT ( 'NONE',  ( 13.64840764549667540, 9.139736423841732040E-16, 0.000000000000000000 ) ) ;
#49118 = CARTESIAN_POINT ( 'NONE',  ( -12.79289321881337216, 12.75929247661558463, 5.000000000000000000 ) ) ;
#49119 = VERTEX_POINT ( 'NONE', #11360 ) ;
#49120 = AXIS2_PLACEMENT_3D ( 'NONE', #24734, #114587, #134965 ) ;
#49121 = VECTOR ( 'NONE', #56644, 1000.000000000000000 ) ;
#49122 = FACE_OUTER_BOUND ( 'NONE', #13416, .T. ) ;
#49123 = CARTESIAN_POINT ( 'NONE',  ( 30.48921356237309510, -27.52281430457076894, 5.000000000000000000 ) ) ;
#49124 = VECTOR ( 'NONE', #4154, 1000.000000000000000 ) ;
#49125 = VECTOR ( 'NONE', #94400, 1000.000000000000227 ) ;
#49126 = ORIENTED_EDGE ( 'NONE', *, *, #135087, .F. ) ;
#49127 = CARTESIAN_POINT ( 'NONE',  ( 24.51665438641027350, 22.22500000000000142, 4.500000000000000888 ) ) ;
#49128 = EDGE_CURVE ( 'NONE', #121024, #40245, #14257, .T. ) ;
#49130 = CARTESIAN_POINT ( 'NONE',  ( 11.99451991528749417, 28.92564299267946382, 4.000000000000000000 ) ) ;
#49129 = VECTOR ( 'NONE', #85975, 1000.000000000000000 ) ;
#49131 = LINE ( 'NONE', #139715, #16886 ) ;
#49132 = VECTOR ( 'NONE', #4768, 1000.000000000000000 ) ;
#49133 = EDGE_CURVE ( 'NONE', #18399, #12755, #91809, .T. ) ;
#49134 = ORIENTED_EDGE ( 'NONE', *, *, #107557, .F. ) ;
#49135 = VERTEX_POINT ( 'NONE', #136034 ) ;
#49136 = DIRECTION ( 'NONE',  ( -0.3543493200069163240, -0.000000000000000000, -0.9351131265310288487 ) ) ;
#49137 = CARTESIAN_POINT ( 'NONE',  ( 34.92499999999998295, 12.75929247661558996, 4.255531930566172072 ) ) ;
#49138 = DIRECTION ( 'NONE',  ( 0.6830127018922180770, -0.6830127018922204085, -0.2588190451025213501 ) ) ;
#49139 = DIRECTION ( 'NONE',  ( -0.7071067811865487940, 0.7071067811865463515, 0.000000000000000000 ) ) ;
#49140 = DIRECTION ( 'NONE',  ( -0.3543493200069162685, -0.000000000000000000, -0.9351131265310288487 ) ) ;
#49141 = ADVANCED_FACE ( 'NONE', ( #113556 ), #13516, .T. ) ;
#49142 = LINE ( 'NONE', #117722, #111412 ) ;
#49143 = CARTESIAN_POINT ( 'NONE',  ( 16.35824297541129368, 15.75929247661555088, 19.34181609438695659 ) ) ;
#49144 = ORIENTED_EDGE ( 'NONE', *, *, #96802, .F. ) ;
#49145 = VERTEX_POINT ( 'NONE', #124447 ) ;
#49146 = VERTEX_POINT ( 'NONE', #133212 ) ;
#49147 = EDGE_CURVE ( 'NONE', #74780, #6489, #22954, .T. ) ;
#49148 = VERTEX_POINT ( 'NONE', #111420 ) ;
#49149 = VECTOR ( 'NONE', #444, 1000.000000000000227 ) ;
#49150 = AXIS2_PLACEMENT_3D ( 'NONE', #33465, #13076, #770 ) ;
#49151 = ORIENTED_EDGE ( 'NONE', *, *, #85407, .F. ) ;
#49152 = DIRECTION ( 'NONE',  ( -1.000000000000000000, -0.000000000000000000, -0.000000000000000000 ) ) ;
#49153 = EDGE_CURVE ( 'NONE', #96833, #94758, #69376, .T. ) ;
#49154 = VECTOR ( 'NONE', #54375, 1000.000000000000000 ) ;
#49155 = DIRECTION ( 'NONE',  ( -0.7071067811865486830, -0.7071067811865464625, -0.000000000000000000 ) ) ;
#49156 = DIRECTION ( 'NONE',  ( -0.7071067811865486830, -0.7071067811865464625, -0.000000000000000000 ) ) ;
#49157 = VECTOR ( 'NONE', #141998, 999.9999999999998863 ) ;
#49158 = CARTESIAN_POINT ( 'NONE',  ( 27.00000000000001421, -7.438727695536411666, -2.045697879312136980 ) ) ;
#49159 = VERTEX_POINT ( 'NONE', #112164 ) ;
#49160 = DIRECTION ( 'NONE',  ( -0.3543493200069162685, -0.000000000000000000, -0.9351131265310288487 ) ) ;
#49161 = CARTESIAN_POINT ( 'NONE',  ( 8.999999999999934275, -15.03360074219758502, 5.000000000000000000 ) ) ;
#49162 = ORIENTED_EDGE ( 'NONE', *, *, #130775, .T. ) ;
#49164 = EDGE_CURVE ( 'NONE', #75310, #74997, #78105, .T. ) ;
#49163 = LINE ( 'NONE', #138297, #4049 ) ;
#49165 = ORIENTED_EDGE ( 'NONE', *, *, #34285, .F. ) ;
#49166 = ORIENTED_EDGE ( 'NONE', *, *, #12907, .T. ) ;
#49167 = DIRECTION ( 'NONE',  ( 2.781805975412905274E-17, -0.3543493200069152138, 0.9351131265310292928 ) ) ;
#49168 = EDGE_LOOP ( 'NONE', ( #79003, #13858, #86503, #138143 ) ) ;
#49169 = EDGE_LOOP ( 'NONE', ( #15091, #135910, #108848 ) ) ;
#49170 = CARTESIAN_POINT ( 'NONE',  ( 72.91709685856477563, 3.054999999999998828, 5.291415217122922066 ) ) ;
#49171 = AXIS2_PLACEMENT_3D ( 'NONE', #8787, #86427, #30621 ) ;
#49172 = VERTEX_POINT ( 'NONE', #121579 ) ;
#49173 = LINE ( 'NONE', #60044, #21088 ) ;
#49174 = ADVANCED_FACE ( 'NONE', ( #89675 ), #34593, .T. ) ;
#49175 = LINE ( 'NONE', #73756, #24210 ) ;
#49176 = CARTESIAN_POINT ( 'NONE',  ( 108.0629301918980900, 1.637169565754157174, 6.110000000000002984 ) ) ;
#49177 = LINE ( 'NONE', #38285, #105063 ) ;
#49178 = LINE ( 'NONE', #4148, #115363 ) ;
#49180 = CARTESIAN_POINT ( 'NONE',  ( 40.60343192894618625, -14.24070752338413293, 19.24067776001735197 ) ) ;
#49179 = VECTOR ( 'NONE', #85116, 1000.000000000000227 ) ;
#49181 = DIRECTION ( 'NONE',  ( -0.7071067811865486830, -0.7071067811865464625, -0.000000000000000000 ) ) ;
#49182 = CARTESIAN_POINT ( 'NONE',  ( -14.20710678118644665, 18.75929247661552779, 5.000000000000000000 ) ) ;
#49183 = CONICAL_SURFACE ( 'NONE', #130209, 2.500000000000000444, 0.9599310885968830309 ) ;
#49184 = ADVANCED_FACE ( 'NONE', ( #110678 ), #56388, .T. ) ;
#49185 = FACE_OUTER_BOUND ( 'NONE', #35544, .T. ) ;
#49186 = LINE ( 'NONE', #57934, #131644 ) ;
#49187 = ORIENTED_EDGE ( 'NONE', *, *, #71866, .T. ) ;
#49188 = ADVANCED_FACE ( 'NONE', ( #12814 ), #101264, .T. ) ;
#49189 = CARTESIAN_POINT ( 'NONE',  ( 131.6379680400227414, -49.11957940092399610, 40.22172306649564177 ) ) ;
#49190 = CARTESIAN_POINT ( 'NONE',  ( 24.29974487139158867, -27.71228299555223273, 4.000000000000000000 ) ) ;
#49191 = ORIENTED_EDGE ( 'NONE', *, *, #111940, .F. ) ;
#49192 = ORIENTED_EDGE ( 'NONE', *, *, #26965, .F. ) ;
#49193 = CIRCLE ( 'NONE', #118599, 2.500000000000000444 ) ;
#49194 = DIRECTION ( 'NONE',  ( 4.681814790819592407E-17, 0.3543493200069153248, 0.9351131265310292928 ) ) ;
#49196 = ORIENTED_EDGE ( 'NONE', *, *, #12077, .F. ) ;
#49195 = AXIS2_PLACEMENT_3D ( 'NONE', #70365, #103628, #8568 ) ;
#49197 =( BOUNDED_CURVE ( )  B_SPLINE_CURVE ( 3, ( #83771, #104024, #71443, #117059 ),
 .UNSPECIFIED., .F., .T. ) 
 B_SPLINE_CURVE_WITH_KNOTS ( ( 4, 4 ),
 ( 2.779374508378135378, 4.199602562396838934 ),
 .UNSPECIFIED. ) 
 CURVE ( )  GEOMETRIC_REPRESENTATION_ITEM ( )  RATIONAL_B_SPLINE_CURVE ( ( 1.000000000000000000, 0.8388583629366628269, 0.8388583629366628269, 1.000000000000000000 ) ) 
 REPRESENTATION_ITEM ( '' )  );
#49198 = DIRECTION ( 'NONE',  ( -0.6830127018922180770, -0.6830127018922204085, -0.2588190451025213501 ) ) ;
#49199 = DIRECTION ( 'NONE',  ( 0.5735764363510444941, 0.8191520442889929088, 0.000000000000000000 ) ) ;
#49200 = PLANE ( 'NONE',  #23203 ) ;
#49201 = ADVANCED_FACE ( 'NONE', ( #35332 ), #114956, .F. ) ;
#49202 = CARTESIAN_POINT ( 'NONE',  ( -15.13014816246815286, 7.677378749015543846, 4.326165144404733098 ) ) ;
#49203 = ORIENTED_EDGE ( 'NONE', *, *, #9676, .F. ) ;
#49204 = FILL_AREA_STYLE ('',( #4906 ) ) ;
#49205 = VECTOR ( 'NONE', #24110, 1000.000000000000000 ) ;
#49206 = VERTEX_POINT ( 'NONE', #138914 ) ;
#49207 = PLANE ( 'NONE',  #65372 ) ;
#49208 = CARTESIAN_POINT ( 'NONE',  ( 30.25456980810189123, -6.871911579029512218, 3.967499999999996252 ) ) ;
#49209 = CARTESIAN_POINT ( 'NONE',  ( -19.49999999999985789, 19.46639925780205971, 5.000000000000000000 ) ) ;
#49210 = CARTESIAN_POINT ( 'NONE',  ( -5.999999999999952927, 8.587461875839151659, 4.000000000000000000 ) ) ;
#49211 = CARTESIAN_POINT ( 'NONE',  ( 5.999999999999956479, 16.93112307739201583, 4.000000000000000000 ) ) ;
#49212 = EDGE_LOOP ( 'NONE', ( #17482, #50138, #124789, #141130, #56466 ) ) ;
#49213 = VERTEX_POINT ( 'NONE', #116435 ) ;
#49214 = ORIENTED_EDGE ( 'NONE', *, *, #1487, .F. ) ;
#49215 = CARTESIAN_POINT ( 'NONE',  ( -34.91107144025656339, 21.84219451764876396, 4.000000000000000000 ) ) ;
#49216 = LINE ( 'NONE', #16537, #127437 ) ;
#49217 = VECTOR ( 'NONE', #59407, 1000.000000000000000 ) ;
#49219 = DIRECTION ( 'NONE',  ( 0.7071067811865486830, -0.7071067811865464625, -0.000000000000000000 ) ) ;
#49218 = VECTOR ( 'NONE', #75767, 1000.000000000000000 ) ;
#49220 = CIRCLE ( 'NONE', #120995, 2.552699999999928693 ) ;
#49221 = PLANE ( 'NONE',  #75134 ) ;
#49222 = CARTESIAN_POINT ( 'NONE',  ( 34.92499999999998295, 13.70115479773738265, 1.769996414796620954 ) ) ;
#49223 = VECTOR ( 'NONE', #140287, 1000.000000000000000 ) ;
#49224 = CARTESIAN_POINT ( 'NONE',  ( 28.49999999999980105, 3.653845994658417418, -4.504631822206436098 ) ) ;
#49225 = VECTOR ( 'NONE', #104389, 1000.000000000000000 ) ;
#49226 = DIRECTION ( 'NONE',  ( 0.3543493200069162685, -0.000000000000000000, -0.9351131265310288487 ) ) ;
#49227 = DIRECTION ( 'NONE',  ( 0.7071067811865487940, 0.7071067811865463515, 0.000000000000000000 ) ) ;
#49228 = LINE ( 'NONE', #3518, #2795 ) ;
#49229 = ORIENTED_EDGE ( 'NONE', *, *, #60258, .T. ) ;
#49230 = DIRECTION ( 'NONE',  ( 0.7071067811865487940, 0.7071067811865463515, 0.000000000000000000 ) ) ;
#49231 = VECTOR ( 'NONE', #98644, 1000.000000000000227 ) ;
#49232 = VECTOR ( 'NONE', #124124, 1000.000000000000000 ) ;
#49233 = MECHANICAL_DESIGN_GEOMETRIC_PRESENTATION_REPRESENTATION (  '', ( #26033 ), #67779 ) ;
#49234 = DIRECTION ( 'NONE',  ( -0.000000000000000000, -0.3543493200069152693, 0.9351131265310292928 ) ) ;
#49235 = ORIENTED_EDGE ( 'NONE', *, *, #100398, .F. ) ;
#49236 = CARTESIAN_POINT ( 'NONE',  ( 47.99451991528749062, 28.92564299267971251, 4.000000000000000000 ) ) ;
#49238 = ORIENTED_EDGE ( 'NONE', *, *, #135902, .T. ) ;
#49237 = LINE ( 'NONE', #36891, #83368 ) ;
#49239 = ORIENTED_EDGE ( 'NONE', *, *, #92070, .T. ) ;
#49240 = CARTESIAN_POINT ( 'NONE',  ( -39.18398860626899705, 28.73617430169814568, 5.000000000000000000 ) ) ;
#49241 = CARTESIAN_POINT ( 'NONE',  ( -5.994519915287488843, 28.92564299267942118, 4.000000000000000000 ) ) ;
#49242 = DIRECTION ( 'NONE',  ( -0.7071067811865486830, 0.7071067811865464625, 0.000000000000000000 ) ) ;
#49243 = ORIENTED_EDGE ( 'NONE', *, *, #32077, .F. ) ;
#49244 = PLANE ( 'NONE',  #32777 ) ;
#49245 = VERTEX_POINT ( 'NONE', #71509 ) ;
#49246 = PLANE ( 'NONE',  #24385 ) ;
#49247 = CARTESIAN_POINT ( 'NONE',  ( -4.499999999999967137, -13.53360074219760101, 5.000000000000000000 ) ) ;
#49249 = EDGE_CURVE ( 'NONE', #101316, #49712, #125161, .T. ) ;
#49248 = CARTESIAN_POINT ( 'NONE',  ( 32.72459685856478728, -1.637169565754161171, 6.109999999999998543 ) ) ;
#49250 = CARTESIAN_POINT ( 'NONE',  ( -12.18398860626900060, 28.73617430169795739, 5.000000000000000000 ) ) ;
#49251 = VECTOR ( 'NONE', #90748, 1000.000000000000000 ) ;
#49252 = CARTESIAN_POINT ( 'NONE',  ( 24.08314806772916228, 21.75929247661548871, 7.311836541448109017 ) ) ;
#49253 = EDGE_CURVE ( 'NONE', #17479, #58130, #139649, .T. ) ;
#49254 = LINE ( 'NONE', #80447, #104726 ) ;
#49255 = CARTESIAN_POINT ( 'NONE',  ( 66.18398860626901126, 28.73617430169833753, 5.000000000000000000 ) ) ;
#49256 = EDGE_CURVE ( 'NONE', #70917, #67449, #138189, .T. ) ;
#49257 = DIRECTION ( 'NONE',  ( 0.7071067811865487940, 0.7071067811865463515, 0.000000000000000000 ) ) ;
#49258 = CARTESIAN_POINT ( 'NONE',  ( 28.56206980810188512, -7.934999999999991616, -2.126176841940955242 ) ) ;
#49259 = CARTESIAN_POINT ( 'NONE',  ( 9.749569808101886892, 3.967499999999998916, 6.871911579029510442 ) ) ;
#49260 = LINE ( 'NONE', #138379, #101505 ) ;
#49261 = CARTESIAN_POINT ( 'NONE',  ( 16.49999999999989697, -4.912538124160701791, 4.000000000000000000 ) ) ;
#49263 = ADVANCED_FACE ( 'NONE', ( #106233 ), #83094, .F. ) ;
#49262 = CARTESIAN_POINT ( 'NONE',  ( 0.000000000000000000, 0.000000000000000000, 5.000000000000000000 ) ) ;
#49264 = ORIENTED_EDGE ( 'NONE', *, *, #21015, .F. ) ;
#49265 = STYLED_ITEM ( 'NONE', ( #21339 ), #100016 ) ;
#49266 = EDGE_LOOP ( 'NONE', ( #101704, #117316, #102713, #54859 ) ) ;
#49267 = CARTESIAN_POINT ( 'NONE',  ( 90.39583333333334281, -2.130196079827427091, 7.949999999999999289 ) ) ;
#49268 = ORIENTED_EDGE ( 'NONE', *, *, #83139, .T. ) ;
#49269 = ORIENTED_EDGE ( 'NONE', *, *, #99636, .T. ) ;
#49270 = MECHANICAL_DESIGN_GEOMETRIC_PRESENTATION_REPRESENTATION (  '', ( #33030 ), #23790 ) ;
#49271 = EDGE_CURVE ( 'NONE', #87588, #119333, #92513, .T. ) ;
#49272 = FACE_BOUND ( 'NONE', #133948, .T. ) ;
#49273 = CARTESIAN_POINT ( 'NONE',  ( 23.37913961620377279, -5.278424836066145431, -3.047499999999993658 ) ) ;
#49274 = AXIS2_PLACEMENT_3D ( 'NONE', #42332, #131467, #119832 ) ;
#49275 = MECHANICAL_DESIGN_GEOMETRIC_PRESENTATION_REPRESENTATION (  '', ( #102555 ), #47031 ) ;
#49276 = DIRECTION ( 'NONE',  ( -0.7071067811865486830, 0.7071067811865464625, 0.000000000000000000 ) ) ;
#49277 = VERTEX_POINT ( 'NONE', #94655 ) ;
#49278 = FACE_OUTER_BOUND ( 'NONE', #82555, .T. ) ;
#49279 = CARTESIAN_POINT ( 'NONE',  ( -45.18398860626900415, 28.73617430169818832, 5.000000000000000000 ) ) ;
#49280 = EDGE_CURVE ( 'NONE', #118878, #81113, #59237, .T. ) ;
#49281 = CARTESIAN_POINT ( 'NONE',  ( 31.96659967656958301, 6.759292476615653023, 12.28218704918529447 ) ) ;
#49282 = CARTESIAN_POINT ( 'NONE',  ( 126.5779968411016796, 6.505456897006314243, 2.228754984098625602 ) ) ;
#49283 = EDGE_CURVE ( 'NONE', #130144, #67630, #70811, .T. ) ;
#49284 = DIRECTION ( 'NONE',  ( 1.000000000000000000, 0.000000000000000000, 0.000000000000000000 ) ) ;
#49285 = CARTESIAN_POINT ( 'NONE',  ( 0.000000000000000000, 0.000000000000000000, 5.000000000000000000 ) ) ;
#49286 = CARTESIAN_POINT ( 'NONE',  ( 5.207106781186512379, -2.240707523384262601, 5.000000000000000000 ) ) ;
#49287 = FACE_OUTER_BOUND ( 'NONE', #47500, .T. ) ;
#49288 = DIRECTION ( 'NONE',  ( -0.6830127018922180770, -0.6830127018922204085, -0.2588190451025213501 ) ) ;
#49289 = CARTESIAN_POINT ( 'NONE',  ( 25.17183060077629975, 12.75929247661558641, 4.000000000000000000 ) ) ;
#49290 = ADVANCED_FACE ( 'NONE', ( #83841 ), #39609, .T. ) ;
#49291 = DIRECTION ( 'NONE',  ( -0.7071067811865486830, 0.7071067811865464625, 0.000000000000000000 ) ) ;
#49292 = EDGE_LOOP ( 'NONE', ( #27525, #27035, #135303, #72249 ) ) ;
#49293 = VERTEX_POINT ( 'NONE', #26568 ) ;
#49294 = CARTESIAN_POINT ( 'NONE',  ( 114.1879301918980900, 6.110000000000002984, -1.637169565754156730 ) ) ;
#49295 = VERTEX_POINT ( 'NONE', #17803 ) ;
#49296 = VECTOR ( 'NONE', #12737, 1000.000000000000000 ) ;
#49297 = EDGE_CURVE ( 'NONE', #133341, #139662, #82391, .T. ) ;
#49298 = AXIS2_PLACEMENT_3D ( 'NONE', #133074, #33061, #9827 ) ;
#49299 = CARTESIAN_POINT ( 'NONE',  ( 32.67183060077624646, 5.259292476615669010, 4.000000000000000000 ) ) ;
#49300 = ORIENTED_EDGE ( 'NONE', *, *, #122910, .F. ) ;
#49301 = DIRECTION ( 'NONE',  ( 0.7071067811865487940, 0.7071067811865463515, 0.000000000000000000 ) ) ;
#49302 = DIRECTION ( 'NONE',  ( -0.3543493200069162685, -0.000000000000000000, -0.9351131265310288487 ) ) ;
#49303 = CARTESIAN_POINT ( 'NONE',  ( 107.2454301918981088, -5.291415217122918513, -3.055000000000000160 ) ) ;
#49304 = VERTEX_POINT ( 'NONE', #126569 ) ;
#49305 = FACE_OUTER_BOUND ( 'NONE', #46783, .T. ) ;
#49306 = ORIENTED_EDGE ( 'NONE', *, *, #90459, .F. ) ;
#49308 = EDGE_CURVE ( 'NONE', #142848, #105496, #72267, .T. ) ;
#49307 = DIRECTION ( 'NONE',  ( 0.7071067811865487940, -0.7071067811865463515, 0.000000000000000000 ) ) ;
#49309 = AXIS2_PLACEMENT_3D ( 'NONE', #126642, #7719, #138984 ) ;
#49310 = DIRECTION ( 'NONE',  ( -0.000000000000000000, 0.000000000000000000, 1.000000000000000000 ) ) ;
#49311 = DIRECTION ( 'NONE',  ( 0.7071067811865487940, 0.7071067811865463515, 0.000000000000000000 ) ) ;
#49312 = ORIENTED_EDGE ( 'NONE', *, *, #101954, .T. ) ;
#49313 = ORIENTED_EDGE ( 'NONE', *, *, #94602, .T. ) ;
#49314 = VERTEX_POINT ( 'NONE', #104093 ) ;
#49315 = CARTESIAN_POINT ( 'NONE',  ( 6.183988606268994381, 28.73617430169791476, 5.000000000000000000 ) ) ;
#49316 = DIRECTION ( 'NONE',  ( 0.6830127018922180770, -0.6830127018922204085, -0.2588190451025213501 ) ) ;
#49317 = CARTESIAN_POINT ( 'NONE',  ( 9.254569808101885897, -6.871911579029512218, 3.967499999999996252 ) ) ;
#49318 = VECTOR ( 'NONE', #39093, 1000.000000000000000 ) ;
#49319 = CARTESIAN_POINT ( 'NONE',  ( 21.43750000000000000, -4.461849672132299105, 4.461849672132299993 ) ) ;
#49320 = EDGE_CURVE ( 'NONE', #9707, #1800, #62074, .T. ) ;
#49321 = DIRECTION ( 'NONE',  ( -0.7071067811865486830, -0.7071067811865464625, 0.000000000000000000 ) ) ;
#49322 = EDGE_LOOP ( 'NONE', ( #110185, #55486, #108851 ) ) ;
#49323 = ORIENTED_EDGE ( 'NONE', *, *, #32197, .T. ) ;
#49324 = DIRECTION ( 'NONE',  ( 0.6830127018922181881, 0.6830127018922202975, -0.2588190451025214056 ) ) ;
#49326 = VERTEX_POINT ( 'NONE', #38174 ) ;
#49325 = EDGE_CURVE ( 'NONE', #110453, #3179, #17120, .T. ) ;
#49327 = ORIENTED_EDGE ( 'NONE', *, *, #20192, .T. ) ;
#49328 = VECTOR ( 'NONE', #125524, 1000.000000000000000 ) ;
#49329 = VECTOR ( 'NONE', #3678, 1000.000000000000000 ) ;
#49330 = CARTESIAN_POINT ( 'NONE',  ( 24.70710678118637915, 14.25929247661557220, 5.000000000000000000 ) ) ;
#49331 = VECTOR ( 'NONE', #27744, 1000.000000000000000 ) ;
#49332 = DIRECTION ( 'NONE',  ( -0.6830127018922181881, 0.6830127018922202975, -0.2588190451025214056 ) ) ;
#49333 = PLANE ( 'NONE',  #137521 ) ;
#49334 = ORIENTED_EDGE ( 'NONE', *, *, #47415, .T. ) ;
#49335 = CARTESIAN_POINT ( 'NONE',  ( 5.395833333333335702, 1.633150327867692431, -6.094999999999989093 ) ) ;
#49336 = ADVANCED_FACE ( 'NONE', ( #80960 ), #25849, .F. ) ;
#49338 = LINE ( 'NONE', #50734, #36371 ) ;
#49337 = VECTOR ( 'NONE', #14750, 1000.000000000000000 ) ;
#49339 = VECTOR ( 'NONE', #128767, 1000.000000000000000 ) ;
#49340 = AXIS2_PLACEMENT_3D ( 'NONE', #92423, #48228, #59152 ) ;
#49341 = CARTESIAN_POINT ( 'NONE',  ( 23.51078643762690490, -27.52281430457038880, 5.000000000000000000 ) ) ;
#49342 = FACE_OUTER_BOUND ( 'NONE', #102137, .T. ) ;
#49343 = ORIENTED_EDGE ( 'NONE', *, *, #76673, .T. ) ;
#49344 = CARTESIAN_POINT ( 'NONE',  ( 32.99999999999976552, -16.02097659208068947, -11.96015758381216365 ) ) ;
#49345 = FACE_BOUND ( 'NONE', #27159, .T. ) ;
#49346 = ORIENTED_EDGE ( 'NONE', *, *, #26359, .T. ) ;
#49347 = DIRECTION ( 'NONE',  ( -0.3543493200069162685, -0.000000000000000000, -0.9351131265310288487 ) ) ;
#49349 = EDGE_CURVE ( 'NONE', #58607, #9195, #60673, .T. ) ;
#49348 = LINE ( 'NONE', #72544, #68925 ) ;
#49350 = DIRECTION ( 'NONE',  ( -0.6830127018922181881, 0.6830127018922202975, -0.2588190451025214056 ) ) ;
#49351 = ORIENTED_EDGE ( 'NONE', *, *, #12263, .T. ) ;
#49352 = LINE ( 'NONE', #114556, #80607 ) ;
#49353 = ORIENTED_EDGE ( 'NONE', *, *, #68289, .F. ) ;
#49354 = VERTEX_POINT ( 'NONE', #49052 ) ;
#49355 = ORIENTED_EDGE ( 'NONE', *, *, #22497, .F. ) ;
#49356 = CARTESIAN_POINT ( 'NONE',  ( 34.18293019189810167, -1.637169565754158951, -6.109999999999998543 ) ) ;
#49357 = ORIENTED_EDGE ( 'NONE', *, *, #141716, .T. ) ;
#49358 = VECTOR ( 'NONE', #18150, 1000.000000000000000 ) ;
#49359 = DIRECTION ( 'NONE',  ( -0.7071067811865486830, 0.7071067811865464625, 0.000000000000000000 ) ) ;
#49360 = DIRECTION ( 'NONE',  ( -0.7071067811865486830, -0.7071067811865464625, 0.000000000000000000 ) ) ;
#49361 = DIRECTION ( 'NONE',  ( -1.000000000000000000, -1.224606353822377258E-16, -0.000000000000000000 ) ) ;
#49362 = ORIENTED_EDGE ( 'NONE', *, *, #133025, .F. ) ;
#49363 = DIRECTION ( 'NONE',  ( 0.000000000000000000, 0.000000000000000000, -1.000000000000000000 ) ) ;
#49364 = DIRECTION ( 'NONE',  ( -0.6830127018922180770, -0.6830127018922204085, -0.2588190451025213501 ) ) ;
#49365 = AXIS2_PLACEMENT_3D ( 'NONE', #85334, #27380, #63636 ) ;
#49366 = PLANE ( 'NONE',  #11240 ) ;
#49367 = PLANE ( 'NONE',  #94866 ) ;
#49368 = ADVANCED_FACE ( 'NONE', ( #93247 ), #41729, .T. ) ;
#49369 = DIRECTION ( 'NONE',  ( 0.6830127018922181881, 0.6830127018922202975, -0.2588190451025214056 ) ) ;
#49370 = VECTOR ( 'NONE', #37979, 1000.000000000000000 ) ;
#49371 = DIRECTION ( 'NONE',  ( 0.3543493200069162685, -0.000000000000000000, -0.9351131265310288487 ) ) ;
#49372 = ORIENTED_EDGE ( 'NONE', *, *, #45248, .F. ) ;
#49373 = ORIENTED_EDGE ( 'NONE', *, *, #120943, .T. ) ;
#49374 = ORIENTED_EDGE ( 'NONE', *, *, #24015, .F. ) ;
#49375 = ORIENTED_EDGE ( 'NONE', *, *, #26786, .T. ) ;
#49376 = DIRECTION ( 'NONE',  ( -0.000000000000000000, 0.000000000000000000, 1.000000000000000000 ) ) ;
#49377 = VERTEX_POINT ( 'NONE', #109111 ) ;
#49378 = ORIENTED_EDGE ( 'NONE', *, *, #137551, .F. ) ;
#49379 = CARTESIAN_POINT ( 'NONE',  ( 60.48921356237309510, -27.52281430457097500, 5.000000000000000000 ) ) ;
#49380 = CARTESIAN_POINT ( 'NONE',  ( 17.06332250466817158, 3.061616997868383634E-16, -2.500000000000000444 ) ) ;
#49381 = EDGE_CURVE ( 'NONE', #108960, #86507, #46490, .T. ) ;
#49382 = EDGE_CURVE ( 'NONE', #75689, #18121, #31573, .T. ) ;
#49383 = CARTESIAN_POINT ( 'NONE',  ( 12.19999999999999574, -59.76999999999998892, -40.00000000000000000 ) ) ;
#49384 = VERTEX_POINT ( 'NONE', #96769 ) ;
#49385 = DIRECTION ( 'NONE',  ( -1.000000000000000000, -1.224606353822377258E-16, -0.000000000000000000 ) ) ;
#49386 = ORIENTED_EDGE ( 'NONE', *, *, #51859, .T. ) ;
#49387 =( BOUNDED_CURVE ( )  B_SPLINE_CURVE ( 2, ( #27307, #106275, #40376, #96132, #93298, #62837, #5551, #137530, #128776, #29452, #17845, #82432, #61433 ),
 .UNSPECIFIED., .F., .T. ) 
 B_SPLINE_CURVE_WITH_KNOTS ( ( 3, 2, 2, 2, 2, 2, 3 ),
 ( 0.3500000000000000333, 0.3583333333333333925, 0.3666666666666666963, 0.3750000000000001110, 0.3833333333333334703, 0.3916666666666667740, 0.4000000000000001332 ),
 .UNSPECIFIED. ) 
 CURVE ( )  GEOMETRIC_REPRESENTATION_ITEM ( )  RATIONAL_B_SPLINE_CURVE ( ( 0.9999999999999997780, 0.9659258262890685343, 1.000000000000000000, 0.9659258262890683122, 1.000000000000000000, 0.9659258262890683122, 1.000000000000000000, 0.9659258262890683122, 1.000000000000000000, 0.9659258262890683122, 1.000000000000000000, 0.9659258262890678681, 1.000000000000000444 ) ) 
 REPRESENTATION_ITEM ( '' )  );
#49389 = VECTOR ( 'NONE', #70475, 1000.000000000000000 ) ;
#49388 = CARTESIAN_POINT ( 'NONE',  ( -25.49999999999981881, 13.08746187583910725, 4.000000000000000000 ) ) ;
#49390 = CARTESIAN_POINT ( 'NONE',  ( 29.99999999999978328, -22.22500000000000142, 4.412002311790018894 ) ) ;
#49391 = VECTOR ( 'NONE', #115651, 1000.000000000000000 ) ;
#49392 = CARTESIAN_POINT ( 'NONE',  ( 3.858736474768553304, 5.808823158059031044, -5.808823158059038150 ) ) ;
#49393 = EDGE_LOOP ( 'NONE', ( #92523, #69683, #57763, #12108 ) ) ;
#49395 = DIRECTION ( 'NONE',  ( -0.000000000000000000, -0.3543493200069152693, 0.9351131265310292928 ) ) ;
#49394 = CARTESIAN_POINT ( 'NONE',  ( 98.49543019189812298, 5.291415217122917625, 3.055000000000002380 ) ) ;
#49396 = CARTESIAN_POINT ( 'NONE',  ( -34.42500000000001137, -3.022814304570547783, 5.000000000000000000 ) ) ;
#49397 = ORIENTED_EDGE ( 'NONE', *, *, #67079, .F. ) ;
#49398 = VERTEX_POINT ( 'NONE', #41012 ) ;
#49399 = LINE ( 'NONE', #103032, #12489 ) ;
#49400 = VERTEX_POINT ( 'NONE', #75796 ) ;
#49402 = VECTOR ( 'NONE', #137704, 1000.000000000000000 ) ;
#49401 = FILL_AREA_STYLE ('',( #116754 ) ) ;
#49403 = LINE ( 'NONE', #25451, #13871 ) ;
#49404 = PLANE ( 'NONE',  #52042 ) ;
#49405 = CARTESIAN_POINT ( 'NONE',  ( -11.99999999999992717, 11.58746187583913390, 4.000000000000000000 ) ) ;
#49406 = FILL_AREA_STYLE ('',( #47973 ) ) ;
#49407 = EDGE_CURVE ( 'NONE', #30975, #75310, #53476, .T. ) ;
#49408 = ORIENTED_EDGE ( 'NONE', *, *, #39267, .F. ) ;
#49409 = LINE ( 'NONE', #60273, #59882 ) ;
#49410 = DIRECTION ( 'NONE',  ( -0.7071067811865487940, 0.7071067811865463515, -0.000000000000000000 ) ) ;
#49411 = LINE ( 'NONE', #3683, #30330 ) ;
#49412 = VERTEX_POINT ( 'NONE', #18510 ) ;
#49413 = FACE_OUTER_BOUND ( 'NONE', #47123, .T. ) ;
#49414 = VECTOR ( 'NONE', #4647, 999.9999999999998863 ) ;
#49415 = DIRECTION ( 'NONE',  ( -0.7071067811865486830, 0.7071067811865464625, 0.000000000000000000 ) ) ;
#49416 = ORIENTED_EDGE ( 'NONE', *, *, #84258, .F. ) ;
#49418 = ORIENTED_EDGE ( 'NONE', *, *, #83488, .T. ) ;
#49417 = CARTESIAN_POINT ( 'NONE',  ( 6.471592354503322042, 9.902892378096218942E-16, 0.000000000000000000 ) ) ;
#49419 = VERTEX_POINT ( 'NONE', #141024 ) ;
#49420 = VECTOR ( 'NONE', #120553, 1000.000000000000114 ) ;
#49421 = CARTESIAN_POINT ( 'NONE',  ( -8.173355474122208975, 12.20286799362002483, -25.50874979209409688 ) ) ;
#49422 = VERTEX_POINT ( 'NONE', #42474 ) ;
#49423 = LINE ( 'NONE', #16002, #134499 ) ;
#49424 = CARTESIAN_POINT ( 'NONE',  ( -15.18398860626900237, 28.73617430169797871, 5.000000000000000000 ) ) ;
#49425 = ADVANCED_FACE ( 'NONE', ( #87382 ), #119959, .F. ) ;
#49426 = EDGE_LOOP ( 'NONE', ( #106818, #81080, #28824, #125946 ) ) ;
#49427 = LINE ( 'NONE', #137848, #62416 ) ;
#49428 = EDGE_CURVE ( 'NONE', #102574, #101765, #58727, .T. ) ;
#49429 = DIRECTION ( 'NONE',  ( -0.000000000000000000, 0.000000000000000000, 1.000000000000000000 ) ) ;
#49430 = DIRECTION ( 'NONE',  ( 1.000000000000000000, 1.224606353822377258E-16, 0.000000000000000000 ) ) ;
#49431 = DIRECTION ( 'NONE',  ( 0.7071067811865486830, -0.7071067811865463515, 0.000000000000000000 ) ) ;
#49432 = DIRECTION ( 'NONE',  ( 1.000000000000000000, 0.000000000000000000, 0.000000000000000000 ) ) ;
#49433 = AXIS2_PLACEMENT_3D ( 'NONE', #136205, #111612, #81138 ) ;
#49434 = DIRECTION ( 'NONE',  ( -0.000000000000000000, -1.000000000000000000, -0.000000000000000000 ) ) ;
#49435 = CARTESIAN_POINT ( 'NONE',  ( 2.292893218813441880, -0.7407075233842735917, 5.000000000000000000 ) ) ;
#49436 = CARTESIAN_POINT ( 'NONE',  ( 28.07919371712955225, 3.975000000000002753, -6.884901960086283523 ) ) ;
#49438 = EDGE_CURVE ( 'NONE', #133821, #42793, #54763, .T. ) ;
#49437 = LINE ( 'NONE', #16017, #57044 ) ;
#49440 = EDGE_CURVE ( 'NONE', #127203, #120495, #131597, .T. ) ;
#49439 = ORIENTED_EDGE ( 'NONE', *, *, #54373, .T. ) ;
#49441 = AXIS2_PLACEMENT_3D ( 'NONE', #80556, #69692, #68971 ) ;
#49442 = VERTEX_POINT ( 'NONE', #117821 ) ;
#49443 = EDGE_LOOP ( 'NONE', ( #64244, #139631, #66155, #15877 ) ) ;
#49444 = CARTESIAN_POINT ( 'NONE',  ( 119.1250000000000142, -7.950000000000000178, -4.867971026610729436E-16 ) ) ;
#49445 = EDGE_LOOP ( 'NONE', ( #36123, #83620, #96954, #29192 ) ) ;
#49446 = ORIENTED_EDGE ( 'NONE', *, *, #54470, .T. ) ;
#49447 = VERTEX_POINT ( 'NONE', #30871 ) ;
#49448 = VECTOR ( 'NONE', #40046, 1000.000000000000000 ) ;
#49449 = DIRECTION ( 'NONE',  ( 0.7071067811865487940, 0.7071067811865463515, 0.000000000000000000 ) ) ;
#49450 = DIRECTION ( 'NONE',  ( 0.7071067811865486830, -0.7071067811865464625, -0.000000000000000000 ) ) ;
#49451 = VERTEX_POINT ( 'NONE', #97517 ) ;
#49452 = LINE ( 'NONE', #40001, #138883 ) ;
#49453 = DIRECTION ( 'NONE',  ( -0.7071067811865486830, -0.7071067811865464625, 0.000000000000000000 ) ) ;
#49454 = EDGE_CURVE ( 'NONE', #108744, #117764, #141775, .T. ) ;
#49455 = DIRECTION ( 'NONE',  ( 0.6830127018922180770, -0.6830127018922204085, -0.2588190451025213501 ) ) ;
#49456 = CARTESIAN_POINT ( 'NONE',  ( 114.9170968585647756, 3.054999999999998828, 5.291415217122922066 ) ) ;
#49457 = ORIENTED_EDGE ( 'NONE', *, *, #108593, .T. ) ;
#49458 = EDGE_CURVE ( 'NONE', #45672, #115183, #32289, .T. ) ;
#49459 = CARTESIAN_POINT ( 'NONE',  ( -7.499999999999944045, 8.319652575858382804, -8.582050562765845214 ) ) ;
#49460 = CARTESIAN_POINT ( 'NONE',  ( 4.213219033033557714, 12.75929247661559351, 10.29404684609036202 ) ) ;
#49461 = DIRECTION ( 'NONE',  ( 0.000000000000000000, 0.000000000000000000, 1.000000000000000000 ) ) ;
#49462 = CARTESIAN_POINT ( 'NONE',  ( 82.91252705046289861, -7.949999999999998401, -4.867971026610728450E-16 ) ) ;
#49463 = DIRECTION ( 'NONE',  ( -0.7071067811865487940, 0.7071067811865463515, 0.000000000000000000 ) ) ;
#49464 = MECHANICAL_DESIGN_GEOMETRIC_PRESENTATION_REPRESENTATION (  '', ( #116575 ), #132857 ) ;
#49465 = DIRECTION ( 'NONE',  ( -0.000000000000000000, 0.000000000000000000, 1.000000000000000000 ) ) ;
#49466 = PRESENTATION_STYLE_ASSIGNMENT (( #117508 ) ) ;
#49467 = CARTESIAN_POINT ( 'NONE',  ( 34.05836038379622721, -7.949999999999997513, -2.130196079827425759 ) ) ;
#49468 = EDGE_CURVE ( 'NONE', #118451, #63434, #118561, .T. ) ;
#49469 = CARTESIAN_POINT ( 'NONE',  ( -2.510786437626908008, -27.52281430457053446, 5.000000000000000000 ) ) ;
#49470 = VECTOR ( 'NONE', #59422, 1000.000000000000000 ) ;
#49471 = ORIENTED_EDGE ( 'NONE', *, *, #128334, .F. ) ;
#49472 = VERTEX_POINT ( 'NONE', #98943 ) ;
#49473 = CARTESIAN_POINT ( 'NONE',  ( 38.62499999999999289, -7.950000000000000178, -4.867971026610729436E-16 ) ) ;
#49474 = EDGE_LOOP ( 'NONE', ( #34354, #29733, #115722, #66585 ) ) ;
#49475 = FACE_OUTER_BOUND ( 'NONE', #115288, .T. ) ;
#49476 = CARTESIAN_POINT ( 'NONE',  ( 9.707106781186476852, 5.259292476615659240, 5.000000000000000000 ) ) ;
#49477 = ORIENTED_EDGE ( 'NONE', *, *, #124799, .F. ) ;
#49478 = EDGE_CURVE ( 'NONE', #85990, #27559, #119268, .T. ) ;
#49479 = DIRECTION ( 'NONE',  ( -0.000000000000000000, 0.000000000000000000, 1.000000000000000000 ) ) ;
#49480 = VECTOR ( 'NONE', #51142, 1000.000000000000000 ) ;
#49481 = FACE_OUTER_BOUND ( 'NONE', #8090, .T. ) ;
#49482 = FACE_OUTER_BOUND ( 'NONE', #57915, .T. ) ;
#49483 = LINE ( 'NONE', #30558, #55747 ) ;
#49484 = CARTESIAN_POINT ( 'NONE',  ( 128.8287635252314658, 0.000000000000000000, -6.109999999999998543 ) ) ;
#49485 = AXIS2_PLACEMENT_3D ( 'NONE', #24679, #92786, #26122 ) ;
#49486 = ORIENTED_EDGE ( 'NONE', *, *, #34008, .T. ) ;
#49487 = CARTESIAN_POINT ( 'NONE',  ( -45.29974487139158867, -27.71228299555237840, 4.000000000000000000 ) ) ;
#49488 = ORIENTED_EDGE ( 'NONE', *, *, #67762, .T. ) ;
#49489 = ADVANCED_FACE ( 'NONE', ( #84539 ), #29410, .T. ) ;
#49490 = CARTESIAN_POINT ( 'NONE',  ( 16.49999999999989342, 9.052185695429077583, 5.000000000000000000 ) ) ;
#49491 = DIRECTION ( 'NONE',  ( 0.6830127018922181881, 0.6830127018922202975, -0.2588190451025214056 ) ) ;
#49492 = DIRECTION ( 'NONE',  ( -4.681814790819591790E-17, -0.3543493200069152693, 0.9351131265310292928 ) ) ;
#49493 = VECTOR ( 'NONE', #30403, 1000.000000000000000 ) ;
#49494 = CARTESIAN_POINT ( 'NONE',  ( 62.97916666666667140, -7.950000000000000178, 2.130196079827424427 ) ) ;
#49495 = ORIENTED_EDGE ( 'NONE', *, *, #122883, .F. ) ;
#49496 = CARTESIAN_POINT ( 'NONE',  ( 51.04209685856476852, 5.291415217122923842, -3.054999999999996163 ) ) ;
#49497 = EDGE_LOOP ( 'NONE', ( #86709, #27485, #115019, #138301 ) ) ;
#49498 = CARTESIAN_POINT ( 'NONE',  ( 0.000000000000000000, 0.000000000000000000, 5.000000000000000000 ) ) ;
#49499 = FACE_OUTER_BOUND ( 'NONE', #35843, .T. ) ;
#49500 = CARTESIAN_POINT ( 'NONE',  ( -19.36246187583889977, 22.22499999999999432, 4.000000000000000000 ) ) ;
#49501 = ADVANCED_FACE ( 'NONE', ( #96090 ), #140327, .F. ) ;
#49502 = EDGE_CURVE ( 'NONE', #123049, #118158, #129437, .T. ) ;
#49503 = DIRECTION ( 'NONE',  ( 0.3543493200069162685, -0.000000000000000000, -0.9351131265310288487 ) ) ;
#49504 = AXIS2_PLACEMENT_3D ( 'NONE', #35967, #88922, #57011 ) ;
#49505 = EDGE_CURVE ( 'NONE', #80353, #36162, #1740, .T. ) ;
#49506 = AXIS2_PLACEMENT_3D ( 'NONE', #36331, #25425, #137793 ) ;
#49507 = CARTESIAN_POINT ( 'NONE',  ( 48.18293019189812298, -1.637169565754158951, -6.109999999999998543 ) ) ;
#49508 = VERTEX_POINT ( 'NONE', #56918 ) ;
#49509 = CARTESIAN_POINT ( 'NONE',  ( 13.49999999999990763, 11.52377502935404330, -1.522421517564115145 ) ) ;
#49510 = CARTESIAN_POINT ( 'NONE',  ( -22.01987774928535657, -17.24070752338410983, 20.23474786156464233 ) ) ;
#49511 = EDGE_LOOP ( 'NONE', ( #142058, #112300, #103971 ) ) ;
#49512 = VERTEX_POINT ( 'NONE', #110523 ) ;
#49513 = AXIS2_PLACEMENT_3D ( 'NONE', #44848, #1262, #132560 ) ;
#49514 = CARTESIAN_POINT ( 'NONE',  ( 19.05000000000000071, 3.174999999999997158, 4.000000000000000000 ) ) ;
#49515 = ORIENTED_EDGE ( 'NONE', *, *, #119278, .F. ) ;
#49516 = LINE ( 'NONE', #126318, #23671 ) ;
#49517 = VERTEX_POINT ( 'NONE', #12651 ) ;
#49518 = DIRECTION ( 'NONE',  ( -0.7071067811865486830, -0.7071067811865464625, 0.000000000000000000 ) ) ;
#49519 = VECTOR ( 'NONE', #73614, 1000.000000000000000 ) ;
#49520 = FACE_BOUND ( 'NONE', #77303, .T. ) ;
#49521 = DIRECTION ( 'NONE',  ( -0.7071067811865487940, 0.7071067811865463515, -0.000000000000000000 ) ) ;
#49522 = FACE_OUTER_BOUND ( 'NONE', #12195, .T. ) ;
#49523 = ORIENTED_EDGE ( 'NONE', *, *, #133337, .F. ) ;
#49524 = SURFACE_SIDE_STYLE ('',( #3788 ) ) ;
#49526 = ORIENTED_EDGE ( 'NONE', *, *, #22336, .F. ) ;
#49525 = CARTESIAN_POINT ( 'NONE',  ( 26.67183060077628554, 11.25929247661559884, 4.000000000000000000 ) ) ;
#49527 = ORIENTED_EDGE ( 'NONE', *, *, #69893, .F. ) ;
#49528 = CARTESIAN_POINT ( 'NONE',  ( 13.49999999999990585, 21.05218569542895679, 5.000000000000000000 ) ) ;
#49529 = ORIENTED_EDGE ( 'NONE', *, *, #123186, .T. ) ;
#49530 = VERTEX_POINT ( 'NONE', #24946 ) ;
#49531 = CARTESIAN_POINT ( 'NONE',  ( 61.74543019189811588, -5.291415217122918513, -3.055000000000000160 ) ) ;
#49533 = ORIENTED_EDGE ( 'NONE', *, *, #131670, .T. ) ;
#49532 = AXIS2_PLACEMENT_3D ( 'NONE', #29521, #93371, #7024 ) ;
#49534 = FACE_OUTER_BOUND ( 'NONE', #117792, .T. ) ;
#49535 = PLANE ( 'NONE',  #82037 ) ;
#49536 = EDGE_CURVE ( 'NONE', #96891, #47238, #58371, .T. ) ;
#49537 = ORIENTED_EDGE ( 'NONE', *, *, #2716, .F. ) ;
#49538 = VECTOR ( 'NONE', #104188, 1000.000000000000000 ) ;
#49539 = CARTESIAN_POINT ( 'NONE',  ( -21.05633424050521540, 8.797022467481218300, 4.404357971607193889 ) ) ;
#49540 = DIRECTION ( 'NONE',  ( -0.7071067811865486830, 0.7071067811865464625, 0.000000000000000000 ) ) ;
#49541 = CARTESIAN_POINT ( 'NONE',  ( 33.18398860626899705, 28.73617430169810305, 5.000000000000000000 ) ) ;
#49542 = CARTESIAN_POINT ( 'NONE',  ( 15.75000000000000000, -7.464222240803106570E-16, -6.094999999999989981 ) ) ;
#49543 =( LENGTH_UNIT ( ) NAMED_UNIT ( * ) SI_UNIT ( .MILLI., .METRE. ) );
#49544 = VERTEX_POINT ( 'NONE', #33032 ) ;
#49545 = VERTEX_POINT ( 'NONE', #77248 ) ;
#49546 = CARTESIAN_POINT ( 'NONE',  ( 29.99999999999979750, 10.55218569542906515, 5.000000000000000000 ) ) ;
#49547 = LINE ( 'NONE', #114742, #127652 ) ;
#49548 = ORIENTED_EDGE ( 'NONE', *, *, #60269, .T. ) ;
#49549 = EDGE_LOOP ( 'NONE', ( #2419, #105975, #1572, #131684 ) ) ;
#49550 = ORIENTED_EDGE ( 'NONE', *, *, #24860, .F. ) ;
#49551 = FACE_OUTER_BOUND ( 'NONE', #74101, .T. ) ;
#49552 = PLANE ( 'NONE',  #59129 ) ;
#49553 = EDGE_CURVE ( 'NONE', #32782, #89832, #54047, .T. ) ;
#49554 = EDGE_CURVE ( 'NONE', #54652, #131882, #11193, .T. ) ;
#49555 = CARTESIAN_POINT ( 'NONE',  ( 11.29289321881337749, 2.259292476615696099, 5.000000000000000000 ) ) ;
#49556 = ORIENTED_EDGE ( 'NONE', *, *, #1643, .F. ) ;
#49557 = DIRECTION ( 'NONE',  ( -0.3543493200069162685, -0.000000000000000000, -0.9351131265310288487 ) ) ;
#49558 = VECTOR ( 'NONE', #14187, 1000.000000000000000 ) ;
#49559 = DIRECTION ( 'NONE',  ( -0.6830127018922181881, 0.6830127018922202975, -0.2588190451025214056 ) ) ;
#49560 = VECTOR ( 'NONE', #143022, 999.9999999999998863 ) ;
#49561 = CARTESIAN_POINT ( 'NONE',  ( 11.00456980810188590, 6.871911579029510442, -3.967499999999998916 ) ) ;
#49562 = LINE ( 'NONE', #37955, #125981 ) ;
#49563 = ORIENTED_EDGE ( 'NONE', *, *, #26301, .T. ) ;
#49564 = EDGE_CURVE ( 'NONE', #70483, #94208, #4781, .T. ) ;
#49565 = FACE_OUTER_BOUND ( 'NONE', #104006, .T. ) ;
#49566 = DIRECTION ( 'NONE',  ( 0.3543493200069162685, -0.000000000000000000, -0.9351131265310288487 ) ) ;
#49567 = DIRECTION ( 'NONE',  ( -0.000000000000000000, 0.000000000000000000, 1.000000000000000000 ) ) ;
#49569 = ORIENTED_EDGE ( 'NONE', *, *, #126307, .F. ) ;
#49568 = DIRECTION ( 'NONE',  ( -0.000000000000000000, 0.000000000000000000, 1.000000000000000000 ) ) ;
#49570 = CARTESIAN_POINT ( 'NONE',  ( 11.56663961620377279, 1.633150327867675555, 6.094999999999998863 ) ) ;
#49571 = ORIENTED_EDGE ( 'NONE', *, *, #70576, .T. ) ;
#49572 = CARTESIAN_POINT ( 'NONE',  ( 2.671830600776449405, -9.740707523384187994, 4.000000000000000000 ) ) ;
#49573 = CARTESIAN_POINT ( 'NONE',  ( 5.999999999999967137, -13.44781430457069327, 5.000000000000000000 ) ) ;
#49574 = DIRECTION ( 'NONE',  ( -0.3543493200069162685, -0.000000000000000000, -0.9351131265310288487 ) ) ;
#49575 = EDGE_CURVE ( 'NONE', #109693, #118985, #133743, .T. ) ;
#49576 = VERTEX_POINT ( 'NONE', #69202 ) ;
#49577 = VECTOR ( 'NONE', #61698, 999.9999999999998863 ) ;
#49578 = FACE_OUTER_BOUND ( 'NONE', #61816, .T. ) ;
#49579 = CARTESIAN_POINT ( 'NONE',  ( -63.48921356237309510, -27.52281430457099631, 5.000000000000000000 ) ) ;
#49580 = CARTESIAN_POINT ( 'NONE',  ( -9.489213562373095101, -27.52281430457062328, 5.000000000000000000 ) ) ;
#49581 = ORIENTED_EDGE ( 'NONE', *, *, #75575, .T. ) ;
#49582 = ADVANCED_FACE ( 'NONE', ( #113386 ), #111998, .F. ) ;
#49583 = FACE_OUTER_BOUND ( 'NONE', #84235, .T. ) ;
#49584 = CARTESIAN_POINT ( 'NONE',  ( -32.99999999999976552, -19.06887692260762890, 4.000000000000000000 ) ) ;
#49586 = AXIS2_PLACEMENT_3D ( 'NONE', #126837, #51455, #85470 ) ;
#49585 = DIRECTION ( 'NONE',  ( 0.000000000000000000, 0.000000000000000000, 1.000000000000000000 ) ) ;
#49587 = DIRECTION ( 'NONE',  ( 0.6830127018922180770, -0.6830127018922204085, -0.2588190451025213501 ) ) ;
#49588 = SURFACE_STYLE_FILL_AREA ( #14778 ) ;
#49589 = AXIS2_PLACEMENT_3D ( 'NONE', #77023, #134240, #89299 ) ;
#49590 = ORIENTED_EDGE ( 'NONE', *, *, #18023, .F. ) ;
#49591 = EDGE_LOOP ( 'NONE', ( #5125, #9760, #105924, #91995 ) ) ;
#49592 = CARTESIAN_POINT ( 'NONE',  ( 34.42499999999998295, 0.000000000000000000, 4.500000000000000888 ) ) ;
#49593 = FACE_OUTER_BOUND ( 'NONE', #96995, .T. ) ;
#49594 = VECTOR ( 'NONE', #34717, 1000.000000000000227 ) ;
#49595 = CARTESIAN_POINT ( 'NONE',  ( 4.062069808101886004, -7.934999999999991616, -2.126176841940955242 ) ) ;
#49596 = CARTESIAN_POINT ( 'NONE',  ( 31.49999999999978684, -2.947814304570800736, 5.000000000000000000 ) ) ;
#49597 = AXIS2_PLACEMENT_3D ( 'NONE', #88779, #102511, #35118 ) ;
#49598 = CARTESIAN_POINT ( 'NONE',  ( 0.000000000000000000, 0.000000000000000000, 5.000000000000000000 ) ) ;
#49599 = LINE ( 'NONE', #8163, #103831 ) ;
#49600 = DIRECTION ( 'NONE',  ( 0.6830127018922181881, 0.6830127018922202975, -0.2588190451025214056 ) ) ;
#49601 = ORIENTED_EDGE ( 'NONE', *, *, #50450, .F. ) ;
#49602 = EDGE_CURVE ( 'NONE', #109637, #24531, #66354, .T. ) ;
#49603 = DIRECTION ( 'NONE',  ( -0.3543493200069162685, -0.000000000000000000, -0.9351131265310288487 ) ) ;
#49604 = LINE ( 'NONE', #3872, #2947 ) ;
#49605 = AXIS2_PLACEMENT_3D ( 'NONE', #7662, #29419, #85956 ) ;
#49606 = DIRECTION ( 'NONE',  ( 0.7071067811865486830, -0.7071067811865464625, -0.000000000000000000 ) ) ;
#49607 = CARTESIAN_POINT ( 'NONE',  ( 50.37043019189811588, -3.055000000000001936, 5.291415217122918513 ) ) ;
#49608 =( BOUNDED_CURVE ( )  B_SPLINE_CURVE ( 2, ( #33477, #67528, #56675, #87111, #21129, #121847, #111723, #12389, #100837, #43599, #109569 ),
 .UNSPECIFIED., .F., .F. ) 
 B_SPLINE_CURVE_WITH_KNOTS ( ( 3, 2, 2, 2, 2, 3 ),
 ( 0.7500000000000001110, 0.7583333333333334147, 0.7666666666666668295, 0.7750000000000000222, 0.7833333333333333259, 0.7910556609953053320 ),
 .UNSPECIFIED. ) 
 CURVE ( )  GEOMETRIC_REPRESENTATION_ITEM ( )  RATIONAL_B_SPLINE_CURVE ( ( 0.9999999999999995559, 0.9659258262890687563, 1.000000000000000000, 0.9659258262890683122, 1.000000000000000000, 0.9659258262890683122, 1.000000000000000000, 0.9659258262890683122, 1.000000000000000000, 0.9684241678951878152, 0.9953696770014417439 ) ) 
 REPRESENTATION_ITEM ( '' )  );
#49609 = CARTESIAN_POINT ( 'NONE',  ( -33.18398860626899705, 28.73617430169810305, 5.000000000000000000 ) ) ;
#49610 = EDGE_CURVE ( 'NONE', #51562, #19565, #35162, .T. ) ;
#49611 = ADVANCED_FACE ( 'NONE', ( #112686 ), #46782, .T. ) ;
#49612 = VECTOR ( 'NONE', #132267, 1000.000000000000000 ) ;
#49613 = VERTEX_POINT ( 'NONE', #122855 ) ;
#49614 = DIRECTION ( 'NONE',  ( 0.000000000000000000, 0.000000000000000000, 1.000000000000000000 ) ) ;
#49615 = ORIENTED_EDGE ( 'NONE', *, *, #121071, .T. ) ;
#49616 = VERTEX_POINT ( 'NONE', #23537 ) ;
#49617 = AXIS2_PLACEMENT_3D ( 'NONE', #100011, #44219, #129224 ) ;
#49618 = DIRECTION ( 'NONE',  ( 0.7071067811865486830, -0.7071067811865464625, -0.000000000000000000 ) ) ;
#49619 = EDGE_CURVE ( 'NONE', #8014, #77672, #74009, .T. ) ;
#49620 = FACE_OUTER_BOUND ( 'NONE', #7132, .T. ) ;
#49621 = LINE ( 'NONE', #106065, #99805 ) ;
#49622 = CARTESIAN_POINT ( 'NONE',  ( -13.49999999999990585, 9.052185695429077583, 5.000000000000000000 ) ) ;
#49623 = EDGE_CURVE ( 'NONE', #57693, #71285, #41358, .T. ) ;
#49624 = FACE_OUTER_BOUND ( 'NONE', #23072, .T. ) ;
#49625 = PRESENTATION_STYLE_ASSIGNMENT (( #16203 ) ) ;
#49626 = ORIENTED_EDGE ( 'NONE', *, *, #114496, .F. ) ;
#49627 = EDGE_CURVE ( 'NONE', #28687, #4133, #103921, .T. ) ;
#49628 = FACE_OUTER_BOUND ( 'NONE', #122760, .T. ) ;
#49629 = DIRECTION ( 'NONE',  ( -0.7071067811865486830, -0.7071067811865464625, 0.000000000000000000 ) ) ;
#49630 = PLANE ( 'NONE',  #117267 ) ;
#49631 = PLANE ( 'NONE',  #119160 ) ;
#49632 = CARTESIAN_POINT ( 'NONE',  ( 104.4958603837962272, -3.974999999999998312, -6.884901960086286188 ) ) ;
#49633 = CARTESIAN_POINT ( 'NONE',  ( 68.47502705046289861, -5.819803920172572198, 5.819803920172572198 ) ) ;
#49634 = LINE ( 'NONE', #69971, #143409 ) ;
#49635 = EDGE_LOOP ( 'NONE', ( #105852, #81989, #79323, #34304 ) ) ;
#49636 = ORIENTED_EDGE ( 'NONE', *, *, #106212, .T. ) ;
#49637 = CARTESIAN_POINT ( 'NONE',  ( 61.22916666666665719, 7.950000000000001954, -2.130196079827421762 ) ) ;
#49638 = EDGE_CURVE ( 'NONE', #70270, #59222, #103231, .T. ) ;
#49639 = CARTESIAN_POINT ( 'NONE',  ( 0.000000000000000000, -21.72500000000000142, 4.500000000000000888 ) ) ;
#49640 = LINE ( 'NONE', #93819, #120306 ) ;
#49641 = DIRECTION ( 'NONE',  ( -0.3543493200069162685, -0.000000000000000000, -0.9351131265310288487 ) ) ;
#49642 = VERTEX_POINT ( 'NONE', #52246 ) ;
#49643 = ADVANCED_FACE ( 'NONE', ( #129085 ), #129803, .F. ) ;
#49644 = AXIS2_PLACEMENT_3D ( 'NONE', #22883, #33820, #133834 ) ;
#49645 = CARTESIAN_POINT ( 'NONE',  ( 11.99451991528749417, 28.92564299267946382, 4.000000000000000000 ) ) ;
#49646 = DIRECTION ( 'NONE',  ( 0.000000000000000000, 0.000000000000000000, 1.000000000000000000 ) ) ;
#49647 = CARTESIAN_POINT ( 'NONE',  ( 60.81293019189811133, -1.637169565754159617, -6.110000000000001208 ) ) ;
#49648 = LINE ( 'NONE', #93826, #129313 ) ;
#49649 = ORIENTED_EDGE ( 'NONE', *, *, #119738, .F. ) ;
#49650 = ORIENTED_EDGE ( 'NONE', *, *, #129720, .F. ) ;
#49651 = DIRECTION ( 'NONE',  ( -0.000000000000000000, -0.000000000000000000, 1.000000000000000000 ) ) ;
#49652 = FACE_OUTER_BOUND ( 'NONE', #60417, .T. ) ;
#49653 = PLANE ( 'NONE',  #109131 ) ;
#49654 = DIRECTION ( 'NONE',  ( -0.7071067811865486830, -0.7071067811865464625, -0.000000000000000000 ) ) ;
#49655 = DIRECTION ( 'NONE',  ( 0.7071067811865486830, -0.7071067811865464625, -0.000000000000000000 ) ) ;
#49657 = ORIENTED_EDGE ( 'NONE', *, *, #68045, .T. ) ;
#49656 = CARTESIAN_POINT ( 'NONE',  ( -17.01299345042646749, -0.9444868035190713274, -36.39086428169088094 ) ) ;
#49658 = LINE ( 'NONE', #61953, #66958 ) ;
#49659 = DIRECTION ( 'NONE',  ( 0.6830127018922180770, -0.6830127018922204085, -0.2588190451025213501 ) ) ;
#49660 = CARTESIAN_POINT ( 'NONE',  ( -17.51078643762690845, -27.52281430457043143, 5.000000000000000000 ) ) ;
#49661 = VECTOR ( 'NONE', #64674, 1000.000000000000000 ) ;
#49662 = CARTESIAN_POINT ( 'NONE',  ( 7.889826771117839144, -22.22500000000000142, 4.785647885939351198 ) ) ;
#49663 = ADVANCED_FACE ( 'NONE', ( #62432 ), #18897, .F. ) ;
#49664 = ORIENTED_EDGE ( 'NONE', *, *, #101176, .F. ) ;
#49665 = EDGE_CURVE ( 'NONE', #45698, #116876, #37279, .T. ) ;
#49666 =( GEOMETRIC_REPRESENTATION_CONTEXT ( 3 ) GLOBAL_UNCERTAINTY_ASSIGNED_CONTEXT ( ( #77950 ) ) GLOBAL_UNIT_ASSIGNED_CONTEXT ( ( #117504, #110905, #100779 ) ) REPRESENTATION_CONTEXT ( 'NONE', 'WORKASPACE' ) );
#49667 = ORIENTED_EDGE ( 'NONE', *, *, #63136, .T. ) ;
#49668 = DIRECTION ( 'NONE',  ( -0.7071067811865487940, 0.7071067811865463515, 0.000000000000000000 ) ) ;
#49669 = CARTESIAN_POINT ( 'NONE',  ( -12.18398860626900060, 28.73617430169795739, 5.000000000000000000 ) ) ;
#49670 = FACE_OUTER_BOUND ( 'NONE', #136146, .T. ) ;
#49671 = LINE ( 'NONE', #4632, #126513 ) ;
#49672 = ORIENTED_EDGE ( 'NONE', *, *, #55691, .F. ) ;
#49673 = VERTEX_POINT ( 'NONE', #128397 ) ;
#49674 = DIRECTION ( 'NONE',  ( 1.000000000000000000, 0.000000000000000000, 0.000000000000000000 ) ) ;
#49675 = CARTESIAN_POINT ( 'NONE',  ( -34.45011844616454511, 9.002304141593867826, 5.000000000000000888 ) ) ;
#49676 = EDGE_LOOP ( 'NONE', ( #107165, #48813, #137232, #108029, #137858, #135447, #11527, #121776, #30124, #116217, #68086, #64312, #37028, #120114, #53655, #118650, #30181, #65479 ) ) ;
#49677 = ORIENTED_EDGE ( 'NONE', *, *, #130652, .T. ) ;
#49678 = PLANE ( 'NONE',  #127796 ) ;
#49679 = EDGE_LOOP ( 'NONE', ( #82156, #86721, #28897, #66313 ) ) ;
#49680 = LINE ( 'NONE', #61295, #117395 ) ;
#49681 = LINE ( 'NONE', #94560, #142017 ) ;
#49682 = AXIS2_PLACEMENT_3D ( 'NONE', #106560, #130512, #107300 ) ;
#49683 = FACE_BOUND ( 'NONE', #6999, .T. ) ;
#49684 = FACE_OUTER_BOUND ( 'NONE', #29086, .T. ) ;
#49685 = CARTESIAN_POINT ( 'NONE',  ( 11.30840764549667554, -2.499999999999998224, 0.000000000000000000 ) ) ;
#49686 = DIRECTION ( 'NONE',  ( -0.7071067811865486830, -0.7071067811865464625, -0.000000000000000000 ) ) ;
#49688 = VERTEX_POINT ( 'NONE', #135874 ) ;
#49687 = DIRECTION ( 'NONE',  ( -0.6830127018922181881, 0.6830127018922202975, -0.2588190451025214056 ) ) ;
#49689 = VECTOR ( 'NONE', #28116, 1000.000000000000000 ) ;
#49690 = LINE ( 'NONE', #104000, #127382 ) ;
#49691 = PRODUCT_CONTEXT ( 'NONE', #13292, 'mechanical' ) ;
#49692 = ORIENTED_EDGE ( 'NONE', *, *, #63158, .F. ) ;
#49693 = AXIS2_PLACEMENT_3D ( 'NONE', #32805, #124079, #11703 ) ;
#49695 = VERTEX_POINT ( 'NONE', #3879 ) ;
#49694 = VECTOR ( 'NONE', #110841, 999.9999999999998863 ) ;
#49696 = CARTESIAN_POINT ( 'NONE',  ( 92.80793019189812298, -6.109999999999998543, 1.637169565754158507 ) ) ;
#49697 = ORIENTED_EDGE ( 'NONE', *, *, #55282, .T. ) ;
#49698 = PLANE ( 'NONE',  #72142 ) ;
#49699 = EDGE_CURVE ( 'NONE', #97631, #89986, #29073, .T. ) ;
#49700 = CARTESIAN_POINT ( 'NONE',  ( 23.99999999999983302, -21.41253812416053748, 4.000000000000000000 ) ) ;
#49701 = VECTOR ( 'NONE', #133147, 1000.000000000000227 ) ;
#49702 = CARTESIAN_POINT ( 'NONE',  ( -24.48921356237309510, -27.52281430457072631, 5.000000000000000000 ) ) ;
#49703 = ORIENTED_EDGE ( 'NONE', *, *, #96467, .F. ) ;
#49704 = CARTESIAN_POINT ( 'NONE',  ( 4.499999999999972466, -11.94781430457070925, 5.000000000000000000 ) ) ;
#49705 = DIRECTION ( 'NONE',  ( 0.000000000000000000, -1.000000000000000000, 0.000000000000000000 ) ) ;
#49706 = CARTESIAN_POINT ( 'NONE',  ( -72.18398860626899705, 28.73617430169837661, 5.000000000000000000 ) ) ;
#49708 = CARTESIAN_POINT ( 'NONE',  ( 13.11547925347946908, 3.815643823912585386, 4.000000000000000000 ) ) ;
#49707 = DIRECTION ( 'NONE',  ( 0.3543493200069162685, -0.000000000000000000, -0.9351131265310288487 ) ) ;
#49709 = DIRECTION ( 'NONE',  ( -0.7071067811865487940, 0.7071067811865463515, -0.000000000000000000 ) ) ;
#49710 = DIRECTION ( 'NONE',  ( -0.6830127018922181881, 0.6830127018922202975, -0.2588190451025214056 ) ) ;
#49711 = CARTESIAN_POINT ( 'NONE',  ( -26.99999999999981881, 2.342191155542426628, -5.001666872980022660 ) ) ;
#49712 = VERTEX_POINT ( 'NONE', #39983 ) ;
#49713 = DIRECTION ( 'NONE',  ( -0.6830127018922180770, -0.6830127018922204085, -0.2588190451025213501 ) ) ;
#49714 = CARTESIAN_POINT ( 'NONE',  ( 15.29974487139158867, -27.71228299555216879, 4.000000000000000000 ) ) ;
#49715 = ADVANCED_FACE ( 'NONE', ( #40672 ), #139291, .F. ) ;
#49716 = ORIENTED_EDGE ( 'NONE', *, *, #36466, .F. ) ;
#49717 = VERTEX_POINT ( 'NONE', #84201 ) ;
#49718 = ADVANCED_FACE ( 'NONE', ( #125730 ), #74744, .F. ) ;
#49719 = ADVANCED_FACE ( 'NONE', ( #118925 ), #84876, .F. ) ;
#49720 = ORIENTED_EDGE ( 'NONE', *, *, #141309, .F. ) ;
#49721 = CARTESIAN_POINT ( 'NONE',  ( 44.47959685856476852, 6.109999999999999432, 1.637169565754164280 ) ) ;
#49722 = VERTEX_POINT ( 'NONE', #3200 ) ;
#49723 = EDGE_CURVE ( 'NONE', #92832, #8140, #47490, .T. ) ;
#49724 = EDGE_CURVE ( 'NONE', #80852, #32222, #124992, .T. ) ;
#49725 = CARTESIAN_POINT ( 'NONE',  ( 12.00413961620377279, -3.047499999999994547, 5.278424836066145431 ) ) ;
#49726 = CARTESIAN_POINT ( 'NONE',  ( -8.727265903332346753, 10.25892755801883638, -28.67759622474984127 ) ) ;
#49727 = ORIENTED_EDGE ( 'NONE', *, *, #85923, .F. ) ;
#49728 = EDGE_CURVE ( 'NONE', #1800, #132295, #114118, .T. ) ;
#49729 = CARTESIAN_POINT ( 'NONE',  ( 14.67183060077636725, -21.74070752338406720, 4.000000000000000000 ) ) ;
#49730 = EDGE_LOOP ( 'NONE', ( #49743, #127015, #55780, #117215 ) ) ;
#49731 = LINE ( 'NONE', #19907, #117 ) ;
#49732 = LINE ( 'NONE', #137436, #137843 ) ;
#49734 = ORIENTED_EDGE ( 'NONE', *, *, #14885, .F. ) ;
#49733 = CARTESIAN_POINT ( 'NONE',  ( 17.99999999999987566, -16.60178936734446964, 0.8616154019347914694 ) ) ;
#49735 = ORIENTED_EDGE ( 'NONE', *, *, #56252, .T. ) ;
#49736 = AXIS2_PLACEMENT_3D ( 'NONE', #107946, #22371, #75370 ) ;
#49737 = DIRECTION ( 'NONE',  ( 0.000000000000000000, -1.000000000000000000, 0.000000000000000000 ) ) ;
#49738 = CARTESIAN_POINT ( 'NONE',  ( -14.08979869950237251, -1.618973607074043919, -40.00000000000000000 ) ) ;
#49739 = EDGE_CURVE ( 'NONE', #7006, #14902, #59761, .T. ) ;
#49740 = ORIENTED_EDGE ( 'NONE', *, *, #50219, .F. ) ;
#49741 = CARTESIAN_POINT ( 'NONE',  ( 1.499999999999994449, 5.696342897626511359, -7.587980461218396755 ) ) ;
#49742 = ORIENTED_EDGE ( 'NONE', *, *, #59547, .T. ) ;
#49743 = ORIENTED_EDGE ( 'NONE', *, *, #75596, .T. ) ;
#49744 = EDGE_LOOP ( 'NONE', ( #3808, #92471, #120229, #77743 ) ) ;
#49745 = EDGE_LOOP ( 'NONE', ( #75273, #51244, #87329, #58382 ) ) ;
#49746 = LINE ( 'NONE', #83807, #716 ) ;
#49747 = EDGE_CURVE ( 'NONE', #23427, #50436, #92340, .T. ) ;
#49748 = DIRECTION ( 'NONE',  ( -0.7071067811865487940, 0.7071067811865463515, 0.000000000000000000 ) ) ;
#49749 = DIRECTION ( 'NONE',  ( 0.3543493200069162685, -0.000000000000000000, -0.9351131265310288487 ) ) ;
#49750 = CARTESIAN_POINT ( 'NONE',  ( -48.48921356237309510, -27.52281430457089328, 5.000000000000000000 ) ) ;
#49751 = ORIENTED_EDGE ( 'NONE', *, *, #26794, .T. ) ;
#49752 = CARTESIAN_POINT ( 'NONE',  ( 23.51078643762690490, -27.52281430457038880, 5.000000000000000000 ) ) ;
#49753 = VERTEX_POINT ( 'NONE', #11563 ) ;
#49754 = EDGE_CURVE ( 'NONE', #31683, #141054, #701, .T. ) ;
#49755 = PLANE ( 'NONE',  #33266 ) ;
#49756 = CIRCLE ( 'NONE', #126116, 9.119999999999999218 ) ;
#49757 = PLANE ( 'NONE',  #108620 ) ;
#49758 = FACE_OUTER_BOUND ( 'NONE', #82982, .T. ) ;
#49759 = CARTESIAN_POINT ( 'NONE',  ( 33.29974487139158867, -27.71228299555229313, 4.000000000000000000 ) ) ;
#49760 =( BOUNDED_CURVE ( )  B_SPLINE_CURVE ( 3, ( #134864, #89880, #34815, #123266 ),
 .UNSPECIFIED., .F., .T. ) 
 B_SPLINE_CURVE_WITH_KNOTS ( ( 4, 4 ),
 ( 5.143245962375949887, 6.645403452391246191 ),
 .UNSPECIFIED. ) 
 CURVE ( )  GEOMETRIC_REPRESENTATION_ITEM ( )  RATIONAL_B_SPLINE_CURVE ( ( 1.000000000000000000, 0.8206354192515208368, 0.8206354192515208368, 1.000000000000000000 ) ) 
 REPRESENTATION_ITEM ( '' )  );
#49761 = DIRECTION ( 'NONE',  ( -1.000000000000000000, -0.000000000000000000, -0.000000000000000000 ) ) ;
#49762 = VERTEX_POINT ( 'NONE', #54424 ) ;
#49763 = AXIS2_PLACEMENT_3D ( 'NONE', #100938, #56779, #22632 ) ;
#49764 = EDGE_LOOP ( 'NONE', ( #72230, #76710, #23013, #109519 ) ) ;
#49766 = VERTEX_POINT ( 'NONE', #108732 ) ;
#49765 = EDGE_CURVE ( 'NONE', #38741, #72729, #32654, .T. ) ;
#49767 = DIRECTION ( 'NONE',  ( 0.7071067811865487940, 0.7071067811865463515, 0.000000000000000000 ) ) ;
#49768 = CARTESIAN_POINT ( 'NONE',  ( -2.999999999999975575, -18.03360074219755660, 5.000000000000000000 ) ) ;
#49769 = DIRECTION ( 'NONE',  ( 1.000000000000000000, 0.000000000000000000, -0.000000000000000000 ) ) ;
#49770 = LINE ( 'NONE', #36032, #10300 ) ;
#49771 = CARTESIAN_POINT ( 'NONE',  ( 0.2480159638836071934, -51.74944211519454029, -38.65549799471448011 ) ) ;
#49772 = CARTESIAN_POINT ( 'NONE',  ( 77.78709685856478018, 3.054999999999997939, 5.291415217122920289 ) ) ;
#49773 = CARTESIAN_POINT ( 'NONE',  ( 74.16252705046288440, 7.949999999999998401, 1.460391307983218338E-15 ) ) ;
#49774 = EDGE_CURVE ( 'NONE', #11133, #61053, #89172, .T. ) ;
#49775 = CARTESIAN_POINT ( 'NONE',  ( -25.39999999999996305, 0.000000000000000000, 0.000000000000000000 ) ) ;
#49776 = VECTOR ( 'NONE', #102701, 1000.000000000000000 ) ;
#49777 = DIRECTION ( 'NONE',  ( 0.6830127018922180770, -0.6830127018922204085, -0.2588190451025214056 ) ) ;
#49778 = LINE ( 'NONE', #72265, #141400 ) ;
#49779 = EDGE_CURVE ( 'NONE', #73748, #68933, #142139, .T. ) ;
#49780 = DIRECTION ( 'NONE',  ( -0.7071067811865487940, 0.7071067811865463515, 0.000000000000000000 ) ) ;
#49781 = ORIENTED_EDGE ( 'NONE', *, *, #134996, .F. ) ;
#49782 = DIRECTION ( 'NONE',  ( -0.7071067811865487940, 0.7071067811865463515, 0.000000000000000000 ) ) ;
#49783 = ORIENTED_EDGE ( 'NONE', *, *, #91721, .F. ) ;
#49784 = ADVANCED_FACE ( 'NONE', ( #42824 ), #87023, .F. ) ;
#49785 = CARTESIAN_POINT ( 'NONE',  ( -34.92500000000001137, 22.22500000000000142, 4.000000000000000000 ) ) ;
#49787 = ORIENTED_EDGE ( 'NONE', *, *, #45314, .T. ) ;
#49786 = CARTESIAN_POINT ( 'NONE',  ( -5.207106781186503497, 15.75929247661555976, 5.000000000000000000 ) ) ;
#49788 = DIRECTION ( 'NONE',  ( -0.000000000000000000, 0.3543493200069153248, 0.9351131265310292928 ) ) ;
#49789 = LINE ( 'NONE', #105542, #47248 ) ;
#49790 = ORIENTED_EDGE ( 'NONE', *, *, #4391, .F. ) ;
#49791 = ORIENTED_EDGE ( 'NONE', *, *, #4006, .T. ) ;
#49792 = DIRECTION ( 'NONE',  ( -1.000000000000000000, -1.369518533665900312E-16, 0.000000000000000000 ) ) ;
#49793 = VERTEX_POINT ( 'NONE', #132708 ) ;
#49794 = CARTESIAN_POINT ( 'NONE',  ( -72.18398860626899705, 28.73617430169837661, 5.000000000000000000 ) ) ;
#49795 = VECTOR ( 'NONE', #107366, 999.9999999999998863 ) ;
#49796 = CARTESIAN_POINT ( 'NONE',  ( 90.20419371712957002, -6.884901960086285300, -3.975000000000000089 ) ) ;
#49798 = VECTOR ( 'NONE', #91609, 999.9999999999998863 ) ;
#49797 = DIRECTION ( 'NONE',  ( -0.7071067811865487940, 0.7071067811865463515, -0.000000000000000000 ) ) ;
#49799 = CIRCLE ( 'NONE', #135576, 28.00000000000003197 ) ;
#49800 = SURFACE_STYLE_FILL_AREA ( #93267 ) ;
#49801 = EDGE_LOOP ( 'NONE', ( #20979, #70193, #75415, #95591 ) ) ;
#49802 = VECTOR ( 'NONE', #53593, 999.9999999999998863 ) ;
#49803 = ADVANCED_FACE ( 'NONE', ( #42112 ), #43515, .F. ) ;
#49804 = DIRECTION ( 'NONE',  ( -0.6830127018922180770, -0.6830127018922204085, -0.2588190451025213501 ) ) ;
#49805 = LINE ( 'NONE', #92534, #6783 ) ;
#49806 = CARTESIAN_POINT ( 'NONE',  ( 24.06249999999999645, 4.461849672132300881, 4.461849672132299105 ) ) ;
#49807 = FACE_OUTER_BOUND ( 'NONE', #71010, .T. ) ;
#49808 = PLANE ( 'NONE',  #21308 ) ;
#49809 = ORIENTED_EDGE ( 'NONE', *, *, #100053, .T. ) ;
#49810 = EDGE_CURVE ( 'NONE', #6090, #39522, #78297, .T. ) ;
#49811 = DIRECTION ( 'NONE',  ( -0.5735764363510499342, -0.8191520442889891340, 0.000000000000000000 ) ) ;
#49812 = ORIENTED_EDGE ( 'NONE', *, *, #127406, .T. ) ;
#49813 = CARTESIAN_POINT ( 'NONE',  ( 85.16709685856477563, -3.055000000000000160, -5.291415217122921177 ) ) ;
#49814 = CARTESIAN_POINT ( 'NONE',  ( -27.18398860626900060, 28.73617430169806042, 5.000000000000000000 ) ) ;
#49815 = CARTESIAN_POINT ( 'NONE',  ( 16.74845587132414693, -11.24070752338416490, 10.39518518046005369 ) ) ;
#49816 = CARTESIAN_POINT ( 'NONE',  ( -26.99999999999980815, -0.03360074219773377668, 5.000000000000000000 ) ) ;
#49817 = VERTEX_POINT ( 'NONE', #55118 ) ;
#49818 = DIRECTION ( 'NONE',  ( 0.000000000000000000, 1.000000000000000000, 0.000000000000000000 ) ) ;
#49819 = CARTESIAN_POINT ( 'NONE',  ( -5.999999999999963585, -10.77435723561695902, -9.972017380717215218 ) ) ;
#49820 = ADVANCED_FACE ( 'NONE', ( #87735 ), #75442, .F. ) ;
#49821 = DIRECTION ( 'NONE',  ( 0.7071067811865487940, 0.7071067811865463515, -0.000000000000000000 ) ) ;
#49823 = EDGE_CURVE ( 'NONE', #80281, #3445, #66703, .T. ) ;
#49822 = CARTESIAN_POINT ( 'NONE',  ( 48.48921356237309510, -27.52281430457089328, 5.000000000000000000 ) ) ;
#49825 = EDGE_LOOP ( 'NONE', ( #32438, #121731, #69105, #53595 ) ) ;
#49824 = PLANE ( 'NONE',  #114588 ) ;
#49826 = LINE ( 'NONE', #83886, #90117 ) ;
#49827 = CARTESIAN_POINT ( 'NONE',  ( -22.96641869250914070, 7.680402717527123890, 4.333886692633072357 ) ) ;
#49828 = LINE ( 'NONE', #18557, #51674 ) ;
#49829 = LINE ( 'NONE', #17174, #28456 ) ;
#49830 = VERTEX_POINT ( 'NONE', #119613 ) ;
#49831 = ADVANCED_FACE ( 'NONE', ( #76892 ), #131970, .T. ) ;
#49832 = ORIENTED_EDGE ( 'NONE', *, *, #55648, .T. ) ;
#49833 = CARTESIAN_POINT ( 'NONE',  ( 77.72959685856477563, -6.110000000000000320, -1.637169565754161393 ) ) ;
#49834 = ORIENTED_EDGE ( 'NONE', *, *, #39241, .T. ) ;
#49835 = SURFACE_STYLE_FILL_AREA ( #59980 ) ;
#49836 = LINE ( 'NONE', #102775, #112808 ) ;
#49837 = LINE ( 'NONE', #48376, #50391 ) ;
#49838 = CARTESIAN_POINT ( 'NONE',  ( -53.99451991528749062, 28.92564299267975869, 4.000000000000000000 ) ) ;
#49839 = ORIENTED_EDGE ( 'NONE', *, *, #1541, .F. ) ;
#49840 = CARTESIAN_POINT ( 'NONE',  ( -12.69999999999998153, 3.061616997868383634E-16, -2.500000000000000444 ) ) ;
#49841 = DIRECTION ( 'NONE',  ( 0.3543493200069162685, -0.000000000000000000, -0.9351131265310288487 ) ) ;
#49842 = ADVANCED_FACE ( 'NONE', ( #98600 ), #97136, .F. ) ;
#49843 = EDGE_LOOP ( 'NONE', ( #70941, #88094, #75825, #130486, #80248, #19622 ) ) ;
#49844 = CARTESIAN_POINT ( 'NONE',  ( 1.055465189827180295, -0.8122627595889222452, 3.860239566300592617 ) ) ;
#49845 = CARTESIAN_POINT ( 'NONE',  ( 33.32919371712955581, -3.975000000000001865, 6.884901960086284411 ) ) ;
#49846 = CARTESIAN_POINT ( 'NONE',  ( 26.99451991528749417, 28.92564299267956685, 4.000000000000000000 ) ) ;
#49847 = ORIENTED_EDGE ( 'NONE', *, *, #2875, .F. ) ;
#49848 = VERTEX_POINT ( 'NONE', #121064 ) ;
#49849 = CARTESIAN_POINT ( 'NONE',  ( 65.45833333333332860, 3.974999999999997424, 6.884901960086288852 ) ) ;
#49850 = ADVANCED_FACE ( 'NONE', ( #108021 ), #64552, .T. ) ;
#49851 = DIRECTION ( 'NONE',  ( -0.6830127018922181881, 0.6830127018922202975, -0.2588190451025214056 ) ) ;
#49852 = CARTESIAN_POINT ( 'NONE',  ( 14.99451991528749595, 28.92564299267948513, 4.000000000000000000 ) ) ;
#49853 = CARTESIAN_POINT ( 'NONE',  ( 24.32816939922335564, -15.74070752338411694, 4.000000000000000000 ) ) ;
#49854 = CARTESIAN_POINT ( 'NONE',  ( 53.45419371712956291, 6.884901960086283523, 3.975000000000002753 ) ) ;
#49855 = DIRECTION ( 'NONE',  ( -0.7071067811865486830, 0.7071067811865464625, 0.000000000000000000 ) ) ;
#49857 = ORIENTED_EDGE ( 'NONE', *, *, #52294, .T. ) ;
#49856 = CIRCLE ( 'NONE', #130883, 2.500000000000000444 ) ;
#49858 = VERTEX_POINT ( 'NONE', #59424 ) ;
#49859 = ORIENTED_EDGE ( 'NONE', *, *, #79441, .F. ) ;
#49860 = VERTEX_POINT ( 'NONE', #48510 ) ;
#49861 = CARTESIAN_POINT ( 'NONE',  ( -38.99451991528749062, 28.92564299267965211, 4.000000000000000000 ) ) ;
#49862 = EDGE_LOOP ( 'NONE', ( #140864, #32512, #129138, #26453 ) ) ;
#49863 = AXIS2_PLACEMENT_3D ( 'NONE', #107328, #119607, #108013 ) ;
#49864 =( NAMED_UNIT ( * ) PLANE_ANGLE_UNIT ( ) SI_UNIT ( $, .RADIAN. ) );
#49865 = DIRECTION ( 'NONE',  ( 0.7071067811865487940, 0.7071067811865463515, 0.000000000000000000 ) ) ;
#49867 = EDGE_CURVE ( 'NONE', #80017, #138017, #15143, .T. ) ;
#49866 = DIRECTION ( 'NONE',  ( -0.000000000000000000, 0.3543493200069152138, -0.9351131265310292928 ) ) ;
#49868 = CARTESIAN_POINT ( 'NONE',  ( 12.69999999999999574, -35.15000000000000568, -39.50000000000000000 ) ) ;
#49869 = CARTESIAN_POINT ( 'NONE',  ( 10.49999999999992539, -8.947814304570741228, 5.000000000000000000 ) ) ;
#49870 = ORIENTED_EDGE ( 'NONE', *, *, #61794, .F. ) ;
#49871 = CARTESIAN_POINT ( 'NONE',  ( 23.00840764549667483, 9.139736423841732040E-16, 0.000000000000000000 ) ) ;
#49872 = CARTESIAN_POINT ( 'NONE',  ( -19.49999999999987210, -2.777013188829482893, 4.549262955118030582 ) ) ;
#49873 = ORIENTED_EDGE ( 'NONE', *, *, #54657, .F. ) ;
#49874 = CARTESIAN_POINT ( 'NONE',  ( -18.12147316337136260, -20.24070752338408141, 7.412974875817832654 ) ) ;
#49875 = VERTEX_POINT ( 'NONE', #25316 ) ;
#49877 = VERTEX_POINT ( 'NONE', #92712 ) ;
#49876 = EDGE_CURVE ( 'NONE', #115809, #18442, #117895, .T. ) ;
#49878 = ADVANCED_FACE ( 'NONE', ( #23917 ), #23158, .F. ) ;
#49879 = DIRECTION ( 'NONE',  ( 0.6830127018922181881, 0.6830127018922202975, -0.2588190451025214056 ) ) ;
#49880 = VERTEX_POINT ( 'NONE', #13708 ) ;
#49881 = ORIENTED_EDGE ( 'NONE', *, *, #34840, .F. ) ;
#49882 = CARTESIAN_POINT ( 'NONE',  ( 74.08376352523143282, -6.110000000000001208, -3.741295971395164515E-16 ) ) ;
#49883 = EDGE_LOOP ( 'NONE', ( #101923, #132608, #41299, #91491 ) ) ;
#49884 = VECTOR ( 'NONE', #99324, 1000.000000000000000 ) ;
#49885 = ADVANCED_FACE ( 'NONE', ( #136947 ), #37658, .T. ) ;
#49886 = ADVANCED_FACE ( 'NONE', ( #81897 ), #81159, .T. ) ;
#49887 =( NAMED_UNIT ( * ) PLANE_ANGLE_UNIT ( ) SI_UNIT ( $, .RADIAN. ) );
#49888 = VECTOR ( 'NONE', #58033, 999.9999999999998863 ) ;
#49890 = EDGE_CURVE ( 'NONE', #19532, #25917, #134843, .T. ) ;
#49889 = CARTESIAN_POINT ( 'NONE',  ( 8.999999999999941380, -6.412538124160696462, 4.000000000000000000 ) ) ;
#49891 = CARTESIAN_POINT ( 'NONE',  ( 108.5004301918981184, -3.055000000000002380, 5.291415217122920289 ) ) ;
#49892 = DIRECTION ( 'NONE',  ( 0.7071067811865487940, 0.7071067811865463515, 0.000000000000000000 ) ) ;
#49893 = AXIS2_PLACEMENT_3D ( 'NONE', #27385, #92645, #136887 ) ;
#49894 = EDGE_CURVE ( 'NONE', #133528, #22423, #92007, .T. ) ;
#49896 = FACE_OUTER_BOUND ( 'NONE', #58634, .T. ) ;
#49895 = CARTESIAN_POINT ( 'NONE',  ( 129.0581452878471680, 0.000000000000000000, -7.029999999999999361 ) ) ;
#49897 = DIRECTION ( 'NONE',  ( 1.000000000000000000, 1.224606353822377258E-16, 0.000000000000000000 ) ) ;
#49898 = EDGE_CURVE ( 'NONE', #108369, #135769, #67436, .T. ) ;
#49899 = PLANE ( 'NONE',  #125724 ) ;
#49900 = EDGE_CURVE ( 'NONE', #126702, #1467, #35538, .T. ) ;
#49901 = ORIENTED_EDGE ( 'NONE', *, *, #73956, .F. ) ;
#49902 = LINE ( 'NONE', #39742, #112852 ) ;
#49903 = LINE ( 'NONE', #107100, #79926 ) ;
#49904 = ORIENTED_EDGE ( 'NONE', *, *, #111270, .F. ) ;
#49905 = ORIENTED_EDGE ( 'NONE', *, *, #58758, .F. ) ;
#49906 = DIRECTION ( 'NONE',  ( 0.6830127018922181881, 0.6830127018922202975, -0.2588190451025214056 ) ) ;
#49907 = EDGE_LOOP ( 'NONE', ( #34151, #90792, #52924, #28309 ) ) ;
#49908 = FACE_OUTER_BOUND ( 'NONE', #63228, .T. ) ;
#49909 = CARTESIAN_POINT ( 'NONE',  ( 12.35051985313232237, 2.500000000000000888, 0.000000000000000000 ) ) ;
#49910 = EDGE_CURVE ( 'NONE', #5604, #60822, #12303, .T. ) ;
#49911 = PLANE ( 'NONE',  #129693 ) ;
#49912 = CARTESIAN_POINT ( 'NONE',  ( 128.8219055147128529, -52.14999999999999147, -41.05261164187028555 ) ) ;
#49913 = VERTEX_POINT ( 'NONE', #34795 ) ;
#49914 = DIRECTION ( 'NONE',  ( 0.000000000000000000, -1.000000000000000000, 0.000000000000000000 ) ) ;
#49915 = ORIENTED_EDGE ( 'NONE', *, *, #100191, .T. ) ;
#49916 = EDGE_CURVE ( 'NONE', #40999, #76459, #90600, .T. ) ;
#49917 = CARTESIAN_POINT ( 'NONE',  ( 4.645403141435220817, -2.126176841940958351, -7.934999999999989839 ) ) ;
#49918 = CARTESIAN_POINT ( 'NONE',  ( 90.78752705046288440, 0.000000000000000000, -7.949999999999998401 ) ) ;
#49919 = PLANE ( 'NONE',  #122253 ) ;
#49920 = DIRECTION ( 'NONE',  ( 0.000000000000000000, -0.000000000000000000, 1.000000000000000000 ) ) ;
#49921 = ORIENTED_EDGE ( 'NONE', *, *, #37158, .T. ) ;
#49922 = ORIENTED_EDGE ( 'NONE', *, *, #54979, .F. ) ;
#49923 = VERTEX_POINT ( 'NONE', #101455 ) ;
#49924 = CARTESIAN_POINT ( 'NONE',  ( -19.17183060077633172, -8.240707523384193323, 4.000000000000000000 ) ) ;
#49925 = CARTESIAN_POINT ( 'NONE',  ( 4.288407645496676857, 2.500000000000002220, 3.061616997868384620E-16 ) ) ;
#49926 = FACE_OUTER_BOUND ( 'NONE', #69382, .T. ) ;
#49927 = LINE ( 'NONE', #94106, #56635 ) ;
#49928 = CARTESIAN_POINT ( 'NONE',  ( -28.49999999999979394, 19.46639925780206326, 5.000000000000000000 ) ) ;
#49929 = CARTESIAN_POINT ( 'NONE',  ( 17.29387692260792164, 22.22500000000000142, 4.000000000000000000 ) ) ;
#49930 = EDGE_CURVE ( 'NONE', #123895, #117989, #57679, .T. ) ;
#49931 = CARTESIAN_POINT ( 'NONE',  ( 6.096670641874017527, -2.240707523384260824, 15.26439735382753859 ) ) ;
#49932 = CARTESIAN_POINT ( 'NONE',  ( 11.81601139373100651, 28.73617430169779041, 5.000000000000000000 ) ) ;
#49933 = LINE ( 'NONE', #113741, #37271 ) ;
#49934 = EDGE_CURVE ( 'NONE', #131273, #88966, #108511, .T. ) ;
#49935 = ORIENTED_EDGE ( 'NONE', *, *, #26910, .F. ) ;
#49936 = CARTESIAN_POINT ( 'NONE',  ( 73.33333333333332860, -6.884901960086287964, 3.974999999999998312 ) ) ;
#49937 = LINE ( 'NONE', #127471, #86459 ) ;
#49938 = EDGE_LOOP ( 'NONE', ( #91812, #64922, #77080, #10961 ) ) ;
#49939 = EDGE_CURVE ( 'NONE', #124008, #52318, #95574, .T. ) ;
#49940 = CARTESIAN_POINT ( 'NONE',  ( 1.499999999999988232, -16.53360074219757792, 5.000000000000000000 ) ) ;
#49942 = ORIENTED_EDGE ( 'NONE', *, *, #62698, .F. ) ;
#49941 = DIRECTION ( 'NONE',  ( 0.000000000000000000, -1.000000000000000000, 0.000000000000000000 ) ) ;
#49943 = DIRECTION ( 'NONE',  ( -0.7071067811865486830, -0.7071067811865464625, 0.000000000000000000 ) ) ;
#49944 = CARTESIAN_POINT ( 'NONE',  ( -2.803796552228843275, -22.22500000000000142, 17.17192473999973146 ) ) ;
#49945 = ORIENTED_EDGE ( 'NONE', *, *, #10257, .T. ) ;
#49946 = FACE_OUTER_BOUND ( 'NONE', #84476, .T. ) ;
#49947 = ORIENTED_EDGE ( 'NONE', *, *, #101707, .F. ) ;
#49948 = CARTESIAN_POINT ( 'NONE',  ( -22.82816939922337696, 15.75929247661555976, 4.000000000000000000 ) ) ;
#49949 = DIRECTION ( 'NONE',  ( -1.000000000000000000, -0.000000000000000000, -0.000000000000000000 ) ) ;
#49950 = CARTESIAN_POINT ( 'NONE',  ( 118.3500270504628986, -5.819803920172572198, -5.819803920172572198 ) ) ;
#49951 = DIRECTION ( 'NONE',  ( -0.7071067811865487940, 0.7071067811865463515, 0.000000000000000000 ) ) ;
#49952 = CARTESIAN_POINT ( 'NONE',  ( 8.816011393731004731, 28.73617430169781173, 5.000000000000000000 ) ) ;
#49953 = AXIS2_PLACEMENT_3D ( 'NONE', #67863, #46094, #44688 ) ;
#49954 = EDGE_CURVE ( 'NONE', #142188, #80902, #139836, .T. ) ;
#49955 = LINE ( 'NONE', #136944, #113936 ) ;
#49956 =( LENGTH_UNIT ( ) NAMED_UNIT ( * ) SI_UNIT ( .MILLI., .METRE. ) );
#49957 = CARTESIAN_POINT ( 'NONE',  ( 17.39159235450332019, 9.902892378096218942E-16, 0.000000000000000000 ) ) ;
#49958 = CARTESIAN_POINT ( 'NONE',  ( 28.27040314143521726, -7.934999999999989839, 2.126176841940957907 ) ) ;
#49959 = CARTESIAN_POINT ( 'NONE',  ( 11.35373647476855297, -5.808823158059035485, -5.808823158059033709 ) ) ;
#49960 = DIRECTION ( 'NONE',  ( -1.000000000000000000, 0.000000000000000000, 0.000000000000000000 ) ) ;
#49961 = DIRECTION ( 'NONE',  ( -0.000000000000000000, 0.3543493200069153248, 0.9351131265310292928 ) ) ;
#49962 = DIRECTION ( 'NONE',  ( -0.7071067811865487940, 0.7071067811865463515, -0.000000000000000000 ) ) ;
#49963 = EDGE_LOOP ( 'NONE', ( #118153, #67638, #135694, #65603 ) ) ;
#49964 = ORIENTED_EDGE ( 'NONE', *, *, #16286, .F. ) ;
#49965 = CARTESIAN_POINT ( 'NONE',  ( 83.10416666666668561, 2.130196079827422206, 7.950000000000001954 ) ) ;
#49967 = EDGE_LOOP ( 'NONE', ( #139094, #130505, #64702, #35282, #1917, #114667 ) ) ;
#49966 = SURFACE_SIDE_STYLE ('',( #5700 ) ) ;
#49968 = ORIENTED_EDGE ( 'NONE', *, *, #131135, .F. ) ;
#49969 = EDGE_CURVE ( 'NONE', #64566, #123173, #16572, .T. ) ;
#49970 =( NAMED_UNIT ( * ) PLANE_ANGLE_UNIT ( ) SI_UNIT ( $, .RADIAN. ) );
#49971 = CARTESIAN_POINT ( 'NONE',  ( 21.18398860626899349, 28.73617430169802134, 5.000000000000000000 ) ) ;
#49972 = DIRECTION ( 'NONE',  ( -0.6830127018922181881, 0.6830127018922202975, -0.2588190451025214056 ) ) ;
#49973 = EDGE_LOOP ( 'NONE', ( #13790, #84954, #103102, #110712 ) ) ;
#49974 = LINE ( 'NONE', #94157, #13937 ) ;
#49975 = LINE ( 'NONE', #28214, #81161 ) ;
#49976 = FACE_OUTER_BOUND ( 'NONE', #92553, .T. ) ;
#49977 = CARTESIAN_POINT ( 'NONE',  ( -20.81601139373100295, 28.73617430169773002, 5.000000000000000000 ) ) ;
#49978 = EDGE_CURVE ( 'NONE', #101548, #70961, #40507, .T. ) ;
#49979 = FACE_OUTER_BOUND ( 'NONE', #70032, .T. ) ;
#49980 = DIRECTION ( 'NONE',  ( 1.000000000000000000, 1.084202172485504681E-16, 0.000000000000000000 ) ) ;
#49981 = DIRECTION ( 'NONE',  ( 0.000000000000000000, 0.000000000000000000, -1.000000000000000000 ) ) ;
#49982 = LINE ( 'NONE', #136979, #12789 ) ;
#49983 = CARTESIAN_POINT ( 'NONE',  ( 18.79653912142945060, 3.821174125832445049E-16, 0.000000000000000000 ) ) ;
#49984 = DIRECTION ( 'NONE',  ( -0.7071067811865486830, 0.7071067811865464625, 0.000000000000000000 ) ) ;
#49985 = CARTESIAN_POINT ( 'NONE',  ( 15.48921356237309510, -27.52281430457066236, 5.000000000000000000 ) ) ;
#49986 = VECTOR ( 'NONE', #35925, 1000.000000000000000 ) ;
#49987 = EDGE_LOOP ( 'NONE', ( #135416, #1385, #33543, #142902 ) ) ;
#49988 = ORIENTED_EDGE ( 'NONE', *, *, #74849, .T. ) ;
#49989 = AXIS2_PLACEMENT_3D ( 'NONE', #84252, #49491, #84930 ) ;
#49990 = CARTESIAN_POINT ( 'NONE',  ( 99.45876352523144703, 0.000000000000000000, -6.110000000000001208 ) ) ;
#49991 = EDGE_LOOP ( 'NONE', ( #127637, #110830, #24533, #79098 ) ) ;
#49992 = AXIS2_PLACEMENT_3D ( 'NONE', #5811, #28332, #77847 ) ;
#49993 = CARTESIAN_POINT ( 'NONE',  ( 122.6835989386367345, -43.14999999999999147, 34.92499999999998295 ) ) ;
#49994 = VECTOR ( 'NONE', #116438, 1000.000000000000000 ) ;
#49995 = CARTESIAN_POINT ( 'NONE',  ( 8.020833333333332149, -6.094999999999989981, -1.633150327867689322 ) ) ;
#49996 = ORIENTED_EDGE ( 'NONE', *, *, #126307, .T. ) ;
#49997 = CARTESIAN_POINT ( 'NONE',  ( 75.81250000000000000, 5.819803920172571310, 5.819803920172576639 ) ) ;
#49999 = EDGE_CURVE ( 'NONE', #7107, #9950, #69151, .T. ) ;
#49998 = CARTESIAN_POINT ( 'NONE',  ( -20.67183060077632817, 11.25929247661560595, 4.000000000000000000 ) ) ;
#50000 = CARTESIAN_POINT ( 'NONE',  ( 101.4120968585647802, 5.291415217122921177, -3.054999999999994831 ) ) ;
#50001 = EDGE_CURVE ( 'NONE', #34999, #3157, #71707, .T. ) ;
#50003 = EDGE_LOOP ( 'NONE', ( #142148, #127281, #13721 ) ) ;
#50002 = ADVANCED_BREP_SHAPE_REPRESENTATION ( '', ( #44753, #127880 ), #118637 ) ;
#50004 = LINE ( 'NONE', #141262, #111413 ) ;
#50005 = ORIENTED_EDGE ( 'NONE', *, *, #125806, .F. ) ;
#50006 = DIRECTION ( 'NONE',  ( 0.6830127018922180770, -0.6830127018922204085, -0.2588190451025213501 ) ) ;
#50007 = CARTESIAN_POINT ( 'NONE',  ( -53.99451991528749062, 28.92564299267975869, 4.000000000000000000 ) ) ;
#50008 = CARTESIAN_POINT ( 'NONE',  ( 32.48334561358932149, 22.22500000000000142, 4.500000000000000888 ) ) ;
#50009 = CARTESIAN_POINT ( 'NONE',  ( -38.99451991528749062, 28.92564299267965211, 4.000000000000000000 ) ) ;
#50010 = ORIENTED_EDGE ( 'NONE', *, *, #61919, .F. ) ;
#50011 = ORIENTED_EDGE ( 'NONE', *, *, #98673, .T. ) ;
#50012 = VERTEX_POINT ( 'NONE', #51377 ) ;
#50013 = CARTESIAN_POINT ( 'NONE',  ( 9.793339364578407924, 21.75929247661549937, 4.998822639870711626 ) ) ;
#50014 = EDGE_CURVE ( 'NONE', #5733, #54899, #46087, .T. ) ;
#50015 = DIRECTION ( 'NONE',  ( -0.7071067811865486830, -0.7071067811865464625, 0.000000000000000000 ) ) ;
#50016 = CARTESIAN_POINT ( 'NONE',  ( 10.71290314143521982, 3.967499999999992699, -6.871911579029513994 ) ) ;
#50017 = CARTESIAN_POINT ( 'NONE',  ( -42.48921356237308800, -27.52281430457085065, 5.000000000000000000 ) ) ;
#50018 =( LENGTH_UNIT ( ) NAMED_UNIT ( * ) SI_UNIT ( .MILLI., .METRE. ) );
#50019 = DIRECTION ( 'NONE',  ( -0.7071067811865486830, -0.7071067811865464625, -0.000000000000000000 ) ) ;
#50020 = VERTEX_POINT ( 'NONE', #104290 ) ;
#50021 = EDGE_LOOP ( 'NONE', ( #8664, #133479, #61771, #11907 ) ) ;
#50022 = CARTESIAN_POINT ( 'NONE',  ( 1.056153167756417099, -22.22500000000000142, -8.634603981399813222 ) ) ;
#50023 = ORIENTED_EDGE ( 'NONE', *, *, #115188, .F. ) ;
#50024 = ORIENTED_EDGE ( 'NONE', *, *, #103297, .T. ) ;
#50025 = CARTESIAN_POINT ( 'NONE',  ( 111.1829301918981230, -1.637169565754158951, -6.109999999999998543 ) ) ;
#50026 = PLANE ( 'NONE',  #23451 ) ;
#50027 = CARTESIAN_POINT ( 'NONE',  ( -15.18398860626900237, 28.73617430169797871, 5.000000000000000000 ) ) ;
#50028 = VERTEX_POINT ( 'NONE', #15827 ) ;
#50029 = PLANE ( 'NONE',  #108465 ) ;
#50030 = CARTESIAN_POINT ( 'NONE',  ( 21.18398860626899349, 28.73617430169802134, 5.000000000000000000 ) ) ;
#50031 = CARTESIAN_POINT ( 'NONE',  ( -81.18398860626899705, 28.73617430169844056, 5.000000000000000000 ) ) ;
#50032 = CARTESIAN_POINT ( 'NONE',  ( -32.99999999999977263, -21.03360074219752462, 5.000000000000000000 ) ) ;
#50033 = VERTEX_POINT ( 'NONE', #137682 ) ;
#50034 = DIRECTION ( 'NONE',  ( 0.7071067811865487940, 0.7071067811865463515, 0.000000000000000000 ) ) ;
#50035 = FACE_BOUND ( 'NONE', #53364, .T. ) ;
#50036 = ORIENTED_EDGE ( 'NONE', *, *, #109282, .F. ) ;
#50037 = DIRECTION ( 'NONE',  ( 0.6830127018922180770, 0.6830127018922202975, -0.2588190451025213501 ) ) ;
#50038 = CARTESIAN_POINT ( 'NONE',  ( 20.51159235450331764, -2.500000000000000444, 3.061616997868384620E-16 ) ) ;
#50039 = CARTESIAN_POINT ( 'NONE',  ( 27.48921356237309155, -27.52281430457074762, 5.000000000000000000 ) ) ;
#50040 = ORIENTED_EDGE ( 'NONE', *, *, #12188, .F. ) ;
#50041 = CARTESIAN_POINT ( 'NONE',  ( 1.629999999999999893, 0.4000000000000001887, -2.303088455023527104 ) ) ;
#50042 = ORIENTED_EDGE ( 'NONE', *, *, #64125, .F. ) ;
#50043 = ORIENTED_EDGE ( 'NONE', *, *, #105187, .T. ) ;
#50044 = ORIENTED_EDGE ( 'NONE', *, *, #75797, .F. ) ;
#50045 = VECTOR ( 'NONE', #118094, 1000.000000000000000 ) ;
#50046 = ADVANCED_FACE ( 'NONE', ( #115873 ), #28191, .F. ) ;
#50047 = CARTESIAN_POINT ( 'NONE',  ( 37.24543019189811588, -5.291415217122918513, -3.055000000000000160 ) ) ;
#50048 = ORIENTED_EDGE ( 'NONE', *, *, #98093, .F. ) ;
#50049 = DIRECTION ( 'NONE',  ( 1.000000000000000000, 0.000000000000000000, 0.000000000000000000 ) ) ;
#50050 = EDGE_CURVE ( 'NONE', #101903, #120463, #39062, .T. ) ;
#50051 = AXIS2_PLACEMENT_3D ( 'NONE', #64803, #31457, #128624 ) ;
#50052 = DIRECTION ( 'NONE',  ( -0.000000000000000000, -0.3543493200069152693, 0.9351131265310292928 ) ) ;
#50053 = CARTESIAN_POINT ( 'NONE',  ( -36.18398860626899705, 28.73617430169812437, 5.000000000000000000 ) ) ;
#50054 = EDGE_CURVE ( 'NONE', #79257, #103562, #99211, .T. ) ;
#50055 = LINE ( 'NONE', #141321, #27415 ) ;
#50056 = EDGE_CURVE ( 'NONE', #70215, #142853, #139103, .T. ) ;
#50057 = CARTESIAN_POINT ( 'NONE',  ( 3.183988606268992161, 28.73617430169789699, 5.000000000000000000 ) ) ;
#50058 = CARTESIAN_POINT ( 'NONE',  ( 2.510786437626908008, -27.52281430457053446, 5.000000000000000000 ) ) ;
#50059 = DIRECTION ( 'NONE',  ( 1.000000000000000000, -0.000000000000000000, 0.000000000000000000 ) ) ;
#50060 = LINE ( 'NONE', #83397, #124670 ) ;
#50061 = DIRECTION ( 'NONE',  ( -0.000000000000000000, -0.000000000000000000, -1.000000000000000000 ) ) ;
#50063 = ADVANCED_FACE ( 'NONE', ( #115153 ), #136283, .T. ) ;
#50062 = AXIS2_PLACEMENT_3D ( 'NONE', #96783, #31585, #12659 ) ;
#50064 = VERTEX_POINT ( 'NONE', #38356 ) ;
#50065 = EDGE_LOOP ( 'NONE', ( #4482, #9398, #137489, #72436 ) ) ;
#50066 = EDGE_LOOP ( 'NONE', ( #54927, #140414, #142241, #106491 ) ) ;
#50067 = VERTEX_POINT ( 'NONE', #82571 ) ;
#50068 = DIRECTION ( 'NONE',  ( 0.000000000000000000, -1.000000000000000000, 0.000000000000000000 ) ) ;
#50069 = ORIENTED_EDGE ( 'NONE', *, *, #127874, .T. ) ;
#50070 = ORIENTED_EDGE ( 'NONE', *, *, #31255, .F. ) ;
#50071 = CARTESIAN_POINT ( 'NONE',  ( 34.49999999999975131, -14.56887692260766620, 4.000000000000000000 ) ) ;
#50072 = ADVANCED_FACE ( 'NONE', ( #17980 ), #107160, .T. ) ;
#50073 = EDGE_CURVE ( 'NONE', #125316, #142771, #94839, .T. ) ;
#50074 = LINE ( 'NONE', #14573, #108782 ) ;
#50075 = ORIENTED_EDGE ( 'NONE', *, *, #47998, .F. ) ;
#50076 = CARTESIAN_POINT ( 'NONE',  ( 150.3000000000000114, 0.000000000000000000, 0.000000000000000000 ) ) ;
#50077 = VERTEX_POINT ( 'NONE', #138376 ) ;
#50078 = EDGE_CURVE ( 'NONE', #118345, #143096, #52082, .T. ) ;
#50079 = AXIS2_PLACEMENT_3D ( 'NONE', #141644, #119151, #29289 ) ;
#50081 = LINE ( 'NONE', #62388, #134709 ) ;
#50080 = AXIS2_PLACEMENT_3D ( 'NONE', #71966, #127007, #47384 ) ;
#50082 = LINE ( 'NONE', #94272, #123775 ) ;
#50083 = VECTOR ( 'NONE', #1456, 1000.000000000000000 ) ;
#50084 = EDGE_LOOP ( 'NONE', ( #36175, #5054, #139329 ) ) ;
#50086 = CARTESIAN_POINT ( 'NONE',  ( 32.67183060077624646, -0.7407075233842753681, 4.000000000000000000 ) ) ;
#50085 = CARTESIAN_POINT ( 'NONE',  ( 103.5995968585647802, -6.109999999999998543, -1.637169565754160727 ) ) ;
#50087 =( LENGTH_UNIT ( ) NAMED_UNIT ( * ) SI_UNIT ( .MILLI., .METRE. ) );
#50088 = CARTESIAN_POINT ( 'NONE',  ( 0.000000000000000000, 0.000000000000000000, 5.000000000000000000 ) ) ;
#50089 = ORIENTED_EDGE ( 'NONE', *, *, #99676, .F. ) ;
#50090 = EDGE_LOOP ( 'NONE', ( #39351, #138256, #114752, #81143 ) ) ;
#50091 = PLANE ( 'NONE',  #63456 ) ;
#50092 = ORIENTED_EDGE ( 'NONE', *, *, #7454, .F. ) ;
#50093 = SURFACE_SIDE_STYLE ('',( #125507 ) ) ;
#50094 = PLANE ( 'NONE',  #120440 ) ;
#50095 = CARTESIAN_POINT ( 'NONE',  ( 32.29289321881323360, -3.740707523384246613, 5.000000000000000000 ) ) ;
#50096 = DIRECTION ( 'NONE',  ( 0.000000000000000000, -1.000000000000000000, 0.000000000000000000 ) ) ;
#50097 = ORIENTED_EDGE ( 'NONE', *, *, #116552, .F. ) ;
#50098 = DIRECTION ( 'NONE',  ( 1.000000000000000000, -1.451651444332054676E-15, 0.000000000000000000 ) ) ;
#50099 = CARTESIAN_POINT ( 'NONE',  ( 9.005480084712511157, 28.92564299267931816, 4.000000000000000000 ) ) ;
#50100 = FACE_OUTER_BOUND ( 'NONE', #113743, .T. ) ;
#50101 = ADVANCED_FACE ( 'NONE', ( #71003 ), #127496, .F. ) ;
#50102 = VERTEX_POINT ( 'NONE', #84031 ) ;
#50103 = CARTESIAN_POINT ( 'NONE',  ( 21.18398860626899349, 28.73617430169802134, 5.000000000000000000 ) ) ;
#50104 = LINE ( 'NONE', #85551, #86364 ) ;
#50105 = VERTEX_POINT ( 'NONE', #28904 ) ;
#50107 = EDGE_LOOP ( 'NONE', ( #73440, #48838, #20227, #60715 ) ) ;
#50106 = DIRECTION ( 'NONE',  ( -0.3543493200069162685, -0.000000000000000000, -0.9351131265310288487 ) ) ;
#50108 = ORIENTED_EDGE ( 'NONE', *, *, #24651, .F. ) ;
#50109 = DIRECTION ( 'NONE',  ( 0.7071067811865487940, 0.7071067811865463515, 0.000000000000000000 ) ) ;
#50110 =( NAMED_UNIT ( * ) PLANE_ANGLE_UNIT ( ) SI_UNIT ( $, .RADIAN. ) );
#50111 = ORIENTED_EDGE ( 'NONE', *, *, #48877, .T. ) ;
#50112 = CARTESIAN_POINT ( 'NONE',  ( 18.48921356237309510, -27.52281430457068367, 5.000000000000000000 ) ) ;
#50113 = DIRECTION ( 'NONE',  ( 0.3543493200069162685, -0.000000000000000000, -0.9351131265310288487 ) ) ;
#50114 = VECTOR ( 'NONE', #74691, 1000.000000000000227 ) ;
#50115 = CARTESIAN_POINT ( 'NONE',  ( 24.32816939922336275, 17.25929247661554200, 4.000000000000000000 ) ) ;
#50116 = ORIENTED_EDGE ( 'NONE', *, *, #101650, .T. ) ;
#50117 = LINE ( 'NONE', #105880, #92483 ) ;
#50118 = DIRECTION ( 'NONE',  ( 0.7071067811865486830, -0.7071067811865464625, -0.000000000000000000 ) ) ;
#50119 = EDGE_CURVE ( 'NONE', #47599, #116794, #110014, .T. ) ;
#50120 = CARTESIAN_POINT ( 'NONE',  ( 51.29974487139158867, -27.71228299555242103, 4.000000000000000000 ) ) ;
#50121 = DIRECTION ( 'NONE',  ( 0.3543493200069162685, -0.000000000000000000, -0.9351131265310288487 ) ) ;
#50122 = CARTESIAN_POINT ( 'NONE',  ( -14.70025512860841133, -27.71228299555195917, 4.000000000000000000 ) ) ;
#50124 = AXIS2_PLACEMENT_3D ( 'NONE', #4068, #136071, #137516 ) ;
#50123 = CARTESIAN_POINT ( 'NONE',  ( 0.000000000000000000, 0.000000000000000000, 5.000000000000000000 ) ) ;
#50125 = CARTESIAN_POINT ( 'NONE',  ( 21.16809626817622103, 8.755558144015518351, 4.000000000000000000 ) ) ;
#50126 = CARTESIAN_POINT ( 'NONE',  ( 28.51669371712955581, 7.950000000000000178, -2.130196079827421318 ) ) ;
#50127 = VERTEX_POINT ( 'NONE', #20143 ) ;
#50128 = ORIENTED_EDGE ( 'NONE', *, *, #21897, .F. ) ;
#50129 = ORIENTED_EDGE ( 'NONE', *, *, #65507, .F. ) ;
#50130 = CARTESIAN_POINT ( 'NONE',  ( 110.8125000000000000, 5.819803920172571310, 5.819803920172575751 ) ) ;
#50131 = EDGE_LOOP ( 'NONE', ( #3557, #95148, #16798, #128944 ) ) ;
#50132 = EDGE_LOOP ( 'NONE', ( #3528, #139298, #83182, #82330 ) ) ;
#50133 = EDGE_CURVE ( 'NONE', #78430, #27599, #96964, .T. ) ;
#50134 = VERTEX_POINT ( 'NONE', #54259 ) ;
#50135 = VECTOR ( 'NONE', #96092, 1000.000000000000227 ) ;
#50136 = CARTESIAN_POINT ( 'NONE',  ( -42.48921356237308800, -27.52281430457085065, 5.000000000000000000 ) ) ;
#50137 = DIRECTION ( 'NONE',  ( -0.7071067811865486830, -0.7071067811865464625, -0.000000000000000000 ) ) ;
#50138 = ORIENTED_EDGE ( 'NONE', *, *, #135634, .F. ) ;
#50139 = CARTESIAN_POINT ( 'NONE',  ( 10.49999999999992539, -13.53360074219760101, 5.000000000000000000 ) ) ;
#50140 = CARTESIAN_POINT ( 'NONE',  ( -17.18753812416040461, -22.22500000000000142, 4.000000000000000000 ) ) ;
#50141 = LINE ( 'NONE', #138575, #124969 ) ;
#50142 = CARTESIAN_POINT ( 'NONE',  ( 21.18398860626899349, 28.73617430169802134, 5.000000000000000000 ) ) ;
#50143 = CARTESIAN_POINT ( 'NONE',  ( 110.6879301918981184, 6.110000000000002984, -1.637169565754156730 ) ) ;
#50144 = EDGE_CURVE ( 'NONE', #68374, #76484, #108554, .T. ) ;
#50145 = ORIENTED_EDGE ( 'NONE', *, *, #102624, .T. ) ;
#50146 = ADVANCED_FACE ( 'NONE', ( #86862 ), #64383, .F. ) ;
#50147 = CARTESIAN_POINT ( 'NONE',  ( -0.6614269816723958861, 22.22500000000000142, 17.98374865626361796 ) ) ;
#50148 =( NAMED_UNIT ( * ) PLANE_ANGLE_UNIT ( ) SI_UNIT ( $, .RADIAN. ) );
#50149 = CARTESIAN_POINT ( 'NONE',  ( -13.49999999999990408, -7.533600742197660516, 5.000000000000000000 ) ) ;
#50150 = CARTESIAN_POINT ( 'NONE',  ( -47.99451991528749062, 28.92564299267971251, 4.000000000000000000 ) ) ;
#50151 = FACE_OUTER_BOUND ( 'NONE', #62445, .T. ) ;
#50152 = LINE ( 'NONE', #63198, #43062 ) ;
#50153 = CARTESIAN_POINT ( 'NONE',  ( 42.51669371712955581, 7.950000000000001066, -2.130196079827421318 ) ) ;
#50154 = VECTOR ( 'NONE', #43798, 1000.000000000000000 ) ;
#50155 = LINE ( 'NONE', #28400, #58406 ) ;
#50156 = DIRECTION ( 'NONE',  ( -1.000000000000000000, -0.000000000000000000, -0.000000000000000000 ) ) ;
#50157 = ORIENTED_EDGE ( 'NONE', *, *, #132798, .T. ) ;
#50158 = VERTEX_POINT ( 'NONE', #41931 ) ;
#50159 = CARTESIAN_POINT ( 'NONE',  ( 32.79166666666666430, 3.975000000000003642, -6.884901960086285300 ) ) ;
#50160 = VECTOR ( 'NONE', #87619, 1000.000000000000000 ) ;
#50161 = ORIENTED_EDGE ( 'NONE', *, *, #24011, .T. ) ;
#50162 = CARTESIAN_POINT ( 'NONE',  ( -1.171830600776460285, 21.75929247661549581, 4.000000000000000000 ) ) ;
#50163 = PRESENTATION_LAYER_ASSIGNMENT (  '', '', ( #89567 ) ) ;
#50164 = DIRECTION ( 'NONE',  ( 0.000000000000000000, 0.000000000000000000, 1.000000000000000000 ) ) ;
#50165 = DIRECTION ( 'NONE',  ( -0.6830127018922180770, -0.6830127018922204085, -0.2588190451025213501 ) ) ;
#50166 = EDGE_CURVE ( 'NONE', #95429, #138852, #132795, .T. ) ;
#50167 = LINE ( 'NONE', #7334, #37632 ) ;
#50168 = SURFACE_SIDE_STYLE ('',( #128444 ) ) ;
#50169 = CARTESIAN_POINT ( 'NONE',  ( 53.99451991528749062, 28.92564299267975869, 4.000000000000000000 ) ) ;
#50170 = CARTESIAN_POINT ( 'NONE',  ( 25.37543019189810067, -5.291415217122920289, -3.055000000000001492 ) ) ;
#50171 = EDGE_CURVE ( 'NONE', #117371, #67034, #121601, .T. ) ;
#50173 = EDGE_LOOP ( 'NONE', ( #133843, #6533, #128566, #83693 ) ) ;
#50172 = PRESENTATION_LAYER_ASSIGNMENT (  '', '', ( #29240 ) ) ;
#50174 = FACE_OUTER_BOUND ( 'NONE', #20249, .T. ) ;
#50175 = VERTEX_POINT ( 'NONE', #109310 ) ;
#50176 = CARTESIAN_POINT ( 'NONE',  ( -1.499999999999984013, -2.947814304570802513, 5.000000000000000000 ) ) ;
#50177 = CARTESIAN_POINT ( 'NONE',  ( -11.70025512860841133, -27.71228299555198049, 4.000000000000000000 ) ) ;
#50178 = CARTESIAN_POINT ( 'NONE',  ( 4.184256412735922304, 2.055000000000001048, 0.000000000000000000 ) ) ;
#50179 = DIRECTION ( 'NONE',  ( -0.7071067811865486830, 0.7071067811865464625, 0.000000000000000000 ) ) ;
#50181 = ORIENTED_EDGE ( 'NONE', *, *, #69811, .F. ) ;
#50180 = EDGE_CURVE ( 'NONE', #29177, #30662, #75976, .T. ) ;
#50182 = AXIS2_PLACEMENT_3D ( 'NONE', #7536, #95982, #76402 ) ;
#50183 = CARTESIAN_POINT ( 'NONE',  ( 53.08376352523143282, -6.110000000000001208, -3.741295971395164515E-16 ) ) ;
#50184 = ORIENTED_EDGE ( 'NONE', *, *, #3880, .T. ) ;
#50185 = DIRECTION ( 'NONE',  ( 0.6830127018922181881, 0.6830127018922202975, -0.2588190451025214056 ) ) ;
#50186 = EDGE_CURVE ( 'NONE', #23136, #92499, #66536, .T. ) ;
#50187 = DIRECTION ( 'NONE',  ( 0.7071067811865487940, 0.7071067811865463515, 0.000000000000000000 ) ) ;
#50188 = DIRECTION ( 'NONE',  ( 0.7071067811865487940, 0.7071067811865463515, 0.000000000000000000 ) ) ;
#50189 = CARTESIAN_POINT ( 'NONE',  ( 5.999999999999961808, -6.033600742197678279, 5.000000000000000000 ) ) ;
#50190 = AXIS2_PLACEMENT_3D ( 'NONE', #75500, #29132, #97202 ) ;
#50191 = VECTOR ( 'NONE', #15206, 1000.000000000000000 ) ;
#50192 = VECTOR ( 'NONE', #137892, 999.9999999999998863 ) ;
#50193 = CARTESIAN_POINT ( 'NONE',  ( 49.49543019189811588, 5.291415217122916737, 3.055000000000001936 ) ) ;
#50194 = ORIENTED_EDGE ( 'NONE', *, *, #10838, .T. ) ;
#50195 = CYLINDRICAL_SURFACE ( 'NONE', #23424, 2.500000000000000000 ) ;
#50196 = CARTESIAN_POINT ( 'NONE',  ( 34.47516574401890921, -4.509482387884330201, 4.998110765256834398 ) ) ;
#50197 = EDGE_LOOP ( 'NONE', ( #42378, #79558, #4592, #90607 ) ) ;
#50198 = EDGE_LOOP ( 'NONE', ( #14933, #51844, #67289, #89928, #116686 ) ) ;
#50199 = VECTOR ( 'NONE', #62990, 1000.000000000000000 ) ;
#50200 = DIRECTION ( 'NONE',  ( 0.7071067811865487940, 0.7071067811865463515, -0.000000000000000000 ) ) ;
#50201 = ORIENTED_EDGE ( 'NONE', *, *, #22647, .F. ) ;
#50202 = EDGE_CURVE ( 'NONE', #237, #70779, #120206, .T. ) ;
#50203 = CARTESIAN_POINT ( 'NONE',  ( -78.48921356237309510, -27.52281430457109934, 5.000000000000000000 ) ) ;
#50204 = PRODUCT_DEFINITION_CONTEXT ( 'detailed design', #23477, 'design' ) ;
#50205 = VERTEX_POINT ( 'NONE', #10681 ) ;
#50206 = LINE ( 'NONE', #116869, #54901 ) ;
#50207 = FACE_OUTER_BOUND ( 'NONE', #54185, .T. ) ;
#50208 = FACE_BOUND ( 'NONE', #103331, .T. ) ;
#50209 = CARTESIAN_POINT ( 'NONE',  ( 9.005480084712511157, 28.92564299267931816, 4.000000000000000000 ) ) ;
#50210 = LINE ( 'NONE', #103827, #49125 ) ;
#50211 = CARTESIAN_POINT ( 'NONE',  ( -11.21837311707497165, 21.74787736706806385, 4.999607392498048419 ) ) ;
#50212 = VERTEX_POINT ( 'NONE', #21598 ) ;
#50213 = CARTESIAN_POINT ( 'NONE',  ( -13.36902924655238323, 1.333290112598358945, 4.303104124266152297 ) ) ;
#50215 = ORIENTED_EDGE ( 'NONE', *, *, #29273, .T. ) ;
#50214 = CARTESIAN_POINT ( 'NONE',  ( -11.70025512860841133, -27.71228299555198049, 4.000000000000000000 ) ) ;
#50216 = EDGE_LOOP ( 'NONE', ( #68853, #55569, #115672, #133503 ) ) ;
#50217 = LINE ( 'NONE', #8092, #14748 ) ;
#50218 = VERTEX_POINT ( 'NONE', #120147 ) ;
#50220 = ORIENTED_EDGE ( 'NONE', *, *, #102795, .T. ) ;
#50219 = EDGE_CURVE ( 'NONE', #61426, #112167, #55663, .T. ) ;
#50221 = CARTESIAN_POINT ( 'NONE',  ( 63.93293019189812298, 1.637169565754156508, 6.110000000000000320 ) ) ;
#50222 = VECTOR ( 'NONE', #3842, 1000.000000000000000 ) ;
#50223 = VERTEX_POINT ( 'NONE', #65124 ) ;
#50224 = DIRECTION ( 'NONE',  ( -0.3543493200069162685, -0.000000000000000000, -0.9351131265310288487 ) ) ;
#50225 = EDGE_CURVE ( 'NONE', #16867, #98425, #143363, .T. ) ;
#50226 = DIRECTION ( 'NONE',  ( 0.7071067811865487940, 0.7071067811865463515, 0.000000000000000000 ) ) ;
#50227 = ORIENTED_EDGE ( 'NONE', *, *, #19027, .F. ) ;
#50228 = AXIS2_PLACEMENT_3D ( 'NONE', #56629, #69622, #133434 ) ;
#50229 = EDGE_CURVE ( 'NONE', #48577, #44804, #527, .T. ) ;
#50230 = ADVANCED_FACE ( 'NONE', ( #118752 ), #88290, .F. ) ;
#50231 = FACE_OUTER_BOUND ( 'NONE', #118696, .T. ) ;
#50232 = CARTESIAN_POINT ( 'NONE',  ( 0.000000000000000000, 0.000000000000000000, 5.000000000000000000 ) ) ;
#50233 = LINE ( 'NONE', #7401, #80605 ) ;
#50234 = DIRECTION ( 'NONE',  ( -0.7071067811865487940, 0.7071067811865463515, -0.000000000000000000 ) ) ;
#50235 = DIRECTION ( 'NONE',  ( -0.7071067811865486830, -0.7071067811865464625, 0.000000000000000000 ) ) ;
#50236 = VERTEX_POINT ( 'NONE', #99864 ) ;
#50237 = ORIENTED_EDGE ( 'NONE', *, *, #128471, .F. ) ;
#50238 = LINE ( 'NONE', #114049, #95972 ) ;
#50239 = DIRECTION ( 'NONE',  ( 0.7071067811865486830, -0.7071067811865464625, -0.000000000000000000 ) ) ;
#50240 = VERTEX_POINT ( 'NONE', #87565 ) ;
#50241 = ORIENTED_EDGE ( 'NONE', *, *, #29909, .F. ) ;
#50242 = EDGE_LOOP ( 'NONE', ( #86700, #25566, #37470, #106690, #14907 ) ) ;
#50243 = CARTESIAN_POINT ( 'NONE',  ( -0.1839886062690032631, 28.73617430169787568, 5.000000000000000000 ) ) ;
#50244 = EDGE_CURVE ( 'NONE', #95686, #11445, #131790, .T. ) ;
#50245 = VECTOR ( 'NONE', #45767, 999.9999999999998863 ) ;
#50246 = EDGE_CURVE ( 'NONE', #33310, #78073, #85398, .T. ) ;
#50247 = DIRECTION ( 'NONE',  ( 0.7071067811865486830, -0.7071067811865464625, -0.000000000000000000 ) ) ;
#50248 = VERTEX_POINT ( 'NONE', #130370 ) ;
#50249 = CARTESIAN_POINT ( 'NONE',  ( -13.17183060077637613, 18.75929247661552068, 4.000000000000000000 ) ) ;
#50250 = EDGE_CURVE ( 'NONE', #126051, #133821, #31062, .T. ) ;
#50251 = AXIS2_PLACEMENT_3D ( 'NONE', #34182, #112451, #100851 ) ;
#50252 = DIRECTION ( 'NONE',  ( -1.000000000000000000, 0.000000000000000000, 0.000000000000000000 ) ) ;
#50253 = CARTESIAN_POINT ( 'NONE',  ( 8.525403141435219823, 2.126176841940962348, 7.934999999999989839 ) ) ;
#50254 = LINE ( 'NONE', #137259, #63496 ) ;
#50255 = EDGE_LOOP ( 'NONE', ( #17074, #120747, #126152, #65193 ) ) ;
#50256 = CIRCLE ( 'NONE', #66406, 2.500000000000000444 ) ;
#50257 = CARTESIAN_POINT ( 'NONE',  ( 75.29974487139158157, -27.71228299555258445, 4.000000000000000000 ) ) ;
#50258 = CARTESIAN_POINT ( 'NONE',  ( 45.18398860626900415, 28.73617430169818832, 5.000000000000000000 ) ) ;
#50259 = EDGE_CURVE ( 'NONE', #128612, #83675, #102735, .T. ) ;
#50261 = ORIENTED_EDGE ( 'NONE', *, *, #91474, .T. ) ;
#50260 = DIRECTION ( 'NONE',  ( 1.000000000000000000, 0.000000000000000000, 0.000000000000000000 ) ) ;
#50262 = CARTESIAN_POINT ( 'NONE',  ( 39.48921356237310221, -27.52281430457082934, 5.000000000000000000 ) ) ;
#50263 = ORIENTED_EDGE ( 'NONE', *, *, #75388, .F. ) ;
#50264 = LINE ( 'NONE', #27060, #130617 ) ;
#50265 = PLANE ( 'NONE',  #44698 ) ;
#50266 = DIRECTION ( 'NONE',  ( 0.000000000000000000, 0.000000000000000000, 1.000000000000000000 ) ) ;
#50267 = ORIENTED_EDGE ( 'NONE', *, *, #116546, .T. ) ;
#50268 = CARTESIAN_POINT ( 'NONE',  ( -18.18398860626898994, 28.73617430169800002, 5.000000000000000000 ) ) ;
#50269 = CARTESIAN_POINT ( 'NONE',  ( 6.940000000000001279, 9.521314400968980422E-16, 0.000000000000000000 ) ) ;
#50270 = CARTESIAN_POINT ( 'NONE',  ( -34.92500000000001137, -6.183345613589518841, 4.500000000000000888 ) ) ;
#50271 = ADVANCED_FACE ( 'NONE', ( #114307 ), #89700, .F. ) ;
#50272 = VERTEX_POINT ( 'NONE', #68690 ) ;
#50273 = PLANE ( 'NONE',  #39317 ) ;
#50274 = DIRECTION ( 'NONE',  ( -0.7071067811865486830, -0.7071067811865464625, -0.000000000000000000 ) ) ;
#50275 = CARTESIAN_POINT ( 'NONE',  ( 18.48921356237309510, -27.52281430457068367, 5.000000000000000000 ) ) ;
#50276 = PLANE ( 'NONE',  #118982 ) ;
#50277 = CARTESIAN_POINT ( 'NONE',  ( 12.81246187583938223, -22.22500000000000142, 4.000000000000000000 ) ) ;
#50278 = ORIENTED_EDGE ( 'NONE', *, *, #138826, .F. ) ;
#50279 = EDGE_CURVE ( 'NONE', #111091, #123707, #45522, .T. ) ;
#50280 = ORIENTED_EDGE ( 'NONE', *, *, #39228, .F. ) ;
#50281 = EDGE_CURVE ( 'NONE', #39184, #56350, #141041, .T. ) ;
#50282 = FACE_OUTER_BOUND ( 'NONE', #43501, .T. ) ;
#50283 = LINE ( 'NONE', #27800, #115318 ) ;
#50284 = AXIS2_PLACEMENT_3D ( 'NONE', #55119, #129086, #32655 ) ;
#50285 = VECTOR ( 'NONE', #99937, 1000.000000000000227 ) ;
#50286 = EDGE_CURVE ( 'NONE', #51035, #95691, #138796, .T. ) ;
#50287 = CARTESIAN_POINT ( 'NONE',  ( 0.4162364747685528554, -7.934999999999990727, 4.858786175617117713E-16 ) ) ;
#50288 = CARTESIAN_POINT ( 'NONE',  ( 0.000000000000000000, 0.000000000000000000, 5.000000000000000000 ) ) ;
#50289 = CARTESIAN_POINT ( 'NONE',  ( 17.20710678118642889, -5.240707523384228850, 5.000000000000000000 ) ) ;
#50290 = CARTESIAN_POINT ( 'NONE',  ( -17.99999999999986855, -22.22500000000000142, 4.412002311790053533 ) ) ;
#50291 = PLANE ( 'NONE',  #83899 ) ;
#50292 = VERTEX_POINT ( 'NONE', #14984 ) ;
#50293 = LINE ( 'NONE', #95918, #132164 ) ;
#50294 = VECTOR ( 'NONE', #57850, 1000.000000000000227 ) ;
#50295 = DIRECTION ( 'NONE',  ( -0.3543493200069162685, -0.000000000000000000, -0.9351131265310288487 ) ) ;
#50296 = CARTESIAN_POINT ( 'NONE',  ( -33.29974487139158867, -27.71228299555229313, 4.000000000000000000 ) ) ;
#50297 = VECTOR ( 'NONE', #68380, 1000.000000000000000 ) ;
#50298 = PLANE ( 'NONE',  #106154 ) ;
#50299 = CARTESIAN_POINT ( 'NONE',  ( 48.62043019189811588, 3.055000000000002380, -5.291415217122917625 ) ) ;
#50300 = DIRECTION ( 'NONE',  ( -0.6830127018922180770, -0.6830127018922204085, -0.2588190451025213501 ) ) ;
#50301 = ORIENTED_EDGE ( 'NONE', *, *, #23637, .T. ) ;
#50302 = EDGE_LOOP ( 'NONE', ( #36815, #85640, #83453, #68668 ) ) ;
#50303 = ADVANCED_FACE ( 'NONE', ( #112189 ), #69398, .F. ) ;
#50304 = ORIENTED_EDGE ( 'NONE', *, *, #39957, .T. ) ;
#50305 = PLANE ( 'NONE',  #103295 ) ;
#50306 = DIRECTION ( 'NONE',  ( 0.7071067811865487940, 0.7071067811865463515, -0.000000000000000000 ) ) ;
#50307 = CARTESIAN_POINT ( 'NONE',  ( 7.139999999999992575, -35.14999999999999858, -11.72188031596274804 ) ) ;
#50308 = FACE_OUTER_BOUND ( 'NONE', #15259, .T. ) ;
#50309 = DIRECTION ( 'NONE',  ( -0.7071067811865486830, 0.7071067811865464625, 0.000000000000000000 ) ) ;
#50310 = FACE_OUTER_BOUND ( 'NONE', #14441, .T. ) ;
#50311 = EDGE_CURVE ( 'NONE', #98221, #8240, #91161, .T. ) ;
#50312 = ORIENTED_EDGE ( 'NONE', *, *, #139650, .F. ) ;
#50313 = PLANE ( 'NONE',  #58080 ) ;
#50314 = CARTESIAN_POINT ( 'NONE',  ( -12.79289321881336328, 15.75929247661555443, 5.000000000000000000 ) ) ;
#50315 = VECTOR ( 'NONE', #29708, 1000.000000000000000 ) ;
#50316 = PLANE ( 'NONE',  #121933 ) ;
#50317 = CARTESIAN_POINT ( 'NONE',  ( -66.48921356237309510, -27.52281430457101763, 5.000000000000000000 ) ) ;
#50318 = DIRECTION ( 'NONE',  ( -0.000000000000000000, 0.000000000000000000, 1.000000000000000000 ) ) ;
#50319 = CARTESIAN_POINT ( 'NONE',  ( 62.20419371712955581, -6.884901960086285300, -3.975000000000000089 ) ) ;
#50320 = AXIS2_PLACEMENT_3D ( 'NONE', #106753, #22149, #101150 ) ;
#50321 = CARTESIAN_POINT ( 'NONE',  ( -59.99451991528749772, 28.92564299267980132, 4.000000000000000000 ) ) ;
#50322 = ORIENTED_EDGE ( 'NONE', *, *, #136185, .T. ) ;
#50323 = ORIENTED_EDGE ( 'NONE', *, *, #29816, .T. ) ;
#50324 = CARTESIAN_POINT ( 'NONE',  ( 63.70833333333332860, -3.974999999999999201, -6.884901960086287964 ) ) ;
#50325 = LINE ( 'NONE', #95234, #42465 ) ;
#50326 = CARTESIAN_POINT ( 'NONE',  ( -15.48921356237309510, -27.52281430457066236, 5.000000000000000000 ) ) ;
#50327 = EDGE_CURVE ( 'NONE', #141201, #62928, #124474, .T. ) ;
#50328 = VECTOR ( 'NONE', #101329, 1000.000000000000000 ) ;
#50329 = ORIENTED_EDGE ( 'NONE', *, *, #76406, .T. ) ;
#50330 = LINE ( 'NONE', #116993, #139380 ) ;
#50331 = LINE ( 'NONE', #37311, #28179 ) ;
#50332 = CARTESIAN_POINT ( 'NONE',  ( 58.47959685856477563, 6.109999999999999432, 1.637169565754164280 ) ) ;
#50333 = EDGE_CURVE ( 'NONE', #81104, #91540, #89016, .T. ) ;
#50334 = AXIS2_PLACEMENT_3D ( 'NONE', #54271, #17991, #29605 ) ;
#50335 = CARTESIAN_POINT ( 'NONE',  ( -42.29974487139158157, -27.71228299555235708, 4.000000000000000000 ) ) ;
#50336 = ORIENTED_EDGE ( 'NONE', *, *, #94911, .T. ) ;
#50337 = ORIENTED_EDGE ( 'NONE', *, *, #12896, .F. ) ;
#50338 = CARTESIAN_POINT ( 'NONE',  ( 0.000000000000000000, 0.000000000000000000, 0.000000000000000000 ) ) ;
#50339 = DIRECTION ( 'NONE',  ( -0.7071067811865486830, -0.7071067811865464625, -0.000000000000000000 ) ) ;
#50340 = DIRECTION ( 'NONE',  ( -0.7071067811865487940, 0.7071067811865463515, -0.000000000000000000 ) ) ;
#50341 = DIRECTION ( 'NONE',  ( 1.000000000000000000, -0.000000000000000000, -0.000000000000000000 ) ) ;
#50342 = EDGE_CURVE ( 'NONE', #134381, #129741, #34614, .T. ) ;
#50343 = CARTESIAN_POINT ( 'NONE',  ( -21.18398860626899349, 28.73617430169802134, 5.000000000000000000 ) ) ;
#50345 = ORIENTED_EDGE ( 'NONE', *, *, #73856, .F. ) ;
#50344 = CARTESIAN_POINT ( 'NONE',  ( 101.2875270504628986, 0.000000000000000000, -7.949999999999998401 ) ) ;
#50346 = EDGE_CURVE ( 'NONE', #128067, #82630, #103413, .T. ) ;
#50347 = LINE ( 'NONE', #7522, #18267 ) ;
#50348 = LINE ( 'NONE', #14843, #128808 ) ;
#50349 = CARTESIAN_POINT ( 'NONE',  ( -6.707106781186496391, 2.259292476615697876, 5.000000000000000000 ) ) ;
#50350 = DIRECTION ( 'NONE',  ( -0.3543493200069162685, -0.000000000000000000, -0.9351131265310288487 ) ) ;
#50351 = ORIENTED_EDGE ( 'NONE', *, *, #41636, .F. ) ;
#50352 = VERTEX_POINT ( 'NONE', #56413 ) ;
#50353 = VECTOR ( 'NONE', #53788, 1000.000000000000000 ) ;
#50354 = EDGE_CURVE ( 'NONE', #49384, #90110, #100596, .T. ) ;
#50355 = DIRECTION ( 'NONE',  ( 0.6830127018922181881, 0.6830127018922202975, -0.2588190451025214056 ) ) ;
#50356 = DIRECTION ( 'NONE',  ( -0.7071067811865487940, 0.7071067811865463515, 0.000000000000000000 ) ) ;
#50357 = CARTESIAN_POINT ( 'NONE',  ( 9.183988606268997046, 28.73617430169793607, 5.000000000000000000 ) ) ;
#50358 = VECTOR ( 'NONE', #131443, 1000.000000000000000 ) ;
#50359 = CARTESIAN_POINT ( 'NONE',  ( 110.9125270504628986, -7.949999999999998401, -4.867971026610728450E-16 ) ) ;
#50360 = CARTESIAN_POINT ( 'NONE',  ( 39.29974487139159578, -27.71228299555233576, 4.000000000000000000 ) ) ;
#50361 = ORIENTED_EDGE ( 'NONE', *, *, #52987, .F. ) ;
#50362 = ORIENTED_EDGE ( 'NONE', *, *, #44948, .T. ) ;
#50363 = DIRECTION ( 'NONE',  ( 0.7071067811865487940, 0.7071067811865463515, 0.000000000000000000 ) ) ;
#50364 = CARTESIAN_POINT ( 'NONE',  ( 0.000000000000000000, -57.15000000000003411, 15.92499999999935589 ) ) ;
#50365 = EDGE_LOOP ( 'NONE', ( #50145, #4847, #53634, #108625 ) ) ;
#50366 = ADVANCED_FACE ( 'NONE', ( #44826 ), #78850, .F. ) ;
#50367 = EDGE_LOOP ( 'NONE', ( #19215, #7679, #124407 ) ) ;
#50368 = CARTESIAN_POINT ( 'NONE',  ( -42.48921356237308800, -27.52281430457085065, 5.000000000000000000 ) ) ;
#50369 = ORIENTED_EDGE ( 'NONE', *, *, #76097, .F. ) ;
#50370 = PLANE ( 'NONE',  #71092 ) ;
#50371 = DIRECTION ( 'NONE',  ( -0.7071067811865486830, -0.7071067811865464625, 0.000000000000000000 ) ) ;
#50372 = EDGE_CURVE ( 'NONE', #100169, #41854, #33912, .T. ) ;
#50373 = AXIS2_PLACEMENT_3D ( 'NONE', #15763, #106358, #139037 ) ;
#50374 = VECTOR ( 'NONE', #62146, 1000.000000000000114 ) ;
#50375 = FACE_BOUND ( 'NONE', #5221, .T. ) ;
#50376 = LINE ( 'NONE', #4656, #87297 ) ;
#50377 = APPLICATION_CONTEXT ( 'automotive_design' ) ;
#50378 = FACE_OUTER_BOUND ( 'NONE', #84550, .T. ) ;
#50380 = ORIENTED_EDGE ( 'NONE', *, *, #110189, .F. ) ;
#50379 = CARTESIAN_POINT ( 'NONE',  ( 16.49999999999988276, -20.53675388469229190, 2.352720554255931518 ) ) ;
#50381 = VECTOR ( 'NONE', #28825, 1000.000000000000000 ) ;
#50382 = VECTOR ( 'NONE', #85664, 999.9999999999998863 ) ;
#50383 = FACE_OUTER_BOUND ( 'NONE', #104889, .T. ) ;
#50384 = ORIENTED_EDGE ( 'NONE', *, *, #4841, .F. ) ;
#50385 = AXIS2_PLACEMENT_3D ( 'NONE', #38933, #26629, #83154 ) ;
#50386 = VERTEX_POINT ( 'NONE', #14280 ) ;
#50387 = CARTESIAN_POINT ( 'NONE',  ( 91.34959685856478018, 6.109999999999996767, 1.637169565754163836 ) ) ;
#50388 = ORIENTED_EDGE ( 'NONE', *, *, #99478, .T. ) ;
#50389 = CARTESIAN_POINT ( 'NONE',  ( 34.92499999999998295, 22.22500000000000142, 4.500000000000000888 ) ) ;
#50390 = EDGE_CURVE ( 'NONE', #88912, #60182, #102010, .T. ) ;
#50391 = VECTOR ( 'NONE', #104151, 1000.000000000000227 ) ;
#50392 = CARTESIAN_POINT ( 'NONE',  ( -25.49999999999982236, 13.46639925780212721, 5.000000000000000000 ) ) ;
#50393 = DIRECTION ( 'NONE',  ( -0.7071067811865486830, 0.7071067811865464625, 0.000000000000000000 ) ) ;
#50394 = ADVANCED_FACE ( 'NONE', ( #46234 ), #90416, .F. ) ;
#50395 = EDGE_CURVE ( 'NONE', #70864, #118081, #25146, .T. ) ;
#50396 = CARTESIAN_POINT ( 'NONE',  ( 32.99999999999977973, -1.447814304570818500, 5.000000000000000000 ) ) ;
#50397 = ORIENTED_EDGE ( 'NONE', *, *, #73020, .F. ) ;
#50398 = CARTESIAN_POINT ( 'NONE',  ( 35.99451991528749772, 28.92564299267963079, 4.000000000000000000 ) ) ;
#50399 = DIRECTION ( 'NONE',  ( -0.3543493200069162685, -0.000000000000000000, -0.9351131265310288487 ) ) ;
#50400 = PLANE ( 'NONE',  #112941 ) ;
#50402 = FACE_OUTER_BOUND ( 'NONE', #60238, .T. ) ;
#50401 = DIRECTION ( 'NONE',  ( 0.7071067811865487940, 0.7071067811865463515, 0.000000000000000000 ) ) ;
#50403 = PLANE ( 'NONE',  #81727 ) ;
#50404 = DIRECTION ( 'NONE',  ( 0.7071067811865486830, -0.7071067811865464625, -0.000000000000000000 ) ) ;
#50405 = DIRECTION ( 'NONE',  ( 0.000000000000000000, 0.000000000000000000, 1.000000000000000000 ) ) ;
#50406 = VERTEX_POINT ( 'NONE', #26594 ) ;
#50407 = EDGE_CURVE ( 'NONE', #474, #57341, #62816, .T. ) ;
#50408 = PLANE ( 'NONE',  #84324 ) ;
#50409 = CARTESIAN_POINT ( 'NONE',  ( -24.48921356237309510, -27.52281430457072631, 5.000000000000000000 ) ) ;
#50410 = VERTEX_POINT ( 'NONE', #6929 ) ;
#50411 = ORIENTED_EDGE ( 'NONE', *, *, #116362, .F. ) ;
#50412 = EDGE_CURVE ( 'NONE', #122541, #113921, #34538, .T. ) ;
#50414 = ORIENTED_EDGE ( 'NONE', *, *, #110596, .F. ) ;
#50413 = EDGE_CURVE ( 'NONE', #24882, #99874, #83865, .T. ) ;
#50415 = CARTESIAN_POINT ( 'NONE',  ( 41.85459685856476852, -1.637169565754161615, 6.110000000000000320 ) ) ;
#50416 = AXIS2_PLACEMENT_3D ( 'NONE', #109217, #20049, #133146 ) ;
#50417 = VERTEX_POINT ( 'NONE', #138213 ) ;
#50418 = EDGE_CURVE ( 'NONE', #25547, #49111, #48344, .T. ) ;
#50419 = CARTESIAN_POINT ( 'NONE',  ( 19.44163961620376924, -6.094999999999989093, 1.633150327867691765 ) ) ;
#50420 = CARTESIAN_POINT ( 'NONE',  ( -11.45531355849511002, 8.356207601636546300, -27.86682228225575031 ) ) ;
#50421 = EDGE_CURVE ( 'NONE', #26574, #30925, #117847, .T. ) ;
#50422 = ORIENTED_EDGE ( 'NONE', *, *, #104100, .F. ) ;
#50423 = CARTESIAN_POINT ( 'NONE',  ( 2.999999999999983569, -3.033600742197712030, 5.000000000000000000 ) ) ;
#50424 = EDGE_LOOP ( 'NONE', ( #27410, #8295, #106507, #121820, #70492, #41804 ) ) ;
#50425 = DIRECTION ( 'NONE',  ( 0.7071067811865487940, 0.7071067811865463515, 0.000000000000000000 ) ) ;
#50426 = DIRECTION ( 'NONE',  ( -0.7071067811865486830, -0.7071067811865464625, 0.000000000000000000 ) ) ;
#50427 = ADVANCED_FACE ( 'NONE', ( #49081 ), #104859, .F. ) ;
#50429 = EDGE_LOOP ( 'NONE', ( #59155, #73399, #3653, #112498 ) ) ;
#50428 = FACE_OUTER_BOUND ( 'NONE', #2721, .T. ) ;
#50430 = ORIENTED_EDGE ( 'NONE', *, *, #126752, .F. ) ;
#50431 =( BOUNDED_CURVE ( )  B_SPLINE_CURVE ( 3, ( #81290, #125493, #15256, #107285 ),
 .UNSPECIFIED., .F., .F. ) 
 B_SPLINE_CURVE_WITH_KNOTS ( ( 4, 4 ),
 ( 5.043186909253409844, 5.074607125596340751 ),
 .UNSPECIFIED. ) 
 CURVE ( )  GEOMETRIC_REPRESENTATION_ITEM ( )  RATIONAL_B_SPLINE_CURVE ( ( 1.000000000000000000, 0.9999177325257868620, 0.9999177325257868620, 1.000000000000000000 ) ) 
 REPRESENTATION_ITEM ( '' )  );
#50432 = FACE_OUTER_BOUND ( 'NONE', #137374, .T. ) ;
#50433 = LINE ( 'NONE', #82353, #41489 ) ;
#50434 = VERTEX_POINT ( 'NONE', #72290 ) ;
#50435 = DIRECTION ( 'NONE',  ( -0.000000000000000000, -1.000000000000000000, -0.000000000000000000 ) ) ;
#50436 = VERTEX_POINT ( 'NONE', #5524 ) ;
#50437 = PRODUCT_DEFINITION_SHAPE ( 'NONE', 'NONE',  #143573 ) ;
#50438 = ORIENTED_EDGE ( 'NONE', *, *, #6260, .T. ) ;
#50439 = ORIENTED_EDGE ( 'NONE', *, *, #94890, .F. ) ;
#50440 = ORIENTED_EDGE ( 'NONE', *, *, #31379, .T. ) ;
#50441 = CARTESIAN_POINT ( 'NONE',  ( -31.82816939922330945, 0.7592924766157069794, 4.000000000000000000 ) ) ;
#50442 = ADVANCED_FACE ( 'NONE', ( #40353 ), #108619, .T. ) ;
#50443 = CARTESIAN_POINT ( 'NONE',  ( 11.99999999999992006, 12.83542986846998168, -1.025386466790397577 ) ) ;
#50444 = DIRECTION ( 'NONE',  ( -0.000000000000000000, -0.3543493200069152693, 0.9351131265310292928 ) ) ;
#50445 = CARTESIAN_POINT ( 'NONE',  ( 17.99999999999987566, -15.03360074219758502, 5.000000000000000000 ) ) ;
#50446 = VERTEX_POINT ( 'NONE', #18533 ) ;
#50447 = PLANE ( 'NONE',  #134679 ) ;
#50448 = ORIENTED_EDGE ( 'NONE', *, *, #91955, .T. ) ;
#50449 = FACE_OUTER_BOUND ( 'NONE', #45296, .T. ) ;
#50450 = EDGE_CURVE ( 'NONE', #120651, #102811, #70835, .T. ) ;
#50451 = CARTESIAN_POINT ( 'NONE',  ( 31.47873647476854941, -5.808823158059033709, 5.808823158059035485 ) ) ;
#50452 = DIRECTION ( 'NONE',  ( -0.000000000000000000, -0.000000000000000000, 1.000000000000000000 ) ) ;
#50453 = CARTESIAN_POINT ( 'NONE',  ( 96.37500000000000000, 7.950000000000000178, 1.460391307983218535E-15 ) ) ;
#50454 = VECTOR ( 'NONE', #58819, 1000.000000000000000 ) ;
#50455 = DIRECTION ( 'NONE',  ( -0.6830127018922180770, -0.6830127018922204085, -0.2588190451025213501 ) ) ;
#50456 = ORIENTED_EDGE ( 'NONE', *, *, #99925, .F. ) ;
#50457 = ORIENTED_EDGE ( 'NONE', *, *, #15855, .T. ) ;
#50458 = ORIENTED_EDGE ( 'NONE', *, *, #51678, .T. ) ;
#50459 = DIRECTION ( 'NONE',  ( 0.7071067811865486830, -0.7071067811865464625, -0.000000000000000000 ) ) ;
#50460 = DIRECTION ( 'NONE',  ( -0.7071067811865487940, 0.7071067811865463515, -0.000000000000000000 ) ) ;
#50461 = LINE ( 'NONE', #60660, #45411 ) ;
#50462 = CARTESIAN_POINT ( 'NONE',  ( 2.602085213965210642E-15, -15.03360074219759035, 5.000000000000000000 ) ) ;
#50463 = EDGE_CURVE ( 'NONE', #125435, #50934, #4060, .T. ) ;
#50464 =( NAMED_UNIT ( * ) SI_UNIT ( $, .STERADIAN. ) SOLID_ANGLE_UNIT ( ) );
#50465 = CARTESIAN_POINT ( 'NONE',  ( 75.16209685856478018, -5.291415217122919401, 3.054999999999998384 ) ) ;
#50466 = CARTESIAN_POINT ( 'NONE',  ( -30.29974487139158867, -27.71228299555227537, 4.000000000000000000 ) ) ;
#50468 = VECTOR ( 'NONE', #24111, 1000.000000000000000 ) ;
#50467 = CARTESIAN_POINT ( 'NONE',  ( 32.29289321881323360, 20.25929247661551713, 5.000000000000000000 ) ) ;
#50469 = DIRECTION ( 'NONE',  ( 0.7071067811865486830, -0.7071067811865464625, -0.000000000000000000 ) ) ;
#50470 = LINE ( 'NONE', #74371, #30487 ) ;
#50471 = CARTESIAN_POINT ( 'NONE',  ( -2.510786437626908008, -27.52281430457053446, 5.000000000000000000 ) ) ;
#50472 = ORIENTED_EDGE ( 'NONE', *, *, #90940, .T. ) ;
#50473 = CARTESIAN_POINT ( 'NONE',  ( 28.49999999999979750, 3.431123077392151277, 4.000000000000000000 ) ) ;
#50474 = ORIENTED_EDGE ( 'NONE', *, *, #41705, .F. ) ;
#50475 = LINE ( 'NONE', #94661, #66959 ) ;
#50477 = VERTEX_POINT ( 'NONE', #93270 ) ;
#50476 = PLANE ( 'NONE',  #39509 ) ;
#50478 = VECTOR ( 'NONE', #37179, 1000.000000000000000 ) ;
#50479 = LINE ( 'NONE', #92521, #120439 ) ;
#50480 = LINE ( 'NONE', #126580, #65758 ) ;
#50481 = VERTEX_POINT ( 'NONE', #81719 ) ;
#50482 = ORIENTED_EDGE ( 'NONE', *, *, #122197, .T. ) ;
#50483 = CYLINDRICAL_SURFACE ( 'NONE', #108814, 28.00000000000001776 ) ;
#50484 = DIRECTION ( 'NONE',  ( 1.000000000000000000, 0.000000000000000000, 0.000000000000000000 ) ) ;
#50485 = AXIS2_PLACEMENT_3D ( 'NONE', #70232, #116537, #93358 ) ;
#50486 = VECTOR ( 'NONE', #83380, 1000.000000000000227 ) ;
#50487 = LINE ( 'NONE', #17819, #93919 ) ;
#50488 = CARTESIAN_POINT ( 'NONE',  ( 94.57919371712955581, 3.975000000000002753, -6.884901960086283523 ) ) ;
#50489 = PLANE ( 'NONE',  #44060 ) ;
#50490 = ORIENTED_EDGE ( 'NONE', *, *, #92239, .F. ) ;
#50491 = LINE ( 'NONE', #141800, #51557 ) ;
#50492 = EDGE_CURVE ( 'NONE', #6418, #81300, #17147, .T. ) ;
#50493 = DIRECTION ( 'NONE',  ( -0.7071067811865487940, 0.7071067811865463515, 0.000000000000000000 ) ) ;
#50494 = CARTESIAN_POINT ( 'NONE',  ( 19.39583333333332860, 1.633150327867687324, -6.094999999999991758 ) ) ;
#50495 = FILL_AREA_STYLE ('',( #130747 ) ) ;
#50496 = LINE ( 'NONE', #117151, #95389 ) ;
#50497 = ORIENTED_EDGE ( 'NONE', *, *, #122873, .F. ) ;
#50499 = EDGE_CURVE ( 'NONE', #105033, #24914, #49805, .T. ) ;
#50498 = FACE_OUTER_BOUND ( 'NONE', #42131, .T. ) ;
#50500 = ORIENTED_EDGE ( 'NONE', *, *, #111916, .T. ) ;
#50501 = CARTESIAN_POINT ( 'NONE',  ( 82.68793019189809002, 6.110000000000002984, -1.637169565754156730 ) ) ;
#50502 = CARTESIAN_POINT ( 'NONE',  ( -45.18398860626900415, 28.73617430169818832, 5.000000000000000000 ) ) ;
#50503 = FACE_OUTER_BOUND ( 'NONE', #44058, .T. ) ;
#50504 = LINE ( 'NONE', #93988, #29349 ) ;
#50505 = ORIENTED_EDGE ( 'NONE', *, *, #23009, .T. ) ;
#50506 = AXIS2_PLACEMENT_3D ( 'NONE', #130715, #108901, #33547 ) ;
#50507 = EDGE_CURVE ( 'NONE', #50434, #18880, #62098, .T. ) ;
#50508 = CARTESIAN_POINT ( 'NONE',  ( -30.79289321881323716, 18.75929247661552068, 5.000000000000000000 ) ) ;
#50509 = CARTESIAN_POINT ( 'NONE',  ( 117.3291937171295558, -3.975000000000001865, 6.884901960086284411 ) ) ;
#50510 = EDGE_CURVE ( 'NONE', #23479, #15065, #15664, .T. ) ;
#50512 = ORIENTED_EDGE ( 'NONE', *, *, #2387, .F. ) ;
#50511 = CARTESIAN_POINT ( 'NONE',  ( 9.005480084712511157, 28.92564299267931816, 4.000000000000000000 ) ) ;
#50514 = PRESENTATION_LAYER_ASSIGNMENT (  '', '', ( #89815 ) ) ;
#50513 = CARTESIAN_POINT ( 'NONE',  ( 20.51078643762690490, -27.52281430457041012, 5.000000000000000000 ) ) ;
#50515 = DIRECTION ( 'NONE',  ( 0.000000000000000000, -1.000000000000000000, 0.000000000000000000 ) ) ;
#50516 = CARTESIAN_POINT ( 'NONE',  ( 58.75000000000000000, -9.735942053221458872E-16, 7.950000000000000178 ) ) ;
#50517 = EDGE_CURVE ( 'NONE', #126622, #115239, #104114, .T. ) ;
#50519 = ORIENTED_EDGE ( 'NONE', *, *, #80792, .T. ) ;
#50518 = ADVANCED_FACE ( 'NONE', ( #61412 ), #4778, .F. ) ;
#50520 = ORIENTED_EDGE ( 'NONE', *, *, #61151, .F. ) ;
#50521 = CARTESIAN_POINT ( 'NONE',  ( 70.00043019189810423, -3.055000000000002380, 5.291415217122920289 ) ) ;
#50522 = ORIENTED_EDGE ( 'NONE', *, *, #97640, .T. ) ;
#50523 = ADVANCED_FACE ( 'NONE', ( #127320 ), #6218, .F. ) ;
#50524 = CARTESIAN_POINT ( 'NONE',  ( -2.510786437626908008, -27.52281430457053446, 5.000000000000000000 ) ) ;
#50525 = LINE ( 'NONE', #28786, #31543 ) ;
#50526 = ORIENTED_EDGE ( 'NONE', *, *, #126688, .T. ) ;
#50527 = AXIS2_PLACEMENT_3D ( 'NONE', #78231, #76078, #88397 ) ;
#50528 = DIRECTION ( 'NONE',  ( -0.000000000000000000, 0.3543493200069153248, 0.9351131265310292928 ) ) ;
#50529 = DIRECTION ( 'NONE',  ( -0.7071067811865487940, 0.7071067811865463515, -0.000000000000000000 ) ) ;
#50530 = AXIS2_PLACEMENT_3D ( 'NONE', #114792, #3195, #47482 ) ;
#50531 = EDGE_CURVE ( 'NONE', #141627, #136986, #120726, .T. ) ;
#50532 = EDGE_LOOP ( 'NONE', ( #30223, #122447, #121831, #64838 ) ) ;
#50533 = CARTESIAN_POINT ( 'NONE',  ( -24.87009481391958943, 1.845822036158551560, 4.338987337627235874 ) ) ;
#50534 = DIRECTION ( 'NONE',  ( 0.7071067811865487940, 0.7071067811865463515, 0.000000000000000000 ) ) ;
#50535 = EDGE_CURVE ( 'NONE', #34536, #6676, #77273, .T. ) ;
#50536 = ORIENTED_EDGE ( 'NONE', *, *, #129057, .F. ) ;
#50537 = EDGE_LOOP ( 'NONE', ( #16250, #45067, #130729, #59383 ) ) ;
#50538 = LINE ( 'NONE', #15712, #91734 ) ;
#50539 = FACE_OUTER_BOUND ( 'NONE', #20997, .T. ) ;
#50540 = CARTESIAN_POINT ( 'NONE',  ( 3.489213562373097322, -27.52281430457057709, 5.000000000000000000 ) ) ;
#50541 = CARTESIAN_POINT ( 'NONE',  ( -2.588385094051669721, 22.22500000000000142, 4.777194822843815025 ) ) ;
#50542 = EDGE_CURVE ( 'NONE', #41817, #20431, #143205, .T. ) ;
#50543 = CARTESIAN_POINT ( 'NONE',  ( 0.000000000000000000, -21.72500000000000142, 4.500000000000000888 ) ) ;
#50544 = FACE_OUTER_BOUND ( 'NONE', #69076, .T. ) ;
#50545 = ORIENTED_EDGE ( 'NONE', *, *, #118760, .F. ) ;
#50546 = ORIENTED_EDGE ( 'NONE', *, *, #30201, .F. ) ;
#50547 = EDGE_LOOP ( 'NONE', ( #137037, #11581, #25456, #37510 ) ) ;
#50548 = ORIENTED_EDGE ( 'NONE', *, *, #79876, .T. ) ;
#50549 = ADVANCED_FACE ( 'NONE', ( #131629 ), #132369, .F. ) ;
#50550 =( NAMED_UNIT ( * ) PLANE_ANGLE_UNIT ( ) SI_UNIT ( $, .RADIAN. ) );
#50551 = ADVANCED_FACE ( 'NONE', ( #21434 ), #108387, .F. ) ;
#50552 = EDGE_CURVE ( 'NONE', #124775, #39127, #33063, .T. ) ;
#50553 = CYLINDRICAL_SURFACE ( 'NONE', #112286, 3.000000000000000000 ) ;
#50554 = ORIENTED_EDGE ( 'NONE', *, *, #59259, .T. ) ;
#50555 = CARTESIAN_POINT ( 'NONE',  ( 0.000000000000000000, 0.000000000000000000, 7.950000000000000178 ) ) ;
#50556 = CARTESIAN_POINT ( 'NONE',  ( -27.29974487139158512, -27.71228299555225405, 4.000000000000000000 ) ) ;
#50557 = CARTESIAN_POINT ( 'NONE',  ( -6.693269933095949753, -3.740707523384248390, 12.88036043432869171 ) ) ;
#50558 = DIRECTION ( 'NONE',  ( 0.7071067811865487940, 0.7071067811865463515, 0.000000000000000000 ) ) ;
#50559 = VECTOR ( 'NONE', #12911, 1000.000000000000000 ) ;
#50560 = PRESENTATION_LAYER_ASSIGNMENT (  '', '', ( #45931 ) ) ;
#50561 = CARTESIAN_POINT ( 'NONE',  ( -15.07337884938728045, -22.22500000000000142, 12.52252134653477533 ) ) ;
#50562 = VERTEX_POINT ( 'NONE', #98967 ) ;
#50563 = EDGE_CURVE ( 'NONE', #139694, #113402, #64951, .T. ) ;
#50564 = FACE_OUTER_BOUND ( 'NONE', #112501, .T. ) ;
#50565 = CYLINDRICAL_SURFACE ( 'NONE', #11707, 0.5000000000000004441 ) ;
#50566 = VECTOR ( 'NONE', #49686, 1000.000000000000000 ) ;
#50567 = VERTEX_POINT ( 'NONE', #85239 ) ;
#50568 = FACE_OUTER_BOUND ( 'NONE', #44011, .T. ) ;
#50569 = EDGE_LOOP ( 'NONE', ( #114392, #136998, #66920, #1995 ) ) ;
#50570 = EDGE_CURVE ( 'NONE', #99547, #109349, #65699, .T. ) ;
#50571 = VECTOR ( 'NONE', #11353, 1000.000000000000000 ) ;
#50572 = CARTESIAN_POINT ( 'NONE',  ( 11.71247294953710671, 0.000000000000000000, 6.094999999999989981 ) ) ;
#50573 = VERTEX_POINT ( 'NONE', #88119 ) ;
#50574 = ORIENTED_EDGE ( 'NONE', *, *, #85471, .T. ) ;
#50575 = CARTESIAN_POINT ( 'NONE',  ( 76.41709685856476142, 3.054999999999998828, 5.291415217122922066 ) ) ;
#50576 = VECTOR ( 'NONE', #102310, 999.9999999999998863 ) ;
#50577 = VERTEX_POINT ( 'NONE', #52617 ) ;
#50578 = VECTOR ( 'NONE', #94936, 1000.000000000000000 ) ;
#50579 = DIRECTION ( 'NONE',  ( -0.3543493200069162685, -0.000000000000000000, -0.9351131265310288487 ) ) ;
#50580 = DIRECTION ( 'NONE',  ( 0.7071067811865487940, -0.7071067811865463515, 0.000000000000000000 ) ) ;
#50582 =( BOUNDED_CURVE ( )  B_SPLINE_CURVE ( 3, ( #81823, #57213, #136160, #103510 ),
 .UNSPECIFIED., .F., .T. ) 
 B_SPLINE_CURVE_WITH_KNOTS ( ( 4, 4 ),
 ( 3.858351980207633591, 3.926990816987243615 ),
 .UNSPECIFIED. ) 
 CURVE ( )  GEOMETRIC_REPRESENTATION_ITEM ( )  RATIONAL_B_SPLINE_CURVE ( ( 1.000000000000000000, 0.9996074310407765395, 0.9996074310407765395, 1.000000000000000000 ) ) 
 REPRESENTATION_ITEM ( '' )  );
#50581 = CARTESIAN_POINT ( 'NONE',  ( 104.8545968585647756, -1.637169565754161615, 6.110000000000000320 ) ) ;
#50583 = FACE_OUTER_BOUND ( 'NONE', #132176, .T. ) ;
#50584 = EDGE_CURVE ( 'NONE', #12119, #9403, #54789, .T. ) ;
#50585 = DIRECTION ( 'NONE',  ( -0.7071067811865486830, -0.7071067811865464625, 0.000000000000000000 ) ) ;
#50586 = DIRECTION ( 'NONE',  ( -0.000000000000000000, -0.3543493200069152693, 0.9351131265310292928 ) ) ;
#50587 = VECTOR ( 'NONE', #89485, 1000.000000000000000 ) ;
#50588 = ADVANCED_FACE ( 'NONE', ( #43198 ), #141801, .F. ) ;
#50589 = CARTESIAN_POINT ( 'NONE',  ( 57.48921356237308800, -27.52281430457095368, 5.000000000000000000 ) ) ;
#50590 = DIRECTION ( 'NONE',  ( -0.7071067811865486830, -0.7071067811865464625, 0.000000000000000000 ) ) ;
#50591 = DIRECTION ( 'NONE',  ( -0.7071067811865487940, 0.7071067811865463515, 0.000000000000000000 ) ) ;
#50592 = ORIENTED_EDGE ( 'NONE', *, *, #20617, .F. ) ;
#50593 = AXIS2_PLACEMENT_3D ( 'NONE', #105017, #51374, #115149 ) ;
#50594 =( NAMED_UNIT ( * ) PLANE_ANGLE_UNIT ( ) SI_UNIT ( $, .RADIAN. ) );
#50595 = CARTESIAN_POINT ( 'NONE',  ( -18.08491323193750588, -12.74070752338414181, 18.74364270924349896 ) ) ;
#50596 = VERTEX_POINT ( 'NONE', #10528 ) ;
#50597 = ORIENTED_EDGE ( 'NONE', *, *, #124828, .T. ) ;
#50598 = CARTESIAN_POINT ( 'NONE',  ( -60.18398860626900415, 28.73617430169829490, 5.000000000000000000 ) ) ;
#50599 = ORIENTED_EDGE ( 'NONE', *, *, #93110, .T. ) ;
#50600 = AXIS2_PLACEMENT_3D ( 'NONE', #47653, #71517, #91815 ) ;
#50601 = DIRECTION ( 'NONE',  ( 0.7071067811865487940, 0.7071067811865463515, 0.000000000000000000 ) ) ;
#50602 = LINE ( 'NONE', #47785, #66371 ) ;
#50603 = AXIS2_PLACEMENT_3D ( 'NONE', #37762, #127614, #60230 ) ;
#50604 = DIRECTION ( 'NONE',  ( -0.3543493200069162685, -0.000000000000000000, -0.9351131265310288487 ) ) ;
#50605 = CARTESIAN_POINT ( 'NONE',  ( -12.70000000000000284, -34.64999999999999147, -40.00000000000000000 ) ) ;
#50606 = ORIENTED_EDGE ( 'NONE', *, *, #65513, .F. ) ;
#50607 = CARTESIAN_POINT ( 'NONE',  ( 0.6130698085689265664, -49.19053253528954173, 40.77637019027827137 ) ) ;
#50608 = EDGE_LOOP ( 'NONE', ( #94120, #104801, #27167, #101356 ) ) ;
#50609 =( BOUNDED_CURVE ( )  B_SPLINE_CURVE ( 2, ( #26946, #80637, #112533, #5163, #101649, #58209, #13191, #114656, #71195, #69786, #57467, #46625, #90804 ),
 .UNSPECIFIED., .F., .T. ) 
 B_SPLINE_CURVE_WITH_KNOTS ( ( 3, 2, 2, 2, 2, 2, 3 ),
 ( 0.2166666666666666741, 0.2194444444444444420, 0.2222222222222222099, 0.2250000000000000056, 0.2277777777777777735, 0.2305555555555555691, 0.2333333333333333370 ),
 .UNSPECIFIED. ) 
 CURVE ( )  GEOMETRIC_REPRESENTATION_ITEM ( )  RATIONAL_B_SPLINE_CURVE ( ( 1.000000000000000000, 0.9659258262890683122, 1.000000000000000000, 0.9659258262890683122, 1.000000000000000000, 0.9659258262890683122, 1.000000000000000000, 0.9659258262890683122, 1.000000000000000000, 0.9659258262890683122, 1.000000000000000000, 0.9659258262890683122, 1.000000000000000000 ) ) 
 REPRESENTATION_ITEM ( '' )  );
#50610 = EDGE_CURVE ( 'NONE', #52815, #21857, #9058, .T. ) ;
#50611 = CARTESIAN_POINT ( 'NONE',  ( 6.687069808101886004, -2.126176841940956130, 7.934999999999991616 ) ) ;
#50612 = DIRECTION ( 'NONE',  ( 0.7071067811865487940, 0.7071067811865463515, 0.000000000000000000 ) ) ;
#50613 = CARTESIAN_POINT ( 'NONE',  ( 14.29289321881336328, -6.740707523384209310, 5.000000000000000000 ) ) ;
#50614 = CARTESIAN_POINT ( 'NONE',  ( -21.83829387547366707, -6.740707523384205757, 16.75550250614861980 ) ) ;
#50615 = ORIENTED_EDGE ( 'NONE', *, *, #115615, .T. ) ;
#50616 = ORIENTED_EDGE ( 'NONE', *, *, #2197, .T. ) ;
#50617 = ORIENTED_EDGE ( 'NONE', *, *, #111430, .T. ) ;
#50618 = CARTESIAN_POINT ( 'NONE',  ( 32.67183060077623935, -3.740707523384248390, 4.000000000000000000 ) ) ;
#50619 = PLANE ( 'NONE',  #129824 ) ;
#50621 = AXIS2_PLACEMENT_3D ( 'NONE', #109079, #9774, #54041 ) ;
#50620 = LINE ( 'NONE', #94105, #40471 ) ;
#50622 = CARTESIAN_POINT ( 'NONE',  ( -12.70000000000000462, -22.26999999999999247, -0.2071067811865474895 ) ) ;
#50623 = DIRECTION ( 'NONE',  ( 0.6830127018922180770, -0.6830127018922204085, -0.2588190451025213501 ) ) ;
#50624 = VECTOR ( 'NONE', #108910, 1000.000000000000227 ) ;
#50625 = CARTESIAN_POINT ( 'NONE',  ( 4.600000000000001421, 9.521314400968980422E-16, 0.000000000000000000 ) ) ;
#50626 = CARTESIAN_POINT ( 'NONE',  ( -5.999999999999956479, -7.068876922607738145, 4.000000000000000000 ) ) ;
#50627 = DIRECTION ( 'NONE',  ( -0.000000000000000000, 0.000000000000000000, 1.000000000000000000 ) ) ;
#50628 = DIRECTION ( 'NONE',  ( 0.000000000000000000, 0.000000000000000000, -1.000000000000000000 ) ) ;
#50629 = EDGE_LOOP ( 'NONE', ( #77293, #78, #79280, #70921 ) ) ;
#50630 = CARTESIAN_POINT ( 'NONE',  ( 36.18398860626899705, 28.73617430169812437, 5.000000000000000000 ) ) ;
#50631 = CARTESIAN_POINT ( 'NONE',  ( -3.005480084712505828, 28.92564299267936079, 4.000000000000000000 ) ) ;
#50632 = EDGE_LOOP ( 'NONE', ( #114362, #119325, #96165, #128514 ) ) ;
#50633 = CARTESIAN_POINT ( 'NONE',  ( -26.29289321881326558, 17.25929247661554200, 5.000000000000000000 ) ) ;
#50635 = VERTEX_POINT ( 'NONE', #53328 ) ;
#50634 = DIRECTION ( 'NONE',  ( 0.6830127018922181881, 0.6830127018922202975, -0.2588190451025214056 ) ) ;
#50636 = LINE ( 'NONE', #62244, #118622 ) ;
#50637 = CARTESIAN_POINT ( 'NONE',  ( -60.18398860626900415, 28.73617430169829490, 5.000000000000000000 ) ) ;
#50638 = ORIENTED_EDGE ( 'NONE', *, *, #61521, .T. ) ;
#50639 = LINE ( 'NONE', #17970, #30489 ) ;
#50640 = UNCERTAINTY_MEASURE_WITH_UNIT (LENGTH_MEASURE( 1.000000000000000082E-05 ), #38963, 'distance_accuracy_value', 'NONE');
#50641 = ORIENTED_EDGE ( 'NONE', *, *, #138909, .F. ) ;
#50642 = CARTESIAN_POINT ( 'NONE',  ( 34.92499999999998295, 22.22500000000000142, 4.000000000000000000 ) ) ;
#50643 =( BOUNDED_CURVE ( )  B_SPLINE_CURVE ( 3, ( #81434, #50211, #39343, #61811 ),
 .UNSPECIFIED., .F., .T. ) 
 B_SPLINE_CURVE_WITH_KNOTS ( ( 4, 4 ),
 ( 1.864375635226928729, 1.933014472006545859 ),
 .UNSPECIFIED. ) 
 CURVE ( )  GEOMETRIC_REPRESENTATION_ITEM ( )  RATIONAL_B_SPLINE_CURVE ( ( 1.000000000000000000, 0.9996074310407763175, 0.9996074310407763175, 1.000000000000000000 ) ) 
 REPRESENTATION_ITEM ( '' )  );
#50644 = CARTESIAN_POINT ( 'NONE',  ( 123.8916937171295416, 2.130196079827421762, 7.950000000000001066 ) ) ;
#50645 = CARTESIAN_POINT ( 'NONE',  ( -21.18398860626899349, 28.73617430169802134, 5.000000000000000000 ) ) ;
#50646 = LINE ( 'NONE', #106408, #101499 ) ;
#50647 = CARTESIAN_POINT ( 'NONE',  ( 1.171830600776462061, -17.24070752338410628, 4.000000000000000000 ) ) ;
#50648 = CARTESIAN_POINT ( 'NONE',  ( 27.29974487139158512, -27.71228299555225405, 4.000000000000000000 ) ) ;
#50649 = CARTESIAN_POINT ( 'NONE',  ( -17.81601139373099940, 28.73617430169775133, 5.000000000000000000 ) ) ;
#50650 = CARTESIAN_POINT ( 'NONE',  ( 32.35373647476855297, -5.808823158059035485, -5.808823158059033709 ) ) ;
#50651 = CARTESIAN_POINT ( 'NONE',  ( 4.062069808101884227, -7.934999999999990727, -2.126176841940955242 ) ) ;
#50652 = CARTESIAN_POINT ( 'NONE',  ( -12.70000000000000284, -40.42999999999999261, -39.50000000000000000 ) ) ;
#50653 = PLANE ( 'NONE',  #88376 ) ;
#50654 = DIRECTION ( 'NONE',  ( 0.7071067811865487940, 0.7071067811865463515, -0.000000000000000000 ) ) ;
#50655 = ORIENTED_EDGE ( 'NONE', *, *, #36969, .T. ) ;
#50656 = ORIENTED_EDGE ( 'NONE', *, *, #3947, .F. ) ;
#50657 = CARTESIAN_POINT ( 'NONE',  ( 87.18749999999998579, -5.819803920172573086, 5.819803920172572198 ) ) ;
#50658 = ORIENTED_EDGE ( 'NONE', *, *, #66978, .F. ) ;
#50659 = PRESENTATION_STYLE_ASSIGNMENT (( #36924 ) ) ;
#50660 = CARTESIAN_POINT ( 'NONE',  ( -8.700255128608413102, -27.71228299555199825, 4.000000000000000000 ) ) ;
#50661 = FACE_OUTER_BOUND ( 'NONE', #143161, .T. ) ;
#50662 = ORIENTED_EDGE ( 'NONE', *, *, #34573, .T. ) ;
#50663 = VECTOR ( 'NONE', #77171, 1000.000000000000000 ) ;
#50664 = VECTOR ( 'NONE', #43153, 1000.000000000000000 ) ;
#50666 = LINE ( 'NONE', #126783, #122716 ) ;
#50665 = AXIS2_PLACEMENT_3D ( 'NONE', #32736, #141482, #98671 ) ;
#50667 = DIRECTION ( 'NONE',  ( 0.6830127018922180770, -0.6830127018922204085, -0.2588190451025213501 ) ) ;
#50669 = EDGE_CURVE ( 'NONE', #130020, #52896, #92963, .T. ) ;
#50668 = VECTOR ( 'NONE', #139905, 1000.000000000000000 ) ;
#50670 = CARTESIAN_POINT ( 'NONE',  ( -11.99999999999991473, -3.412538124160724884, 4.000000000000000000 ) ) ;
#50671 = CARTESIAN_POINT ( 'NONE',  ( 17.99999999999988276, -13.39766691384881092, -10.96608748226469565 ) ) ;
#50672 = EDGE_CURVE ( 'NONE', #42023, #79690, #46190, .T. ) ;
#50673 = ADVANCED_FACE ( 'NONE', ( #96114 ), #140348, .T. ) ;
#50674 = DIRECTION ( 'NONE',  ( -1.000000000000000000, -0.000000000000000000, -0.000000000000000000 ) ) ;
#50675 = CARTESIAN_POINT ( 'NONE',  ( -24.34427593291135139, 5.931737808750704666, 4.000000000000000000 ) ) ;
#50676 =( NAMED_UNIT ( * ) PLANE_ANGLE_UNIT ( ) SI_UNIT ( $, .RADIAN. ) );
#50678 = CARTESIAN_POINT ( 'NONE',  ( -11.51078643762690490, -27.52281430457047406, 5.000000000000000000 ) ) ;
#50677 = VECTOR ( 'NONE', #133865, 1000.000000000000000 ) ;
#50679 = CARTESIAN_POINT ( 'NONE',  ( 33.48921356237309510, -27.52281430457078670, 5.000000000000000000 ) ) ;
#50680 = DIRECTION ( 'NONE',  ( -0.3543493200069162685, -0.000000000000000000, -0.9351131265310288487 ) ) ;
#50681 = VECTOR ( 'NONE', #132861, 1000.000000000000000 ) ;
#50682 = CARTESIAN_POINT ( 'NONE',  ( -9.183988606268997046, 28.73617430169793607, 5.000000000000000000 ) ) ;
#50683 = CARTESIAN_POINT ( 'NONE',  ( 56.39204447045845825, -48.22435659090886162, 37.54366622512055329 ) ) ;
#50684 = EDGE_CURVE ( 'NONE', #106952, #65100, #142512, .T. ) ;
#50685 = EDGE_CURVE ( 'NONE', #93631, #39593, #41755, .T. ) ;
#50686 = EDGE_LOOP ( 'NONE', ( #100527, #138902, #140958, #124658 ) ) ;
#50687 = ORIENTED_EDGE ( 'NONE', *, *, #7824, .T. ) ;
#50688 = CARTESIAN_POINT ( 'NONE',  ( 98.29209685856477563, -5.291415217122921177, 3.054999999999999272 ) ) ;
#50689 = EDGE_LOOP ( 'NONE', ( #103570, #139139, #52619, #118410 ) ) ;
#50690 = ADVANCED_FACE ( 'NONE', ( #122879 ), #11961, .F. ) ;
#50691 = PRESENTATION_STYLE_ASSIGNMENT (( #128264 ) ) ;
#50692 = CIRCLE ( 'NONE', #89994, 1.749999999999999778 ) ;
#50693 = EDGE_CURVE ( 'NONE', #57164, #66617, #68531, .T. ) ;
#50694 = PLANE ( 'NONE',  #110251 ) ;
#50695 = ORIENTED_EDGE ( 'NONE', *, *, #61450, .F. ) ;
#50696 = CARTESIAN_POINT ( 'NONE',  ( 0.000000000000000000, 0.000000000000000000, 5.000000000000000000 ) ) ;
#50697 = DIRECTION ( 'NONE',  ( 0.6830127018922181881, 0.6830127018922202975, -0.2588190451025214056 ) ) ;
#50698 = EDGE_CURVE ( 'NONE', #130424, #76656, #90243, .T. ) ;
#50699 = AXIS2_PLACEMENT_3D ( 'NONE', #47510, #57648, #89530 ) ;
#50700 = CARTESIAN_POINT ( 'NONE',  ( 91.05793019189812298, 6.110000000000000320, -1.637169565754156064 ) ) ;
#50701 = VERTEX_POINT ( 'NONE', #58394 ) ;
#50702 = CARTESIAN_POINT ( 'NONE',  ( -34.42500000000001137, 0.000000000000000000, 4.500000000000000888 ) ) ;
#50703 = ORIENTED_EDGE ( 'NONE', *, *, #60189, .T. ) ;
#50704 = LINE ( 'NONE', #128275, #80083 ) ;
#50705 = CARTESIAN_POINT ( 'NONE',  ( -59.99451991528749772, 28.92564299267980132, 4.000000000000000000 ) ) ;
#50706 = DIRECTION ( 'NONE',  ( -0.000000000000000000, 0.000000000000000000, 1.000000000000000000 ) ) ;
#50707 = AXIS2_PLACEMENT_3D ( 'NONE', #69995, #125036, #24995 ) ;
#50708 = DIRECTION ( 'NONE',  ( 0.6830127018922180770, -0.6830127018922204085, -0.2588190451025213501 ) ) ;
#50709 = PRESENTATION_LAYER_ASSIGNMENT (  '', '', ( #97015 ) ) ;
#50710 = EDGE_CURVE ( 'NONE', #3311, #63026, #11222, .T. ) ;
#50711 = VECTOR ( 'NONE', #33881, 999.9999999999998863 ) ;
#50712 = ORIENTED_EDGE ( 'NONE', *, *, #5662, .T. ) ;
#50713 = ORIENTED_EDGE ( 'NONE', *, *, #49723, .T. ) ;
#50714 = EDGE_LOOP ( 'NONE', ( #138632, #14018, #119132, #84289 ) ) ;
#50715 = LINE ( 'NONE', #126138, #132542 ) ;
#50716 = LINE ( 'NONE', #117364, #133357 ) ;
#50717 = CARTESIAN_POINT ( 'NONE',  ( 13.04623647476855375, -7.934999999999990727, 4.858786175617117713E-16 ) ) ;
#50718 = EDGE_CURVE ( 'NONE', #105033, #58332, #55501, .T. ) ;
#50719 = DIRECTION ( 'NONE',  ( 0.000000000000000000, -1.000000000000000000, 0.000000000000000000 ) ) ;
#50720 = EDGE_LOOP ( 'NONE', ( #41844, #66879, #18225, #106360 ) ) ;
#50721 = ORIENTED_EDGE ( 'NONE', *, *, #13226, .T. ) ;
#50722 = CARTESIAN_POINT ( 'NONE',  ( -13.22578070446010301, 4.485909045323550615, 4.327832195654622183 ) ) ;
#50723 = ORIENTED_EDGE ( 'NONE', *, *, #79742, .F. ) ;
#50724 = ORIENTED_EDGE ( 'NONE', *, *, #27860, .F. ) ;
#50725 = EDGE_CURVE ( 'NONE', #55173, #43690, #133765, .T. ) ;
#50726 = COLOUR_RGB ( '', 0.66274510, 0.83137255, 0.94901961) ;
#50727 = CARTESIAN_POINT ( 'NONE',  ( 112.6412635252314658, 4.472830434245835818, 4.472830434245840259 ) ) ;
#50728 = ADVANCED_FACE ( 'NONE', ( #33760 ), #56945, .F. ) ;
#50729 = DIRECTION ( 'NONE',  ( 0.7071067811865487940, 0.7071067811865463515, -0.000000000000000000 ) ) ;
#50730 = DIRECTION ( 'NONE',  ( -0.000000000000000000, 0.3543493200069153248, 0.9351131265310292928 ) ) ;
#50731 = ORIENTED_EDGE ( 'NONE', *, *, #119286, .T. ) ;
#50732 = CARTESIAN_POINT ( 'NONE',  ( -21.18398860626899349, 28.73617430169802134, 5.000000000000000000 ) ) ;
#50733 = EDGE_CURVE ( 'NONE', #68374, #101800, #44656, .T. ) ;
#50734 = CARTESIAN_POINT ( 'NONE',  ( 30.18398860626900060, 28.73617430169808173, 5.000000000000000000 ) ) ;
#50735 = CARTESIAN_POINT ( 'NONE',  ( -34.42500000000001137, 0.000000000000000000, 4.500000000000000888 ) ) ;
#50736 = CARTESIAN_POINT ( 'NONE',  ( 6.540657738503846907, 4.202752102959690472E-16, 0.000000000000000000 ) ) ;
#50737 = VERTEX_POINT ( 'NONE', #102577 ) ;
#50738 = ADVANCED_FACE ( 'NONE', ( #101116 ), #13376, .F. ) ;
#50739 = CARTESIAN_POINT ( 'NONE',  ( 68.99451991528748351, 28.92564299267986172, 4.000000000000000000 ) ) ;
#50740 = FACE_BOUND ( 'NONE', #92790, .T. ) ;
#50741 = ORIENTED_EDGE ( 'NONE', *, *, #80202, .F. ) ;
#50742 = FACE_OUTER_BOUND ( 'NONE', #93197, .T. ) ;
#50743 = CARTESIAN_POINT ( 'NONE',  ( 3.423278458063512719, 11.25929247661559529, 17.85071094206583808 ) ) ;
#50744 = FILL_AREA_STYLE_COLOUR ( '', #102424 ) ;
#50745 = ORIENTED_EDGE ( 'NONE', *, *, #15485, .F. ) ;
#50746 = CARTESIAN_POINT ( 'NONE',  ( 27.48921356237309155, -27.52281430457074762, 5.000000000000000000 ) ) ;
#50747 = ORIENTED_EDGE ( 'NONE', *, *, #47048, .F. ) ;
#50748 = ORIENTED_EDGE ( 'NONE', *, *, #21836, .T. ) ;
#50749 = EDGE_CURVE ( 'NONE', #134120, #101708, #99686, .T. ) ;
#50750 = ORIENTED_EDGE ( 'NONE', *, *, #88891, .T. ) ;
#50751 = CARTESIAN_POINT ( 'NONE',  ( 30.53709685856477307, -3.054999999999998828, -5.291415217122919401 ) ) ;
#50752 = CYLINDRICAL_SURFACE ( 'NONE', #48336, 0.5000000000000004441 ) ;
#50753 = DIRECTION ( 'NONE',  ( -0.000000000000000000, 0.3543493200069153248, 0.9351131265310292928 ) ) ;
#50754 = LINE ( 'NONE', #96356, #80892 ) ;
#50755 = LINE ( 'NONE', #6475, #56689 ) ;
#50756 = EDGE_CURVE ( 'NONE', #9912, #91707, #135898, .T. ) ;
#50757 = DIRECTION ( 'NONE',  ( -0.000000000000000000, 0.3543493200069153248, 0.9351131265310292928 ) ) ;
#50758 = FACE_OUTER_BOUND ( 'NONE', #33383, .T. ) ;
#50759 = CARTESIAN_POINT ( 'NONE',  ( 54.48921356237310221, -27.52281430457093236, 5.000000000000000000 ) ) ;
#50760 = LINE ( 'NONE', #20246, #29785 ) ;
#50761 = DIRECTION ( 'NONE',  ( -0.7071067811865487940, 0.7071067811865463515, 0.000000000000000000 ) ) ;
#50762 = CARTESIAN_POINT ( 'NONE',  ( -20.16347128873438521, 15.75929247661555799, 9.299976744542872709 ) ) ;
#50763 = VERTEX_POINT ( 'NONE', #36575 ) ;
#50764 = ORIENTED_EDGE ( 'NONE', *, *, #605, .F. ) ;
#50765 = VECTOR ( 'NONE', #8750, 1000.000000000000114 ) ;
#50766 = VERTEX_POINT ( 'NONE', #123630 ) ;
#50767 = VERTEX_POINT ( 'NONE', #80824 ) ;
#50768 = DIRECTION ( 'NONE',  ( 0.000000000000000000, 1.000000000000000000, 0.000000000000000000 ) ) ;
#50769 = VECTOR ( 'NONE', #5270, 1000.000000000000114 ) ;
#50770 = VECTOR ( 'NONE', #59061, 1000.000000000000000 ) ;
#50771 = ORIENTED_EDGE ( 'NONE', *, *, #105014, .F. ) ;
#50773 = ORIENTED_EDGE ( 'NONE', *, *, #143462, .F. ) ;
#50772 = VECTOR ( 'NONE', #32389, 1000.000000000000000 ) ;
#50774 = CARTESIAN_POINT ( 'NONE',  ( 19.41999999999999815, 9.521314400968980422E-16, 0.000000000000000000 ) ) ;
#50775 = DIRECTION ( 'NONE',  ( 0.7071067811865486830, -0.7071067811865464625, -0.000000000000000000 ) ) ;
#50776 = ADVANCED_FACE ( 'NONE', ( #125015 ), #57653, .F. ) ;
#50777 = DIRECTION ( 'NONE',  ( -0.000000000000000000, -0.3543493200069152693, 0.9351131265310292928 ) ) ;
#50778 = ORIENTED_EDGE ( 'NONE', *, *, #57502, .F. ) ;
#50779 = DIRECTION ( 'NONE',  ( -1.000000000000000000, -0.000000000000000000, -0.000000000000000000 ) ) ;
#50781 = EDGE_LOOP ( 'NONE', ( #80223, #81641, #113387, #2794 ) ) ;
#50780 = CIRCLE ( 'NONE', #140998, 2.500000000000000888 ) ;
#50782 = CARTESIAN_POINT ( 'NONE',  ( 34.49999999999976552, 21.05432934483073026, 4.994342998332161443 ) ) ;
#50783 = CARTESIAN_POINT ( 'NONE',  ( 32.87956980810189123, 3.967499999999998916, 6.871911579029510442 ) ) ;
#50784 = CARTESIAN_POINT ( 'NONE',  ( 5.754569808101886785, -6.871911579029512218, 3.967499999999996252 ) ) ;
#50785 = ORIENTED_EDGE ( 'NONE', *, *, #108991, .F. ) ;
#50786 = CARTESIAN_POINT ( 'NONE',  ( 100.2454301918981230, -5.291415217122919401, -3.055000000000000604 ) ) ;
#50787 = LINE ( 'NONE', #106556, #113788 ) ;
#50788 = LINE ( 'NONE', #117438, #55847 ) ;
#50789 = VERTEX_POINT ( 'NONE', #66376 ) ;
#50790 = ORIENTED_EDGE ( 'NONE', *, *, #98081, .T. ) ;
#50791 = DIRECTION ( 'NONE',  ( -0.6830127018922180770, -0.6830127018922204085, -0.2588190451025213501 ) ) ;
#50792 = EDGE_LOOP ( 'NONE', ( #131013, #113991, #65935, #10044 ) ) ;
#50793 = AXIS2_PLACEMENT_3D ( 'NONE', #102722, #95931, #115682 ) ;
#50794 = FACE_OUTER_BOUND ( 'NONE', #90884, .T. ) ;
#50796 = CARTESIAN_POINT ( 'NONE',  ( -30.18398860626900060, 28.73617430169808173, 5.000000000000000000 ) ) ;
#50795 = AXIS2_PLACEMENT_3D ( 'NONE', #122092, #133018, #141742 ) ;
#50797 = CARTESIAN_POINT ( 'NONE',  ( -21.79289321881330110, 18.75929247661552779, 5.000000000000000000 ) ) ;
#50798 = LINE ( 'NONE', #63128, #5647 ) ;
#50799 = CARTESIAN_POINT ( 'NONE',  ( 183.4813685602576925, -52.14999999947626463, -41.03936837847464858 ) ) ;
#50801 = EDGE_CURVE ( 'NONE', #141779, #140054, #78670, .T. ) ;
#50800 = EDGE_LOOP ( 'NONE', ( #104731, #24592, #76958 ) ) ;
#50802 = CYLINDRICAL_SURFACE ( 'NONE', #106088, 0.5000000000000004441 ) ;
#50803 = AXIS2_PLACEMENT_3D ( 'NONE', #77787, #902, #35744 ) ;
#50804 = EDGE_CURVE ( 'NONE', #14634, #131639, #124306, .T. ) ;
#50805 = LINE ( 'NONE', #53672, #218 ) ;
#50806 = DIRECTION ( 'NONE',  ( -0.7071067811865486830, -0.7071067811865464625, 0.000000000000000000 ) ) ;
#50807 = VERTEX_POINT ( 'NONE', #110548 ) ;
#50808 = DIRECTION ( 'NONE',  ( 0.000000000000000000, -1.000000000000000000, 0.000000000000000000 ) ) ;
#50809 = CIRCLE ( 'NONE', #6770, 2.500000000000000444 ) ;
#50811 = MECHANICAL_DESIGN_GEOMETRIC_PRESENTATION_REPRESENTATION (  '', ( #108712 ), #62414 ) ;
#50810 = CARTESIAN_POINT ( 'NONE',  ( 8.994519915287490619, 28.92564299267944250, 4.000000000000000000 ) ) ;
#50812 = ORIENTED_EDGE ( 'NONE', *, *, #11047, .T. ) ;
#50813 = VECTOR ( 'NONE', #121413, 1000.000000000000000 ) ;
#50815 = ORIENTED_EDGE ( 'NONE', *, *, #3240, .F. ) ;
#50814 = CARTESIAN_POINT ( 'NONE',  ( 0.6713702758573106832, -52.14999999999999147, -41.05044666116291552 ) ) ;
#50816 = EDGE_CURVE ( 'NONE', #15918, #76576, #109476, .T. ) ;
#50818 = ORIENTED_EDGE ( 'NONE', *, *, #136700, .T. ) ;
#50817 = VECTOR ( 'NONE', #76201, 1000.000000000000000 ) ;
#50819 = DIRECTION ( 'NONE',  ( -0.5735764363510501562, 0.8191520442889890230, 1.003171929053521419E-16 ) ) ;
#50820 = VECTOR ( 'NONE', #65859, 1000.000000000000000 ) ;
#50821 = SURFACE_STYLE_USAGE ( .BOTH. , #93609 ) ;
#50822 = EDGE_LOOP ( 'NONE', ( #58236, #111754, #16842, #36868, #73891 ) ) ;
#50823 = FACE_OUTER_BOUND ( 'NONE', #21142, .T. ) ;
#50824 = VECTOR ( 'NONE', #101220, 1000.000000000000000 ) ;
#50825 = DIRECTION ( 'NONE',  ( -0.6830127018922181881, 0.6830127018922202975, -0.2588190451025214056 ) ) ;
#50826 = DIRECTION ( 'NONE',  ( -0.7071067811865487940, 0.7071067811865463515, 0.000000000000000000 ) ) ;
#50827 = CARTESIAN_POINT ( 'NONE',  ( 13.96000000000000085, 2.055000000000001492, 0.000000000000000000 ) ) ;
#50828 = CARTESIAN_POINT ( 'NONE',  ( -34.92500000000001137, -22.22500000000000142, 4.000000000000000000 ) ) ;
#50829 = CARTESIAN_POINT ( 'NONE',  ( 20.74722711705611644, 22.22500000000000142, -16.09628799178753766 ) ) ;
#50830 = CARTESIAN_POINT ( 'NONE',  ( 3.183988606268992161, 28.73617430169789699, 5.000000000000000000 ) ) ;
#50831 = VECTOR ( 'NONE', #49949, 1000.000000000000000 ) ;
#50832 = DIRECTION ( 'NONE',  ( -0.000000000000000000, 0.000000000000000000, 1.000000000000000000 ) ) ;
#50833 = CARTESIAN_POINT ( 'NONE',  ( 14.51078643762690490, -27.52281430457045275, 5.000000000000000000 ) ) ;
#50834 =( LENGTH_UNIT ( ) NAMED_UNIT ( * ) SI_UNIT ( .MILLI., .METRE. ) );
#50835 = ORIENTED_EDGE ( 'NONE', *, *, #54641, .F. ) ;
#50836 = ORIENTED_EDGE ( 'NONE', *, *, #99334, .F. ) ;
#50837 = ORIENTED_EDGE ( 'NONE', *, *, #91676, .F. ) ;
#50838 = CARTESIAN_POINT ( 'NONE',  ( 112.2708333333333144, -7.949999999999999289, -2.130196079827426203 ) ) ;
#50839 = ORIENTED_EDGE ( 'NONE', *, *, #52176, .F. ) ;
#50840 = ORIENTED_EDGE ( 'NONE', *, *, #17954, .T. ) ;
#50841 = ORIENTED_EDGE ( 'NONE', *, *, #4471, .F. ) ;
#50842 = FILL_AREA_STYLE_COLOUR ( '', #29411 ) ;
#50843 = LINE ( 'NONE', #95033, #118007 ) ;
#50844 = EDGE_LOOP ( 'NONE', ( #117220, #118608, #5736, #118339 ) ) ;
#50845 = DIRECTION ( 'NONE',  ( 1.000000000000000000, 0.000000000000000000, 0.000000000000000000 ) ) ;
#50846 = DIRECTION ( 'NONE',  ( -0.7071067811865487940, 0.7071067811865463515, -0.000000000000000000 ) ) ;
#50847 = CARTESIAN_POINT ( 'NONE',  ( -24.18398860626899705, 28.73617430169804265, 5.000000000000000000 ) ) ;
#50848 = FACE_OUTER_BOUND ( 'NONE', #15889, .T. ) ;
#50849 = CARTESIAN_POINT ( 'NONE',  ( 102.0837635252314328, -6.110000000000001208, -3.741295971395164515E-16 ) ) ;
#50850 = ORIENTED_EDGE ( 'NONE', *, *, #30784, .T. ) ;
#50851 = EDGE_CURVE ( 'NONE', #62405, #137509, #22811, .T. ) ;
#50852 = CARTESIAN_POINT ( 'NONE',  ( -13.27644930412397350, 4.689949953678146599, 5.000000000000000000 ) ) ;
#50853 = DIRECTION ( 'NONE',  ( -0.7071067811865486830, -0.7071067811865464625, 0.000000000000000000 ) ) ;
#50854 = LINE ( 'NONE', #40699, #19607 ) ;
#50855 = LINE ( 'NONE', #5881, #68402 ) ;
#50856 = CARTESIAN_POINT ( 'NONE',  ( -23.57672154193631542, 11.25929247661559529, 17.85071094206589493 ) ) ;
#50857 = DIRECTION ( 'NONE',  ( 0.000000000000000000, 0.000000000000000000, 1.000000000000000000 ) ) ;
#50858 = CARTESIAN_POINT ( 'NONE',  ( 36.24586038379622011, 3.974999999999996980, 6.884901960086287964 ) ) ;
#50859 = CARTESIAN_POINT ( 'NONE',  ( -12.20000000000000284, -40.42999999999999261, 19.06900128115122328 ) ) ;
#50860 = ADVANCED_FACE ( 'NONE', ( #72110 ), #84399, .F. ) ;
#50861 = EDGE_CURVE ( 'NONE', #111356, #38643, #114824, .T. ) ;
#50862 = DIRECTION ( 'NONE',  ( 0.000000000000000000, -1.000000000000000000, 0.000000000000000000 ) ) ;
#50863 = VERTEX_POINT ( 'NONE', #27846 ) ;
#50864 = EDGE_LOOP ( 'NONE', ( #93942, #54612, #106597, #129719, #41083 ) ) ;
#50865 = CARTESIAN_POINT ( 'NONE',  ( 25.64583333333332504, 2.130196079827431976, -7.949999999999999289 ) ) ;
#50866 = ADVANCED_FACE ( 'NONE', ( #71367 ), #138767, .F. ) ;
#50867 = ORIENTED_EDGE ( 'NONE', *, *, #114029, .T. ) ;
#50868 = DIRECTION ( 'NONE',  ( -0.7071067811865486830, -0.7071067811865464625, -0.000000000000000000 ) ) ;
#50869 = EDGE_CURVE ( 'NONE', #22009, #19810, #16979, .T. ) ;
#50870 = CARTESIAN_POINT ( 'NONE',  ( 77.99451991528749772, 28.92564299267992567, 4.000000000000000000 ) ) ;
#50871 = EDGE_CURVE ( 'NONE', #94372, #98076, #59098, .T. ) ;
#50872 = CARTESIAN_POINT ( 'NONE',  ( 21.29974487139158512, -27.71228299555221142, 4.000000000000000000 ) ) ;
#50873 =( LENGTH_UNIT ( ) NAMED_UNIT ( * ) SI_UNIT ( .MILLI., .METRE. ) );
#50874 = DIRECTION ( 'NONE',  ( -0.7071067811865487940, 0.7071067811865463515, 0.000000000000000000 ) ) ;
#50875 = ADVANCED_FACE ( 'NONE', ( #27125 ), #103948, .F. ) ;
#50876 = CARTESIAN_POINT ( 'NONE',  ( 25.95876352523143638, 0.000000000000000000, -6.110000000000001208 ) ) ;
#50877 = ORIENTED_EDGE ( 'NONE', *, *, #36349, .T. ) ;
#50878 = CARTESIAN_POINT ( 'NONE',  ( 2.999999999999978240, -18.03360074219755660, 5.000000000000000000 ) ) ;
#50879 = EDGE_LOOP ( 'NONE', ( #19859, #8216, #52094, #8276 ) ) ;
#50880 = CARTESIAN_POINT ( 'NONE',  ( -72.48921356237309510, -27.52281430457106026, 5.000000000000000000 ) ) ;
#50881 = VECTOR ( 'NONE', #17780, 999.9999999999998863 ) ;
#50882 = AXIS2_PLACEMENT_3D ( 'NONE', #129217, #142959, #108871 ) ;
#50883 = LINE ( 'NONE', #116121, #43057 ) ;
#50885 =( BOUNDED_CURVE ( )  B_SPLINE_CURVE ( 2, ( #81816, #38280, #47076, #102116, #82499, #101383, #81084, #13642, #79694, #92631, #123876, #2028, #2778 ),
 .UNSPECIFIED., .F., .T. ) 
 B_SPLINE_CURVE_WITH_KNOTS ( ( 3, 2, 2, 2, 2, 2, 3 ),
 ( 0.2999999999999999889, 0.3027777777777777568, 0.3055555555555555802, 0.3083333333333333481, 0.3111111111111111160, 0.3138888888888888840, 0.3166666666666666519 ),
 .UNSPECIFIED. ) 
 CURVE ( )  GEOMETRIC_REPRESENTATION_ITEM ( )  RATIONAL_B_SPLINE_CURVE ( ( 1.000000000000000000, 0.9659258262890683122, 1.000000000000000000, 0.9659258262890683122, 1.000000000000000000, 0.9659258262890683122, 1.000000000000000000, 0.9659258262890683122, 1.000000000000000000, 0.9659258262890683122, 1.000000000000000000, 0.9659258262890683122, 1.000000000000000000 ) ) 
 REPRESENTATION_ITEM ( '' )  );
#50884 = PLANE ( 'NONE',  #122786 ) ;
#50886 = AXIS2_PLACEMENT_3D ( 'NONE', #132983, #120616, #10436 ) ;
#50887 = ADVANCED_FACE ( 'NONE', ( #39462 ), #126433, .F. ) ;
#50888 = CARTESIAN_POINT ( 'NONE',  ( 2.994519915287485734, 28.92564299267940342, 4.000000000000000000 ) ) ;
#50889 = ORIENTED_EDGE ( 'NONE', *, *, #30909, .F. ) ;
#50890 = CARTESIAN_POINT ( 'NONE',  ( 46.37543019189810423, -5.291415217122920289, -3.055000000000001492 ) ) ;
#50891 = ADVANCED_FACE ( 'NONE', ( #125754 ), #3904, .T. ) ;
#50892 = VERTEX_POINT ( 'NONE', #116989 ) ;
#50893 = CARTESIAN_POINT ( 'NONE',  ( -30.48921356237309510, -27.52281430457076894, 5.000000000000000000 ) ) ;
#50894 = CARTESIAN_POINT ( 'NONE',  ( -32.99999999999976552, -3.033600742197708477, 5.000000000000000000 ) ) ;
#50895 = DIRECTION ( 'NONE',  ( -1.000000000000000000, -1.224606353822377258E-16, -0.000000000000000000 ) ) ;
#50896 = CARTESIAN_POINT ( 'NONE',  ( 28.00000000000002487, -52.14999999999999147, 34.92500000000003268 ) ) ;
#50897 = AXIS2_PLACEMENT_3D ( 'NONE', #99114, #88285, #143358 ) ;
#50898 = EDGE_CURVE ( 'NONE', #131955, #73568, #114139, .T. ) ;
#50899 = VECTOR ( 'NONE', #8151, 1000.000000000000000 ) ;
#50900 = CARTESIAN_POINT ( 'NONE',  ( 51.68293019189811588, -1.637169565754158951, -6.109999999999998543 ) ) ;
#50901 = ORIENTED_EDGE ( 'NONE', *, *, #105018, .F. ) ;
#50902 = DIRECTION ( 'NONE',  ( -0.000000000000000000, 0.000000000000000000, 1.000000000000000000 ) ) ;
#50903 = CARTESIAN_POINT ( 'NONE',  ( -22.49999999999984013, 12.05218569542904561, 5.000000000000000000 ) ) ;
#50904 = ORIENTED_EDGE ( 'NONE', *, *, #970, .F. ) ;
#50905 = ORIENTED_EDGE ( 'NONE', *, *, #102951, .F. ) ;
#50906 = AXIS2_PLACEMENT_3D ( 'NONE', #113950, #111060, #80627 ) ;
#50907 = VECTOR ( 'NONE', #44343, 1000.000000000000000 ) ;
#50908 = CARTESIAN_POINT ( 'NONE',  ( 10.49999999999992539, -14.56887692260766087, 4.000000000000000000 ) ) ;
#50909 = ORIENTED_EDGE ( 'NONE', *, *, #8467, .T. ) ;
#50910 = DIRECTION ( 'NONE',  ( -0.7071067811865487940, 0.7071067811865463515, -0.000000000000000000 ) ) ;
#50911 = ORIENTED_EDGE ( 'NONE', *, *, #59423, .T. ) ;
#50912 = CARTESIAN_POINT ( 'NONE',  ( 2.292893218813443657, -3.740707523384248390, 5.000000000000000000 ) ) ;
#50913 = EDGE_CURVE ( 'NONE', #127807, #7538, #4596, .T. ) ;
#50914 = DIRECTION ( 'NONE',  ( -0.7071067811865486830, -0.7071067811865464625, 0.000000000000000000 ) ) ;
#50915 = VECTOR ( 'NONE', #43923, 999.9999999999998863 ) ;
#50916 = VECTOR ( 'NONE', #72645, 999.9999999999998863 ) ;
#50918 = AXIS2_PLACEMENT_3D ( 'NONE', #115870, #17976, #17296 ) ;
#50917 = DIRECTION ( 'NONE',  ( -0.3543493200069163240, -0.000000000000000000, 0.9351131265310288487 ) ) ;
#50919 = FACE_BOUND ( 'NONE', #31345, .T. ) ;
#50920 = PLANE ( 'NONE',  #78087 ) ;
#50921 = VECTOR ( 'NONE', #58603, 1000.000000000000000 ) ;
#50922 = DIRECTION ( 'NONE',  ( -0.6830127018922181881, 0.6830127018922202975, -0.2588190451025214056 ) ) ;
#50923 = CARTESIAN_POINT ( 'NONE',  ( 34.42499999999998295, 10.54139925780192932, 5.000000000000000000 ) ) ;
#50924 = VERTEX_POINT ( 'NONE', #40191 ) ;
#50925 = SURFACE_STYLE_USAGE ( .BOTH. , #19700 ) ;
#50927 = ORIENTED_EDGE ( 'NONE', *, *, #114096, .F. ) ;
#50926 = CARTESIAN_POINT ( 'NONE',  ( -9.299744871391588674, -27.71228299555212971, 4.000000000000000000 ) ) ;
#50928 = VECTOR ( 'NONE', #79968, 1000.000000000000000 ) ;
#50929 = EDGE_LOOP ( 'NONE', ( #94784, #98258, #59238, #121914 ) ) ;
#50930 = DIRECTION ( 'NONE',  ( -1.000000000000000000, -0.000000000000000000, -0.000000000000000000 ) ) ;
#50931 = EDGE_CURVE ( 'NONE', #118585, #10464, #127148, .T. ) ;
#50932 = ORIENTED_EDGE ( 'NONE', *, *, #53683, .T. ) ;
#50933 = CARTESIAN_POINT ( 'NONE',  ( 57.95376352523144448, -6.109999999999998543, -3.741295971395162543E-16 ) ) ;
#50934 = VERTEX_POINT ( 'NONE', #92366 ) ;
#50935 = FACE_OUTER_BOUND ( 'NONE', #26851, .T. ) ;
#50936 = CARTESIAN_POINT ( 'NONE',  ( -7.140000000000000568, -35.14999999999999147, -39.79289321881344677 ) ) ;
#50937 = EDGE_CURVE ( 'NONE', #48062, #48429, #5356, .T. ) ;
#50938 = EDGE_LOOP ( 'NONE', ( #98999, #76328, #23114, #35587, #9693 ) ) ;
#50939 = CARTESIAN_POINT ( 'NONE',  ( 36.18398860626899705, 28.73617430169812437, 5.000000000000000000 ) ) ;
#50940 = VECTOR ( 'NONE', #119113, 1000.000000000000000 ) ;
#50941 = CARTESIAN_POINT ( 'NONE',  ( 34.39583333333332860, -2.130196079827351596, 7.950000000000043698 ) ) ;
#50942 = ADVANCED_FACE ( 'NONE', ( #94513 ), #48905, .T. ) ;
#50943 = CARTESIAN_POINT ( 'NONE',  ( 102.2083333333333286, -3.974999999999999201, -6.884901960086287964 ) ) ;
#50944 = DIRECTION ( 'NONE',  ( 0.6830127018922180770, -0.6830127018922204085, -0.2588190451025213501 ) ) ;
#50945 = CARTESIAN_POINT ( 'NONE',  ( -15.18398860626900237, 28.73617430169797871, 5.000000000000000000 ) ) ;
#50946 = CARTESIAN_POINT ( 'NONE',  ( 11.20710678118646975, 3.759292476615673007, 5.000000000000000000 ) ) ;
#50947 = ORIENTED_EDGE ( 'NONE', *, *, #18036, .F. ) ;
#50948 = VECTOR ( 'NONE', #63974, 1000.000000000000000 ) ;
#50949 = ORIENTED_EDGE ( 'NONE', *, *, #33574, .F. ) ;
#50950 = CARTESIAN_POINT ( 'NONE',  ( -3.183988606268992161, 28.73617430169789699, 5.000000000000000000 ) ) ;
#50951 = DIRECTION ( 'NONE',  ( -1.000000000000000000, -1.224606353822377258E-16, -0.000000000000000000 ) ) ;
#50952 = ORIENTED_EDGE ( 'NONE', *, *, #134100, .T. ) ;
#50953 = ORIENTED_EDGE ( 'NONE', *, *, #59774, .T. ) ;
#50954 = ORIENTED_EDGE ( 'NONE', *, *, #102262, .F. ) ;
#50955 = LINE ( 'NONE', #68615, #134637 ) ;
#50956 = EDGE_CURVE ( 'NONE', #488, #37639, #6755, .T. ) ;
#50957 = FACE_OUTER_BOUND ( 'NONE', #102044, .T. ) ;
#50958 = ORIENTED_EDGE ( 'NONE', *, *, #87813, .T. ) ;
#50959 = CARTESIAN_POINT ( 'NONE',  ( 25.73493329717933875, 12.75929247661558996, 18.34774599283950280 ) ) ;
#50960 = CARTESIAN_POINT ( 'NONE',  ( -34.92500000000001137, -22.22500000000000142, 4.500000000000000888 ) ) ;
#50961 = CARTESIAN_POINT ( 'NONE',  ( 13.19206980810188412, -7.934999999999991616, -2.126176841940955242 ) ) ;
#50962 = DIRECTION ( 'NONE',  ( 0.5735764363510451602, 0.8191520442889924647, 0.000000000000000000 ) ) ;
#50963 = ORIENTED_EDGE ( 'NONE', *, *, #79615, .T. ) ;
#50964 = FACE_OUTER_BOUND ( 'NONE', #78945, .T. ) ;
#50965 = CARTESIAN_POINT ( 'NONE',  ( 17.99999999999987566, -7.068876922607736368, 4.000000000000000000 ) ) ;
#50966 = CARTESIAN_POINT ( 'NONE',  ( 0.000000000000000000, 0.000000000000000000, 5.000000000000000000 ) ) ;
#50968 = VERTEX_POINT ( 'NONE', #60509 ) ;
#50967 = CARTESIAN_POINT ( 'NONE',  ( -9.489213562373095101, -27.52281430457062328, 5.000000000000000000 ) ) ;
#50969 = LINE ( 'NONE', #16149, #23964 ) ;
#50970 = ORIENTED_EDGE ( 'NONE', *, *, #9053, .T. ) ;
#50971 = LINE ( 'NONE', #95167, #56546 ) ;
#50972 = PLANE ( 'NONE',  #5290 ) ;
#50973 = CARTESIAN_POINT ( 'NONE',  ( 108.6250000000000000, -7.950000000000000178, -4.867971026610729436E-16 ) ) ;
#50974 = ORIENTED_EDGE ( 'NONE', *, *, #90496, .F. ) ;
#50975 = AXIS2_PLACEMENT_3D ( 'NONE', #55612, #31011, #109968 ) ;
#50976 = EDGE_CURVE ( 'NONE', #1799, #31655, #49640, .T. ) ;
#50977 = LINE ( 'NONE', #93046, #12411 ) ;
#50978 = PLANE ( 'NONE',  #115807 ) ;
#50979 = FACE_OUTER_BOUND ( 'NONE', #54327, .T. ) ;
#50980 = VECTOR ( 'NONE', #51064, 1000.000000000000000 ) ;
#50981 = EDGE_LOOP ( 'NONE', ( #127860, #109657, #135244, #78052 ) ) ;
#50982 = VECTOR ( 'NONE', #127443, 999.9999999999998863 ) ;
#50983 = VECTOR ( 'NONE', #108716, 1000.000000000000000 ) ;
#50984 = PRESENTATION_LAYER_ASSIGNMENT (  '', '', ( #53231 ) ) ;
#50985 = PLANE ( 'NONE',  #62493 ) ;
#50986 = DIRECTION ( 'NONE',  ( -0.7071067811865486830, 0.7071067811865464625, 0.000000000000000000 ) ) ;
#50987 = CARTESIAN_POINT ( 'NONE',  ( -24.18398860626899705, 28.73617430169804265, 5.000000000000000000 ) ) ;
#50988 = VECTOR ( 'NONE', #33495, 1000.000000000000000 ) ;
#50989 = DIRECTION ( 'NONE',  ( -1.000000000000000000, 0.000000000000000000, -0.000000000000000000 ) ) ;
#50990 = DIRECTION ( 'NONE',  ( -0.7071067811865486830, 0.7071067811865464625, 0.000000000000000000 ) ) ;
#50991 = ORIENTED_EDGE ( 'NONE', *, *, #116443, .F. ) ;
#50992 = EDGE_CURVE ( 'NONE', #103755, #122142, #141617, .T. ) ;
#50993 = ORIENTED_EDGE ( 'NONE', *, *, #21883, .T. ) ;
#50994 = DIRECTION ( 'NONE',  ( 0.7071067811865487940, 0.7071067811865463515, -0.000000000000000000 ) ) ;
#50995 = AXIS2_PLACEMENT_3D ( 'NONE', #62451, #69225, #124300 ) ;
#50996 = DIRECTION ( 'NONE',  ( -1.000000000000000000, -1.224606353822377258E-16, -0.000000000000000000 ) ) ;
#50997 = CARTESIAN_POINT ( 'NONE',  ( 10.91623647476855297, -7.934999999999990727, 4.858786175617117713E-16 ) ) ;
#50998 = DIRECTION ( 'NONE',  ( -0.6830127018922181881, 0.6830127018922202975, -0.2588190451025214056 ) ) ;
#50999 = CARTESIAN_POINT ( 'NONE',  ( 10.06000000000000050, 2.055000000000001492, 0.000000000000000000 ) ) ;
#51000 = DIRECTION ( 'NONE',  ( -0.7071067811865486830, -0.7071067811865464625, 0.000000000000000000 ) ) ;
#51001 = ORIENTED_EDGE ( 'NONE', *, *, #123643, .F. ) ;
#51002 = PLANE ( 'NONE',  #37254 ) ;
#51003 = LINE ( 'NONE', #80959, #283 ) ;
#51004 = CARTESIAN_POINT ( 'NONE',  ( 34.49999999999976552, 6.277155672890305738, -3.510561720659021834 ) ) ;
#51005 = VECTOR ( 'NONE', #117283, 1000.000000000000000 ) ;
#51006 = CARTESIAN_POINT ( 'NONE',  ( -6.792893218813411238, 6.759292476615643253, 5.000000000000000000 ) ) ;
#51007 = CARTESIAN_POINT ( 'NONE',  ( 46.57876352523145158, -7.482591942790327058E-16, 6.109999999999999432 ) ) ;
#51008 = DIRECTION ( 'NONE',  ( 1.000000000000000000, 0.000000000000000000, 0.000000000000000000 ) ) ;
#51009 = EDGE_LOOP ( 'NONE', ( #84841, #3914, #127666, #42772 ) ) ;
#51010 = CARTESIAN_POINT ( 'NONE',  ( -8.483345613589495571, 22.22500000000000142, 4.500000000000000888 ) ) ;
#51011 = VECTOR ( 'NONE', #88568, 1000.000000000000227 ) ;
#51012 = EDGE_LOOP ( 'NONE', ( #119660, #100823, #14705, #78898 ) ) ;
#51013 = AXIS2_PLACEMENT_3D ( 'NONE', #59771, #48889, #69217 ) ;
#51014 = ORIENTED_EDGE ( 'NONE', *, *, #17406, .F. ) ;
#51015 = LINE ( 'NONE', #6730, #40816 ) ;
#51016 = VECTOR ( 'NONE', #59920, 999.9999999999998863 ) ;
#51017 = DIRECTION ( 'NONE',  ( 0.6830127018922180770, -0.6830127018922204085, -0.2588190451025213501 ) ) ;
#51018 = DIRECTION ( 'NONE',  ( -1.000000000000000000, -0.000000000000000000, -0.000000000000000000 ) ) ;
#51019 = PLANE ( 'NONE',  #92608 ) ;
#51020 = CARTESIAN_POINT ( 'NONE',  ( 82.08333333333334281, 6.884901960086290629, -3.974999999999994316 ) ) ;
#51021 = CARTESIAN_POINT ( 'NONE',  ( -18.48921356237309510, -27.52281430457068367, 5.000000000000000000 ) ) ;
#51022 = VECTOR ( 'NONE', #49767, 999.9999999999998863 ) ;
#51023 = ORIENTED_EDGE ( 'NONE', *, *, #130953, .T. ) ;
#51024 = CARTESIAN_POINT ( 'NONE',  ( 1.942999468602176316, 2.238834683357417088, -5.749481961982899847 ) ) ;
#51025 = DIRECTION ( 'NONE',  ( -0.7071067811865486830, 0.7071067811865464625, 0.000000000000000000 ) ) ;
#51026 = CARTESIAN_POINT ( 'NONE',  ( -31.49999999999977973, -5.947814304570768762, 5.000000000000000000 ) ) ;
#51027 = SURFACE_SIDE_STYLE ('',( #6746 ) ) ;
#51028 = CARTESIAN_POINT ( 'NONE',  ( -39.48921356237310221, -27.52281430457082934, 5.000000000000000000 ) ) ;
#51029 = CARTESIAN_POINT ( 'NONE',  ( -9.299744871391588674, -27.71228299555212971, 4.000000000000000000 ) ) ;
#51030 = CARTESIAN_POINT ( 'NONE',  ( 67.74586038379622721, 3.974999999999996980, 6.884901960086287964 ) ) ;
#51031 = EDGE_CURVE ( 'NONE', #117931, #80430, #140868, .T. ) ;
#51032 = CARTESIAN_POINT ( 'NONE',  ( 20.19999999999999929, 9.521314400968980422E-16, 0.000000000000000000 ) ) ;
#51033 = AXIS2_PLACEMENT_3D ( 'NONE', #12564, #122759, #56843 ) ;
#51034 = EDGE_LOOP ( 'NONE', ( #79628, #35593, #135413, #141568 ) ) ;
#51035 = VERTEX_POINT ( 'NONE', #142340 ) ;
#51036 = CARTESIAN_POINT ( 'NONE',  ( 53.64583333333332860, 2.130196079827431976, -7.949999999999999289 ) ) ;
#51037 = FACE_OUTER_BOUND ( 'NONE', #132874, .T. ) ;
#51038 = ADVANCED_FACE ( 'NONE', ( #96631 ), #41568, .F. ) ;
#51039 = DIRECTION ( 'NONE',  ( -0.7071067811865486830, -0.7071067811865464625, 0.000000000000000000 ) ) ;
#51040 = EDGE_CURVE ( 'NONE', #37517, #109570, #65514, .T. ) ;
#51041 = VECTOR ( 'NONE', #137700, 1000.000000000000000 ) ;
#51042 = DIRECTION ( 'NONE',  ( 0.6830127018922180770, -0.6830127018922204085, -0.2588190451025213501 ) ) ;
#51043 = ORIENTED_EDGE ( 'NONE', *, *, #132076, .T. ) ;
#51044 = EDGE_CURVE ( 'NONE', #140231, #31707, #131456, .T. ) ;
#51045 = CARTESIAN_POINT ( 'NONE',  ( -3.328169399223505742, -15.74070752338412049, 4.000000000000000000 ) ) ;
#51046 = CARTESIAN_POINT ( 'NONE',  ( 53.37543019189811133, -5.291415217122920289, -3.055000000000001492 ) ) ;
#51047 = ORIENTED_EDGE ( 'NONE', *, *, #8711, .F. ) ;
#51048 = LINE ( 'NONE', #50335, #64157 ) ;
#51049 = ORIENTED_EDGE ( 'NONE', *, *, #53665, .T. ) ;
#51050 = VERTEX_POINT ( 'NONE', #53917 ) ;
#51051 = AXIS2_PLACEMENT_3D ( 'NONE', #65972, #78256, #45639 ) ;
#51052 = CARTESIAN_POINT ( 'NONE',  ( 181.1500000000000057, -43.14999999999999147, 31.92499999999998295 ) ) ;
#51053 = CARTESIAN_POINT ( 'NONE',  ( -7.140000000000001457, -60.26999999999998892, -11.72188031596275337 ) ) ;
#51054 = LINE ( 'NONE', #106836, #46692 ) ;
#51055 = EDGE_CURVE ( 'NONE', #39646, #40495, #64768, .T. ) ;
#51056 = DIRECTION ( 'NONE',  ( 0.000000000000000000, -1.000000000000000000, 0.000000000000000000 ) ) ;
#51057 = EDGE_CURVE ( 'NONE', #7970, #10035, #34682, .T. ) ;
#51058 = DIRECTION ( 'NONE',  ( -0.7071067811865486830, -0.7071067811865464625, 0.000000000000000000 ) ) ;
#51060 = ORIENTED_EDGE ( 'NONE', *, *, #52756, .T. ) ;
#51059 = CARTESIAN_POINT ( 'NONE',  ( 99.97502705046289861, -5.819803920172573086, 5.819803920172573086 ) ) ;
#51061 = DIRECTION ( 'NONE',  ( -0.000000000000000000, 0.3543493200069153248, 0.9351131265310292928 ) ) ;
#51062 = CARTESIAN_POINT ( 'NONE',  ( -12.32816939922344623, 11.25929247661559884, 4.000000000000000000 ) ) ;
#51063 = CARTESIAN_POINT ( 'NONE',  ( -12.32816939922343913, 17.25929247661554200, 4.000000000000000000 ) ) ;
#51064 = DIRECTION ( 'NONE',  ( 0.7071067811865486830, -0.7071067811865464625, -0.000000000000000000 ) ) ;
#51065 = DIRECTION ( 'NONE',  ( 0.7071067811865487940, 0.7071067811865463515, 0.000000000000000000 ) ) ;
#51066 = AXIS2_PLACEMENT_3D ( 'NONE', #63827, #42077, #108699 ) ;
#51068 = ADVANCED_FACE ( 'NONE', ( #9639 ), #21253, .F. ) ;
#51067 =( BOUNDED_CURVE ( )  B_SPLINE_CURVE ( 2, ( #33028, #11189, #55470, #99655, #122122, #328, #88818, #133048, #22776, #67056, #69199, #138737, #91649 ),
 .UNSPECIFIED., .F., .T. ) 
 B_SPLINE_CURVE_WITH_KNOTS ( ( 3, 2, 2, 2, 2, 2, 3 ),
 ( 0.9166666666666666297, 0.9194444444444443976, 0.9222222222222222765, 0.9250000000000000444, 0.9277777777777778123, 0.9305555555555555802, 0.9333333333333333481 ),
 .UNSPECIFIED. ) 
 CURVE ( )  GEOMETRIC_REPRESENTATION_ITEM ( )  RATIONAL_B_SPLINE_CURVE ( ( 1.000000000000000000, 0.9659258262890683122, 1.000000000000000000, 0.9659258262890683122, 1.000000000000000000, 0.9659258262890683122, 1.000000000000000000, 0.9659258262890683122, 1.000000000000000000, 0.9659258262890683122, 1.000000000000000000, 0.9659258262890683122, 1.000000000000000000 ) ) 
 REPRESENTATION_ITEM ( '' )  );
#51069 = ORIENTED_EDGE ( 'NONE', *, *, #87193, .T. ) ;
#51070 = ORIENTED_EDGE ( 'NONE', *, *, #113244, .F. ) ;
#51071 = CARTESIAN_POINT ( 'NONE',  ( 89.03752705046288440, -9.735942053221456900E-16, 7.949999999999998401 ) ) ;
#51072 = CARTESIAN_POINT ( 'NONE',  ( 76.03709685856478018, -3.054999999999998828, -5.291415217122919401 ) ) ;
#51073 = LINE ( 'NONE', #72144, #139035 ) ;
#51074 = CARTESIAN_POINT ( 'NONE',  ( 6.618384906019920244, -2.240707523384264377, 13.37739548510237952 ) ) ;
#51075 = CARTESIAN_POINT ( 'NONE',  ( 73.28752705046288440, 0.000000000000000000, -7.949999999999998401 ) ) ;
#51076 = EDGE_LOOP ( 'NONE', ( #1321, #40973, #15121, #131205 ) ) ;
#51078 = EDGE_CURVE ( 'NONE', #37121, #32625, #30728, .T. ) ;
#51077 = ORIENTED_EDGE ( 'NONE', *, *, #78197, .F. ) ;
#51079 = CARTESIAN_POINT ( 'NONE',  ( 30.18398860626900060, 28.73617430169808173, 5.000000000000000000 ) ) ;
#51081 = VECTOR ( 'NONE', #57621, 999.9999999999998863 ) ;
#51080 =( NAMED_UNIT ( * ) SI_UNIT ( $, .STERADIAN. ) SOLID_ANGLE_UNIT ( ) );
#51082 = ORIENTED_EDGE ( 'NONE', *, *, #54596, .F. ) ;
#51083 = VECTOR ( 'NONE', #73064, 1000.000000000000227 ) ;
#51085 = ORIENTED_EDGE ( 'NONE', *, *, #49978, .T. ) ;
#51084 = VECTOR ( 'NONE', #40220, 1000.000000000000000 ) ;
#51086 = CARTESIAN_POINT ( 'NONE',  ( 5.999999999999956479, -0.2811185226894233335, -5.995736974527527074 ) ) ;
#51087 = ORIENTED_EDGE ( 'NONE', *, *, #45197, .F. ) ;
#51088 = DIRECTION ( 'NONE',  ( 0.000000000000000000, 0.000000000000000000, 1.000000000000000000 ) ) ;
#51089 = EDGE_CURVE ( 'NONE', #132586, #24733, #8884, .T. ) ;
#51090 = VECTOR ( 'NONE', #88614, 1000.000000000000000 ) ;
#51091 = AXIS2_PLACEMENT_3D ( 'NONE', #43336, #141956, #75958 ) ;
#51092 = AXIS2_PLACEMENT_3D ( 'NONE', #59225, #70111, #91797 ) ;
#51093 = AXIS2_PLACEMENT_3D ( 'NONE', #117974, #121398, #7808 ) ;
#51094 = VECTOR ( 'NONE', #73601, 1000.000000000000227 ) ;
#51095 = FACE_BOUND ( 'NONE', #92668, .T. ) ;
#51096 = CARTESIAN_POINT ( 'NONE',  ( -34.92500000000001137, 11.81665438641030441, 4.500000000000000888 ) ) ;
#51097 = DIRECTION ( 'NONE',  ( 0.000000000000000000, -1.000000000000000000, 0.000000000000000000 ) ) ;
#51099 = LINE ( 'NONE', #32189, #17849 ) ;
#51098 = AXIS2_PLACEMENT_3D ( 'NONE', #50847, #28389, #40691 ) ;
#51101 = ORIENTED_EDGE ( 'NONE', *, *, #33672, .F. ) ;
#51100 = LINE ( 'NONE', #117729, #18033 ) ;
#51102 = DIRECTION ( 'NONE',  ( 0.7071067811865487940, 0.7071067811865463515, 0.000000000000000000 ) ) ;
#51104 = ADVANCED_FACE ( 'NONE', ( #109691 ), #10359, .F. ) ;
#51103 = CONTEXT_DEPENDENT_SHAPE_REPRESENTATION ( #87431, #109553 ) ;
#51105 = ORIENTED_EDGE ( 'NONE', *, *, #7766, .T. ) ;
#51106 = VERTEX_POINT ( 'NONE', #143035 ) ;
#51107 = CARTESIAN_POINT ( 'NONE',  ( 84.78709685856478018, 3.054999999999997495, 5.291415217122919401 ) ) ;
#51108 = ORIENTED_EDGE ( 'NONE', *, *, #127353, .F. ) ;
#51109 = DIRECTION ( 'NONE',  ( 0.7071067811865487940, 0.7071067811865463515, 0.000000000000000000 ) ) ;
#51110 = AXIS2_PLACEMENT_3D ( 'NONE', #114284, #27261, #4750 ) ;
#51111 = CARTESIAN_POINT ( 'NONE',  ( 11.99451991528749417, 28.92564299267946382, 4.000000000000000000 ) ) ;
#51112 = CARTESIAN_POINT ( 'NONE',  ( -34.92500000000001137, -0.8020632299005174826, 13.72581505463524998 ) ) ;
#51113 = ORIENTED_EDGE ( 'NONE', *, *, #49876, .T. ) ;
#51114 = DIRECTION ( 'NONE',  ( -1.000000000000000000, 0.000000000000000000, 0.000000000000000000 ) ) ;
#51115 = VECTOR ( 'NONE', #31319, 1000.000000000000000 ) ;
#51116 = CARTESIAN_POINT ( 'NONE',  ( -34.92499999999999005, -3.270000000000012896, -40.00000000000000000 ) ) ;
#51117 = ADVANCED_FACE ( 'NONE', ( #76360 ), #43721, .T. ) ;
#51118 = CARTESIAN_POINT ( 'NONE',  ( -54.48921356237310221, -27.52281430457093236, 5.000000000000000000 ) ) ;
#51119 = CARTESIAN_POINT ( 'NONE',  ( -57.18398860626899705, 28.73617430169827358, 5.000000000000000000 ) ) ;
#51120 = VECTOR ( 'NONE', #31252, 1000.000000000000000 ) ;
#51121 = FACE_OUTER_BOUND ( 'NONE', #50084, .T. ) ;
#51122 = CARTESIAN_POINT ( 'NONE',  ( -28.49999999999979750, -10.91253812416064406, 4.000000000000000000 ) ) ;
#51123 = EDGE_LOOP ( 'NONE', ( #62159, #67963, #11137, #27951 ) ) ;
#51124 = CONICAL_SURFACE ( 'NONE', #20978, 2.055000000000001048, 0.9599310885968758145 ) ;
#51125 = CARTESIAN_POINT ( 'NONE',  ( 12.48921356237309155, -27.52281430457064104, 5.000000000000000000 ) ) ;
#51126 = LINE ( 'NONE', #73584, #111375 ) ;
#51127 = ORIENTED_EDGE ( 'NONE', *, *, #83440, .F. ) ;
#51128 = ORIENTED_EDGE ( 'NONE', *, *, #20363, .T. ) ;
#51129 = EDGE_CURVE ( 'NONE', #138233, #1245, #97355, .T. ) ;
#51130 = VECTOR ( 'NONE', #130890, 999.9999999999998863 ) ;
#51131 = EDGE_LOOP ( 'NONE', ( #74335, #110843, #56307, #100635 ) ) ;
#51132 = CARTESIAN_POINT ( 'NONE',  ( 43.45876352523143993, 0.000000000000000000, -6.110000000000001208 ) ) ;
#51133 = VERTEX_POINT ( 'NONE', #18358 ) ;
#51134 = CARTESIAN_POINT ( 'NONE',  ( 18.27497294953710494, 4.461849672132300881, 4.461849672132299105 ) ) ;
#51135 = CARTESIAN_POINT ( 'NONE',  ( -14.91938099157687958, 4.277364139441302449, -29.65621814313812976 ) ) ;
#51136 = ORIENTED_EDGE ( 'NONE', *, *, #38949, .F. ) ;
#51137 = DIRECTION ( 'NONE',  ( 0.6830127018922180770, -0.6830127018922204085, -0.2588190451025213501 ) ) ;
#51138 = ORIENTED_EDGE ( 'NONE', *, *, #60669, .F. ) ;
#51139 = CARTESIAN_POINT ( 'NONE',  ( 18.77004279457781166, 21.73644205237998506, 5.000000000000000888 ) ) ;
#51140 = AXIS2_PLACEMENT_3D ( 'NONE', #66032, #76174, #44276 ) ;
#51141 = LINE ( 'NONE', #71460, #133104 ) ;
#51143 = ORIENTED_EDGE ( 'NONE', *, *, #33549, .T. ) ;
#51142 = DIRECTION ( 'NONE',  ( 0.7071067811865486830, -0.7071067811865464625, -0.000000000000000000 ) ) ;
#51144 = ORIENTED_EDGE ( 'NONE', *, *, #37929, .T. ) ;
#51145 = CYLINDRICAL_SURFACE ( 'NONE', #14431, 2.500000000000000000 ) ;
#51146 = VERTEX_POINT ( 'NONE', #140188 ) ;
#51147 = CARTESIAN_POINT ( 'NONE',  ( 11.99451991528749417, 28.92564299267946382, 4.000000000000000000 ) ) ;
#51148 = EDGE_LOOP ( 'NONE', ( #36599, #9270, #121779, #113828 ) ) ;
#51150 = ORIENTED_EDGE ( 'NONE', *, *, #30909, .T. ) ;
#51149 = EDGE_CURVE ( 'NONE', #89715, #87848, #40875, .T. ) ;
#51151 = ORIENTED_EDGE ( 'NONE', *, *, #87211, .T. ) ;
#51152 = VERTEX_POINT ( 'NONE', #62634 ) ;
#51153 = CARTESIAN_POINT ( 'NONE',  ( 24.39999999999999858, -2.600000000000055600, -28.92500000000001492 ) ) ;
#51154 = VECTOR ( 'NONE', #16525, 1000.000000000000000 ) ;
#51155 = FACE_OUTER_BOUND ( 'NONE', #122490, .T. ) ;
#51157 = EDGE_CURVE ( 'NONE', #59760, #81280, #7503, .T. ) ;
#51156 = DIRECTION ( 'NONE',  ( -0.7071067811865486830, -0.7071067811865464625, 0.000000000000000000 ) ) ;
#51158 = CARTESIAN_POINT ( 'NONE',  ( -28.49999999999980460, -16.91253812416058366, 4.000000000000000000 ) ) ;
#51159 = ORIENTED_EDGE ( 'NONE', *, *, #80067, .T. ) ;
#51160 = EDGE_CURVE ( 'NONE', #110495, #92174, #51763, .T. ) ;
#51161 = CARTESIAN_POINT ( 'NONE',  ( 38.99451991528749062, 28.92564299267965211, 4.000000000000000000 ) ) ;
#51162 = ORIENTED_EDGE ( 'NONE', *, *, #85604, .T. ) ;
#51163 = AXIS2_PLACEMENT_3D ( 'NONE', #68197, #76914, #100775 ) ;
#51164 = DIRECTION ( 'NONE',  ( -0.7071067811865487940, 0.7071067811865463515, -0.000000000000000000 ) ) ;
#51165 = FACE_OUTER_BOUND ( 'NONE', #35475, .T. ) ;
#51166 = CARTESIAN_POINT ( 'NONE',  ( 4.499999999999968914, -4.216083040037243101, -7.486842126848666901 ) ) ;
#51167 = VERTEX_POINT ( 'NONE', #107542 ) ;
#51168 = DIRECTION ( 'NONE',  ( 1.000000000000000000, 0.000000000000000000, 0.000000000000000000 ) ) ;
#51169 = DIRECTION ( 'NONE',  ( 0.6830127018922180770, -0.6830127018922204085, -0.2588190451025213501 ) ) ;
#51170 = ORIENTED_EDGE ( 'NONE', *, *, #122326, .F. ) ;
#51171 = ORIENTED_EDGE ( 'NONE', *, *, #65291, .F. ) ;
#51172 = ORIENTED_EDGE ( 'NONE', *, *, #90182, .F. ) ;
#51173 = CARTESIAN_POINT ( 'NONE',  ( 3.489213562373097322, -27.52281430457057709, 5.000000000000000000 ) ) ;
#51174 = DIRECTION ( 'NONE',  ( 0.7071067811865486830, -0.7071067811865464625, -0.000000000000000000 ) ) ;
#51175 = DIRECTION ( 'NONE',  ( 0.000000000000000000, -1.000000000000000000, 0.000000000000000000 ) ) ;
#51176 = VECTOR ( 'NONE', #133358, 999.9999999999998863 ) ;
#51177 = CARTESIAN_POINT ( 'NONE',  ( 2.999999998680793478, -47.86718710719738112, -37.19897551713944495 ) ) ;
#51178 = CARTESIAN_POINT ( 'NONE',  ( 72.68293019189810877, -1.637169565754159173, -6.109999999999999432 ) ) ;
#51179 = EDGE_CURVE ( 'NONE', #90251, #9331, #113405, .T. ) ;
#51180 = CARTESIAN_POINT ( 'NONE',  ( 23.29289321881329755, 17.25929247661554911, 5.000000000000000000 ) ) ;
#51181 = AXIS2_PLACEMENT_3D ( 'NONE', #39544, #28667, #130111 ) ;
#51182 = VECTOR ( 'NONE', #114006, 1000.000000000000000 ) ;
#51183 = DIRECTION ( 'NONE',  ( -0.000000000000000000, 0.3543493200069153248, 0.9351131265310292928 ) ) ;
#51184 = CARTESIAN_POINT ( 'NONE',  ( -29.99999999999979039, 7.588810512006185505, -3.013526669885157716 ) ) ;
#51185 = CARTESIAN_POINT ( 'NONE',  ( 9.208651418775088970, 4.584330080086930965E-16, 0.000000000000000000 ) ) ;
#51186 = CARTESIAN_POINT ( 'NONE',  ( -55.65468426143998215, -60.26999999999998892, 25.00000000000000000 ) ) ;
#51187 = ORIENTED_EDGE ( 'NONE', *, *, #88492, .F. ) ;
#51188 = AXIS2_PLACEMENT_3D ( 'NONE', #49579, #114083, #38672 ) ;
#51189 = VECTOR ( 'NONE', #87915, 999.9999999999998863 ) ;
#51190 = AXIS2_PLACEMENT_3D ( 'NONE', #38515, #126921, #6538 ) ;
#51192 = FACE_OUTER_BOUND ( 'NONE', #29600, .T. ) ;
#51191 = AXIS2_PLACEMENT_3D ( 'NONE', #47880, #92044, #5000 ) ;
#51193 = EDGE_LOOP ( 'NONE', ( #127031, #111196, #55186, #20035 ) ) ;
#51194 = AXIS2_PLACEMENT_3D ( 'NONE', #107471, #8134, #52373 ) ;
#51195 = LINE ( 'NONE', #51913, #122395 ) ;
#51197 = ORIENTED_EDGE ( 'NONE', *, *, #125327, .T. ) ;
#51196 = DIRECTION ( 'NONE',  ( 0.3543493200069162685, -0.000000000000000000, -0.9351131265310288487 ) ) ;
#51198 = CARTESIAN_POINT ( 'NONE',  ( 20.99999999999985079, 7.007997736742463957, -8.085015511992065029 ) ) ;
#51199 = FACE_OUTER_BOUND ( 'NONE', #81914, .T. ) ;
#51200 = EDGE_LOOP ( 'NONE', ( #98466, #52991, #68428 ) ) ;
#51201 = ORIENTED_EDGE ( 'NONE', *, *, #27513, .T. ) ;
#51202 = DIRECTION ( 'NONE',  ( 1.000000000000000000, -0.000000000000000000, 0.000000000000000000 ) ) ;
#51203 = DIRECTION ( 'NONE',  ( 0.3543493200069162685, -0.000000000000000000, -0.9351131265310288487 ) ) ;
#51204 = VECTOR ( 'NONE', #75141, 999.9999999999998863 ) ;
#51205 = LINE ( 'NONE', #75117, #114705 ) ;
#51206 = CARTESIAN_POINT ( 'NONE',  ( 97.64169371712954160, -2.130196079827424871, -7.949999999999999289 ) ) ;
#51207 = LINE ( 'NONE', #30891, #99488 ) ;
#51208 = EDGE_CURVE ( 'NONE', #37388, #100143, #121972, .T. ) ;
#51209 = CARTESIAN_POINT ( 'NONE',  ( 7.828169399223469327, -17.24070752338410628, 4.000000000000000000 ) ) ;
#51210 = ORIENTED_EDGE ( 'NONE', *, *, #103694, .T. ) ;
#51211 = CARTESIAN_POINT ( 'NONE',  ( -8.207106781186482181, -17.24070752338409918, 5.000000000000000000 ) ) ;
#51212 = ADVANCED_FACE ( 'NONE', ( #2321 ), #1607, .F. ) ;
#51213 = CARTESIAN_POINT ( 'NONE',  ( -45.29974487139158867, -27.71228299555237840, 4.000000000000000000 ) ) ;
#51214 = CARTESIAN_POINT ( 'NONE',  ( 31.06250000000000000, 4.461849672132300881, 4.461849672132299105 ) ) ;
#51215 = VECTOR ( 'NONE', #30510, 1000.000000000000000 ) ;
#51216 = FACE_OUTER_BOUND ( 'NONE', #43809, .T. ) ;
#51217 = ORIENTED_EDGE ( 'NONE', *, *, #96986, .T. ) ;
#51218 = EDGE_CURVE ( 'NONE', #85852, #121024, #101830, .T. ) ;
#51219 = EDGE_CURVE ( 'NONE', #113826, #139855, #46640, .T. ) ;
#51220 =( GEOMETRIC_REPRESENTATION_CONTEXT ( 3 ) GLOBAL_UNCERTAINTY_ASSIGNED_CONTEXT ( ( #54778 ) ) GLOBAL_UNIT_ASSIGNED_CONTEXT ( ( #16091, #38608, #82143 ) ) REPRESENTATION_CONTEXT ( 'NONE', 'WORKASPACE' ) );
#51221 = LINE ( 'NONE', #16401, #441 ) ;
#51222 = ORIENTED_EDGE ( 'NONE', *, *, #25782, .T. ) ;
#51223 = VECTOR ( 'NONE', #10378, 1000.000000000000227 ) ;
#51224 = CARTESIAN_POINT ( 'NONE',  ( 87.50043019189810423, -3.055000000000002380, 5.291415217122920289 ) ) ;
#51225 = VECTOR ( 'NONE', #86067, 999.9999999999998863 ) ;
#51226 = DIRECTION ( 'NONE',  ( 1.000000000000000000, 0.000000000000000000, 0.000000000000000000 ) ) ;
#51227 = CARTESIAN_POINT ( 'NONE',  ( 4.499999999999966249, 9.431123077392086884, 4.000000000000000000 ) ) ;
#51228 = CARTESIAN_POINT ( 'NONE',  ( 6.183988606268994381, 28.73617430169791476, 5.000000000000000000 ) ) ;
#51229 = ORIENTED_EDGE ( 'NONE', *, *, #22626, .T. ) ;
#51230 = VECTOR ( 'NONE', #111052, 999.9999999999998863 ) ;
#51231 = CARTESIAN_POINT ( 'NONE',  ( 25.63753812416080180, 22.22500000000000142, 4.000000000000000000 ) ) ;
#51232 = CARTESIAN_POINT ( 'NONE',  ( -39.18398860626899705, 28.73617430169814568, 5.000000000000000000 ) ) ;
#51233 = EDGE_CURVE ( 'NONE', #115565, #52479, #85561, .T. ) ;
#51234 = DIRECTION ( 'NONE',  ( -1.000000000000000000, -0.000000000000000000, -0.000000000000000000 ) ) ;
#51235 = VECTOR ( 'NONE', #112506, 1000.000000000000000 ) ;
#51236 = EDGE_CURVE ( 'NONE', #4967, #68187, #33710, .T. ) ;
#51238 = ORIENTED_EDGE ( 'NONE', *, *, #82807, .F. ) ;
#51237 = CARTESIAN_POINT ( 'NONE',  ( 18.48921356237309510, -27.52281430457068367, 5.000000000000000000 ) ) ;
#51239 = LINE ( 'NONE', #49104, #83099 ) ;
#51240 = LINE ( 'NONE', #128777, #89288 ) ;
#51241 = CARTESIAN_POINT ( 'NONE',  ( 17.18753812416040461, -22.22500000000000142, 4.000000000000000000 ) ) ;
#51242 = DIRECTION ( 'NONE',  ( -0.000000000000000000, -0.3543493200069152693, 0.9351131265310292928 ) ) ;
#51243 = ORIENTED_EDGE ( 'NONE', *, *, #21463, .T. ) ;
#51244 = ORIENTED_EDGE ( 'NONE', *, *, #123501, .F. ) ;
#51245 = CARTESIAN_POINT ( 'NONE',  ( 71.60459685856477563, 1.637169565754164946, -6.109999999999999432 ) ) ;
#51246 = VECTOR ( 'NONE', #117199, 999.9999999999998863 ) ;
#51247 = VERTEX_POINT ( 'NONE', #907 ) ;
#51248 = EDGE_CURVE ( 'NONE', #48427, #76949, #135055, .T. ) ;
#51249 = AXIS2_PLACEMENT_3D ( 'NONE', #42510, #88136, #64237 ) ;
#51250 = CARTESIAN_POINT ( 'NONE',  ( 72.29974487139158157, -27.71228299555256669, 4.000000000000000000 ) ) ;
#51251 = FACE_OUTER_BOUND ( 'NONE', #95597, .T. ) ;
#51252 = EDGE_LOOP ( 'NONE', ( #23498, #68962, #47622, #77817 ) ) ;
#51253 = EDGE_CURVE ( 'NONE', #15605, #128738, #90065, .T. ) ;
#51254 = VECTOR ( 'NONE', #128204, 1000.000000000000000 ) ;
#51255 = CARTESIAN_POINT ( 'NONE',  ( 0.000000000000000000, 60.00000000000000000, -4.000000000000000000 ) ) ;
#51256 = DIRECTION ( 'NONE',  ( 0.5735764363510444941, 0.8191520442889929088, 0.000000000000000000 ) ) ;
#51257 = ORIENTED_EDGE ( 'NONE', *, *, #81474, .T. ) ;
#51258 = CARTESIAN_POINT ( 'NONE',  ( 17.11087965568911073, 8.820243421702873121, 4.000000000000000000 ) ) ;
#51259 = CARTESIAN_POINT ( 'NONE',  ( 34.35002705046289151, -5.819803920172573086, -5.819803920172573086 ) ) ;
#51260 = ADVANCED_FACE ( 'NONE', ( #13923 ), #89369, .F. ) ;
#51261 = CARTESIAN_POINT ( 'NONE',  ( 5.999999999999981348, 20.58746187583903620, 4.000000000000000000 ) ) ;
#51262 = AXIS2_PLACEMENT_3D ( 'NONE', #44230, #33377, #89151 ) ;
#51263 = VERTEX_POINT ( 'NONE', #99501 ) ;
#51264 = ORIENTED_EDGE ( 'NONE', *, *, #57602, .F. ) ;
#51265 = FACE_OUTER_BOUND ( 'NONE', #73750, .T. ) ;
#51266 = PLANE ( 'NONE',  #53120 ) ;
#51267 = EDGE_CURVE ( 'NONE', #3592, #270, #45190, .T. ) ;
#51268 = CARTESIAN_POINT ( 'NONE',  ( 65.99451991528749772, 28.92564299267984396, 4.000000000000000000 ) ) ;
#51269 = LINE ( 'NONE', #94731, #51295 ) ;
#51270 = ADVANCED_FACE ( 'NONE', ( #35016 ), #132179, .F. ) ;
#51271 = VECTOR ( 'NONE', #8025, 1000.000000000000000 ) ;
#51272 = DIRECTION ( 'NONE',  ( 1.000000000000000000, 0.000000000000000000, 0.000000000000000000 ) ) ;
#51273 = DIRECTION ( 'NONE',  ( 0.7071067811865487940, 0.7071067811865463515, 0.000000000000000000 ) ) ;
#51275 = EDGE_CURVE ( 'NONE', #109227, #56761, #111847, .T. ) ;
#51274 =( NAMED_UNIT ( * ) PLANE_ANGLE_UNIT ( ) SI_UNIT ( $, .RADIAN. ) );
#51276 = ORIENTED_EDGE ( 'NONE', *, *, #143334, .T. ) ;
#51277 = VERTEX_POINT ( 'NONE', #122698 ) ;
#51278 = EDGE_LOOP ( 'NONE', ( #21058, #123138, #141952 ) ) ;
#51279 = VERTEX_POINT ( 'NONE', #78499 ) ;
#51281 = EDGE_CURVE ( 'NONE', #17061, #136777, #100949, .T. ) ;
#51280 = PRESENTATION_LAYER_ASSIGNMENT (  '', '', ( #32764 ) ) ;
#51282 =( BOUNDED_CURVE ( )  B_SPLINE_CURVE ( 3, ( #85220, #140333, #84544, #7657 ),
 .UNSPECIFIED., .F., .F. ) 
 B_SPLINE_CURVE_WITH_KNOTS ( ( 4, 4 ),
 ( 2.779374508378134045, 4.199602562396879790 ),
 .UNSPECIFIED. ) 
 CURVE ( )  GEOMETRIC_REPRESENTATION_ITEM ( )  RATIONAL_B_SPLINE_CURVE ( ( 1.000000000000000000, 0.8388583629366537231, 0.8388583629366537231, 1.000000000000000000 ) ) 
 REPRESENTATION_ITEM ( '' )  );
#51283 = AXIS2_PLACEMENT_3D ( 'NONE', #129506, #9878, #98338 ) ;
#51284 = LINE ( 'NONE', #128820, #52046 ) ;
#51285 = ORIENTED_EDGE ( 'NONE', *, *, #635, .T. ) ;
#51286 = CARTESIAN_POINT ( 'NONE',  ( 9.183988606268997046, 28.73617430169793607, 5.000000000000000000 ) ) ;
#51287 = CARTESIAN_POINT ( 'NONE',  ( 25.49999999999982947, -9.462702396500981550, -9.474982329943568260 ) ) ;
#51288 = CARTESIAN_POINT ( 'NONE',  ( 1.320799999999990870, 1.617513492313812843E-16, 9.407735506486140764 ) ) ;
#51289 = FACE_OUTER_BOUND ( 'NONE', #89440, .T. ) ;
#51290 = VECTOR ( 'NONE', #22421, 1000.000000000000000 ) ;
#51291 = AXIS2_PLACEMENT_3D ( 'NONE', #46984, #135389, #4785 ) ;
#51292 = AXIS2_PLACEMENT_3D ( 'NONE', #70989, #42650, #84698 ) ;
#51293 = DIRECTION ( 'NONE',  ( 4.681814790819592407E-17, 0.3543493200069153248, 0.9351131265310292928 ) ) ;
#51294 = ORIENTED_EDGE ( 'NONE', *, *, #67568, .T. ) ;
#51295 = VECTOR ( 'NONE', #72344, 1000.000000000000000 ) ;
#51296 = CARTESIAN_POINT ( 'NONE',  ( -3.489213562373097322, -27.52281430457057709, 5.000000000000000000 ) ) ;
#51297 = EDGE_LOOP ( 'NONE', ( #79096, #27052, #84270, #82712 ) ) ;
#51298 = CARTESIAN_POINT ( 'NONE',  ( 78.29974487139158157, -27.71228299555260577, 4.000000000000000000 ) ) ;
#51299 = ORIENTED_EDGE ( 'NONE', *, *, #35551, .F. ) ;
#51300 = CARTESIAN_POINT ( 'NONE',  ( 13.46247294953710494, -7.464222240803106570E-16, -6.094999999999989981 ) ) ;
#51301 = ORIENTED_EDGE ( 'NONE', *, *, #63681, .F. ) ;
#51302 = AXIS2_PLACEMENT_3D ( 'NONE', #11795, #98813, #143047 ) ;
#51303 = CARTESIAN_POINT ( 'NONE',  ( 73.20876352523143282, -7.482591942790329030E-16, 6.110000000000001208 ) ) ;
#51304 = VERTEX_POINT ( 'NONE', #33591 ) ;
#51305 = PLANE ( 'NONE',  #34987 ) ;
#51306 = CARTESIAN_POINT ( 'NONE',  ( 63.18398860626900415, 28.73617430169831621, 5.000000000000000000 ) ) ;
#51307 = CARTESIAN_POINT ( 'NONE',  ( 108.9379301918980758, -6.110000000000001208, 1.637169565754158951 ) ) ;
#51308 = PLANE ( 'NONE',  #7763 ) ;
#51309 = CIRCLE ( 'NONE', #132367, 4.750000000000000000 ) ;
#51310 = LINE ( 'NONE', #63635, #37104 ) ;
#51311 = DIRECTION ( 'NONE',  ( -0.6830127018922181881, 0.6830127018922202975, -0.2588190451025214056 ) ) ;
#51312 = LINE ( 'NONE', #7770, #130376 ) ;
#51313 = PRESENTATION_STYLE_ASSIGNMENT (( #114411 ) ) ;
#51314 = VECTOR ( 'NONE', #131870, 999.9999999999998863 ) ;
#51315 = DIRECTION ( 'NONE',  ( 0.3543493200069162685, -0.000000000000000000, -0.9351131265310288487 ) ) ;
#51316 = ORIENTED_EDGE ( 'NONE', *, *, #122558, .F. ) ;
#51317 = VECTOR ( 'NONE', #38235, 1000.000000000000000 ) ;
#51318 = CARTESIAN_POINT ( 'NONE',  ( -51.29974487139158867, -27.71228299555242103, 4.000000000000000000 ) ) ;
#51319 = LINE ( 'NONE', #117241, #35934 ) ;
#51320 = ORIENTED_EDGE ( 'NONE', *, *, #21388, .T. ) ;
#51321 = VECTOR ( 'NONE', #92836, 999.9999999999998863 ) ;
#51322 = ORIENTED_EDGE ( 'NONE', *, *, #129421, .F. ) ;
#51323 = DIRECTION ( 'NONE',  ( -0.6830127018922180770, -0.6830127018922204085, -0.2588190451025213501 ) ) ;
#51324 = ORIENTED_EDGE ( 'NONE', *, *, #67832, .T. ) ;
#51325 = VECTOR ( 'NONE', #88294, 1000.000000000000000 ) ;
#51326 = CARTESIAN_POINT ( 'NONE',  ( -7.140000000000001457, 12.19802518668052471, 4.711086268963008195 ) ) ;
#51327 = LINE ( 'NONE', #129571, #31595 ) ;
#51328 = ADVANCED_FACE ( 'NONE', ( #22643 ), #77792, .T. ) ;
#51329 = LINE ( 'NONE', #83981, #120464 ) ;
#51330 = ORIENTED_EDGE ( 'NONE', *, *, #46123, .T. ) ;
#51331 = ADVANCED_FACE ( 'NONE', ( #23382 ), #67654, .T. ) ;
#51332 = FACE_OUTER_BOUND ( 'NONE', #138677, .T. ) ;
#51333 = ORIENTED_EDGE ( 'NONE', *, *, #10713, .F. ) ;
#51334 = AXIS2_PLACEMENT_3D ( 'NONE', #40252, #29329, #51828 ) ;
#51335 = CARTESIAN_POINT ( 'NONE',  ( 7.416236474768552078, -7.934999999999990727, 4.858786175617117713E-16 ) ) ;
#51336 = FACE_OUTER_BOUND ( 'NONE', #142766, .T. ) ;
#51337 = CARTESIAN_POINT ( 'NONE',  ( 0.000000000000000000, 0.000000000000000000, 5.000000000000000000 ) ) ;
#51338 = EDGE_CURVE ( 'NONE', #82669, #80263, #137169, .T. ) ;
#51339 = FACE_OUTER_BOUND ( 'NONE', #137728, .T. ) ;
#51340 = ORIENTED_EDGE ( 'NONE', *, *, #3658, .F. ) ;
#51341 = ORIENTED_EDGE ( 'NONE', *, *, #129731, .F. ) ;
#51342 = STYLED_ITEM ( 'NONE', ( #52988 ), #23446 ) ;
#51343 = ORIENTED_EDGE ( 'NONE', *, *, #134041, .F. ) ;
#51344 = CARTESIAN_POINT ( 'NONE',  ( 21.18398860626899349, 28.73617430169802134, 5.000000000000000000 ) ) ;
#51345 = LINE ( 'NONE', #20825, #111284 ) ;
#51346 = CARTESIAN_POINT ( 'NONE',  ( 6.005480084712508493, 28.92564299267933947, 4.000000000000000000 ) ) ;
#51347 = AXIS2_PLACEMENT_3D ( 'NONE', #107507, #64019, #140832 ) ;
#51348 = CARTESIAN_POINT ( 'NONE',  ( -45.29974487139158867, -27.71228299555237840, 4.000000000000000000 ) ) ;
#51349 = LINE ( 'NONE', #9200, #62175 ) ;
#51350 = DIRECTION ( 'NONE',  ( -1.000000000000000000, -0.000000000000000000, -0.000000000000000000 ) ) ;
#51351 = EDGE_CURVE ( 'NONE', #83817, #137730, #124850, .T. ) ;
#51352 = DIRECTION ( 'NONE',  ( -0.7071067811865486830, 0.7071067811865464625, 0.000000000000000000 ) ) ;
#51353 = DIRECTION ( 'NONE',  ( -0.7071067811865486830, 0.7071067811865464625, 0.000000000000000000 ) ) ;
#51355 = VECTOR ( 'NONE', #30249, 1000.000000000000000 ) ;
#51354 = CARTESIAN_POINT ( 'NONE',  ( 41.24999999999999289, -9.735942053221458872E-16, 7.950000000000000178 ) ) ;
#51356 = ORIENTED_EDGE ( 'NONE', *, *, #88197, .T. ) ;
#51357 = CARTESIAN_POINT ( 'NONE',  ( 74.35416666666667140, -2.130196079827425759, -7.950000000000000178 ) ) ;
#51358 = AXIS2_PLACEMENT_3D ( 'NONE', #127090, #7437, #51702 ) ;
#51359 = EDGE_CURVE ( 'NONE', #46464, #5794, #82794, .T. ) ;
#51360 = DIRECTION ( 'NONE',  ( 0.6830127018922180770, -0.6830127018922204085, -0.2588190451025213501 ) ) ;
#51361 = ORIENTED_EDGE ( 'NONE', *, *, #5307, .F. ) ;
#51362 = DIRECTION ( 'NONE',  ( -0.000000000000000000, -0.3543493200069152693, 0.9351131265310292928 ) ) ;
#51364 = ORIENTED_EDGE ( 'NONE', *, *, #113042, .F. ) ;
#51363 = DIRECTION ( 'NONE',  ( 0.3543493200069162685, -0.000000000000000000, -0.9351131265310288487 ) ) ;
#51365 = CARTESIAN_POINT ( 'NONE',  ( 0.4892135623730947680, -27.52281430457055578, 5.000000000000000000 ) ) ;
#51366 =( NAMED_UNIT ( * ) PLANE_ANGLE_UNIT ( ) SI_UNIT ( $, .RADIAN. ) );
#51367 = EDGE_CURVE ( 'NONE', #36267, #130911, #103784, .T. ) ;
#51369 = ORIENTED_EDGE ( 'NONE', *, *, #46481, .T. ) ;
#51368 = AXIS2_PLACEMENT_3D ( 'NONE', #133770, #58400, #22819 ) ;
#51370 = LINE ( 'NONE', #141963, #21157 ) ;
#51371 = ORIENTED_EDGE ( 'NONE', *, *, #121037, .F. ) ;
#51372 = CARTESIAN_POINT ( 'NONE',  ( 120.3916937171295700, 2.130196079827421762, 7.950000000000001066 ) ) ;
#51373 = CARTESIAN_POINT ( 'NONE',  ( 12.70710678118645731, -15.74070752338412049, 5.000000000000000000 ) ) ;
#51374 = DIRECTION ( 'NONE',  ( 0.6830127018922181881, 0.6830127018922202975, -0.2588190451025214056 ) ) ;
#51375 = CARTESIAN_POINT ( 'NONE',  ( 19.58200623001875940, -2.499999999999996447, 0.000000000000000000 ) ) ;
#51376 = EDGE_CURVE ( 'NONE', #121547, #17180, #5892, .T. ) ;
#51377 = CARTESIAN_POINT ( 'NONE',  ( 17.99999999999987210, -13.06887692260767686, 4.000000000000000000 ) ) ;
#51378 = CARTESIAN_POINT ( 'NONE',  ( 8.166666666666667851, -5.278424836066145431, -3.047499999999993658 ) ) ;
#51379 = CARTESIAN_POINT ( 'NONE',  ( 10.47873647476855119, -5.808823158059033709, 5.808823158059035485 ) ) ;
#51380 = VECTOR ( 'NONE', #114107, 1000.000000000000000 ) ;
#51381 = VECTOR ( 'NONE', #63976, 999.9999999999998863 ) ;
#51382 = CARTESIAN_POINT ( 'NONE',  ( -34.42500000000001137, 16.54139925780184583, 5.000000000000000000 ) ) ;
#51383 = DIRECTION ( 'NONE',  ( -0.000000000000000000, -0.3543493200069152693, 0.9351131265310292928 ) ) ;
#51384 = ORIENTED_EDGE ( 'NONE', *, *, #108419, .F. ) ;
#51386 = ORIENTED_EDGE ( 'NONE', *, *, #45307, .F. ) ;
#51385 = ADVANCED_FACE ( 'NONE', ( #49475 ), #16047, .F. ) ;
#51388 = EDGE_CURVE ( 'NONE', #103866, #130801, #15342, .T. ) ;
#51387 = VECTOR ( 'NONE', #120431, 1000.000000000000000 ) ;
#51389 = CARTESIAN_POINT ( 'NONE',  ( 79.89583333333331439, -2.130196079827427091, 7.949999999999999289 ) ) ;
#51390 = CIRCLE ( 'NONE', #7367, 2.500000000000000888 ) ;
#51391 =( LENGTH_UNIT ( ) NAMED_UNIT ( * ) SI_UNIT ( .MILLI., .METRE. ) );
#51392 = VERTEX_POINT ( 'NONE', #47358 ) ;
#51393 = CARTESIAN_POINT ( 'NONE',  ( 91.22502705046289861, 5.819803920172573974, -5.819803920172573086 ) ) ;
#51394 = PLANE ( 'NONE',  #125079 ) ;
#51395 = VECTOR ( 'NONE', #111273, 1000.000000000000000 ) ;
#51396 = VECTOR ( 'NONE', #86009, 1000.000000000000000 ) ;
#51397 = PLANE ( 'NONE',  #110374 ) ;
#51398 = EDGE_LOOP ( 'NONE', ( #23144, #110300, #107320, #125286 ) ) ;
#51399 = EDGE_CURVE ( 'NONE', #31547, #11149, #127726, .T. ) ;
#51400 = PLANE ( 'NONE',  #63 ) ;
#51401 = DIRECTION ( 'NONE',  ( 0.000000000000000000, -1.000000000000000000, 0.000000000000000000 ) ) ;
#51402 = DIRECTION ( 'NONE',  ( 0.7071067811865487940, 0.7071067811865463515, -0.000000000000000000 ) ) ;
#51403 = ADVANCED_FACE ( 'NONE', ( #37125 ), #48733, .T. ) ;
#51404 = EDGE_CURVE ( 'NONE', #95958, #3113, #38563, .T. ) ;
#51406 = ORIENTED_EDGE ( 'NONE', *, *, #20157, .T. ) ;
#51405 = LINE ( 'NONE', #72478, #93812 ) ;
#51407 = FACE_OUTER_BOUND ( 'NONE', #120599, .T. ) ;
#51408 = DIRECTION ( 'NONE',  ( -0.000000000000000000, 0.3543493200069153248, 0.9351131265310292928 ) ) ;
#51409 = DIRECTION ( 'NONE',  ( -0.000000000000000000, 0.000000000000000000, 1.000000000000000000 ) ) ;
#51410 = CARTESIAN_POINT ( 'NONE',  ( 12.70701326429294831, -21.74070752338406365, 4.999753212805217117 ) ) ;
#51411 = CARTESIAN_POINT ( 'NONE',  ( -27.48921356237309155, -27.52281430457074762, 5.000000000000000000 ) ) ;
#51412 = CARTESIAN_POINT ( 'NONE',  ( 53.94409967708047304, -48.16486758952285641, 37.61253110040706815 ) ) ;
#51413 = ORIENTED_EDGE ( 'NONE', *, *, #73769, .F. ) ;
#51414 = VERTEX_POINT ( 'NONE', #93665 ) ;
#51415 = CARTESIAN_POINT ( 'NONE',  ( 97.85459685856477563, -1.637169565754161615, 6.110000000000000320 ) ) ;
#51416 = ORIENTED_EDGE ( 'NONE', *, *, #102808, .T. ) ;
#51417 = EDGE_CURVE ( 'NONE', #75249, #32200, #37871, .T. ) ;
#51418 = SURFACE_STYLE_FILL_AREA ( #126122 ) ;
#51419 = CARTESIAN_POINT ( 'NONE',  ( 16.49999999999990052, 19.08746187583904685, 4.000000000000000000 ) ) ;
#51420 = EDGE_LOOP ( 'NONE', ( #70821, #46222, #11050, #49905 ) ) ;
#51421 = ADVANCED_FACE ( 'NONE', ( #48033 ), #59629, .F. ) ;
#51422 = LINE ( 'NONE', #116658, #11992 ) ;
#51423 = CARTESIAN_POINT ( 'NONE',  ( 3.489213562373097322, -27.52281430457057709, 5.000000000000000000 ) ) ;
#51424 = VECTOR ( 'NONE', #3298, 1000.000000000000000 ) ;
#51425 = STYLED_ITEM ( 'NONE', ( #123669 ), #54318 ) ;
#51426 = CARTESIAN_POINT ( 'NONE',  ( 94.70376352523145158, 6.109999999999998543, 1.122388791418548911E-15 ) ) ;
#51427 = VERTEX_POINT ( 'NONE', #104520 ) ;
#51428 = VECTOR ( 'NONE', #118873, 1000.000000000000000 ) ;
#51429 = LINE ( 'NONE', #85444, #53592 ) ;
#51430 = ORIENTED_EDGE ( 'NONE', *, *, #12104, .T. ) ;
#51431 = CARTESIAN_POINT ( 'NONE',  ( -34.49999999999976552, 7.464255608400418573, 4.994342998332163219 ) ) ;
#51432 = CARTESIAN_POINT ( 'NONE',  ( 19.28515664589288647, 1.196650378695337302, -30.59010235425025215 ) ) ;
#51433 = VECTOR ( 'NONE', #138939, 999.9999999999998863 ) ;
#51434 = DIRECTION ( 'NONE',  ( 1.000000000000000000, 0.000000000000000000, 1.899332272967292827E-15 ) ) ;
#51435 = ORIENTED_EDGE ( 'NONE', *, *, #103716, .T. ) ;
#51436 = VERTEX_POINT ( 'NONE', #3745 ) ;
#51437 = VERTEX_POINT ( 'NONE', #135740 ) ;
#51438 = DIRECTION ( 'NONE',  ( -0.000000000000000000, -0.3543493200069152693, 0.9351131265310292928 ) ) ;
#51439 = PLANE ( 'NONE',  #142572 ) ;
#51440 = CARTESIAN_POINT ( 'NONE',  ( 5.462903141435219823, -3.967499999999994476, 6.871911579029513106 ) ) ;
#51441 = VECTOR ( 'NONE', #138666, 1000.000000000000000 ) ;
#51442 = DIRECTION ( 'NONE',  ( -0.000000000000000000, -0.3543493200069152693, 0.9351131265310292928 ) ) ;
#51443 = EDGE_CURVE ( 'NONE', #93248, #33386, #71212, .T. ) ;
#51445 = ADVANCED_FACE ( 'NONE', ( #5177 ), #17508, .F. ) ;
#51444 = SURFACE_SIDE_STYLE ('',( #94908 ) ) ;
#51446 = VERTEX_POINT ( 'NONE', #82105 ) ;
#51447 =( BOUNDED_CURVE ( )  B_SPLINE_CURVE ( 3, ( #44734, #67155, #56324, #24353 ),
 .UNSPECIFIED., .F., .T. ) 
 B_SPLINE_CURVE_WITH_KNOTS ( ( 4, 4 ),
 ( 5.143245962375972091, 6.645403452391246191 ),
 .UNSPECIFIED. ) 
 CURVE ( )  GEOMETRIC_REPRESENTATION_ITEM ( )  RATIONAL_B_SPLINE_CURVE ( ( 1.000000000000000000, 0.8206354192515258328, 0.8206354192515258328, 1.000000000000000000 ) ) 
 REPRESENTATION_ITEM ( '' )  );
#51448 = ORIENTED_EDGE ( 'NONE', *, *, #69542, .T. ) ;
#51449 = DIRECTION ( 'NONE',  ( 0.6830127018922181881, 0.6830127018922202975, -0.2588190451025214056 ) ) ;
#51450 = EDGE_LOOP ( 'NONE', ( #69749, #98118, #138519, #8363 ) ) ;
#51451 = VERTEX_POINT ( 'NONE', #50162 ) ;
#51452 = AXIS2_PLACEMENT_3D ( 'NONE', #14497, #68908, #114511 ) ;
#51453 = VECTOR ( 'NONE', #105020, 1000.000000000000000 ) ;
#51454 = SURFACE_STYLE_USAGE ( .BOTH. , #78733 ) ;
#51455 = DIRECTION ( 'NONE',  ( 0.6830127018922181881, 0.6830127018922202975, -0.2588190451025214056 ) ) ;
#51456 = VERTEX_POINT ( 'NONE', #126283 ) ;
#51457 = VECTOR ( 'NONE', #11539, 1000.000000000000000 ) ;
#51458 = LINE ( 'NONE', #95649, #50668 ) ;
#51459 = PRESENTATION_STYLE_ASSIGNMENT (( #63068 ) ) ;
#51460 = ORIENTED_EDGE ( 'NONE', *, *, #120067, .T. ) ;
#51461 = CARTESIAN_POINT ( 'NONE',  ( 10.88982677111781783, -22.22500000000000142, 4.785647885939352086 ) ) ;
#51462 = CARTESIAN_POINT ( 'NONE',  ( -48.18398860626899705, 28.73617430169820608, 5.000000000000000000 ) ) ;
#51463 = ORIENTED_EDGE ( 'NONE', *, *, #34020, .F. ) ;
#51464 = LINE ( 'NONE', #7919, #117471 ) ;
#51465 = CARTESIAN_POINT ( 'NONE',  ( -4.499999999999968914, -2.568876922607790103, 4.000000000000000000 ) ) ;
#51466 = LINE ( 'NONE', #142057, #42288 ) ;
#51467 = ORIENTED_EDGE ( 'NONE', *, *, #43353, .T. ) ;
#51468 = DIRECTION ( 'NONE',  ( -0.7071067811865486830, -0.7071067811865464625, -0.000000000000000000 ) ) ;
#51469 = ORIENTED_EDGE ( 'NONE', *, *, #140543, .T. ) ;
#51470 = VERTEX_POINT ( 'NONE', #103106 ) ;
#51471 = VECTOR ( 'NONE', #703, 1000.000000000000114 ) ;
#51472 =( BOUNDED_CURVE ( )  B_SPLINE_CURVE ( 3, ( #26926, #15305, #71176, #137856 ),
 .UNSPECIFIED., .F., .T. ) 
 B_SPLINE_CURVE_WITH_KNOTS ( ( 4, 4 ),
 ( 5.920967161967926273, 7.341195215986641820 ),
 .UNSPECIFIED. ) 
 CURVE ( )  GEOMETRIC_REPRESENTATION_ITEM ( )  RATIONAL_B_SPLINE_CURVE ( ( 1.000000000000000000, 0.8388583629366603844, 0.8388583629366603844, 1.000000000000000000 ) ) 
 REPRESENTATION_ITEM ( '' )  );
#51473 = EDGE_LOOP ( 'NONE', ( #126004, #20895, #34025, #32392 ) ) ;
#51474 = CARTESIAN_POINT ( 'NONE',  ( 33.01626352523144448, -4.472830434245838482, 4.472830434245838482 ) ) ;
#51475 = PLANE ( 'NONE',  #46496 ) ;
#51476 = LINE ( 'NONE', #84804, #35740 ) ;
#51477 = CARTESIAN_POINT ( 'NONE',  ( -34.49999999999976552, -2.945670655169033481, 4.994342998332163219 ) ) ;
#51478 = CARTESIAN_POINT ( 'NONE',  ( 22.49999999999985434, 16.46639925780209524, 5.000000000000000000 ) ) ;
#51479 = CARTESIAN_POINT ( 'NONE',  ( -1.499999999999984013, 7.087461875839178305, 4.000000000000000000 ) ) ;
#51480 = LINE ( 'NONE', #63792, #133814 ) ;
#51481 = VECTOR ( 'NONE', #44055, 1000.000000000000000 ) ;
#51482 = AXIS2_PLACEMENT_3D ( 'NONE', #67026, #21377, #10473 ) ;
#51483 = VECTOR ( 'NONE', #36113, 1000.000000000000000 ) ;
#51484 = LINE ( 'NONE', #29007, #116389 ) ;
#51485 = AXIS2_PLACEMENT_3D ( 'NONE', #59877, #125115, #72221 ) ;
#51486 = LINE ( 'NONE', #129020, #66859 ) ;
#51487 = CARTESIAN_POINT ( 'NONE',  ( -0.005480084712502889671, 28.92564299267938210, 4.000000000000000000 ) ) ;
#51488 = CARTESIAN_POINT ( 'NONE',  ( 3.005480084712505828, 28.92564299267936079, 4.000000000000000000 ) ) ;
#51489 = VERTEX_POINT ( 'NONE', #26961 ) ;
#51490 = ORIENTED_EDGE ( 'NONE', *, *, #132645, .F. ) ;
#51491 = ORIENTED_EDGE ( 'NONE', *, *, #120816, .T. ) ;
#51492 = VECTOR ( 'NONE', #115511, 1000.000000000000000 ) ;
#51493 = EDGE_LOOP ( 'NONE', ( #124344, #34051, #81648, #21631 ) ) ;
#51494 = CIRCLE ( 'NONE', #2832, 2.500000000000000888 ) ;
#51495 = DIRECTION ( 'NONE',  ( -0.7071067811865486830, 0.7071067811865464625, 0.000000000000000000 ) ) ;
#51496 = ORIENTED_EDGE ( 'NONE', *, *, #106, .F. ) ;
#51498 = EDGE_LOOP ( 'NONE', ( #85606, #134980, #37129, #32089 ) ) ;
#51497 = ADVANCED_FACE ( 'NONE', ( #71934 ), #91525, .F. ) ;
#51499 = DIRECTION ( 'NONE',  ( -0.000000000000000000, 0.000000000000000000, 1.000000000000000000 ) ) ;
#51500 = SURFACE_STYLE_FILL_AREA ( #31874 ) ;
#51501 = PLANE ( 'NONE',  #40993 ) ;
#51502 = EDGE_CURVE ( 'NONE', #39673, #42516, #74046, .T. ) ;
#51503 = EDGE_CURVE ( 'NONE', #143429, #128927, #52980, .T. ) ;
#51504 = CARTESIAN_POINT ( 'NONE',  ( 5.816011393731002066, 28.73617430169783304, 5.000000000000000000 ) ) ;
#51505 = ORIENTED_EDGE ( 'NONE', *, *, #55197, .F. ) ;
#51506 = FACE_OUTER_BOUND ( 'NONE', #104118, .T. ) ;
#51507 = VERTEX_POINT ( 'NONE', #63205 ) ;
#51509 = EDGE_CURVE ( 'NONE', #121, #126591, #85610, .T. ) ;
#51508 = CARTESIAN_POINT ( 'NONE',  ( 28.49999999999981526, 22.08746187583901843, 4.000000000000000000 ) ) ;
#51510 = EDGE_CURVE ( 'NONE', #3281, #130856, #86362, .T. ) ;
#51511 = CARTESIAN_POINT ( 'NONE',  ( -22.49999999999984723, -6.839392718269148297, -8.480912228396030983 ) ) ;
#51512 = CARTESIAN_POINT ( 'NONE',  ( 13.48373647476855375, -5.808823158059035485, -5.808823158059033709 ) ) ;
#51513 = ORIENTED_EDGE ( 'NONE', *, *, #137074, .F. ) ;
#51514 = CARTESIAN_POINT ( 'NONE',  ( 91.05793019189812298, 6.110000000000001208, -1.637169565754156286 ) ) ;
#51515 = ADVANCED_FACE ( 'NONE', ( #87062 ), #108768, .F. ) ;
#51516 = CARTESIAN_POINT ( 'NONE',  ( 15.70710678118643422, -9.740707523384182664, 5.000000000000000000 ) ) ;
#51517 = DIRECTION ( 'NONE',  ( 0.000000000000000000, -1.000000000000000000, 0.000000000000000000 ) ) ;
#51518 = ORIENTED_EDGE ( 'NONE', *, *, #133450, .F. ) ;
#51519 = ORIENTED_EDGE ( 'NONE', *, *, #79405, .T. ) ;
#51520 = DIRECTION ( 'NONE',  ( 0.000000000000000000, -1.000000000000000000, 0.000000000000000000 ) ) ;
#51521 = ORIENTED_EDGE ( 'NONE', *, *, #39237, .T. ) ;
#51522 = DIRECTION ( 'NONE',  ( 1.000000000000000000, 0.000000000000000000, 0.000000000000000000 ) ) ;
#51523 = FACE_OUTER_BOUND ( 'NONE', #44010, .T. ) ;
#51524 = LINE ( 'NONE', #86293, #79826 ) ;
#51525 = LINE ( 'NONE', #31196, #24091 ) ;
#51526 = ORIENTED_EDGE ( 'NONE', *, *, #65697, .T. ) ;
#51527 = STYLED_ITEM ( 'NONE', ( #261 ), #100104 ) ;
#51528 = DIRECTION ( 'NONE',  ( -0.7071067811865487940, 0.7071067811865463515, -0.000000000000000000 ) ) ;
#51529 = EDGE_CURVE ( 'NONE', #15565, #23831, #16208, .T. ) ;
#51530 = VECTOR ( 'NONE', #80233, 1000.000000000000000 ) ;
#51531 = CARTESIAN_POINT ( 'NONE',  ( 5.994519915287488843, 28.92564299267942118, 4.000000000000000000 ) ) ;
#51532 = CARTESIAN_POINT ( 'NONE',  ( 31.49999999999978684, -1.592773361805341459, -6.492772025301299266 ) ) ;
#51533 = EDGE_LOOP ( 'NONE', ( #18024, #50904, #80591, #131217 ) ) ;
#51534 = CYLINDRICAL_SURFACE ( 'NONE', #35129, 0.5000000000000004441 ) ;
#51535 = AXIS2_PLACEMENT_3D ( 'NONE', #51052, #138780, #117003 ) ;
#51536 = AXIS2_PLACEMENT_3D ( 'NONE', #54983, #55698, #68037 ) ;
#51537 = EDGE_CURVE ( 'NONE', #93024, #66606, #118033, .T. ) ;
#51538 = CARTESIAN_POINT ( 'NONE',  ( 20.99999999999986855, 14.58746187583909482, 4.000000000000000000 ) ) ;
#51539 = ORIENTED_EDGE ( 'NONE', *, *, #101494, .T. ) ;
#51541 = ORIENTED_EDGE ( 'NONE', *, *, #93045, .T. ) ;
#51540 = FACE_OUTER_BOUND ( 'NONE', #49212, .T. ) ;
#51542 = LINE ( 'NONE', #95737, #111872 ) ;
#51543 = CARTESIAN_POINT ( 'NONE',  ( 18.79289321881332953, 18.75929247661552779, 5.000000000000000000 ) ) ;
#51544 = EDGE_CURVE ( 'NONE', #112859, #77801, #52280, .T. ) ;
#51545 = EDGE_LOOP ( 'NONE', ( #78404, #12734, #133275, #81142 ) ) ;
#51546 = CARTESIAN_POINT ( 'NONE',  ( -7.499999999999936939, -4.912538124160708897, 4.000000000000000000 ) ) ;
#51547 = CARTESIAN_POINT ( 'NONE',  ( 27.00000000000001421, 3.441786896390103934, 7.166352137582786774 ) ) ;
#51548 = DIRECTION ( 'NONE',  ( -0.7071067811865486830, -0.7071067811865464625, 0.000000000000000000 ) ) ;
#51549 = CARTESIAN_POINT ( 'NONE',  ( 21.18398860626899349, 28.73617430169802134, 5.000000000000000000 ) ) ;
#51550 = CYLINDRICAL_SURFACE ( 'NONE', #141569, 0.5000000000000001110 ) ;
#51551 = CARTESIAN_POINT ( 'NONE',  ( 2.916666666666666963, 5.278424836066147208, 3.047499999999990550 ) ) ;
#51552 = AXIS2_PLACEMENT_3D ( 'NONE', #117030, #126467, #138810 ) ;
#51554 = EDGE_CURVE ( 'NONE', #123479, #80179, #141442, .T. ) ;
#51553 = CARTESIAN_POINT ( 'NONE',  ( 46.93749999999999289, 5.819803920172574863, -5.819803920172573086 ) ) ;
#51555 = DIRECTION ( 'NONE',  ( 0.6830127018922180770, -0.6830127018922204085, -0.2588190451025213501 ) ) ;
#51556 = DIRECTION ( 'NONE',  ( -0.7071067811865487940, 0.7071067811865463515, -0.000000000000000000 ) ) ;
#51557 = VECTOR ( 'NONE', #97547, 1000.000000000000000 ) ;
#51558 = CARTESIAN_POINT ( 'NONE',  ( -38.75830541574789123, 0.7592924766157104211, 14.37146558664991680 ) ) ;
#51559 = CARTESIAN_POINT ( 'NONE',  ( 0.000000000000000000, 0.000000000000000000, 5.000000000000000000 ) ) ;
#51560 = LINE ( 'NONE', #19620, #124078 ) ;
#51561 = ORIENTED_EDGE ( 'NONE', *, *, #40773, .T. ) ;
#51562 = VERTEX_POINT ( 'NONE', #18941 ) ;
#51563 = EDGE_LOOP ( 'NONE', ( #181, #92805, #12690, #50220 ) ) ;
#51564 = EDGE_CURVE ( 'NONE', #110816, #111848, #103855, .T. ) ;
#51565 = CARTESIAN_POINT ( 'NONE',  ( 115.3333333333333286, -6.884901960086287964, 3.974999999999998312 ) ) ;
#51566 = ORIENTED_EDGE ( 'NONE', *, *, #113714, .T. ) ;
#51567 = ORIENTED_EDGE ( 'NONE', *, *, #96887, .T. ) ;
#51568 = ADVANCED_FACE ( 'NONE', ( #140710 ), #131279, .F. ) ;
#51569 = ORIENTED_EDGE ( 'NONE', *, *, #100955, .T. ) ;
#51570 = DIRECTION ( 'NONE',  ( -0.6830127018922181881, 0.6830127018922202975, -0.2588190451025214056 ) ) ;
#51571 = CARTESIAN_POINT ( 'NONE',  ( -36.48921356237310221, -27.52281430457080802, 5.000000000000000000 ) ) ;
#51572 = AXIS2_PLACEMENT_3D ( 'NONE', #53381, #75174, #120771 ) ;
#51573 = ORIENTED_EDGE ( 'NONE', *, *, #20117, .T. ) ;
#51574 = CYLINDRICAL_SURFACE ( 'NONE', #16090, 0.5000000000000004441 ) ;
#51575 = ADVANCED_FACE ( 'NONE', ( #84916 ), #55590, .T. ) ;
#51576 = CARTESIAN_POINT ( 'NONE',  ( 39.18398860626899705, 28.73617430169814568, 5.000000000000000000 ) ) ;
#51577 = LINE ( 'NONE', #39269, #32471 ) ;
#51578 = DIRECTION ( 'NONE',  ( 0.000000000000000000, -1.000000000000000000, 0.000000000000000000 ) ) ;
#51579 = CARTESIAN_POINT ( 'NONE',  ( 102.3754301918981184, -5.291415217122920289, -3.055000000000001492 ) ) ;
#51580 = EDGE_LOOP ( 'NONE', ( #142863, #3034, #58499, #100820 ) ) ;
#51581 = DIRECTION ( 'NONE',  ( 0.7071067811865487940, 0.7071067811865463515, -0.000000000000000000 ) ) ;
#51582 = DIRECTION ( 'NONE',  ( -0.6830127018922180770, -0.6830127018922204085, -0.2588190451025213501 ) ) ;
#51583 = AXIS2_PLACEMENT_3D ( 'NONE', #110368, #22634, #34270 ) ;
#51584 = FACE_OUTER_BOUND ( 'NONE', #143340, .T. ) ;
#51585 = CARTESIAN_POINT ( 'NONE',  ( 27.78752705046289151, 0.000000000000000000, -7.949999999999998401 ) ) ;
#51586 = LINE ( 'NONE', #142861, #86192 ) ;
#51587 = CARTESIAN_POINT ( 'NONE',  ( -3.489213562373097322, -27.52281430457057709, 5.000000000000000000 ) ) ;
#51588 = VERTEX_POINT ( 'NONE', #129129 ) ;
#51589 = ORIENTED_EDGE ( 'NONE', *, *, #103674, .T. ) ;
#51590 = CARTESIAN_POINT ( 'NONE',  ( 24.62499999999999289, -7.950000000000000178, -4.867971026610729436E-16 ) ) ;
#51591 = ORIENTED_EDGE ( 'NONE', *, *, #40735, .T. ) ;
#51592 = ADVANCED_FACE ( 'NONE', ( #63896 ), #53738, .F. ) ;
#51593 = DIRECTION ( 'NONE',  ( -0.7071067811865486830, 0.7071067811865464625, 0.000000000000000000 ) ) ;
#51594 = DIRECTION ( 'NONE',  ( 0.7071067811865486830, -0.7071067811865464625, -0.000000000000000000 ) ) ;
#51595 = CIRCLE ( 'NONE', #95534, 2.055000000000000604 ) ;
#51596 = MECHANICAL_DESIGN_GEOMETRIC_PRESENTATION_REPRESENTATION (  '', ( #77059 ), #39082 ) ;
#51597 = DIRECTION ( 'NONE',  ( 1.000000000000000000, 0.000000000000000000, 0.000000000000000000 ) ) ;
#51598 = DIRECTION ( 'NONE',  ( 0.000000000000000000, -1.000000000000000000, 0.000000000000000000 ) ) ;
#51599 = VECTOR ( 'NONE', #85013, 1000.000000000000000 ) ;
#51600 = CARTESIAN_POINT ( 'NONE',  ( 31.82816939922330945, 21.75929247661549581, 4.000000000000000000 ) ) ;
#51602 = AXIS2_PLACEMENT_3D ( 'NONE', #6834, #95314, #68781 ) ;
#51601 = DIRECTION ( 'NONE',  ( -0.3543493200069162685, -0.000000000000000000, -0.9351131265310288487 ) ) ;
#51603 = CARTESIAN_POINT ( 'NONE',  ( 122.9954301918981230, 5.291415217122916737, 3.055000000000001936 ) ) ;
#51604 = ORIENTED_EDGE ( 'NONE', *, *, #46492, .F. ) ;
#51605 = PLANE ( 'NONE',  #73387 ) ;
#51606 = ORIENTED_EDGE ( 'NONE', *, *, #23223, .F. ) ;
#51607 = VECTOR ( 'NONE', #121361, 1000.000000000000000 ) ;
#51608 = AXIS2_PLACEMENT_3D ( 'NONE', #72654, #76730, #95048 ) ;
#51609 = CARTESIAN_POINT ( 'NONE',  ( -8.186508646023558100, -15.74070752338411694, 8.904080028138961822 ) ) ;
#51610 = DIRECTION ( 'NONE',  ( -1.000000000000000000, -1.224606353822377258E-16, -0.000000000000000000 ) ) ;
#51611 = CARTESIAN_POINT ( 'NONE',  ( 20.51078643762690490, -27.52281430457041012, 5.000000000000000000 ) ) ;
#51612 = ORIENTED_EDGE ( 'NONE', *, *, #22525, .T. ) ;
#51613 = EDGE_CURVE ( 'NONE', #135652, #96844, #52955, .T. ) ;
#51614 = CARTESIAN_POINT ( 'NONE',  ( 45.20876352523143993, -7.482591942790329030E-16, 6.110000000000001208 ) ) ;
#51615 = ORIENTED_EDGE ( 'NONE', *, *, #38078, .F. ) ;
#51616 = LINE ( 'NONE', #82819, #21576 ) ;
#51617 = DIRECTION ( 'NONE',  ( 0.000000000000000000, -0.000000000000000000, -1.000000000000000000 ) ) ;
#51618 = CARTESIAN_POINT ( 'NONE',  ( 7.171830600776420539, -5.240707523384230626, 4.000000000000000000 ) ) ;
#51619 = LINE ( 'NONE', #85637, #55435 ) ;
#51620 = EDGE_CURVE ( 'NONE', #121270, #2749, #74785, .T. ) ;
#51621 = AXIS2_PLACEMENT_3D ( 'NONE', #113375, #93073, #136559 ) ;
#51622 = CARTESIAN_POINT ( 'NONE',  ( 35.49543019189811588, 5.291415217122916737, 3.055000000000001936 ) ) ;
#51623 = ORIENTED_EDGE ( 'NONE', *, *, #83427, .F. ) ;
#51624 = CARTESIAN_POINT ( 'NONE',  ( -31.49999999999977973, -20.56887692260759337, 4.000000000000000000 ) ) ;
#51625 = ORIENTED_EDGE ( 'NONE', *, *, #123833, .T. ) ;
#51626 = VERTEX_POINT ( 'NONE', #40023 ) ;
#51627 = ORIENTED_EDGE ( 'NONE', *, *, #30602, .F. ) ;
#51628 = EDGE_CURVE ( 'NONE', #115355, #101030, #95063, .T. ) ;
#51629 = CIRCLE ( 'NONE', #132681, 2.500000000000000888 ) ;
#51630 = ADVANCED_FACE ( 'NONE', ( #29110 ), #62466, .T. ) ;
#51631 = CARTESIAN_POINT ( 'NONE',  ( 59.87086038379622721, 6.884901960086289741, -3.974999999999993427 ) ) ;
#51632 = ORIENTED_EDGE ( 'NONE', *, *, #85034, .T. ) ;
#51633 = VECTOR ( 'NONE', #29373, 1000.000000000000000 ) ;
#51634 =( LENGTH_UNIT ( ) NAMED_UNIT ( * ) SI_UNIT ( .MILLI., .METRE. ) );
#51635 = VECTOR ( 'NONE', #96829, 1000.000000000000000 ) ;
#51636 = PLANE ( 'NONE',  #16400 ) ;
#51637 = FACE_BOUND ( 'NONE', #115341, .T. ) ;
#51638 = ADVANCED_FACE ( 'NONE', ( #58591 ), #46263, .F. ) ;
#51639 = CARTESIAN_POINT ( 'NONE',  ( -8.999999999999934275, -18.03360074219754949, 5.000000000000000000 ) ) ;
#51640 = CARTESIAN_POINT ( 'NONE',  ( 7.940000000000001279, -33.26999999999999602, -10.00000000000000178 ) ) ;
#51641 = LINE ( 'NONE', #74836, #122591 ) ;
#51642 = ORIENTED_EDGE ( 'NONE', *, *, #81155, .F. ) ;
#51643 = CARTESIAN_POINT ( 'NONE',  ( 42.48921356237308800, -27.52281430457085065, 5.000000000000000000 ) ) ;
#51644 = ORIENTED_EDGE ( 'NONE', *, *, #64654, .F. ) ;
#51645 = ORIENTED_EDGE ( 'NONE', *, *, #21907, .T. ) ;
#51646 = CARTESIAN_POINT ( 'NONE',  ( -23.01844734635655954, 18.75929247661551713, 20.33588619593448144 ) ) ;
#51647 = ORIENTED_EDGE ( 'NONE', *, *, #126095, .F. ) ;
#51648 = AXIS2_PLACEMENT_3D ( 'NONE', #26740, #118563, #70986 ) ;
#51649 = CARTESIAN_POINT ( 'NONE',  ( 59.41209685856478728, 5.291415217122921177, -3.054999999999994831 ) ) ;
#51650 = VERTEX_POINT ( 'NONE', #13567 ) ;
#51651 = DIRECTION ( 'NONE',  ( -0.7071067811865487940, 0.7071067811865463515, -0.000000000000000000 ) ) ;
#51652 = DIRECTION ( 'NONE',  ( -0.7071067811865487940, 0.7071067811865463515, -0.000000000000000000 ) ) ;
#51653 = AXIS2_PLACEMENT_3D ( 'NONE', #135771, #13247, #91555 ) ;
#51654 = EDGE_LOOP ( 'NONE', ( #28916, #129345, #25548, #70765 ) ) ;
#51655 = CARTESIAN_POINT ( 'NONE',  ( -11.51078643762690490, -27.52281430457047406, 5.000000000000000000 ) ) ;
#51656 = VECTOR ( 'NONE', #4595, 1000.000000000000227 ) ;
#51657 = DIRECTION ( 'NONE',  ( -0.000000000000000000, -0.3543493200069152693, 0.9351131265310292928 ) ) ;
#51658 = DIRECTION ( 'NONE',  ( 0.3543493200069162685, -0.000000000000000000, -0.9351131265310288487 ) ) ;
#51659 = FACE_OUTER_BOUND ( 'NONE', #88151, .T. ) ;
#51660 = CARTESIAN_POINT ( 'NONE',  ( 12.48921356237309155, -27.52281430457064104, 5.000000000000000000 ) ) ;
#51661 = LINE ( 'NONE', #8794, #115812 ) ;
#51662 = ORIENTED_EDGE ( 'NONE', *, *, #68906, .T. ) ;
#51663 = VECTOR ( 'NONE', #3023, 1000.000000000000000 ) ;
#51664 = ORIENTED_EDGE ( 'NONE', *, *, #40276, .T. ) ;
#51665 = CARTESIAN_POINT ( 'NONE',  ( 19.73330628287043709, -6.094999999999989981, -1.633150327867689322 ) ) ;
#51666 = CARTESIAN_POINT ( 'NONE',  ( -28.17183060077627488, -8.240707523384195099, 4.000000000000000000 ) ) ;
#51667 = EDGE_LOOP ( 'NONE', ( #119281, #99608, #110975, #128830 ) ) ;
#51668 = VERTEX_POINT ( 'NONE', #2703 ) ;
#51669 = ORIENTED_EDGE ( 'NONE', *, *, #77504, .F. ) ;
#51670 = CARTESIAN_POINT ( 'NONE',  ( 0.000000000000000000, 0.000000000000000000, 5.000000000000000000 ) ) ;
#51671 = FACE_OUTER_BOUND ( 'NONE', #65178, .T. ) ;
#51672 = EDGE_CURVE ( 'NONE', #132730, #110607, #80311, .T. ) ;
#51673 = CARTESIAN_POINT ( 'NONE',  ( 7.600000000000009415, 0.000000000000000000, 1.249999999999971578 ) ) ;
#51674 = VECTOR ( 'NONE', #83145, 1000.000000000000227 ) ;
#51675 = VERTEX_POINT ( 'NONE', #57847 ) ;
#51676 = DIRECTION ( 'NONE',  ( 0.7071067811865487940, 0.7071067811865463515, -0.000000000000000000 ) ) ;
#51678 = EDGE_CURVE ( 'NONE', #84275, #87748, #81013, .T. ) ;
#51677 = PRESENTATION_STYLE_ASSIGNMENT (( #116913 ) ) ;
#51679 = EDGE_CURVE ( 'NONE', #49159, #48229, #48366, .T. ) ;
#51680 = CARTESIAN_POINT ( 'NONE',  ( 16.54623647476855552, -7.934999999999990727, 4.858786175617117713E-16 ) ) ;
#51681 = CARTESIAN_POINT ( 'NONE',  ( 59.99451991528749772, 28.92564299267980132, 4.000000000000000000 ) ) ;
#51682 = ADVANCED_FACE ( 'NONE', ( #70172 ), #4081, .F. ) ;
#51683 = VERTEX_POINT ( 'NONE', #142867 ) ;
#51684 = CARTESIAN_POINT ( 'NONE',  ( 127.5162635252314516, -4.472830434245839371, 4.472830434245839371 ) ) ;
#51685 = EDGE_CURVE ( 'NONE', #49717, #39409, #114332, .T. ) ;
#51686 = DIRECTION ( 'NONE',  ( 0.7071067811865486830, -0.7071067811865464625, -0.000000000000000000 ) ) ;
#51687 = DIRECTION ( 'NONE',  ( 0.3543493200069162685, -0.000000000000000000, -0.9351131265310288487 ) ) ;
#51688 = CONICAL_SURFACE ( 'NONE', #49433, 1.142820323027522456, 0.2617993877991512952 ) ;
#51690 = ORIENTED_EDGE ( 'NONE', *, *, #128910, .T. ) ;
#51689 = DIRECTION ( 'NONE',  ( 0.000000000000000000, -1.000000000000000000, 0.000000000000000000 ) ) ;
#51691 = CARTESIAN_POINT ( 'NONE',  ( 10.83747294953710671, 6.094999999999989981, -1.119633336120465690E-15 ) ) ;
#51692 = EDGE_LOOP ( 'NONE', ( #82076, #92769, #3689, #90425 ) ) ;
#51693 = EDGE_CURVE ( 'NONE', #75711, #49314, #59283, .T. ) ;
#51694 = LINE ( 'NONE', #35679, #123780 ) ;
#51695 = DIRECTION ( 'NONE',  ( 1.000000000000000000, 0.000000000000000000, 0.000000000000000000 ) ) ;
#51696 = DIRECTION ( 'NONE',  ( 1.000000000000000000, 1.224606353822377258E-16, 0.000000000000000000 ) ) ;
#51698 = EDGE_LOOP ( 'NONE', ( #80851, #107105, #46488, #138436 ) ) ;
#51697 = AXIS2_PLACEMENT_3D ( 'NONE', #45794, #132811, #47255 ) ;
#51699 = ADVANCED_FACE ( 'NONE', ( #124497 ), #102037, .F. ) ;
#51700 = CARTESIAN_POINT ( 'NONE',  ( 24.91272823266826109, 2.053671025133813277, 5.000000000000000000 ) ) ;
#51701 = FACE_OUTER_BOUND ( 'NONE', #141494, .T. ) ;
#51702 = DIRECTION ( 'NONE',  ( 0.000000000000000000, 0.000000000000000000, 1.000000000000000000 ) ) ;
#51703 = VECTOR ( 'NONE', #116218, 1000.000000000000000 ) ;
#51704 = ORIENTED_EDGE ( 'NONE', *, *, #80863, .F. ) ;
#51705 = PRESENTATION_LAYER_ASSIGNMENT (  '', '', ( #93287 ) ) ;
#51706 = CARTESIAN_POINT ( 'NONE',  ( 0.000000000000000000, 0.000000000000000000, 5.000000000000000000 ) ) ;
#51707 = LINE ( 'NONE', #7442, #125728 ) ;
#51708 = AXIS2_PLACEMENT_3D ( 'NONE', #113880, #58119, #5080 ) ;
#51709 = CARTESIAN_POINT ( 'NONE',  ( 0.7123099396602788902, -21.73547319004781642, 4.999917730833664642 ) ) ;
#51710 = ADVANCED_FACE ( 'NONE', ( #79629 ), #43554, .T. ) ;
#51711 = CARTESIAN_POINT ( 'NONE',  ( -60.48921356237309510, -27.52281430457097500, 5.000000000000000000 ) ) ;
#51712 = LINE ( 'NONE', #140147, #113206 ) ;
#51713 = EDGE_LOOP ( 'NONE', ( #85174, #27069, #85669, #104297, #78756 ) ) ;
#51714 = VERTEX_POINT ( 'NONE', #26614 ) ;
#51715 = DIRECTION ( 'NONE',  ( 0.7071067811865487940, 0.7071067811865463515, 0.000000000000000000 ) ) ;
#51716 = CARTESIAN_POINT ( 'NONE',  ( 3.730677800976790248, -49.14999999999999147, 40.92499999999998295 ) ) ;
#51717 = ADVANCED_FACE ( 'NONE', ( #76929 ), #91190, .T. ) ;
#51718 = CARTESIAN_POINT ( 'NONE',  ( 13.97873647476855119, -5.808823158059033709, 5.808823158059035485 ) ) ;
#51719 = LINE ( 'NONE', #94475, #87545 ) ;
#51720 = VECTOR ( 'NONE', #8004, 1000.000000000000000 ) ;
#51721 = LINE ( 'NONE', #37996, #57643 ) ;
#51722 = CARTESIAN_POINT ( 'NONE',  ( 14.99999999999990230, -1.447814304570822053, 5.000000000000000000 ) ) ;
#51723 = ORIENTED_EDGE ( 'NONE', *, *, #81909, .T. ) ;
#51724 = LINE ( 'NONE', #123417, #120763 ) ;
#51725 = LINE ( 'NONE', #52408, #56304 ) ;
#51726 = PLANE ( 'NONE',  #43689 ) ;
#51727 = CARTESIAN_POINT ( 'NONE',  ( 41.76626352523145158, 4.472830434245839371, -4.472830434245839371 ) ) ;
#51728 = VECTOR ( 'NONE', #65621, 1000.000000000000000 ) ;
#51729 = DIRECTION ( 'NONE',  ( 0.7071067811865486830, -0.7071067811865464625, -0.000000000000000000 ) ) ;
#51730 = VERTEX_POINT ( 'NONE', #91859 ) ;
#51731 = PLANE ( 'NONE',  #46522 ) ;
#51732 = VECTOR ( 'NONE', #125440, 1000.000000000000000 ) ;
#51733 = EDGE_LOOP ( 'NONE', ( #72268, #135276, #87572, #119602 ) ) ;
#51734 = EDGE_CURVE ( 'NONE', #48675, #117423, #143526, .T. ) ;
#51735 = EDGE_LOOP ( 'NONE', ( #39816, #98567, #62415, #28693, #139224 ) ) ;
#51736 = DIRECTION ( 'NONE',  ( 0.6830127018922180770, -0.6830127018922204085, -0.2588190451025213501 ) ) ;
#51737 = DIRECTION ( 'NONE',  ( -0.7071067811865486830, -0.7071067811865464625, 0.000000000000000000 ) ) ;
#51739 = EDGE_CURVE ( 'NONE', #63249, #44387, #139136, .T. ) ;
#51738 =( BOUNDED_CURVE ( )  B_SPLINE_CURVE ( 3, ( #36698, #48297, #37437, #115655 ),
 .UNSPECIFIED., .F., .F. ) 
 B_SPLINE_CURVE_WITH_KNOTS ( ( 4, 4 ),
 ( 1.901594255663617172, 1.933014472006534534 ),
 .UNSPECIFIED. ) 
 CURVE ( )  GEOMETRIC_REPRESENTATION_ITEM ( )  RATIONAL_B_SPLINE_CURVE ( ( 1.000000000000000000, 0.9999177325257868620, 0.9999177325257868620, 1.000000000000000000 ) ) 
 REPRESENTATION_ITEM ( '' )  );
#51740 =( NAMED_UNIT ( * ) PLANE_ANGLE_UNIT ( ) SI_UNIT ( $, .RADIAN. ) );
#51742 = VECTOR ( 'NONE', #43849, 1000.000000000000000 ) ;
#51741 = CARTESIAN_POINT ( 'NONE',  ( -4.499999999999962697, -17.94781430457065241, 5.000000000000000000 ) ) ;
#51743 = LINE ( 'NONE', #110357, #44001 ) ;
#51744 = LINE ( 'NONE', #21234, #71986 ) ;
#51745 = CARTESIAN_POINT ( 'NONE',  ( 32.99451991528749062, 28.92564299267960948, 4.000000000000000000 ) ) ;
#51746 = ORIENTED_EDGE ( 'NONE', *, *, #90683, .T. ) ;
#51747 = DIRECTION ( 'NONE',  ( -0.3543493200069163240, -0.000000000000000000, 0.9351131265310288487 ) ) ;
#51748 = LINE ( 'NONE', #17647, #42296 ) ;
#51749 = CARTESIAN_POINT ( 'NONE',  ( 32.99999999999977973, -0.8619312979531654761, -5.102805207349749850 ) ) ;
#51750 = CARTESIAN_POINT ( 'NONE',  ( 29.11162361894740513, 9.759292476615618384, 17.35367589129205967 ) ) ;
#51751 = CARTESIAN_POINT ( 'NONE',  ( -6.489213562373093325, -27.52281430457059841, 5.000000000000000000 ) ) ;
#51752 = EDGE_CURVE ( 'NONE', #23719, #132598, #66051, .T. ) ;
#51753 = CARTESIAN_POINT ( 'NONE',  ( 103.3291937171295700, -3.975000000000001865, 6.884901960086284411 ) ) ;
#51754 = CIRCLE ( 'NONE', #24003, 9.119999999999999218 ) ;
#51755 = CARTESIAN_POINT ( 'NONE',  ( 70.51669371712954160, 7.950000000000001066, -2.130196079827421318 ) ) ;
#51756 = VECTOR ( 'NONE', #30102, 1000.000000000000227 ) ;
#51757 = CARTESIAN_POINT ( 'NONE',  ( 0.000000000000000000, -5.520864266206504263E-14, 0.000000000000000000 ) ) ;
#51758 = VERTEX_POINT ( 'NONE', #68713 ) ;
#51759 = VERTEX_POINT ( 'NONE', #36085 ) ;
#51760 = CARTESIAN_POINT ( 'NONE',  ( 53.20833333333332860, -3.974999999999999201, -6.884901960086287964 ) ) ;
#51761 = DIRECTION ( 'NONE',  ( 1.000000000000000000, 0.000000000000000000, 0.000000000000000000 ) ) ;
#51762 = EDGE_CURVE ( 'NONE', #2559, #141411, #25172, .T. ) ;
#51763 = LINE ( 'NONE', #85079, #2234 ) ;
#51764 =( NAMED_UNIT ( * ) PLANE_ANGLE_UNIT ( ) SI_UNIT ( $, .RADIAN. ) );
#51765 = ORIENTED_EDGE ( 'NONE', *, *, #130933, .F. ) ;
#51766 = LINE ( 'NONE', #49645, #118529 ) ;
#51767 = CARTESIAN_POINT ( 'NONE',  ( 51.62543019189811133, 5.291415217122919401, 3.055000000000002824 ) ) ;
#51768 = EDGE_LOOP ( 'NONE', ( #41881, #53685, #126149, #86836, #141197, #141337 ) ) ;
#51769 = DIRECTION ( 'NONE',  ( -0.6830127018922180770, -0.6830127018922204085, -0.2588190451025213501 ) ) ;
#51770 = ORIENTED_EDGE ( 'NONE', *, *, #116005, .F. ) ;
#51771 = ORIENTED_EDGE ( 'NONE', *, *, #30027, .F. ) ;
#51772 = PRESENTATION_LAYER_ASSIGNMENT (  '', '', ( #77250 ) ) ;
#51773 = CARTESIAN_POINT ( 'NONE',  ( 34.82816939922328459, -2.240707523384267930, 4.000000000000000000 ) ) ;
#51774 = CARTESIAN_POINT ( 'NONE',  ( -29.99451991528749417, 28.92564299267958816, 4.000000000000000000 ) ) ;
#51775 = CARTESIAN_POINT ( 'NONE',  ( -12.69999999999998153, 0.000000000000000000, 2.500000000000000444 ) ) ;
#51776 = CARTESIAN_POINT ( 'NONE',  ( 2.999999999999999112, -1.600000000000013634, 20.40202195861969159 ) ) ;
#51777 = VERTEX_POINT ( 'NONE', #3407 ) ;
#51778 = EDGE_CURVE ( 'NONE', #90362, #121849, #74100, .T. ) ;
#51779 = CARTESIAN_POINT ( 'NONE',  ( -12.70701326429296252, -21.74070752338406010, 4.999753212805220670 ) ) ;
#51780 = CARTESIAN_POINT ( 'NONE',  ( 13.22674160717825842, -11.24070752338416135, 18.24660765846985200 ) ) ;
#51783 = EDGE_CURVE ( 'NONE', #105463, #112966, #49387, .T. ) ;
#51782 = ORIENTED_EDGE ( 'NONE', *, *, #33505, .T. ) ;
#51781 = LINE ( 'NONE', #105410, #82337 ) ;
#51784 = CARTESIAN_POINT ( 'NONE',  ( 127.0000000000000000, 1.564650039245123914, 6.154215649023822010 ) ) ;
#51785 = EDGE_CURVE ( 'NONE', #74639, #136354, #59971, .T. ) ;
#51786 = DIRECTION ( 'NONE',  ( 0.9707728879609256456, 0.000000000000000000, -0.2400000000000085398 ) ) ;
#51787 = MECHANICAL_DESIGN_GEOMETRIC_PRESENTATION_REPRESENTATION (  '', ( #142027 ), #125873 ) ;
#51788 = CARTESIAN_POINT ( 'NONE',  ( 30.29974487139158867, -27.71228299555227537, 4.000000000000000000 ) ) ;
#51789 = CARTESIAN_POINT ( 'NONE',  ( -29.29289321881324426, -18.74070752338408852, 5.000000000000000000 ) ) ;
#51790 = DIRECTION ( 'NONE',  ( 0.7071067811865487940, 0.7071067811865463515, 0.000000000000000000 ) ) ;
#51791 = ORIENTED_EDGE ( 'NONE', *, *, #102615, .F. ) ;
#51792 = EDGE_CURVE ( 'NONE', #95280, #34098, #73689, .T. ) ;
#51793 = EDGE_LOOP ( 'NONE', ( #78785, #10248, #125354, #113329 ) ) ;
#51794 = AXIS2_PLACEMENT_3D ( 'NONE', #81087, #35461, #100691 ) ;
#51795 = CARTESIAN_POINT ( 'NONE',  ( 0.000000000000000000, 0.000000000000000000, 5.000000000000000000 ) ) ;
#51796 = CARTESIAN_POINT ( 'NONE',  ( 78.66209685856479439, -5.291415217122919401, 3.054999999999997939 ) ) ;
#51797 = CARTESIAN_POINT ( 'NONE',  ( -8.816011393731004731, 28.73617430169781173, 5.000000000000000000 ) ) ;
#51798 = CARTESIAN_POINT ( 'NONE',  ( -51.18398860626899705, 28.73617430169823095, 5.000000000000000000 ) ) ;
#51799 = ORIENTED_EDGE ( 'NONE', *, *, #138459, .T. ) ;
#51800 = EDGE_LOOP ( 'NONE', ( #25400, #51047, #121685, #98069 ) ) ;
#51801 = CARTESIAN_POINT ( 'NONE',  ( -14.99999999999988809, 14.96639925780210412, 5.000000000000000000 ) ) ;
#51802 = SURFACE_STYLE_USAGE ( .BOTH. , #19853 ) ;
#51803 = ORIENTED_EDGE ( 'NONE', *, *, #60849, .F. ) ;
#51805 = EDGE_CURVE ( 'NONE', #133751, #3412, #129480, .T. ) ;
#51804 = AXIS2_PLACEMENT_3D ( 'NONE', #83191, #16469, #17887 ) ;
#51806 = ORIENTED_EDGE ( 'NONE', *, *, #129461, .T. ) ;
#51807 = EDGE_CURVE ( 'NONE', #69645, #20118, #51239, .T. ) ;
#51808 = CARTESIAN_POINT ( 'NONE',  ( -42.18398860626899705, 28.73617430169816700, 5.000000000000000000 ) ) ;
#51809 = EDGE_LOOP ( 'NONE', ( #138296, #83843, #35646, #59223 ) ) ;
#51810 = DIRECTION ( 'NONE',  ( -0.000000000000000000, 0.3543493200069153248, 0.9351131265310291818 ) ) ;
#51811 = ADVANCED_FACE ( 'NONE', ( #9686 ), #8239, .F. ) ;
#51812 = DIRECTION ( 'NONE',  ( -1.000000000000000000, -1.224606353822377258E-16, -0.000000000000000000 ) ) ;
#51813 = FACE_BOUND ( 'NONE', #90176, .T. ) ;
#51814 = EDGE_CURVE ( 'NONE', #14957, #38790, #49826, .T. ) ;
#51815 = CARTESIAN_POINT ( 'NONE',  ( -34.75611968250420603, -4.294349301475885561, 4.955485411084901592 ) ) ;
#51817 = ORIENTED_EDGE ( 'NONE', *, *, #21388, .F. ) ;
#51816 = CARTESIAN_POINT ( 'NONE',  ( 33.18398860626899705, 28.73617430169810305, 5.000000000000000000 ) ) ;
#51818 = CIRCLE ( 'NONE', #37951, 2.999999999999999112 ) ;
#51819 = SURFACE_STYLE_FILL_AREA ( #8949 ) ;
#51820 = APPLICATION_PROTOCOL_DEFINITION ( 'draft international standard', 'automotive_design', 1998, #139319 ) ;
#51821 = ORIENTED_EDGE ( 'NONE', *, *, #115101, .F. ) ;
#51822 = AXIS2_PLACEMENT_3D ( 'NONE', #57279, #136223, #68864 ) ;
#51823 = ORIENTED_EDGE ( 'NONE', *, *, #9039, .F. ) ;
#51824 = CARTESIAN_POINT ( 'NONE',  ( 86.09959685856478018, -6.109999999999997655, -1.637169565754160283 ) ) ;
#51825 = VERTEX_POINT ( 'NONE', #38920 ) ;
#51826 = PLANE ( 'NONE',  #61597 ) ;
#51827 = FACE_OUTER_BOUND ( 'NONE', #98779, .T. ) ;
#51828 = DIRECTION ( 'NONE',  ( 0.7071067811865487940, 0.7071067811865463515, 0.000000000000000000 ) ) ;
#51829 = VECTOR ( 'NONE', #80755, 1000.000000000000000 ) ;
#51830 = DIRECTION ( 'NONE',  ( -0.000000000000000000, -0.000000000000000000, 1.000000000000000000 ) ) ;
#51831 = DIRECTION ( 'NONE',  ( -0.000000000000000000, 0.000000000000000000, 1.000000000000000000 ) ) ;
#51832 = CARTESIAN_POINT ( 'NONE',  ( 3.005480084712505828, 28.92564299267936079, 4.000000000000000000 ) ) ;
#51833 = CIRCLE ( 'NONE', #40260, 2.256103126841972895 ) ;
#51834 = DIRECTION ( 'NONE',  ( -0.7071067811865486830, -0.7071067811865464625, 0.000000000000000000 ) ) ;
#51835 = CARTESIAN_POINT ( 'NONE',  ( 21.48921356237309155, -27.52281430457070499, 5.000000000000000000 ) ) ;
#51836 = CARTESIAN_POINT ( 'NONE',  ( 180.8471172286433273, -48.98543874033772738, -39.51758185027073011 ) ) ;
#51837 = PLANE ( 'NONE',  #130274 ) ;
#51838 = ORIENTED_EDGE ( 'NONE', *, *, #11688, .F. ) ;
#51839 = CARTESIAN_POINT ( 'NONE',  ( -3.183988606268992161, 28.73617430169789699, 5.000000000000000000 ) ) ;
#51840 = CARTESIAN_POINT ( 'NONE',  ( -27.69326993309582008, -3.740707523384241728, 12.88036043432873967 ) ) ;
#51841 = ORIENTED_EDGE ( 'NONE', *, *, #3693, .T. ) ;
#51842 = EDGE_LOOP ( 'NONE', ( #24447, #31586, #89923, #29660 ) ) ;
#51843 = AXIS2_PLACEMENT_3D ( 'NONE', #26889, #71135, #86289 ) ;
#51844 = ORIENTED_EDGE ( 'NONE', *, *, #14016, .T. ) ;
#51845 = CARTESIAN_POINT ( 'NONE',  ( 34.85459685856477563, -1.637169565754161615, 6.110000000000000320 ) ) ;
#51846 = VERTEX_POINT ( 'NONE', #104883 ) ;
#51847 = VECTOR ( 'NONE', #28727, 1000.000000000000000 ) ;
#51848 = PLANE ( 'NONE',  #53305 ) ;
#51849 = VECTOR ( 'NONE', #111547, 999.9999999999998863 ) ;
#51850 = ADVANCED_FACE ( 'NONE', ( #83143 ), #28771, .F. ) ;
#51851 = VECTOR ( 'NONE', #14569, 1000.000000000000000 ) ;
#51852 = CARTESIAN_POINT ( 'NONE',  ( 19.29580628287044064, -5.278424836066144543, 3.047499999999995879 ) ) ;
#51853 =( BOUNDED_CURVE ( )  B_SPLINE_CURVE ( 2, ( #54044, #53275, #304, #33008, #76496, #119936, #9776, #109813, #97489, #58157, #54737, #22759, #64178 ),
 .UNSPECIFIED., .F., .T. ) 
 B_SPLINE_CURVE_WITH_KNOTS ( ( 3, 2, 2, 2, 2, 2, 3 ),
 ( 0.2999999999999999889, 0.3027777777777777568, 0.3055555555555555802, 0.3083333333333333481, 0.3111111111111111160, 0.3138888888888888840, 0.3166666666666666519 ),
 .UNSPECIFIED. ) 
 CURVE ( )  GEOMETRIC_REPRESENTATION_ITEM ( )  RATIONAL_B_SPLINE_CURVE ( ( 1.000000000000000000, 0.9659258262890683122, 1.000000000000000000, 0.9659258262890683122, 1.000000000000000000, 0.9659258262890683122, 1.000000000000000000, 0.9659258262890683122, 1.000000000000000000, 0.9659258262890683122, 1.000000000000000000, 0.9659258262890683122, 1.000000000000000000 ) ) 
 REPRESENTATION_ITEM ( '' )  );
#51854 = CARTESIAN_POINT ( 'NONE',  ( 12.81928177610584640, 7.016045820313829395, -30.84182252500521315 ) ) ;
#51855 = EDGE_CURVE ( 'NONE', #45746, #107805, #71560, .T. ) ;
#51856 = EDGE_LOOP ( 'NONE', ( #16586, #89380, #143439, #72406 ) ) ;
#51857 = ADVANCED_FACE ( 'NONE', ( #18555 ), #70856, .T. ) ;
#51858 = DIRECTION ( 'NONE',  ( 0.3543493200069162685, -0.000000000000000000, -0.9351131265310288487 ) ) ;
#51860 = ORIENTED_EDGE ( 'NONE', *, *, #53136, .F. ) ;
#51859 = EDGE_CURVE ( 'NONE', #94800, #63599, #4802, .T. ) ;
#51861 = DIRECTION ( 'NONE',  ( 1.000000000000000000, 0.000000000000000000, 0.000000000000000000 ) ) ;
#51862 = VECTOR ( 'NONE', #62084, 1000.000000000000227 ) ;
#51863 = DIRECTION ( 'NONE',  ( 0.000000000000000000, 0.000000000000000000, 1.000000000000000000 ) ) ;
#51865 = VERTEX_POINT ( 'NONE', #15686 ) ;
#51864 = DIRECTION ( 'NONE',  ( 0.6830127018922181881, 0.6830127018922202975, -0.2588190451025214056 ) ) ;
#51866 = ORIENTED_EDGE ( 'NONE', *, *, #115191, .T. ) ;
#51867 = EDGE_CURVE ( 'NONE', #71156, #113103, #138962, .T. ) ;
#51868 = DIRECTION ( 'NONE',  ( 0.5735764363510453823, -0.8191520442889923537, 1.003171929053525486E-16 ) ) ;
#51869 = ORIENTED_EDGE ( 'NONE', *, *, #140266, .F. ) ;
#51870 = DIRECTION ( 'NONE',  ( 0.000000000000000000, -1.000000000000000000, 0.000000000000000000 ) ) ;
#51871 = ORIENTED_EDGE ( 'NONE', *, *, #75588, .F. ) ;
#51872 = ORIENTED_EDGE ( 'NONE', *, *, #37156, .T. ) ;
#51873 = ORIENTED_EDGE ( 'NONE', *, *, #79857, .F. ) ;
#51874 = EDGE_CURVE ( 'NONE', #50240, #108415, #60716, .T. ) ;
#51875 = CARTESIAN_POINT ( 'NONE',  ( 30.18398860626900060, 28.73617430169808173, 5.000000000000000000 ) ) ;
#51876 = VECTOR ( 'NONE', #90569, 1000.000000000000000 ) ;
#51877 = FACE_OUTER_BOUND ( 'NONE', #61438, .T. ) ;
#51878 = DIRECTION ( 'NONE',  ( -0.7071067811865487940, 0.7071067811865463515, 0.000000000000000000 ) ) ;
#51879 = ADVANCED_FACE ( 'NONE', ( #105574 ), #6235, .F. ) ;
#51880 = CARTESIAN_POINT ( 'NONE',  ( -2.671830600776447184, 14.25929247661557397, 4.000000000000000000 ) ) ;
#51881 = DIRECTION ( 'NONE',  ( -0.7071067811865487940, 0.7071067811865463515, -0.000000000000000000 ) ) ;
#51882 = EDGE_CURVE ( 'NONE', #133731, #124530, #117168, .T. ) ;
#51883 = ORIENTED_EDGE ( 'NONE', *, *, #99478, .F. ) ;
#51884 = DIRECTION ( 'NONE',  ( -0.000000000000000000, 0.3543493200069153248, 0.9351131265310292928 ) ) ;
#51885 = VERTEX_POINT ( 'NONE', #383 ) ;
#51886 = CARTESIAN_POINT ( 'NONE',  ( 23.99999999999983302, 13.93112307739204425, 4.000000000000000000 ) ) ;
#51887 = ADVANCED_FACE ( 'NONE', ( #75149 ), #109880, .F. ) ;
#51888 = CARTESIAN_POINT ( 'NONE',  ( 32.06206980810188867, -7.934999999999991616, -2.126176841940955242 ) ) ;
#51889 = PLANE ( 'NONE',  #124955 ) ;
#51891 = EDGE_LOOP ( 'NONE', ( #99755, #32320, #36205, #95859 ) ) ;
#51890 = AXIS2_PLACEMENT_3D ( 'NONE', #91956, #123902, #14405 ) ;
#51892 = CARTESIAN_POINT ( 'NONE',  ( -29.29289321881324426, -9.740707523384182664, 5.000000000000000000 ) ) ;
#51893 = ORIENTED_EDGE ( 'NONE', *, *, #95529, .F. ) ;
#51894 = VERTEX_POINT ( 'NONE', #21454 ) ;
#51895 = EDGE_LOOP ( 'NONE', ( #72517, #33674, #73442, #54590, #51642 ) ) ;
#51896 = FACE_OUTER_BOUND ( 'NONE', #53848, .T. ) ;
#51897 = CARTESIAN_POINT ( 'NONE',  ( -26.99451991528749417, 28.92564299267956685, 4.000000000000000000 ) ) ;
#51898 = CARTESIAN_POINT ( 'NONE',  ( -30.48921356237309510, -27.52281430457076894, 5.000000000000000000 ) ) ;
#51899 = CARTESIAN_POINT ( 'NONE',  ( 69.48921356237309510, -27.52281430457103895, 5.000000000000000000 ) ) ;
#51900 = CARTESIAN_POINT ( 'NONE',  ( 3.010427959778297691, -48.08977582060965261, -37.49964900842701354 ) ) ;
#51901 = CARTESIAN_POINT ( 'NONE',  ( 72.39126352523145158, -4.472830434245839371, -4.472830434245839371 ) ) ;
#51902 = CARTESIAN_POINT ( 'NONE',  ( -5.671830600776424092, -12.74070752338414891, 4.000000000000000000 ) ) ;
#51903 = CARTESIAN_POINT ( 'NONE',  ( 57.48921356237308800, -27.52281430457095368, 5.000000000000000000 ) ) ;
#51904 = DIRECTION ( 'NONE',  ( 0.7071067811865487940, 0.7071067811865463515, -0.000000000000000000 ) ) ;
#51905 = DIRECTION ( 'NONE',  ( -0.7071067811865486830, 0.7071067811865464625, 0.000000000000000000 ) ) ;
#51906 = ORIENTED_EDGE ( 'NONE', *, *, #135838, .T. ) ;
#51907 = DIRECTION ( 'NONE',  ( 1.000000000000000000, 0.000000000000000000, 0.000000000000000000 ) ) ;
#51908 = EDGE_CURVE ( 'NONE', #26241, #132436, #76569, .T. ) ;
#51909 = ORIENTED_EDGE ( 'NONE', *, *, #89786, .F. ) ;
#51910 = CARTESIAN_POINT ( 'NONE',  ( -10.82334089840020930, 5.259292476615665457, 15.86257073897100511 ) ) ;
#51911 = LINE ( 'NONE', #30127, #36031 ) ;
#51912 = ORIENTED_EDGE ( 'NONE', *, *, #129229, .F. ) ;
#51913 = CARTESIAN_POINT ( 'NONE',  ( -8.999999999999937828, -5.527737879153202805, -7.983877177622351162 ) ) ;
#51915 = ORIENTED_EDGE ( 'NONE', *, *, #70876, .F. ) ;
#51914 = LINE ( 'NONE', #39619, #30265 ) ;
#51916 = DIRECTION ( 'NONE',  ( -0.7071067811865486830, -0.7071067811865464625, 0.000000000000000000 ) ) ;
#51917 = DIRECTION ( 'NONE',  ( 0.3543493200069162685, -0.000000000000000000, -0.9351131265310288487 ) ) ;
#51918 = ORIENTED_EDGE ( 'NONE', *, *, #95529, .T. ) ;
#51919 = EDGE_LOOP ( 'NONE', ( #17478, #99688, #92565 ) ) ;
#51920 = PLANE ( 'NONE',  #6972 ) ;
#51921 = LINE ( 'NONE', #86692, #88448 ) ;
#51922 = AXIS2_PLACEMENT_3D ( 'NONE', #38111, #138849, #127225 ) ;
#51923 = CARTESIAN_POINT ( 'NONE',  ( -33.75860074219772855, 21.72500000000000142, 5.000000000000000000 ) ) ;
#51924 = EDGE_CURVE ( 'NONE', #139982, #16938, #65717, .T. ) ;
#51925 = CARTESIAN_POINT ( 'NONE',  ( 97.49586038379624142, -3.974999999999998312, -6.884901960086286188 ) ) ;
#51926 = CARTESIAN_POINT ( 'NONE',  ( 0.000000000000000000, 0.000000000000000000, 6.349999999999997868 ) ) ;
#51927 = AXIS2_PLACEMENT_3D ( 'NONE', #14983, #61920, #80284 ) ;
#51928 = FACE_OUTER_BOUND ( 'NONE', #53569, .T. ) ;
#51929 = ORIENTED_EDGE ( 'NONE', *, *, #137788, .F. ) ;
#51930 = CARTESIAN_POINT ( 'NONE',  ( -20.99451991528748707, 28.92564299267952777, 4.000000000000000000 ) ) ;
#51931 = ADVANCED_FACE ( 'NONE', ( #20718 ), #22139, .F. ) ;
#51932 = DIRECTION ( 'NONE',  ( -1.000000000000000000, -1.224606353822377258E-16, -0.000000000000000000 ) ) ;
#51933 = CARTESIAN_POINT ( 'NONE',  ( 33.39583333333333570, 1.633150327867687324, -6.094999999999991758 ) ) ;
#51934 = CARTESIAN_POINT ( 'NONE',  ( 14.67183060077636725, -12.74070752338415069, 4.000000000000000000 ) ) ;
#51935 = ORIENTED_EDGE ( 'NONE', *, *, #38303, .T. ) ;
#51936 = DIRECTION ( 'NONE',  ( -0.7071067811865487940, 0.7071067811865463515, 0.000000000000000000 ) ) ;
#51937 = ORIENTED_EDGE ( 'NONE', *, *, #405, .T. ) ;
#51938 = AXIS2_PLACEMENT_3D ( 'NONE', #3512, #47804, #82540 ) ;
#51939 = ADVANCED_FACE ( 'NONE', ( #31618 ), #64245, .F. ) ;
#51940 = CARTESIAN_POINT ( 'NONE',  ( 81.52126352523141861, -4.472830434245839371, -4.472830434245840259 ) ) ;
#51941 = CARTESIAN_POINT ( 'NONE',  ( 6.183988606268994381, 28.73617430169791476, 5.000000000000000000 ) ) ;
#51942 = CARTESIAN_POINT ( 'NONE',  ( 52.60764783923754351, -49.05583548141699168, -39.86617647058817937 ) ) ;
#51943 = VERTEX_POINT ( 'NONE', #142531 ) ;
#51944 = CARTESIAN_POINT ( 'NONE',  ( -4.499999999999972466, 21.05218569542895679, 5.000000000000000000 ) ) ;
#51945 = DIRECTION ( 'NONE',  ( -0.6830127018922181881, 0.6830127018922202975, -0.2588190451025214056 ) ) ;
#51946 = VECTOR ( 'NONE', #87867, 1000.000000000000000 ) ;
#51947 = CARTESIAN_POINT ( 'NONE',  ( -7.940000000000007496, -39.92999999999999261, -10.00000000000000178 ) ) ;
#51948 = EDGE_CURVE ( 'NONE', #83415, #92406, #64976, .T. ) ;
#51950 = VERTEX_POINT ( 'NONE', #88870 ) ;
#51949 = LINE ( 'NONE', #118607, #77591 ) ;
#51951 = CARTESIAN_POINT ( 'NONE',  ( -39.18398860626899705, 28.73617430169814568, 5.000000000000000000 ) ) ;
#51952 = CARTESIAN_POINT ( 'NONE',  ( 1.500000000000000000, 3.812371101874758372E-16, -3.113037248396092416 ) ) ;
#51953 = CARTESIAN_POINT ( 'NONE',  ( 1.649863965247968967, -3.804504390074225917, 5.216255841094045387 ) ) ;
#51954 = CARTESIAN_POINT ( 'NONE',  ( -38.99451991528749062, 28.92564299267965211, 4.000000000000000000 ) ) ;
#51955 = AXIS2_PLACEMENT_3D ( 'NONE', #19570, #108684, #42782 ) ;
#51956 = EDGE_LOOP ( 'NONE', ( #31503, #66467, #2812, #108028 ) ) ;
#51957 = ORIENTED_EDGE ( 'NONE', *, *, #133563, .T. ) ;
#51958 = CARTESIAN_POINT ( 'NONE',  ( 76.12543019189810423, 5.291415217122919401, 3.055000000000002824 ) ) ;
#51959 = AXIS2_PLACEMENT_3D ( 'NONE', #116221, #39390, #61182 ) ;
#51960 = ORIENTED_EDGE ( 'NONE', *, *, #26831, .F. ) ;
#51961 = DIRECTION ( 'NONE',  ( 0.3543493200069162685, -0.000000000000000000, -0.9351131265310288487 ) ) ;
#51962 = CARTESIAN_POINT ( 'NONE',  ( -19.00193056682084247, -22.22500000000000142, 4.500000000000000888 ) ) ;
#51963 = DIRECTION ( 'NONE',  ( 0.7071067811865487940, -0.7071067811865463515, 0.000000000000000000 ) ) ;
#51964 = DIRECTION ( 'NONE',  ( -0.7071067811865486830, -0.7071067811865464625, -0.000000000000000000 ) ) ;
#51965 = ORIENTED_EDGE ( 'NONE', *, *, #99024, .F. ) ;
#51966 = LINE ( 'NONE', #19323, #76931 ) ;
#51967 = CARTESIAN_POINT ( 'NONE',  ( 36.53752705046288440, -9.735942053221456900E-16, 7.949999999999998401 ) ) ;
#51968 = VERTEX_POINT ( 'NONE', #43218 ) ;
#51969 = ADVANCED_FACE ( 'NONE', ( #107726 ), #84515, .T. ) ;
#51970 = CARTESIAN_POINT ( 'NONE',  ( 19.49999999999985789, 1.030536316426522436, -5.498701923753846366 ) ) ;
#51971 = LINE ( 'NONE', #96149, #140492 ) ;
#51972 = CARTESIAN_POINT ( 'NONE',  ( 0.000000000000000000, 0.000000000000000000, 5.000000000000000000 ) ) ;
#51973 = ORIENTED_EDGE ( 'NONE', *, *, #122041, .T. ) ;
#51974 = ORIENTED_EDGE ( 'NONE', *, *, #119367, .F. ) ;
#51975 = ADVANCED_FACE ( 'NONE', ( #131650 ), #13396, .F. ) ;
#51976 = DIRECTION ( 'NONE',  ( 0.7071067811865487940, 0.7071067811865463515, -0.000000000000000000 ) ) ;
#51977 = ADVANCED_FACE ( 'NONE', ( #56964 ), #134508, .F. ) ;
#51978 = DIRECTION ( 'NONE',  ( 0.7071067811865487940, 0.7071067811865463515, 0.000000000000000000 ) ) ;
#51979 = FACE_OUTER_BOUND ( 'NONE', #70063, .T. ) ;
#51980 = CARTESIAN_POINT ( 'NONE',  ( 25.40000000000000568, -5.414183704902473693, -5.631019616293379215 ) ) ;
#51981 = CARTESIAN_POINT ( 'NONE',  ( -7.499999999999951150, -2.173586137069146051, -4.605770156576128649 ) ) ;
#51982 = CARTESIAN_POINT ( 'NONE',  ( -2.331532588401415307, -18.74070752338408496, 20.73178291233840298 ) ) ;
#51983 = CARTESIAN_POINT ( 'NONE',  ( 0.5743220282099938956, -0.6000000000000000888, 4.263778219380816914 ) ) ;
#51984 = ORIENTED_EDGE ( 'NONE', *, *, #52461, .F. ) ;
#51985 = ORIENTED_EDGE ( 'NONE', *, *, #10218, .T. ) ;
#51986 = EDGE_LOOP ( 'NONE', ( #34396, #116685, #17169, #82761 ) ) ;
#51987 = ORIENTED_EDGE ( 'NONE', *, *, #71017, .F. ) ;
#51988 = CARTESIAN_POINT ( 'NONE',  ( -18.29974487139159223, -27.71228299555219010, 4.000000000000000000 ) ) ;
#51989 = EDGE_CURVE ( 'NONE', #142104, #44292, #2517, .T. ) ;
#51990 = VECTOR ( 'NONE', #115980, 1000.000000000000000 ) ;
#51991 = CARTESIAN_POINT ( 'NONE',  ( 5.510786437626906675, -27.52281430457051314, 5.000000000000000000 ) ) ;
#51992 = VERTEX_POINT ( 'NONE', #124325 ) ;
#51993 = CARTESIAN_POINT ( 'NONE',  ( -24.48921356237309510, -27.52281430457072631, 5.000000000000000000 ) ) ;
#51994 = DIRECTION ( 'NONE',  ( 0.7071067811865486830, -0.7071067811865464625, -0.000000000000000000 ) ) ;
#51995 = CARTESIAN_POINT ( 'NONE',  ( 2.207106781186526590, -20.24070752338407431, 5.000000000000000000 ) ) ;
#51996 = LINE ( 'NONE', #60772, #18338 ) ;
#51997 = CARTESIAN_POINT ( 'NONE',  ( 27.00000000000001066, -5.997342894908404887, -3.744407088454140276 ) ) ;
#51998 = ORIENTED_EDGE ( 'NONE', *, *, #68123, .F. ) ;
#51999 = DIRECTION ( 'NONE',  ( -0.3543493200069162685, -0.000000000000000000, -0.9351131265310288487 ) ) ;
#52000 = CARTESIAN_POINT ( 'NONE',  ( 11.56505274454301357, 0.000000000000000000, 2.500000000000000444 ) ) ;
#52001 = EDGE_LOOP ( 'NONE', ( #77540, #15027, #77920, #123333 ) ) ;
#52002 = CARTESIAN_POINT ( 'NONE',  ( -27.18398860626900060, 28.73617430169806042, 5.000000000000000000 ) ) ;
#52003 = ORIENTED_EDGE ( 'NONE', *, *, #27940, .F. ) ;
#52004 = CARTESIAN_POINT ( 'NONE',  ( 24.48921356237309510, -27.52281430457072631, 5.000000000000000000 ) ) ;
#52005 = VERTEX_POINT ( 'NONE', #3244 ) ;
#52006 = CARTESIAN_POINT ( 'NONE',  ( 67.81293019189809002, -1.637169565754159617, -6.110000000000001208 ) ) ;
#52007 = VECTOR ( 'NONE', #127805, 1000.000000000000000 ) ;
#52008 = ORIENTED_EDGE ( 'NONE', *, *, #72900, .T. ) ;
#52009 = EDGE_LOOP ( 'NONE', ( #103572, #125944, #108718, #61592 ) ) ;
#52010 = LINE ( 'NONE', #96194, #129860 ) ;
#52011 = VECTOR ( 'NONE', #124837, 1000.000000000000000 ) ;
#52012 = EDGE_CURVE ( 'NONE', #16132, #36659, #62309, .T. ) ;
#52013 = DIRECTION ( 'NONE',  ( -0.000000000000000000, 0.3543493200069153248, 0.9351131265310292928 ) ) ;
#52014 = CARTESIAN_POINT ( 'NONE',  ( 97.85459685856477563, -1.637169565754161615, 6.110000000000000320 ) ) ;
#52015 = CARTESIAN_POINT ( 'NONE',  ( -6.489213562373093325, -27.52281430457059841, 5.000000000000000000 ) ) ;
#52016 = EDGE_CURVE ( 'NONE', #62936, #80963, #123647, .T. ) ;
#52017 = AXIS2_PLACEMENT_3D ( 'NONE', #75637, #9628, #21243 ) ;
#52018 = CARTESIAN_POINT ( 'NONE',  ( 74.99451991528749772, 28.92564299267990435, 4.000000000000000000 ) ) ;
#52019 = DIRECTION ( 'NONE',  ( 0.7071067811865486830, -0.7071067811865464625, -0.000000000000000000 ) ) ;
#52020 = FACE_OUTER_BOUND ( 'NONE', #40710, .T. ) ;
#52021 = EDGE_CURVE ( 'NONE', #73316, #59163, #102596, .T. ) ;
#52022 = EDGE_CURVE ( 'NONE', #135619, #10069, #80144, .T. ) ;
#52023 = CARTESIAN_POINT ( 'NONE',  ( 14.99999999999990941, 11.58746187583913034, 4.000000000000000000 ) ) ;
#52024 = DIRECTION ( 'NONE',  ( 0.000000000000000000, -1.000000000000000000, 0.000000000000000000 ) ) ;
#52025 = ORIENTED_EDGE ( 'NONE', *, *, #88274, .F. ) ;
#52026 = CARTESIAN_POINT ( 'NONE',  ( -34.49999999999975131, 11.52377502935399889, -1.522421517564005899 ) ) ;
#52027 = VECTOR ( 'NONE', #125887, 999.9999999999998863 ) ;
#52028 = ORIENTED_EDGE ( 'NONE', *, *, #19235, .T. ) ;
#52029 = ORIENTED_EDGE ( 'NONE', *, *, #44575, .F. ) ;
#52030 = ORIENTED_EDGE ( 'NONE', *, *, #134532, .T. ) ;
#52031 = ORIENTED_EDGE ( 'NONE', *, *, #82155, .F. ) ;
#52032 = DIRECTION ( 'NONE',  ( 0.000000000000000000, 0.000000000000000000, -1.000000000000000000 ) ) ;
#52033 = CARTESIAN_POINT ( 'NONE',  ( -20.67183060077632817, -15.74070752338412404, 4.000000000000000000 ) ) ;
#52034 = ADVANCED_FACE ( 'NONE', ( #47534 ), #46826, .T. ) ;
#52035 = PLANE ( 'NONE',  #13887 ) ;
#52036 = ADVANCED_FACE ( 'NONE', ( #91694 ), #91013, .F. ) ;
#52037 = ORIENTED_EDGE ( 'NONE', *, *, #35581, .T. ) ;
#52038 = CARTESIAN_POINT ( 'NONE',  ( 0.3619179557511837397, -48.99280962439293319, 39.49606053969938557 ) ) ;
#52039 = VERTEX_POINT ( 'NONE', #100443 ) ;
#52040 = ADVANCED_FACE ( 'NONE', ( #14842 ), #35924, .F. ) ;
#52041 = CONICAL_SURFACE ( 'NONE', #142398, 2.055000000000001048, 0.9599310885968758145 ) ;
#52042 = AXIS2_PLACEMENT_3D ( 'NONE', #93589, #115285, #60267 ) ;
#52043 = CARTESIAN_POINT ( 'NONE',  ( 0.9995698081018860037, -3.967499999999998028, -6.871911579029511330 ) ) ;
#52044 = LINE ( 'NONE', #26713, #79477 ) ;
#52045 = DIRECTION ( 'NONE',  ( -0.7071067811865486830, -0.7071067811865464625, -0.000000000000000000 ) ) ;
#52046 = VECTOR ( 'NONE', #136842, 1000.000000000000000 ) ;
#52047 = CARTESIAN_POINT ( 'NONE',  ( -33.18398860626899705, 28.73617430169810305, 5.000000000000000000 ) ) ;
#52048 = ORIENTED_EDGE ( 'NONE', *, *, #73753, .F. ) ;
#52049 = ORIENTED_EDGE ( 'NONE', *, *, #52798, .F. ) ;
#52050 = EDGE_LOOP ( 'NONE', ( #53443, #142866, #58961, #39757 ) ) ;
#52051 = DIRECTION ( 'NONE',  ( 0.000000000000000000, -1.000000000000000000, 0.000000000000000000 ) ) ;
#52052 = CARTESIAN_POINT ( 'NONE',  ( -34.92499999999997584, -21.76999999999999247, -0.5000000000000000000 ) ) ;
#52053 = ADVANCED_FACE ( 'NONE', ( #25722 ), #114160, .F. ) ;
#52054 = LINE ( 'NONE', #51346, #12602 ) ;
#52055 = DIRECTION ( 'NONE',  ( -0.7071067811865487940, 0.7071067811865463515, 0.000000000000000000 ) ) ;
#52056 = DIRECTION ( 'NONE',  ( -0.6830127018922181881, 0.6830127018922202975, -0.2588190451025214056 ) ) ;
#52057 = FACE_OUTER_BOUND ( 'NONE', #25082, .T. ) ;
#52058 = CARTESIAN_POINT ( 'NONE',  ( 51.18398860626899705, 28.73617430169823095, 5.000000000000000000 ) ) ;
#52059 = CARTESIAN_POINT ( 'NONE',  ( 25.81293019189810778, -1.637169565754159617, -6.110000000000001208 ) ) ;
#52060 = FILL_AREA_STYLE_COLOUR ( '', #136913 ) ;
#52061 = ORIENTED_EDGE ( 'NONE', *, *, #114565, .F. ) ;
#52062 = FACE_OUTER_BOUND ( 'NONE', #52110, .T. ) ;
#52063 = EDGE_CURVE ( 'NONE', #126052, #50012, #22834, .T. ) ;
#52064 = DIRECTION ( 'NONE',  ( 1.000000000000000000, 0.000000000000000000, 0.000000000000000000 ) ) ;
#52065 = ORIENTED_EDGE ( 'NONE', *, *, #88593, .T. ) ;
#52066 = CARTESIAN_POINT ( 'NONE',  ( -4.171830600776436526, -2.240707523384257716, 4.000000000000000000 ) ) ;
#52068 = ORIENTED_EDGE ( 'NONE', *, *, #74053, .T. ) ;
#52067 = LINE ( 'NONE', #30307, #141416 ) ;
#52069 = DIRECTION ( 'NONE',  ( 0.7071067811865486830, -0.7071067811865464625, -0.000000000000000000 ) ) ;
#52070 = EDGE_CURVE ( 'NONE', #113191, #121130, #67104, .T. ) ;
#52071 = DIRECTION ( 'NONE',  ( 0.000000000000000000, -0.3543493200069152138, 0.9351131265310292928 ) ) ;
#52072 = ORIENTED_EDGE ( 'NONE', *, *, #108289, .T. ) ;
#52073 = CARTESIAN_POINT ( 'NONE',  ( 3.250000000000000000, 4.999999999999997335, -7.627214432543508948 ) ) ;
#52074 = UNCERTAINTY_MEASURE_WITH_UNIT (LENGTH_MEASURE( 1.000000000000000082E-05 ), #53104, 'distance_accuracy_value', 'NONE');
#52075 = ORIENTED_EDGE ( 'NONE', *, *, #75822, .F. ) ;
#52076 = CARTESIAN_POINT ( 'NONE',  ( -14.33153258840134292, -18.74070752338409207, 20.73178291233837811 ) ) ;
#52077 = EDGE_CURVE ( 'NONE', #19525, #21831, #43772, .T. ) ;
#52078 = CARTESIAN_POINT ( 'NONE',  ( 119.9541937171295700, 6.884901960086283523, 3.975000000000002753 ) ) ;
#52079 = LINE ( 'NONE', #65854, #29962 ) ;
#52080 = FACE_OUTER_BOUND ( 'NONE', #6379, .T. ) ;
#52081 = CARTESIAN_POINT ( 'NONE',  ( 24.47336096364199420, -5.240707523384228850, 16.25846745537501548 ) ) ;
#52082 = LINE ( 'NONE', #140503, #34472 ) ;
#52083 = CARTESIAN_POINT ( 'NONE',  ( 7.437500000000000000, -4.461849672132299105, 4.461849672132299993 ) ) ;
#52084 = CARTESIAN_POINT ( 'NONE',  ( 12.95790314143521904, 6.871911579029515771, 3.967499999999989146 ) ) ;
#52085 = CARTESIAN_POINT ( 'NONE',  ( 23.63159235450331863, 9.902892378096218942E-16, 0.000000000000000000 ) ) ;
#52086 = LINE ( 'NONE', #39067, #64055 ) ;
#52087 = EDGE_LOOP ( 'NONE', ( #56039, #82798, #78565, #72947, #10243 ) ) ;
#52088 = VERTEX_POINT ( 'NONE', #24302 ) ;
#52089 = EDGE_LOOP ( 'NONE', ( #64005, #78869, #52463, #15085 ) ) ;
#52090 = LINE ( 'NONE', #96268, #129063 ) ;
#52091 = LINE ( 'NONE', #65868, #78636 ) ;
#52092 = CARTESIAN_POINT ( 'NONE',  ( 0.000000000000000000, -4.870000000000014317, 500000.0000000000582 ) ) ;
#52093 = CARTESIAN_POINT ( 'NONE',  ( 29.53752705046289151, -9.735942053221456900E-16, 7.949999999999998401 ) ) ;
#52094 = ORIENTED_EDGE ( 'NONE', *, *, #58339, .T. ) ;
#52095 = CARTESIAN_POINT ( 'NONE',  ( 18.18398860626898994, 28.73617430169800002, 5.000000000000000000 ) ) ;
#52096 = LINE ( 'NONE', #74584, #102113 ) ;
#52097 = CARTESIAN_POINT ( 'NONE',  ( -12.69999999999998153, 0.000000000000000000, 2.500000000000000444 ) ) ;
#52098 = CARTESIAN_POINT ( 'NONE',  ( 0.3394530118782065897, -51.90335959434332835, 39.28179725402794276 ) ) ;
#52100 = ORIENTED_EDGE ( 'NONE', *, *, #41368, .F. ) ;
#52099 = LINE ( 'NONE', #30346, #19706 ) ;
#52101 = CARTESIAN_POINT ( 'NONE',  ( 40.52083333333332860, 7.949999999999998401, 2.130196079827431532 ) ) ;
#52102 = FILL_AREA_STYLE ('',( #10707 ) ) ;
#52103 = CARTESIAN_POINT ( 'NONE',  ( -19.02459472929562878, 22.22500000000000142, 11.02525794543162263 ) ) ;
#52104 = CARTESIAN_POINT ( 'NONE',  ( 0.000000000000000000, 0.000000000000000000, 5.000000000000000000 ) ) ;
#52105 = CARTESIAN_POINT ( 'NONE',  ( 0.000000000000000000, 0.000000000000000000, 5.000000000000000000 ) ) ;
#52106 = CARTESIAN_POINT ( 'NONE',  ( 58.54058136200207230, -46.07581969935849742, 35.63601533998080839 ) ) ;
#52107 = ORIENTED_EDGE ( 'NONE', *, *, #28548, .F. ) ;
#52108 = AXIS2_PLACEMENT_3D ( 'NONE', #110034, #56441, #45547 ) ;
#52109 = ORIENTED_EDGE ( 'NONE', *, *, #75762, .T. ) ;
#52110 = EDGE_LOOP ( 'NONE', ( #90592, #127318, #57001, #33733 ) ) ;
#52111 = CARTESIAN_POINT ( 'NONE',  ( 104.7087635252314328, -7.482591942790329030E-16, 6.110000000000001208 ) ) ;
#52112 = ORIENTED_EDGE ( 'NONE', *, *, #33371, .T. ) ;
#52113 = VECTOR ( 'NONE', #12150, 1000.000000000000000 ) ;
#52114 = CARTESIAN_POINT ( 'NONE',  ( 124.7734390271609328, -44.54322672567447228, 35.04755940937926084 ) ) ;
#52115 = LINE ( 'NONE', #74605, #6332 ) ;
#52116 = ORIENTED_EDGE ( 'NONE', *, *, #13493, .F. ) ;
#52117 = PLANE ( 'NONE',  #74531 ) ;
#52119 =( BOUNDED_CURVE ( )  B_SPLINE_CURVE ( 2, ( #60181, #104356, #5021, #49319, #93506, #18778, #73898, #117366, #52136, #40564, #118066, #128979, #129684 ),
 .UNSPECIFIED., .F., .F. ) 
 B_SPLINE_CURVE_WITH_KNOTS ( ( 3, 2, 2, 2, 2, 2, 3 ),
 ( 0.6000000000000000888, 0.6083333333333333925, 0.6166666666666668073, 0.6250000000000001110, 0.6333333333333334147, 0.6416666666666668295, 0.6500000000000001332 ),
 .UNSPECIFIED. ) 
 CURVE ( )  GEOMETRIC_REPRESENTATION_ITEM ( )  RATIONAL_B_SPLINE_CURVE ( ( 0.9999999999999995559, 0.9659258262890687563, 1.000000000000000000, 0.9659258262890683122, 1.000000000000000000, 0.9659258262890683122, 1.000000000000000000, 0.9659258262890683122, 1.000000000000000000, 0.9659258262890683122, 1.000000000000000000, 0.9659258262890678681, 1.000000000000000444 ) ) 
 REPRESENTATION_ITEM ( '' )  );
#52118 = PLANE ( 'NONE',  #118316 ) ;
#52120 = CARTESIAN_POINT ( 'NONE',  ( 99.66209685856478018, -5.291415217122919401, 3.054999999999997939 ) ) ;
#52121 = CIRCLE ( 'NONE', #77608, 2.500000000000000888 ) ;
#52122 = ORIENTED_EDGE ( 'NONE', *, *, #67754, .F. ) ;
#52123 = VECTOR ( 'NONE', #39300, 1000.000000000000000 ) ;
#52124 = CARTESIAN_POINT ( 'NONE',  ( -57.48921356237308800, -27.52281430457095368, 5.000000000000000000 ) ) ;
#52125 = CARTESIAN_POINT ( 'NONE',  ( 30.18398860626900060, 28.73617430169808173, 5.000000000000000000 ) ) ;
#52126 = DIRECTION ( 'NONE',  ( 0.7071067811865487940, 0.7071067811865463515, -0.000000000000000000 ) ) ;
#52127 = CARTESIAN_POINT ( 'NONE',  ( 30.81349135397619676, -15.74070752338412760, 8.904080028138867675 ) ) ;
#52128 = ORIENTED_EDGE ( 'NONE', *, *, #4292, .T. ) ;
#52129 = EDGE_LOOP ( 'NONE', ( #57687, #41762, #109214, #25608 ) ) ;
#52130 = ADVANCED_FACE ( 'NONE', ( #34469 ), #64673, .T. ) ;
#52131 = ORIENTED_EDGE ( 'NONE', *, *, #63822, .T. ) ;
#52132 = CARTESIAN_POINT ( 'NONE',  ( 37.21321903303336143, 12.75929247661558996, 10.29404684609044018 ) ) ;
#52133 = ADVANCED_FACE ( 'NONE', ( #12691 ), #35209, .F. ) ;
#52134 = CARTESIAN_POINT ( 'NONE',  ( 31.82816939922330945, 9.759292476615621936, 4.000000000000000000 ) ) ;
#52135 = CARTESIAN_POINT ( 'NONE',  ( 9.692069808101887674, -7.934999999999990727, -2.126176841940955242 ) ) ;
#52136 = CARTESIAN_POINT ( 'NONE',  ( 22.16666666666666785, -5.278424836066145431, -3.047499999999993658 ) ) ;
#52137 = AXIS2_PLACEMENT_3D ( 'NONE', #65150, #42685, #10021 ) ;
#52139 = VECTOR ( 'NONE', #130858, 1000.000000000000000 ) ;
#52138 =( LENGTH_UNIT ( ) NAMED_UNIT ( * ) SI_UNIT ( .MILLI., .METRE. ) );
#52140 = EDGE_LOOP ( 'NONE', ( #1578, #111029, #58321, #79278, #138681 ) ) ;
#52143 = VERTEX_POINT ( 'NONE', #94533 ) ;
#52142 = EDGE_CURVE ( 'NONE', #73921, #75761, #38051, .T. ) ;
#52141 = AXIS2_PLACEMENT_3D ( 'NONE', #99652, #119707, #47242 ) ;
#52144 = VERTEX_POINT ( 'NONE', #5377 ) ;
#52145 = VERTEX_POINT ( 'NONE', #117694 ) ;
#52146 = EDGE_CURVE ( 'NONE', #47459, #109538, #115548, .T. ) ;
#52147 = DIRECTION ( 'NONE',  ( -0.000000000000000000, -0.3543493200069152693, 0.9351131265310292928 ) ) ;
#52148 = CARTESIAN_POINT ( 'NONE',  ( -4.499999999999966249, -16.53360074219757081, 5.000000000000000000 ) ) ;
#52149 = ORIENTED_EDGE ( 'NONE', *, *, #59628, .F. ) ;
#52150 = PLANE ( 'NONE',  #127017 ) ;
#52151 = DIRECTION ( 'NONE',  ( 0.000000000000000000, 1.000000000000000000, 0.000000000000000000 ) ) ;
#52152 = DIRECTION ( 'NONE',  ( 0.000000000000000000, 1.000000000000000000, 0.000000000000000000 ) ) ;
#52153 = LINE ( 'NONE', #97040, #101565 ) ;
#52154 = EDGE_CURVE ( 'NONE', #136489, #95449, #50347, .T. ) ;
#52155 = EDGE_CURVE ( 'NONE', #46584, #73005, #139528, .T. ) ;
#52156 = EDGE_LOOP ( 'NONE', ( #142644, #48032, #103961, #86913 ) ) ;
#52157 = CARTESIAN_POINT ( 'NONE',  ( -8.207106781186485733, 12.75929247661559351, 5.000000000000000000 ) ) ;
#52158 = FACE_BOUND ( 'NONE', #24947, .T. ) ;
#52159 = ORIENTED_EDGE ( 'NONE', *, *, #88105, .T. ) ;
#52160 = CARTESIAN_POINT ( 'NONE',  ( 34.49999999999975842, 19.46425560840029689, 4.994342998332160555 ) ) ;
#52161 = CARTESIAN_POINT ( 'NONE',  ( 19.49365931317388245, -0.02952910816523741239, -31.02252017457930577 ) ) ;
#52162 = LINE ( 'NONE', #107935, #134916 ) ;
#52163 = ORIENTED_EDGE ( 'NONE', *, *, #132488, .T. ) ;
#52164 = CARTESIAN_POINT ( 'NONE',  ( -30.29974487139158867, -27.71228299555227537, 4.000000000000000000 ) ) ;
#52165 = EDGE_LOOP ( 'NONE', ( #915, #14299, #12695, #110439, #19463, #53031 ) ) ;
#52166 = EDGE_LOOP ( 'NONE', ( #91588, #80910, #93340, #23574, #94598, #33502 ) ) ;
#52167 = ORIENTED_EDGE ( 'NONE', *, *, #133650, .F. ) ;
#52168 = CARTESIAN_POINT ( 'NONE',  ( 27.32876352523144803, 0.000000000000000000, -6.109999999999998543 ) ) ;
#52169 = FACE_OUTER_BOUND ( 'NONE', #14667, .T. ) ;
#52170 = DIRECTION ( 'NONE',  ( -0.6830127018922181881, 0.6830127018922202975, -0.2588190451025214056 ) ) ;
#52171 = CARTESIAN_POINT ( 'NONE',  ( 21.44840764549667611, 9.139736423841732040E-16, 0.000000000000000000 ) ) ;
#52172 = EDGE_CURVE ( 'NONE', #116772, #27223, #61270, .T. ) ;
#52173 = FACE_OUTER_BOUND ( 'NONE', #13104, .T. ) ;
#52174 = CARTESIAN_POINT ( 'NONE',  ( 22.07159235450331991, 2.500000000000001776, 0.000000000000000000 ) ) ;
#52175 = CARTESIAN_POINT ( 'NONE',  ( -56.99451991528749062, 28.92564299267978001, 4.000000000000000000 ) ) ;
#52176 = EDGE_CURVE ( 'NONE', #58880, #96438, #103972, .T. ) ;
#52177 = EDGE_CURVE ( 'NONE', #23024, #33945, #29288, .T. ) ;
#52178 = DIRECTION ( 'NONE',  ( -0.6830127018922181881, 0.6830127018922202975, -0.2588190451025214056 ) ) ;
#52179 = CARTESIAN_POINT ( 'NONE',  ( -34.45011844616455221, -11.99769585840591724, 5.000000000000000888 ) ) ;
#52180 = DIRECTION ( 'NONE',  ( -0.7071067811865487940, 0.7071067811865463515, 0.000000000000000000 ) ) ;
#52181 = ORIENTED_EDGE ( 'NONE', *, *, #35424, .F. ) ;
#52182 = VERTEX_POINT ( 'NONE', #137360 ) ;
#52183 = EDGE_LOOP ( 'NONE', ( #112218, #108199, #11980, #8512 ) ) ;
#52184 = VERTEX_POINT ( 'NONE', #104710 ) ;
#52185 = CARTESIAN_POINT ( 'NONE',  ( 30.15612307739221265, -22.22500000000000142, 4.000000000000000000 ) ) ;
#52186 = ORIENTED_EDGE ( 'NONE', *, *, #99245, .F. ) ;
#52187 = EDGE_CURVE ( 'NONE', #64560, #79180, #138793, .T. ) ;
#52188 = VERTEX_POINT ( 'NONE', #38749 ) ;
#52189 = DIRECTION ( 'NONE',  ( 1.000000000000000000, 0.000000000000000000, 0.000000000000000000 ) ) ;
#52190 = FACE_OUTER_BOUND ( 'NONE', #32858, .T. ) ;
#52191 = EDGE_CURVE ( 'NONE', #118217, #66142, #27865, .T. ) ;
#52192 = EDGE_CURVE ( 'NONE', #117439, #122913, #136617, .T. ) ;
#52193 = LINE ( 'NONE', #127628, #94812 ) ;
#52194 = ORIENTED_EDGE ( 'NONE', *, *, #142895, .T. ) ;
#52195 = CARTESIAN_POINT ( 'NONE',  ( -14.99999999999989342, -3.033600742197705369, 5.000000000000000000 ) ) ;
#52196 = ORIENTED_EDGE ( 'NONE', *, *, #91676, .T. ) ;
#52197 = DIRECTION ( 'NONE',  ( 0.000000000000000000, 0.000000000000000000, 1.000000000000000000 ) ) ;
#52198 = VECTOR ( 'NONE', #40893, 1000.000000000000000 ) ;
#52199 = CARTESIAN_POINT ( 'NONE',  ( 15.67180000000000639, 3.174999999999997602, 5.000000000000000000 ) ) ;
#52200 = EDGE_CURVE ( 'NONE', #89639, #89080, #126451, .T. ) ;
#52201 = CARTESIAN_POINT ( 'NONE',  ( 9.400403141435219823, -7.934999999999989839, 2.126176841940957907 ) ) ;
#52202 = ORIENTED_EDGE ( 'NONE', *, *, #94553, .F. ) ;
#52203 = CARTESIAN_POINT ( 'NONE',  ( 96.30793019189810877, -6.109999999999999432, 1.637169565754158507 ) ) ;
#52204 = EDGE_CURVE ( 'NONE', #63895, #119902, #81570, .T. ) ;
#52205 = DIRECTION ( 'NONE',  ( -0.000000000000000000, -0.3543493200069152693, 0.9351131265310292928 ) ) ;
#52206 = VECTOR ( 'NONE', #92399, 1000.000000000000000 ) ;
#52207 = LINE ( 'NONE', #53653, #111160 ) ;
#52208 = PLANE ( 'NONE',  #102085 ) ;
#52209 = ORIENTED_EDGE ( 'NONE', *, *, #70841, .F. ) ;
#52210 = EDGE_LOOP ( 'NONE', ( #135770, #104324, #133197, #84883 ) ) ;
#52211 = PLANE ( 'NONE',  #93643 ) ;
#52212 = EDGE_LOOP ( 'NONE', ( #122282, #83433, #82793, #41822, #134397 ) ) ;
#52213 = CARTESIAN_POINT ( 'NONE',  ( 0.000000000000000000, -49.85820393249939286, 34.92500000000001847 ) ) ;
#52214 = CARTESIAN_POINT ( 'NONE',  ( 23.99999999999983658, 14.96639925780211122, 5.000000000000000000 ) ) ;
#52215 = EDGE_CURVE ( 'NONE', #111091, #35748, #28602, .T. ) ;
#52216 = LINE ( 'NONE', #107305, #54354 ) ;
#52217 = CARTESIAN_POINT ( 'NONE',  ( -13.49999999999990052, -9.462702396501018853, -9.474982329943482995 ) ) ;
#52218 = EDGE_LOOP ( 'NONE', ( #51645, #75878, #65262, #111126 ) ) ;
#52219 = LINE ( 'NONE', #76866, #99263 ) ;
#52220 = VECTOR ( 'NONE', #78123, 999.9999999999998863 ) ;
#52221 = LINE ( 'NONE', #39960, #58267 ) ;
#52222 = CARTESIAN_POINT ( 'NONE',  ( -12.79289321881336328, 18.75929247661552068, 5.000000000000000000 ) ) ;
#52223 = ORIENTED_EDGE ( 'NONE', *, *, #125074, .F. ) ;
#52224 = DIRECTION ( 'NONE',  ( 0.000000000000000000, 0.000000000000000000, -1.000000000000000000 ) ) ;
#52225 = LINE ( 'NONE', #41337, #134911 ) ;
#52226 = VERTEX_POINT ( 'NONE', #73531 ) ;
#52228 = VERTEX_POINT ( 'NONE', #117012 ) ;
#52227 = DIRECTION ( 'NONE',  ( 0.7071067811865486830, -0.7071067811865464625, -0.000000000000000000 ) ) ;
#52229 = ORIENTED_EDGE ( 'NONE', *, *, #21298, .F. ) ;
#52230 = CARTESIAN_POINT ( 'NONE',  ( 20.99451991528748707, 28.92564299267952777, 4.000000000000000000 ) ) ;
#52232 = EDGE_CURVE ( 'NONE', #124219, #63953, #17679, .T. ) ;
#52231 = DIRECTION ( 'NONE',  ( 1.000000000000000000, -0.000000000000000000, 0.000000000000000000 ) ) ;
#52233 = EDGE_LOOP ( 'NONE', ( #106735, #60961, #92424, #72392 ) ) ;
#52234 = DIRECTION ( 'NONE',  ( 0.000000000000000000, -1.000000000000000000, 0.000000000000000000 ) ) ;
#52235 = VECTOR ( 'NONE', #11248, 1000.000000000000000 ) ;
#52236 = EDGE_CURVE ( 'NONE', #57178, #98347, #27148, .T. ) ;
#52237 = CARTESIAN_POINT ( 'NONE',  ( 1.042387978378689573, -0.3999999999999998002, -2.015694669338588429 ) ) ;
#52238 = EDGE_CURVE ( 'NONE', #115828, #119455, #49658, .T. ) ;
#52239 = VECTOR ( 'NONE', #28224, 999.9999999999998863 ) ;
#52240 = LINE ( 'NONE', #19608, #20648 ) ;
#52241 = VECTOR ( 'NONE', #13129, 1000.000000000000000 ) ;
#52242 = CARTESIAN_POINT ( 'NONE',  ( 21.79289321881331176, -20.24070752338407431, 5.000000000000000000 ) ) ;
#52243 = CARTESIAN_POINT ( 'NONE',  ( -16.50229999999999464, 3.130000000000007887, -2.396719511207313368E-16 ) ) ;
#52244 = CARTESIAN_POINT ( 'NONE',  ( -42.48921356237308800, -27.52281430457085065, 5.000000000000000000 ) ) ;
#52245 = DIRECTION ( 'NONE',  ( 0.3543493200069162685, -0.000000000000000000, -0.9351131265310288487 ) ) ;
#52246 = CARTESIAN_POINT ( 'NONE',  ( -31.49999999999977973, -7.912538124160673370, 4.000000000000000000 ) ) ;
#52247 = CARTESIAN_POINT ( 'NONE',  ( 8.292986735706890045, -21.74070752338406365, 4.999753212805221558 ) ) ;
#52248 = CARTESIAN_POINT ( 'NONE',  ( 42.48921356237308800, -27.52281430457085065, 5.000000000000000000 ) ) ;
#52249 = DIRECTION ( 'NONE',  ( -0.7071067811865486830, -0.7071067811865464625, 0.000000000000000000 ) ) ;
#52250 = EDGE_CURVE ( 'NONE', #121222, #33858, #93836, .T. ) ;
#52251 = CARTESIAN_POINT ( 'NONE',  ( 0.000000000000000000, 0.000000000000000000, 5.000000000000000000 ) ) ;
#52252 = ORIENTED_EDGE ( 'NONE', *, *, #68574, .F. ) ;
#52253 = EDGE_LOOP ( 'NONE', ( #39891, #105164, #64179, #53044 ) ) ;
#52254 = EDGE_LOOP ( 'NONE', ( #11083, #63103, #125840, #124047 ) ) ;
#52255 = CARTESIAN_POINT ( 'NONE',  ( 109.0625000000000000, -5.819803920172572198, -5.819803920172573086 ) ) ;
#52256 = ORIENTED_EDGE ( 'NONE', *, *, #86407, .F. ) ;
#52257 = EDGE_LOOP ( 'NONE', ( #127169, #70294, #49649, #83917 ) ) ;
#52258 = ORIENTED_EDGE ( 'NONE', *, *, #20545, .F. ) ;
#52259 = CARTESIAN_POINT ( 'NONE',  ( 25.39999999999999858, -2.600000000000013856, 20.40202195861968448 ) ) ;
#52260 = DIRECTION ( 'NONE',  ( -0.6830127018922180770, -0.6830127018922204085, -0.2588190451025213501 ) ) ;
#52261 = ORIENTED_EDGE ( 'NONE', *, *, #81942, .F. ) ;
#52262 = LINE ( 'NONE', #27645, #106332 ) ;
#52263 = CARTESIAN_POINT ( 'NONE',  ( -34.92500000000001137, -22.22500000000000142, 4.000000000000000000 ) ) ;
#52264 = LINE ( 'NONE', #117497, #132030 ) ;
#52265 = CARTESIAN_POINT ( 'NONE',  ( -18.18398860626898994, 28.73617430169800002, 5.000000000000000000 ) ) ;
#52266 = CARTESIAN_POINT ( 'NONE',  ( 100.7712635252314328, 4.472830434245839371, 4.472830434245842035 ) ) ;
#52267 = ORIENTED_EDGE ( 'NONE', *, *, #56005, .T. ) ;
#52268 = CARTESIAN_POINT ( 'NONE',  ( 11.29289321881338459, -3.740707523384243505, 5.000000000000000000 ) ) ;
#52269 =( NAMED_UNIT ( * ) SI_UNIT ( $, .STERADIAN. ) SOLID_ANGLE_UNIT ( ) );
#52270 = CARTESIAN_POINT ( 'NONE',  ( -15.56584921360887108, 8.021612662230191759, 4.000000000000000000 ) ) ;
#52271 = PLANE ( 'NONE',  #111834 ) ;
#52272 = LINE ( 'NONE', #140698, #93840 ) ;
#52273 = CARTESIAN_POINT ( 'NONE',  ( 3.250000000000000000, 0.000000000000000000, 4.999999999999998224 ) ) ;
#52274 = DIRECTION ( 'NONE',  ( 0.000000000000000000, -1.000000000000000000, 0.000000000000000000 ) ) ;
#52275 = DIRECTION ( 'NONE',  ( 0.7071067811865487940, 0.7071067811865463515, -0.000000000000000000 ) ) ;
#52276 = ORIENTED_EDGE ( 'NONE', *, *, #27556, .T. ) ;
#52277 = ORIENTED_EDGE ( 'NONE', *, *, #60727, .F. ) ;
#52278 = CARTESIAN_POINT ( 'NONE',  ( 27.83333333333332149, -6.884901960086287964, 3.974999999999998312 ) ) ;
#52279 = ORIENTED_EDGE ( 'NONE', *, *, #2155, .F. ) ;
#52280 = LINE ( 'NONE', #7329, #34783 ) ;
#52281 = EDGE_CURVE ( 'NONE', #106633, #56871, #22925, .T. ) ;
#52282 = DIRECTION ( 'NONE',  ( -1.000000000000000000, 0.000000000000000000, 0.000000000000000000 ) ) ;
#52283 = DIRECTION ( 'NONE',  ( -0.6830127018922180770, -0.6830127018922204085, -0.2588190451025213501 ) ) ;
#52284 = CARTESIAN_POINT ( 'NONE',  ( -3.005480084712505828, 28.92564299267936079, 4.000000000000000000 ) ) ;
#52285 = CARTESIAN_POINT ( 'NONE',  ( -17.29289321881333308, -12.74070752338415247, 5.000000000000000000 ) ) ;
#52286 = CARTESIAN_POINT ( 'NONE',  ( -30.32816939922332367, 20.25929247661551003, 4.000000000000000000 ) ) ;
#52287 = CARTESIAN_POINT ( 'NONE',  ( 121.3912635252314374, -4.472830434245839371, -4.472830434245839371 ) ) ;
#52288 = ORIENTED_EDGE ( 'NONE', *, *, #34345, .T. ) ;
#52289 = DIRECTION ( 'NONE',  ( -0.000000000000000000, 0.3543493200069152138, -0.9351131265310292928 ) ) ;
#52290 = ORIENTED_EDGE ( 'NONE', *, *, #106090, .F. ) ;
#52291 = DIRECTION ( 'NONE',  ( -0.3543493200069162685, -0.000000000000000000, -0.9351131265310288487 ) ) ;
#52292 = DIRECTION ( 'NONE',  ( 0.000000000000000000, 0.000000000000000000, 1.000000000000000000 ) ) ;
#52293 = CARTESIAN_POINT ( 'NONE',  ( 1.042387978378689573, 4.202752102959690472E-16, 0.000000000000000000 ) ) ;
#52294 = EDGE_CURVE ( 'NONE', #40982, #25852, #130784, .T. ) ;
#52295 = PLANE ( 'NONE',  #27913 ) ;
#52296 = ORIENTED_EDGE ( 'NONE', *, *, #109651, .F. ) ;
#52297 = CARTESIAN_POINT ( 'NONE',  ( 44.18793019189810423, 6.110000000000002984, -1.637169565754156730 ) ) ;
#52298 = EDGE_CURVE ( 'NONE', #74460, #56797, #53939, .T. ) ;
#52299 = ORIENTED_EDGE ( 'NONE', *, *, #81653, .T. ) ;
#52300 = DIRECTION ( 'NONE',  ( 0.3543493200069162685, -0.000000000000000000, -0.9351131265310288487 ) ) ;
#52301 = CARTESIAN_POINT ( 'NONE',  ( 6.291777089830439706, -15.74070752338412404, 19.73771281079099182 ) ) ;
#52302 = CARTESIAN_POINT ( 'NONE',  ( 11.24139925780195171, 21.72500000000000142, 5.000000000000000000 ) ) ;
#52303 = CARTESIAN_POINT ( 'NONE',  ( 35.90156419391741593, 11.25929247661559884, 10.79108189686415642 ) ) ;
#52304 =( BOUNDED_CURVE ( )  B_SPLINE_CURVE ( 2, ( #46765, #48144, #37261, #114103, #14787, #24934, #34404, #35143, #102536, #67791, #92324, #59060, #114785 ),
 .UNSPECIFIED., .F., .T. ) 
 B_SPLINE_CURVE_WITH_KNOTS ( ( 3, 2, 2, 2, 2, 2, 3 ),
 ( 0.5999999999999999778, 0.6027777777777777457, 0.6055555555555555136, 0.6083333333333332815, 0.6111111111111111605, 0.6138888888888889284, 0.6166666666666666963 ),
 .UNSPECIFIED. ) 
 CURVE ( )  GEOMETRIC_REPRESENTATION_ITEM ( )  RATIONAL_B_SPLINE_CURVE ( ( 1.000000000000000000, 0.9659258262890683122, 1.000000000000000000, 0.9659258262890683122, 1.000000000000000000, 0.9659258262890683122, 1.000000000000000000, 0.9659258262890683122, 1.000000000000000000, 0.9659258262890683122, 1.000000000000000000, 0.9659258262890683122, 1.000000000000000000 ) ) 
 REPRESENTATION_ITEM ( '' )  );
#52305 = EDGE_CURVE ( 'NONE', #107270, #127430, #19134, .T. ) ;
#52306 = EDGE_CURVE ( 'NONE', #79941, #124966, #87963, .T. ) ;
#52307 = AXIS2_PLACEMENT_3D ( 'NONE', #20025, #140397, #21485 ) ;
#52308 = CARTESIAN_POINT ( 'NONE',  ( 43.80793019189810877, -6.109999999999998543, 1.637169565754158063 ) ) ;
#52309 = ORIENTED_EDGE ( 'NONE', *, *, #68411, .T. ) ;
#52310 = EDGE_CURVE ( 'NONE', #42625, #6455, #131477, .T. ) ;
#52311 = CARTESIAN_POINT ( 'NONE',  ( -17.99999999999986855, -15.41253812416059965, 4.000000000000000000 ) ) ;
#52312 = ORIENTED_EDGE ( 'NONE', *, *, #65798, .T. ) ;
#52313 = ORIENTED_EDGE ( 'NONE', *, *, #19102, .T. ) ;
#52314 = ORIENTED_EDGE ( 'NONE', *, *, #92959, .F. ) ;
#52315 = ADVANCED_FACE ( 'NONE', ( #132205 ), #109712, .T. ) ;
#52316 = CARTESIAN_POINT ( 'NONE',  ( 25.49999999999982947, 22.22500000000000142, 4.362957392718778138 ) ) ;
#52317 = CARTESIAN_POINT ( 'NONE',  ( 79.70419371712955581, -6.884901960086285300, -3.975000000000000089 ) ) ;
#52318 = VERTEX_POINT ( 'NONE', #42343 ) ;
#52319 = CARTESIAN_POINT ( 'NONE',  ( 43.82919371712955581, -3.975000000000001865, 6.884901960086284411 ) ) ;
#52320 = AXIS2_PLACEMENT_3D ( 'NONE', #132354, #77258, #111252 ) ;
#52321 = DIRECTION ( 'NONE',  ( -0.5735764363510501562, 0.8191520442889890230, 1.003171929053521419E-16 ) ) ;
#52322 = EDGE_CURVE ( 'NONE', #12211, #44871, #29999, .T. ) ;
#52323 = FACE_OUTER_BOUND ( 'NONE', #89185, .T. ) ;
#52324 = FACE_BOUND ( 'NONE', #94238, .T. ) ;
#52325 = ORIENTED_EDGE ( 'NONE', *, *, #142645, .F. ) ;
#52326 = CARTESIAN_POINT ( 'NONE',  ( 33.79289321881321939, 18.75929247661552779, 5.000000000000000000 ) ) ;
#52327 = DIRECTION ( 'NONE',  ( -0.7071067811865487940, 0.7071067811865463515, -0.000000000000000000 ) ) ;
#52328 = CARTESIAN_POINT ( 'NONE',  ( -60.18398860626900415, 28.73617430169829490, 5.000000000000000000 ) ) ;
#52329 = VERTEX_POINT ( 'NONE', #142360 ) ;
#52330 = LINE ( 'NONE', #117561, #55045 ) ;
#52331 = EDGE_LOOP ( 'NONE', ( #75587, #59341, #82694, #50336 ) ) ;
#52333 = ORIENTED_EDGE ( 'NONE', *, *, #31725, .F. ) ;
#52332 = EDGE_CURVE ( 'NONE', #48062, #52188, #98135, .T. ) ;
#52334 = DIRECTION ( 'NONE',  ( 0.3543493200069162685, -0.000000000000000000, -0.9351131265310288487 ) ) ;
#52335 = VECTOR ( 'NONE', #9670, 1000.000000000000000 ) ;
#52336 = ORIENTED_EDGE ( 'NONE', *, *, #23372, .T. ) ;
#52337 = VECTOR ( 'NONE', #134330, 1000.000000000000000 ) ;
#52338 = CARTESIAN_POINT ( 'NONE',  ( 54.74543019189812298, -5.291415217122918513, -3.055000000000000160 ) ) ;
#52339 = VERTEX_POINT ( 'NONE', #75670 ) ;
#52340 = LINE ( 'NONE', #108120, #39534 ) ;
#52341 = AXIS2_PLACEMENT_3D ( 'NONE', #46448, #81189, #79798 ) ;
#52342 = LINE ( 'NONE', #17562, #93594 ) ;
#52343 = EDGE_CURVE ( 'NONE', #89978, #10977, #119842, .T. ) ;
#52344 = ORIENTED_EDGE ( 'NONE', *, *, #61392, .T. ) ;
#52345 = FACE_OUTER_BOUND ( 'NONE', #142253, .T. ) ;
#52346 = AXIS2_PLACEMENT_3D ( 'NONE', #71009, #115158, #13012 ) ;
#52347 = EDGE_CURVE ( 'NONE', #118128, #82989, #122602, .T. ) ;
#52348 = DIRECTION ( 'NONE',  ( -0.7071067811865486830, -0.7071067811865464625, -0.000000000000000000 ) ) ;
#52349 = CARTESIAN_POINT ( 'NONE',  ( 19.49999999999986500, -17.91344420646041158, 1.358650452708509038 ) ) ;
#52350 = DIRECTION ( 'NONE',  ( 1.000000000000000000, 0.000000000000000000, 0.000000000000000000 ) ) ;
#52351 = EDGE_CURVE ( 'NONE', #143094, #68410, #40895, .T. ) ;
#52352 = LINE ( 'NONE', #21152, #67971 ) ;
#52353 = DIRECTION ( 'NONE',  ( 0.7071067811865487940, 0.7071067811865463515, 0.000000000000000000 ) ) ;
#52354 = VERTEX_POINT ( 'NONE', #8221 ) ;
#52355 = ORIENTED_EDGE ( 'NONE', *, *, #78901, .F. ) ;
#52356 = CARTESIAN_POINT ( 'NONE',  ( 1.734933297179483525, 12.75929247661558996, 18.34774599283955965 ) ) ;
#52357 = DIRECTION ( 'NONE',  ( -0.3543493200069162685, -0.000000000000000000, -0.9351131265310288487 ) ) ;
#52358 = ORIENTED_EDGE ( 'NONE', *, *, #11409, .T. ) ;
#52359 = ADVANCED_FACE ( 'NONE', ( #121297 ), #53164, .T. ) ;
#52360 = EDGE_LOOP ( 'NONE', ( #51791, #110695, #130234, #139246 ) ) ;
#52361 = VERTEX_POINT ( 'NONE', #10383 ) ;
#52362 = FACE_OUTER_BOUND ( 'NONE', #57365, .T. ) ;
#52363 = CARTESIAN_POINT ( 'NONE',  ( -1.499999999999994449, 19.08746187583905751, 4.000000000000000000 ) ) ;
#52364 = FACE_OUTER_BOUND ( 'NONE', #91303, .T. ) ;
#52365 = EDGE_LOOP ( 'NONE', ( #36980, #109427, #124148, #110099, #81275 ) ) ;
#52366 = CARTESIAN_POINT ( 'NONE',  ( -42.29974487139158157, -27.71228299555235708, 4.000000000000000000 ) ) ;
#52367 = DIRECTION ( 'NONE',  ( 0.7071067811865486830, -0.7071067811865464625, -0.000000000000000000 ) ) ;
#52368 = CARTESIAN_POINT ( 'NONE',  ( 22.67123647476855552, 0.000000000000000000, 7.934999999999990727 ) ) ;
#52369 = DIRECTION ( 'NONE',  ( -0.7071067811865486830, -0.7071067811865464625, 0.000000000000000000 ) ) ;
#52370 = EDGE_LOOP ( 'NONE', ( #2094, #1226, #9522, #3343 ) ) ;
#52371 = CARTESIAN_POINT ( 'NONE',  ( 116.2870968585647802, 3.054999999999997939, 5.291415217122920289 ) ) ;
#52372 = EDGE_CURVE ( 'NONE', #112966, #108472, #69706, .T. ) ;
#52373 = DIRECTION ( 'NONE',  ( 0.000000000000000000, 0.000000000000000000, 1.000000000000000000 ) ) ;
#52374 = DIRECTION ( 'NONE',  ( 0.7071067811865487940, 0.7071067811865463515, 0.000000000000000000 ) ) ;
#52376 = ORIENTED_EDGE ( 'NONE', *, *, #60401, .T. ) ;
#52375 = DIRECTION ( 'NONE',  ( 0.000000000000000000, 1.000000000000000000, 0.000000000000000000 ) ) ;
#52377 = AXIS2_PLACEMENT_3D ( 'NONE', #372, #3746, #11233 ) ;
#52378 = FACE_OUTER_BOUND ( 'NONE', #124083, .T. ) ;
#52379 = ORIENTED_EDGE ( 'NONE', *, *, #120168, .F. ) ;
#52380 = CARTESIAN_POINT ( 'NONE',  ( 34.92499999999998295, 13.70193056682084887, 4.500000000000000888 ) ) ;
#52381 = EDGE_CURVE ( 'NONE', #83142, #32075, #79027, .T. ) ;
#52382 = DIRECTION ( 'NONE',  ( 0.7071067811865487940, 0.7071067811865463515, -0.000000000000000000 ) ) ;
#52383 = CARTESIAN_POINT ( 'NONE',  ( 12.69999999999999574, -25.83999999999998565, 13.17925390838734323 ) ) ;
#52384 = EDGE_LOOP ( 'NONE', ( #9123, #33563, #5978, #123495 ) ) ;
#52385 = PLANE ( 'NONE',  #95827 ) ;
#52386 = CARTESIAN_POINT ( 'NONE',  ( -33.48921356237309510, -27.52281430457078670, 5.000000000000000000 ) ) ;
#52387 = CARTESIAN_POINT ( 'NONE',  ( -19.87251829384141288, -2.732064206673406659, -33.82029841778192747 ) ) ;
#52388 = VECTOR ( 'NONE', #26411, 1000.000000000000000 ) ;
#52389 = ORIENTED_EDGE ( 'NONE', *, *, #89007, .T. ) ;
#52390 = CARTESIAN_POINT ( 'NONE',  ( -31.82816939922330945, -5.240707523384227073, 4.000000000000000000 ) ) ;
#52391 = CARTESIAN_POINT ( 'NONE',  ( 16.49999999999987566, 8.319652575858389909, -8.582050562765786594 ) ) ;
#52392 = FACE_OUTER_BOUND ( 'NONE', #17121, .T. ) ;
#52393 = LINE ( 'NONE', #86477, #20702 ) ;
#52394 = VERTEX_POINT ( 'NONE', #95969 ) ;
#52395 = ORIENTED_EDGE ( 'NONE', *, *, #108825, .T. ) ;
#52396 = FACE_OUTER_BOUND ( 'NONE', #76764, .T. ) ;
#52397 = CARTESIAN_POINT ( 'NONE',  ( 31.49999999999977973, 8.900465351122178959, -2.516491619111585809 ) ) ;
#52398 = CARTESIAN_POINT ( 'NONE',  ( 14.27040314143522082, -7.934999999999989839, 2.126176841940957907 ) ) ;
#52399 = VECTOR ( 'NONE', #62004, 1000.000000000000000 ) ;
#52400 = FILL_AREA_STYLE_COLOUR ( '', #1907 ) ;
#52401 = EDGE_CURVE ( 'NONE', #117130, #25131, #64182, .T. ) ;
#52402 = FACE_OUTER_BOUND ( 'NONE', #87843, .T. ) ;
#52403 = DIRECTION ( 'NONE',  ( 0.6830127018922180770, -0.6830127018922204085, -0.2588190451025213501 ) ) ;
#52404 = VECTOR ( 'NONE', #39687, 1000.000000000000000 ) ;
#52405 = ORIENTED_EDGE ( 'NONE', *, *, #114159, .T. ) ;
#52406 =( LENGTH_UNIT ( ) NAMED_UNIT ( * ) SI_UNIT ( .MILLI., .METRE. ) );
#52407 = CARTESIAN_POINT ( 'NONE',  ( 23.20710678118638270, -17.24070752338410628, 5.000000000000000000 ) ) ;
#52408 = CARTESIAN_POINT ( 'NONE',  ( 60.18398860626900415, 28.73617430169829490, 5.000000000000000000 ) ) ;
#52409 = DIRECTION ( 'NONE',  ( 1.000000000000000000, 0.000000000000000000, 0.000000000000000000 ) ) ;
#52410 = CARTESIAN_POINT ( 'NONE',  ( 34.76626352523145158, 4.472830434245839371, -4.472830434245839371 ) ) ;
#52411 = DIRECTION ( 'NONE',  ( -1.000000000000000000, 6.248375730189539568E-15, 0.000000000000000000 ) ) ;
#52412 = VERTEX_POINT ( 'NONE', #111868 ) ;
#52413 = CARTESIAN_POINT ( 'NONE',  ( 33.79289321881321939, -5.240707523384228850, 5.000000000000000000 ) ) ;
#52414 = ORIENTED_EDGE ( 'NONE', *, *, #104940, .F. ) ;
#52415 = TOROIDAL_SURFACE ( 'NONE', #138115, 2.000000000000000000, 1.000000000000000000 ) ;
#52416 = VERTEX_POINT ( 'NONE', #111111 ) ;
#52417 = LINE ( 'NONE', #96602, #89542 ) ;
#52418 = CARTESIAN_POINT ( 'NONE',  ( 29.99999999999979394, -6.108550654416931458, -3.114665004254898673 ) ) ;
#52419 = EDGE_LOOP ( 'NONE', ( #124088, #5196, #73520, #99839, #15341, #33180 ) ) ;
#52420 =( NAMED_UNIT ( * ) SI_UNIT ( $, .STERADIAN. ) SOLID_ANGLE_UNIT ( ) );
#52421 = LINE ( 'NONE', #96606, #46576 ) ;
#52422 = CARTESIAN_POINT ( 'NONE',  ( 0.000000000000000000, 0.000000000000000000, 5.000000000000000000 ) ) ;
#52423 = VECTOR ( 'NONE', #1112, 1000.000000000000000 ) ;
#52424 = PLANE ( 'NONE',  #53425 ) ;
#52425 = CARTESIAN_POINT ( 'NONE',  ( 7.828169399223476432, -11.24070752338416135, 4.000000000000000000 ) ) ;
#52426 = ORIENTED_EDGE ( 'NONE', *, *, #35654, .F. ) ;
#52427 = DIRECTION ( 'NONE',  ( 1.734723475976806848E-16, -1.000000000000000000, 0.000000000000000000 ) ) ;
#52428 = FACE_OUTER_BOUND ( 'NONE', #51533, .T. ) ;
#52429 = FACE_OUTER_BOUND ( 'NONE', #10560, .T. ) ;
#52430 = CARTESIAN_POINT ( 'NONE',  ( 8.999999999999941380, 4.965500833774342482, -4.007596771432676341 ) ) ;
#52431 = AXIS2_PLACEMENT_3D ( 'NONE', #139359, #64615, #7355 ) ;
#52432 = CARTESIAN_POINT ( 'NONE',  ( 34.45011844616451668, 6.002304141593879372, 5.000000000000000888 ) ) ;
#52433 = VECTOR ( 'NONE', #140223, 1000.000000000000000 ) ;
#52434 = CARTESIAN_POINT ( 'NONE',  ( 59.57919371712955581, 3.975000000000002753, -6.884901960086283523 ) ) ;
#52435 = VECTOR ( 'NONE', #107390, 1000.000000000000000 ) ;
#52436 = DIRECTION ( 'NONE',  ( 0.000000000000000000, 0.000000000000000000, 1.000000000000000000 ) ) ;
#52437 = VERTEX_POINT ( 'NONE', #132934 ) ;
#52438 = ORIENTED_EDGE ( 'NONE', *, *, #16138, .T. ) ;
#52439 = VECTOR ( 'NONE', #14954, 1000.000000000000227 ) ;
#52440 = CARTESIAN_POINT ( 'NONE',  ( 58.60416666666665719, 2.130196079827422206, 7.950000000000001954 ) ) ;
#52441 = CARTESIAN_POINT ( 'NONE',  ( 21.48921356237309155, -27.52281430457070499, 5.000000000000000000 ) ) ;
#52442 = CARTESIAN_POINT ( 'NONE',  ( 181.1500000000000057, -43.14999999999999147, 40.92499999999998295 ) ) ;
#52444 = CARTESIAN_POINT ( 'NONE',  ( -33.29974487139158867, -27.71228299555229313, 4.000000000000000000 ) ) ;
#52443 = CIRCLE ( 'NONE', #8425, 2.500000000000000888 ) ;
#52445 = ORIENTED_EDGE ( 'NONE', *, *, #73936, .F. ) ;
#52446 = DIRECTION ( 'NONE',  ( 0.7071067811865486830, -0.7071067811865464625, -0.000000000000000000 ) ) ;
#52447 = CARTESIAN_POINT ( 'NONE',  ( 45.20876352523143993, -7.482591942790329030E-16, 6.110000000000001208 ) ) ;
#52448 = EDGE_LOOP ( 'NONE', ( #64333, #7083, #58677, #2489, #65657 ) ) ;
#52449 = EDGE_CURVE ( 'NONE', #40381, #142459, #56809, .T. ) ;
#52450 = DIRECTION ( 'NONE',  ( 0.3543493200069162685, -0.000000000000000000, -0.9351131265310288487 ) ) ;
#52451 = ORIENTED_EDGE ( 'NONE', *, *, #103654, .T. ) ;
#52452 = ORIENTED_EDGE ( 'NONE', *, *, #19130, .F. ) ;
#52453 = DIRECTION ( 'NONE',  ( 0.000000000000000000, 0.000000000000000000, 1.000000000000000000 ) ) ;
#52454 = LINE ( 'NONE', #120543, #66234 ) ;
#52455 = CARTESIAN_POINT ( 'NONE',  ( -34.92500000000001137, -17.99387692260789251, 4.000000000000000000 ) ) ;
#52456 = EDGE_CURVE ( 'NONE', #121050, #42538, #80675, .T. ) ;
#52457 = CARTESIAN_POINT ( 'NONE',  ( -69.18398860626899705, 28.73617430169835529, 5.000000000000000000 ) ) ;
#52458 = ORIENTED_EDGE ( 'NONE', *, *, #140060, .F. ) ;
#52459 = LINE ( 'NONE', #140891, #14143 ) ;
#52460 = EDGE_CURVE ( 'NONE', #89130, #126442, #46658, .T. ) ;
#52461 = EDGE_CURVE ( 'NONE', #111700, #40790, #135760, .T. ) ;
#52463 = ORIENTED_EDGE ( 'NONE', *, *, #13326, .F. ) ;
#52462 = CARTESIAN_POINT ( 'NONE',  ( -17.00355154389407275, -0.9028365174813322014, -35.76436417572673321 ) ) ;
#52464 = DIRECTION ( 'NONE',  ( 1.000000000000000000, 0.000000000000000000, -0.000000000000000000 ) ) ;
#52465 = LINE ( 'NONE', #63395, #119473 ) ;
#52466 = LINE ( 'NONE', #140898, #93471 ) ;
#52467 = FACE_OUTER_BOUND ( 'NONE', #49591, .T. ) ;
#52469 = ORIENTED_EDGE ( 'NONE', *, *, #4826, .F. ) ;
#52468 = EDGE_CURVE ( 'NONE', #24662, #11839, #88697, .T. ) ;
#52470 = EDGE_CURVE ( 'NONE', #50212, #57095, #133621, .T. ) ;
#52471 = ORIENTED_EDGE ( 'NONE', *, *, #52920, .F. ) ;
#52472 = VECTOR ( 'NONE', #31176, 1000.000000000000000 ) ;
#52473 = FACE_OUTER_BOUND ( 'NONE', #51034, .T. ) ;
#52474 = CARTESIAN_POINT ( 'NONE',  ( 65.09959685856478018, -6.109999999999997655, -1.637169565754160283 ) ) ;
#52475 = CARTESIAN_POINT ( 'NONE',  ( -0.4892135623730947680, -27.52281430457055578, 5.000000000000000000 ) ) ;
#52476 = EDGE_CURVE ( 'NONE', #25093, #70259, #79987, .T. ) ;
#52477 = CARTESIAN_POINT ( 'NONE',  ( 27.18398860626900060, 28.73617430169806042, 5.000000000000000000 ) ) ;
#52478 = CARTESIAN_POINT ( 'NONE',  ( -18.48921356237309510, -27.52281430457068367, 5.000000000000000000 ) ) ;
#52479 = VERTEX_POINT ( 'NONE', #78522 ) ;
#52480 = ORIENTED_EDGE ( 'NONE', *, *, #138282, .T. ) ;
#52481 = VECTOR ( 'NONE', #52282, 1000.000000000000000 ) ;
#52482 = EDGE_CURVE ( 'NONE', #82894, #80563, #58247, .T. ) ;
#52483 = DIRECTION ( 'NONE',  ( -1.000000000000000000, -1.224606353822377258E-16, -0.000000000000000000 ) ) ;
#52484 = DIRECTION ( 'NONE',  ( -0.6830127018922180770, -0.6830127018922204085, -0.2588190451025213501 ) ) ;
#52485 = ORIENTED_EDGE ( 'NONE', *, *, #68236, .F. ) ;
#52486 = EDGE_CURVE ( 'NONE', #94514, #115757, #24843, .T. ) ;
#52487 = ORIENTED_EDGE ( 'NONE', *, *, #95735, .T. ) ;
#52488 = LINE ( 'NONE', #75691, #141662 ) ;
#52489 = EDGE_LOOP ( 'NONE', ( #141374, #98419, #93324, #15011 ) ) ;
#52490 = CARTESIAN_POINT ( 'NONE',  ( 0.000000000000000000, 0.000000000000000000, 5.000000000000000000 ) ) ;
#52491 = PLANE ( 'NONE',  #54941 ) ;
#52492 = AXIS2_PLACEMENT_3D ( 'NONE', #48702, #94332, #116801 ) ;
#52493 = ADVANCED_FACE ( 'NONE', ( #45909 ), #33611, .F. ) ;
#52494 = DIRECTION ( 'NONE',  ( 0.6830127018922181881, 0.6830127018922202975, -0.2588190451025214056 ) ) ;
#52495 = AXIS2_PLACEMENT_3D ( 'NONE', #82653, #27527, #73910 ) ;
#52496 = FACE_BOUND ( 'NONE', #122840, .T. ) ;
#52497 = DIRECTION ( 'NONE',  ( 1.000000000000000000, 0.000000000000000000, 0.000000000000000000 ) ) ;
#52498 = DIRECTION ( 'NONE',  ( -1.000000000000000000, -1.224606353822377258E-16, -0.000000000000000000 ) ) ;
#52499 = DIRECTION ( 'NONE',  ( -0.7071067811865486830, -0.7071067811865464625, 0.000000000000000000 ) ) ;
#52501 = ORIENTED_EDGE ( 'NONE', *, *, #25250, .T. ) ;
#52500 = FACE_OUTER_BOUND ( 'NONE', #114413, .T. ) ;
#52502 = ADVANCED_FACE ( 'NONE', ( #195 ), #100275, .F. ) ;
#52503 = PRESENTATION_STYLE_ASSIGNMENT (( #28642 ) ) ;
#52504 = ITEM_DEFINED_TRANSFORMATION ( 'NONE', 'NONE', #14642,  #127880 ) ;
#52506 = ORIENTED_EDGE ( 'NONE', *, *, #120905, .T. ) ;
#52505 = VECTOR ( 'NONE', #51657, 1000.000000000000000 ) ;
#52507 = ORIENTED_EDGE ( 'NONE', *, *, #13061, .F. ) ;
#52508 = CARTESIAN_POINT ( 'NONE',  ( 86.82876352523145158, 0.000000000000000000, -6.109999999999998543 ) ) ;
#52509 = ORIENTED_EDGE ( 'NONE', *, *, #89886, .T. ) ;
#52510 = CIRCLE ( 'NONE', #1562, 2.055000000000001048 ) ;
#52511 = CARTESIAN_POINT ( 'NONE',  ( -17.29289321881334018, 17.25929247661554200, 5.000000000000000000 ) ) ;
#52512 = ADVANCED_FACE ( 'NONE', ( #11078 ), #55351, .T. ) ;
#52513 = EDGE_LOOP ( 'NONE', ( #20948, #34710, #103495, #7855 ) ) ;
#52514 = LINE ( 'NONE', #95304, #9705 ) ;
#52515 = CARTESIAN_POINT ( 'NONE',  ( 13.08100000000000307, 3.174999999999998046, 1.444000000000000394 ) ) ;
#52516 = ADVANCED_FACE ( 'NONE', ( #56089 ), #929, .F. ) ;
#52517 = CARTESIAN_POINT ( 'NONE',  ( -24.70710678118637915, 17.25929247661554911, 5.000000000000000000 ) ) ;
#52518 = DIRECTION ( 'NONE',  ( 0.6830127018922180770, -0.6830127018922204085, -0.2588190451025213501 ) ) ;
#52519 = DIRECTION ( 'NONE',  ( 0.3543493200069162685, -0.000000000000000000, -0.9351131265310288487 ) ) ;
#52520 = EDGE_CURVE ( 'NONE', #115378, #104397, #79282, .T. ) ;
#52521 = CARTESIAN_POINT ( 'NONE',  ( 0.000000000000000000, 0.000000000000000000, 5.000000000000000000 ) ) ;
#52522 = CARTESIAN_POINT ( 'NONE',  ( 21.48921356237309155, -27.52281430457070499, 5.000000000000000000 ) ) ;
#52523 = EDGE_LOOP ( 'NONE', ( #127725, #63305, #100991 ) ) ;
#52524 = CARTESIAN_POINT ( 'NONE',  ( 34.92499999999998295, 6.662461875838954661, 4.000000000000000000 ) ) ;
#52525 = ORIENTED_EDGE ( 'NONE', *, *, #26465, .F. ) ;
#52526 = LINE ( 'NONE', #95319, #109744 ) ;
#52527 = EDGE_CURVE ( 'NONE', #82948, #80191, #123484, .T. ) ;
#52528 = FACE_OUTER_BOUND ( 'NONE', #118872, .T. ) ;
#52529 = EDGE_CURVE ( 'NONE', #80080, #68527, #68392, .T. ) ;
#52530 = VERTEX_POINT ( 'NONE', #50894 ) ;
#52532 = VERTEX_POINT ( 'NONE', #114693 ) ;
#52531 = VECTOR ( 'NONE', #79292, 1000.000000000000000 ) ;
#52533 = ORIENTED_EDGE ( 'NONE', *, *, #35017, .F. ) ;
#52534 = CARTESIAN_POINT ( 'NONE',  ( 37.91709685856477563, 3.054999999999998828, 5.291415217122922066 ) ) ;
#52535 = ORIENTED_EDGE ( 'NONE', *, *, #28442, .F. ) ;
#52536 = CARTESIAN_POINT ( 'NONE',  ( 45.47916666666666430, -7.950000000000000178, 2.130196079827424427 ) ) ;
#52537 = VECTOR ( 'NONE', #17023, 1000.000000000000000 ) ;
#52538 = VECTOR ( 'NONE', #27518, 1000.000000000000227 ) ;
#52539 = VECTOR ( 'NONE', #35022, 1000.000000000000227 ) ;
#52540 = CARTESIAN_POINT ( 'NONE',  ( 22.21247294953710494, 0.000000000000000000, 6.094999999999989981 ) ) ;
#52541 = CARTESIAN_POINT ( 'NONE',  ( 0.8904098635733341816, 12.57359452820395163, -26.74927803365304868 ) ) ;
#52542 = ORIENTED_EDGE ( 'NONE', *, *, #84770, .F. ) ;
#52543 = EDGE_CURVE ( 'NONE', #117239, #23453, #50809, .T. ) ;
#52544 = CARTESIAN_POINT ( 'NONE',  ( -20.99999999999985079, -12.03360074219761344, 5.000000000000000000 ) ) ;
#52545 = VECTOR ( 'NONE', #56383, 1000.000000000000000 ) ;
#52546 = ORIENTED_EDGE ( 'NONE', *, *, #131323, .F. ) ;
#52547 = DIRECTION ( 'NONE',  ( 0.000000000000000000, 1.000000000000000000, 0.000000000000000000 ) ) ;
#52548 = CARTESIAN_POINT ( 'NONE',  ( 63.48921356237309510, -27.52281430457099631, 5.000000000000000000 ) ) ;
#52550 = EDGE_LOOP ( 'NONE', ( #28052, #91922, #4510, #7861, #57978, #92111 ) ) ;
#52549 = CARTESIAN_POINT ( 'NONE',  ( 2.999999999999981792, -2.904428200921304271, -6.989807076074948000 ) ) ;
#52551 = ORIENTED_EDGE ( 'NONE', *, *, #131964, .T. ) ;
#52552 = LINE ( 'NONE', #96732, #35366 ) ;
#52553 = DIRECTION ( 'NONE',  ( -0.6830127018922180770, -0.6830127018922204085, -0.2588190451025213501 ) ) ;
#52554 = EDGE_LOOP ( 'NONE', ( #98077, #114643, #44863, #38269 ) ) ;
#52555 = PLANE ( 'NONE',  #124554 ) ;
#52556 = ORIENTED_EDGE ( 'NONE', *, *, #22328, .T. ) ;
#52557 = EDGE_LOOP ( 'NONE', ( #80046, #37518, #26555, #26577 ) ) ;
#52558 = EDGE_CURVE ( 'NONE', #3888, #138634, #39313, .T. ) ;
#52559 = ORIENTED_EDGE ( 'NONE', *, *, #93787, .T. ) ;
#52560 = CARTESIAN_POINT ( 'NONE',  ( -18.32816939922339472, -15.74070752338412760, 4.000000000000000000 ) ) ;
#52561 = LINE ( 'NONE', #96744, #77106 ) ;
#52562 = LINE ( 'NONE', #38313, #32982 ) ;
#52563 = FACE_OUTER_BOUND ( 'NONE', #12611, .T. ) ;
#52564 = EDGE_CURVE ( 'NONE', #140080, #23121, #58971, .T. ) ;
#52565 = DIRECTION ( 'NONE',  ( 0.7071067811865487940, -0.7071067811865463515, 0.000000000000000000 ) ) ;
#52566 = ORIENTED_EDGE ( 'NONE', *, *, #86450, .F. ) ;
#52568 = ADVANCED_FACE ( 'NONE', ( #60363 ), #104061, .T. ) ;
#52567 = DIRECTION ( 'NONE',  ( -0.7071067811865486830, 0.7071067811865464625, 0.000000000000000000 ) ) ;
#52569 = ORIENTED_EDGE ( 'NONE', *, *, #11407, .F. ) ;
#52570 = VECTOR ( 'NONE', #119396, 1000.000000000000000 ) ;
#52571 = LINE ( 'NONE', #85919, #123490 ) ;
#52572 = CARTESIAN_POINT ( 'NONE',  ( 33.22873647476855297, 5.808823158059031044, -5.808823158059038150 ) ) ;
#52573 = VECTOR ( 'NONE', #102517, 1000.000000000000000 ) ;
#52574 = ORIENTED_EDGE ( 'NONE', *, *, #77923, .T. ) ;
#52575 = DIRECTION ( 'NONE',  ( -0.7071067811865487940, 0.7071067811865463515, -0.000000000000000000 ) ) ;
#52576 = DIRECTION ( 'NONE',  ( -1.000000000000000000, -0.000000000000000000, -0.000000000000000000 ) ) ;
#52577 = ADVANCED_FACE ( 'NONE', ( #49499 ), #81406, .T. ) ;
#52578 = ORIENTED_EDGE ( 'NONE', *, *, #41911, .F. ) ;
#52579 = ORIENTED_EDGE ( 'NONE', *, *, #87439, .T. ) ;
#52580 = PLANE ( 'NONE',  #6980 ) ;
#52581 = DIRECTION ( 'NONE',  ( -0.7071067811865486830, -0.7071067811865464625, 0.000000000000000000 ) ) ;
#52582 = LINE ( 'NONE', #41003, #33122 ) ;
#52583 = AXIS2_PLACEMENT_3D ( 'NONE', #44110, #133960, #36099 ) ;
#52584 = CARTESIAN_POINT ( 'NONE',  ( -34.42500000000001137, -18.02281430457038880, 5.000000000000000000 ) ) ;
#52585 = CARTESIAN_POINT ( 'NONE',  ( 68.89126352523142316, -4.472830434245839371, -4.472830434245839371 ) ) ;
#52586 = EDGE_CURVE ( 'NONE', #125809, #65260, #127747, .T. ) ;
#52587 = FACE_BOUND ( 'NONE', #112272, .T. ) ;
#52588 = LINE ( 'NONE', #31569, #48533 ) ;
#52589 = ADVANCED_FACE ( 'NONE', ( #128458 ), #6608, .F. ) ;
#52590 = CARTESIAN_POINT ( 'NONE',  ( 48.48921356237309510, -27.52281430457089328, 5.000000000000000000 ) ) ;
#52591 = CARTESIAN_POINT ( 'NONE',  ( -17.99999999999987566, -13.06887692260767331, 4.000000000000000000 ) ) ;
#52592 = VERTEX_POINT ( 'NONE', #61784 ) ;
#52593 = CARTESIAN_POINT ( 'NONE',  ( -51.18398860626899705, 28.73617430169823095, 5.000000000000000000 ) ) ;
#52594 = CIRCLE ( 'NONE', #1649, 2.500000000000000888 ) ;
#52595 = ORIENTED_EDGE ( 'NONE', *, *, #27974, .F. ) ;
#52596 = LINE ( 'NONE', #122127, #87167 ) ;
#52597 = FILL_AREA_STYLE_COLOUR ( '', #117029 ) ;
#52598 = EDGE_LOOP ( 'NONE', ( #12392, #11587, #59486, #129743 ) ) ;
#52599 = PLANE ( 'NONE',  #13729 ) ;
#52601 = ORIENTED_EDGE ( 'NONE', *, *, #72555, .T. ) ;
#52600 = DIRECTION ( 'NONE',  ( 0.7071067811865486830, -0.7071067811865464625, -0.000000000000000000 ) ) ;
#52602 = CARTESIAN_POINT ( 'NONE',  ( 0.4644480930543399833, 0.3999999999999995226, 2.317232462839659668 ) ) ;
#52603 = AXIS2_PLACEMENT_3D ( 'NONE', #140417, #6281, #115059 ) ;
#52604 = ADVANCED_FACE ( 'NONE', ( #28433 ), #70547, .F. ) ;
#52605 = CARTESIAN_POINT ( 'NONE',  ( 34.49999999999975131, -20.94567065516883630, 4.994342998332155226 ) ) ;
#52606 = CARTESIAN_POINT ( 'NONE',  ( 19.89359858452208130, -2.055000000000000160, 0.000000000000000000 ) ) ;
#52607 = EDGE_LOOP ( 'NONE', ( #52830, #54180, #128717, #13059 ) ) ;
#52608 = VERTEX_POINT ( 'NONE', #104543 ) ;
#52609 = LINE ( 'NONE', #97537, #109221 ) ;
#52610 = LINE ( 'NONE', #96104, #77693 ) ;
#52611 = CARTESIAN_POINT ( 'NONE',  ( 87.57919371712957002, 3.975000000000002753, -6.884901960086283523 ) ) ;
#52612 = DIRECTION ( 'NONE',  ( -0.7071067811865486830, 0.7071067811865464625, 0.000000000000000000 ) ) ;
#52613 = CARTESIAN_POINT ( 'NONE',  ( -45.18398860626900415, 28.73617430169818832, 5.000000000000000000 ) ) ;
#52614 = EDGE_LOOP ( 'NONE', ( #34363, #126829, #17285, #17063, #99889, #114925 ) ) ;
#52615 = VECTOR ( 'NONE', #82842, 1000.000000000000000 ) ;
#52616 = DIRECTION ( 'NONE',  ( -0.7071067811865486830, -0.7071067811865464625, 0.000000000000000000 ) ) ;
#52617 = CARTESIAN_POINT ( 'NONE',  ( -7.499999999999940492, -8.947814304570741228, 5.000000000000000000 ) ) ;
#52618 = CARTESIAN_POINT ( 'NONE',  ( 31.79166666666666785, -3.047499999999994547, 5.278424836066145431 ) ) ;
#52619 = ORIENTED_EDGE ( 'NONE', *, *, #56437, .F. ) ;
#52620 = CARTESIAN_POINT ( 'NONE',  ( 39.48921356237310221, -27.52281430457082934, 5.000000000000000000 ) ) ;
#52621 = VERTEX_POINT ( 'NONE', #116852 ) ;
#52622 = CARTESIAN_POINT ( 'NONE',  ( 76.70876352523144703, -7.482591942790329030E-16, 6.110000000000001208 ) ) ;
#52623 = DIRECTION ( 'NONE',  ( 0.000000000000000000, -1.000000000000000000, 0.000000000000000000 ) ) ;
#52624 = CARTESIAN_POINT ( 'NONE',  ( -26.27718569542921401, -21.72499999999999432, 5.000000000000000000 ) ) ;
#52625 = VERTEX_POINT ( 'NONE', #14689 ) ;
#52626 = CARTESIAN_POINT ( 'NONE',  ( -45.18398860626900415, 28.73617430169818832, 5.000000000000000000 ) ) ;
#52627 = CARTESIAN_POINT ( 'NONE',  ( 0.000000000000000000, 0.000000000000000000, 5.000000000000000000 ) ) ;
#52628 = AXIS2_PLACEMENT_3D ( 'NONE', #128119, #29484, #117894 ) ;
#52629 = CARTESIAN_POINT ( 'NONE',  ( 5.443598275411213550, 3.821174125832445049E-16, 0.000000000000000000 ) ) ;
#52630 = CARTESIAN_POINT ( 'NONE',  ( 27.18398860626900060, 28.73617430169806042, 5.000000000000000000 ) ) ;
#52631 = EDGE_CURVE ( 'NONE', #62501, #22625, #137911, .T. ) ;
#52633 = VERTEX_POINT ( 'NONE', #105949 ) ;
#52632 = CARTESIAN_POINT ( 'NONE',  ( 8.811592354503320124, 2.500000000000001776, 0.000000000000000000 ) ) ;
#52634 = CARTESIAN_POINT ( 'NONE',  ( 128.8216926156730722, -52.14999999996970814, -41.05175048930497184 ) ) ;
#52635 = CARTESIAN_POINT ( 'NONE',  ( 5.475998614145475507, 22.03583458319438648, 4.979811245910084061 ) ) ;
#52636 = CARTESIAN_POINT ( 'NONE',  ( 23.54739889332687497, 7.099584588756134629, 5.000000000000000000 ) ) ;
#52637 = CONICAL_SURFACE ( 'NONE', #8513, 2.500000000000000444, 0.9599310885968830309 ) ;
#52638 = DIRECTION ( 'NONE',  ( 0.7071067811865487940, 0.7071067811865463515, 0.000000000000000000 ) ) ;
#52640 = CIRCLE ( 'NONE', #61988, 2.500000000000000888 ) ;
#52639 = VECTOR ( 'NONE', #2370, 1000.000000000000227 ) ;
#52641 = ORIENTED_EDGE ( 'NONE', *, *, #37132, .T. ) ;
#52642 = ORIENTED_EDGE ( 'NONE', *, *, #108294, .F. ) ;
#52644 = EDGE_CURVE ( 'NONE', #95429, #82756, #3764, .T. ) ;
#52643 = VECTOR ( 'NONE', #42872, 1000.000000000000000 ) ;
#52645 = CARTESIAN_POINT ( 'NONE',  ( 77.87543019189810423, -5.291415217122920289, -3.055000000000001492 ) ) ;
#52646 = ORIENTED_EDGE ( 'NONE', *, *, #84859, .T. ) ;
#52647 = ADVANCED_FACE ( 'NONE', ( #127000 ), #59647, .F. ) ;
#52648 = LINE ( 'NONE', #30182, #56907 ) ;
#52649 = DIRECTION ( 'NONE',  ( -0.000000000000000000, 0.000000000000000000, 1.000000000000000000 ) ) ;
#52650 = EDGE_CURVE ( 'NONE', #1167, #15218, #99285, .T. ) ;
#52652 = AXIS2_PLACEMENT_3D ( 'NONE', #16432, #136097, #36779 ) ;
#52651 = CARTESIAN_POINT ( 'NONE',  ( 0.000000000000000000, 0.000000000000000000, 5.000000000000000000 ) ) ;
#52653 = DIRECTION ( 'NONE',  ( 1.000000000000000000, 1.224606353822377258E-16, 0.000000000000000000 ) ) ;
#52654 = VERTEX_POINT ( 'NONE', #92960 ) ;
#52655 = EDGE_CURVE ( 'NONE', #93595, #22044, #38584, .T. ) ;
#52656 = LINE ( 'NONE', #119326, #26094 ) ;
#52657 = DIRECTION ( 'NONE',  ( -0.7071067811865486830, -0.7071067811865464625, 0.000000000000000000 ) ) ;
#52658 = ORIENTED_EDGE ( 'NONE', *, *, #59895, .F. ) ;
#52659 = ADVANCED_FACE ( 'NONE', ( #137196 ), #37893, .F. ) ;
#52660 = CARTESIAN_POINT ( 'NONE',  ( 39.29974487139159578, -27.71228299555233576, 4.000000000000000000 ) ) ;
#52661 = DIRECTION ( 'NONE',  ( 0.7071067811865487940, 0.7071067811865463515, 0.000000000000000000 ) ) ;
#52662 = DIRECTION ( 'NONE',  ( 0.6830127018922180770, -0.6830127018922204085, -0.2588190451025213501 ) ) ;
#52663 = ORIENTED_EDGE ( 'NONE', *, *, #138615, .F. ) ;
#52664 = ORIENTED_EDGE ( 'NONE', *, *, #40797, .T. ) ;
#52665 = EDGE_CURVE ( 'NONE', #53640, #25047, #105261, .T. ) ;
#52666 = EDGE_CURVE ( 'NONE', #132148, #80135, #19675, .T. ) ;
#52667 = FACE_BOUND ( 'NONE', #119731, .T. ) ;
#52668 = LINE ( 'NONE', #88174, #40938 ) ;
#52669 = DIRECTION ( 'NONE',  ( 0.6830127018922180770, -0.6830127018922204085, -0.2588190451025213501 ) ) ;
#52670 = DIRECTION ( 'NONE',  ( -0.7071067811865486830, 0.7071067811865464625, 0.000000000000000000 ) ) ;
#52671 = AXIS2_PLACEMENT_3D ( 'NONE', #12606, #14755, #92297 ) ;
#52672 = DIRECTION ( 'NONE',  ( 0.7071067811865486830, -0.7071067811865464625, -0.000000000000000000 ) ) ;
#52673 = EDGE_CURVE ( 'NONE', #78369, #19810, #20370, .T. ) ;
#52674 = CARTESIAN_POINT ( 'NONE',  ( -4.499999999999972466, 18.43112307739199451, 4.000000000000000000 ) ) ;
#52675 = ORIENTED_EDGE ( 'NONE', *, *, #106127, .T. ) ;
#52676 = CIRCLE ( 'NONE', #124397, 0.5000000000000004441 ) ;
#52677 = ORIENTED_EDGE ( 'NONE', *, *, #100955, .F. ) ;
#52678 =( BOUNDED_CURVE ( )  B_SPLINE_CURVE ( 2, ( #80886, #1824, #133138, #33816, #45422, #22879, #35258, #67148, #111340, #100496, #1141, #89598, #133828 ),
 .UNSPECIFIED., .F., .T. ) 
 B_SPLINE_CURVE_WITH_KNOTS ( ( 3, 2, 2, 2, 2, 2, 3 ),
 ( 0.1500000000000000222, 0.1583333333333333537, 0.1666666666666666852, 0.1750000000000000444, 0.1833333333333333759, 0.1916666666666667351, 0.2000000000000000666 ),
 .UNSPECIFIED. ) 
 CURVE ( )  GEOMETRIC_REPRESENTATION_ITEM ( )  RATIONAL_B_SPLINE_CURVE ( ( 0.9999999999999998890, 0.9659258262890684232, 1.000000000000000000, 0.9659258262890683122, 1.000000000000000000, 0.9659258262890683122, 1.000000000000000000, 0.9659258262890683122, 1.000000000000000000, 0.9659258262890683122, 1.000000000000000000, 0.9659258262890680902, 1.000000000000000222 ) ) 
 REPRESENTATION_ITEM ( '' )  );
#52679 = VERTEX_POINT ( 'NONE', #129150 ) ;
#52680 = ORIENTED_EDGE ( 'NONE', *, *, #116687, .T. ) ;
#52681 = CARTESIAN_POINT ( 'NONE',  ( 183.9257687383401105, -48.73293412427400284, 38.67339632249573356 ) ) ;
#52682 = CARTESIAN_POINT ( 'NONE',  ( 34.92499999999998295, -13.91861162105995753, 18.69616556237237504 ) ) ;
#52683 = CARTESIAN_POINT ( 'NONE',  ( 60.48921356237309510, -27.52281430457097500, 5.000000000000000000 ) ) ;
#52684 = ORIENTED_EDGE ( 'NONE', *, *, #5394, .F. ) ;
#52685 = CARTESIAN_POINT ( 'NONE',  ( -32.56319896779150724, -12.74070752338415247, 9.898150129686451137 ) ) ;
#52686 = DIRECTION ( 'NONE',  ( -0.6830127018922180770, -0.6830127018922204085, -0.2588190451025213501 ) ) ;
#52687 = EDGE_CURVE ( 'NONE', #33206, #97401, #64614, .T. ) ;
#52688 = LINE ( 'NONE', #7003, #48489 ) ;
#52689 = CARTESIAN_POINT ( 'NONE',  ( 1.252729709573792150, 0.4274928414560493217, 3.798934289757320837 ) ) ;
#52690 = ORIENTED_EDGE ( 'NONE', *, *, #18226, .F. ) ;
#52691 = CARTESIAN_POINT ( 'NONE',  ( 36.18398860626899705, 28.73617430169812437, 5.000000000000000000 ) ) ;
#52692 = CARTESIAN_POINT ( 'NONE',  ( 0.1161069444170889225, -0.4000000000000003553, 2.220360628129160130 ) ) ;
#52693 = ORIENTED_EDGE ( 'NONE', *, *, #106186, .T. ) ;
#52694 = FACE_OUTER_BOUND ( 'NONE', #142900, .T. ) ;
#52695 = ORIENTED_EDGE ( 'NONE', *, *, #22794, .T. ) ;
#52696 = ORIENTED_EDGE ( 'NONE', *, *, #87561, .F. ) ;
#52697 = ORIENTED_EDGE ( 'NONE', *, *, #78441, .T. ) ;
#52698 = CARTESIAN_POINT ( 'NONE',  ( 67.08376352523143282, -6.110000000000001208, -3.741295971395164515E-16 ) ) ;
#52699 = VERTEX_POINT ( 'NONE', #62487 ) ;
#52700 = ORIENTED_EDGE ( 'NONE', *, *, #75296, .T. ) ;
#52701 = EDGE_CURVE ( 'NONE', #3406, #142587, #31982, .T. ) ;
#52702 = CARTESIAN_POINT ( 'NONE',  ( 28.22674160717816960, -11.24070752338416490, 18.24660765846989108 ) ) ;
#52703 = FACE_OUTER_BOUND ( 'NONE', #42407, .T. ) ;
#52704 = VECTOR ( 'NONE', #104386, 1000.000000000000000 ) ;
#52705 = CARTESIAN_POINT ( 'NONE',  ( 101.5004301918981042, -3.055000000000002380, 5.291415217122920289 ) ) ;
#52706 = CARTESIAN_POINT ( 'NONE',  ( -12.18398860626900060, 28.73617430169795739, 5.000000000000000000 ) ) ;
#52707 = ADVANCED_FACE ( 'NONE', ( #142198 ), #18215, .F. ) ;
#52708 = EDGE_LOOP ( 'NONE', ( #65188, #95186, #128986, #59597 ) ) ;
#52709 = CARTESIAN_POINT ( 'NONE',  ( 7.499999999999944045, -9.462702396501008195, -9.474982329943534509 ) ) ;
#52710 = CARTESIAN_POINT ( 'NONE',  ( 23.99999999999984013, -19.44781430457063465, 5.000000000000000000 ) ) ;
#52711 = CARTESIAN_POINT ( 'NONE',  ( 90.68750000000001421, -5.819803920172573974, 5.819803920172573086 ) ) ;
#52712 = CARTESIAN_POINT ( 'NONE',  ( -20.99999999999985079, 17.96639925780207747, 5.000000000000000000 ) ) ;
#52713 = EDGE_LOOP ( 'NONE', ( #100873, #45946, #9609, #75652 ) ) ;
#52714 = DIRECTION ( 'NONE',  ( -0.000000000000000000, -0.000000000000000000, 1.000000000000000000 ) ) ;
#52715 = EDGE_CURVE ( 'NONE', #8196, #126872, #63232, .T. ) ;
#52716 = ORIENTED_EDGE ( 'NONE', *, *, #9230, .F. ) ;
#52717 = ORIENTED_EDGE ( 'NONE', *, *, #111717, .F. ) ;
#52718 = EDGE_LOOP ( 'NONE', ( #9688, #29944, #34732, #119963 ) ) ;
#52719 = CARTESIAN_POINT ( 'NONE',  ( 125.9120968585647802, 5.291415217122921177, -3.054999999999994831 ) ) ;
#52720 = ORIENTED_EDGE ( 'NONE', *, *, #120004, .F. ) ;
#52721 = AXIS2_PLACEMENT_3D ( 'NONE', #99797, #133172, #469 ) ;
#52722 = DIRECTION ( 'NONE',  ( 0.7071067811865486830, -0.7071067811865464625, -0.000000000000000000 ) ) ;
#52723 = DIRECTION ( 'NONE',  ( -0.6830127018922180770, -0.6830127018922204085, -0.2588190451025213501 ) ) ;
#52724 = STYLED_ITEM ( 'NONE', ( #107755 ), #111895 ) ;
#52725 = EDGE_CURVE ( 'NONE', #18615, #58810, #7354, .T. ) ;
#52726 = CARTESIAN_POINT ( 'NONE',  ( -2.999999999999975131, 5.587461875839191627, 4.000000000000000000 ) ) ;
#52727 = ORIENTED_EDGE ( 'NONE', *, *, #101580, .F. ) ;
#52728 = CARTESIAN_POINT ( 'NONE',  ( 3.340980275923999709, -49.02095135882318999, 39.67421197283140089 ) ) ;
#52729 = ORIENTED_EDGE ( 'NONE', *, *, #83462, .T. ) ;
#52730 = AXIS2_PLACEMENT_3D ( 'NONE', #130544, #119614, #64553 ) ;
#52731 = AXIS2_PLACEMENT_3D ( 'NONE', #134933, #46515, #14545 ) ;
#52732 = CARTESIAN_POINT ( 'NONE',  ( 3.916236474768552522, -7.934999999999990727, 4.858786175617117713E-16 ) ) ;
#52733 = SURFACE_STYLE_USAGE ( .BOTH. , #142621 ) ;
#52734 = DIRECTION ( 'NONE',  ( 0.000000000000000000, 1.000000000000000000, 0.000000000000000000 ) ) ;
#52735 = CARTESIAN_POINT ( 'NONE',  ( 10.46945953031644372, -8.432637487761466488, -4.375000000000003553 ) ) ;
#52736 = ORIENTED_EDGE ( 'NONE', *, *, #116301, .F. ) ;
#52737 = ORIENTED_EDGE ( 'NONE', *, *, #14416, .T. ) ;
#52738 = ORIENTED_EDGE ( 'NONE', *, *, #115448, .T. ) ;
#52739 = DIRECTION ( 'NONE',  ( -0.7071067811865486830, -0.7071067811865464625, 0.000000000000000000 ) ) ;
#52740 = DIRECTION ( 'NONE',  ( 0.6830127018922180770, -0.6830127018922204085, -0.2588190451025213501 ) ) ;
#52741 = LINE ( 'NONE', #86109, #112158 ) ;
#52742 = PLANE ( 'NONE',  #99173 ) ;
#52743 = LINE ( 'NONE', #84680, #85073 ) ;
#52744 = DIRECTION ( 'NONE',  ( 0.7071067811865487940, 0.7071067811865463515, 0.000000000000000000 ) ) ;
#52745 = ADVANCED_FACE ( 'NONE', ( #29828 ), #140731, .F. ) ;
#52746 = CARTESIAN_POINT ( 'NONE',  ( 32.52126352523142572, -4.472830434245839371, -4.472830434245840259 ) ) ;
#52747 = DIRECTION ( 'NONE',  ( 0.6830127018922180770, -0.6830127018922204085, -0.2588190451025213501 ) ) ;
#52748 = CYLINDRICAL_SURFACE ( 'NONE', #37373, 4.000000000000000000 ) ;
#52749 = ORIENTED_EDGE ( 'NONE', *, *, #56951, .T. ) ;
#52750 = PLANE ( 'NONE',  #74288 ) ;
#52751 = FACE_OUTER_BOUND ( 'NONE', #114051, .T. ) ;
#52752 = ORIENTED_EDGE ( 'NONE', *, *, #89164, .F. ) ;
#52753 = DIRECTION ( 'NONE',  ( 0.000000000000000000, 0.000000000000000000, 1.000000000000000000 ) ) ;
#52755 = EDGE_LOOP ( 'NONE', ( #137439, #6906, #87980, #143497 ) ) ;
#52754 = CARTESIAN_POINT ( 'NONE',  ( 42.27083333333332149, -7.949999999999998401, -2.130196079827426203 ) ) ;
#52756 = EDGE_CURVE ( 'NONE', #76898, #136430, #85635, .T. ) ;
#52757 = DIRECTION ( 'NONE',  ( 0.7071067811865486830, -0.7071067811865464625, -0.000000000000000000 ) ) ;
#52758 = ORIENTED_EDGE ( 'NONE', *, *, #64465, .F. ) ;
#52760 = VECTOR ( 'NONE', #86955, 1000.000000000000227 ) ;
#52759 = PLANE ( 'NONE',  #69326 ) ;
#52761 = ORIENTED_EDGE ( 'NONE', *, *, #133863, .T. ) ;
#52762 = CARTESIAN_POINT ( 'NONE',  ( -17.20710678118642178, 15.75929247661555976, 5.000000000000000000 ) ) ;
#52763 = EDGE_LOOP ( 'NONE', ( #42651, #24739, #40559, #68721, #90818 ) ) ;
#52764 = PRESENTATION_STYLE_ASSIGNMENT (( #63689 ) ) ;
#52765 = CARTESIAN_POINT ( 'NONE',  ( 126.5166937171295700, 7.950000000000001066, -2.130196079827421318 ) ) ;
#52766 = DIRECTION ( 'NONE',  ( 0.6830127018922180770, -0.6830127018922204085, -0.2588190451025213501 ) ) ;
#52767 = LINE ( 'NONE', #20857, #76376 ) ;
#52768 = CARTESIAN_POINT ( 'NONE',  ( 78.18398860626899705, 28.73617430169841924, 5.000000000000000000 ) ) ;
#52769 = CARTESIAN_POINT ( 'NONE',  ( 31.92500000000001492, -7.729999999999995985, 3.180000000000000160 ) ) ;
#52770 = DIRECTION ( 'NONE',  ( -0.3543493200069162685, -0.000000000000000000, -0.9351131265310288487 ) ) ;
#52771 = CARTESIAN_POINT ( 'NONE',  ( 0.5833333333333334814, -5.278424836066144543, 3.047499999999995879 ) ) ;
#52772 = CARTESIAN_POINT ( 'NONE',  ( 19.08290314143522437, 3.967499999999992699, -6.871911579029513994 ) ) ;
#52773 = PLANE ( 'NONE',  #69879 ) ;
#52774 = DIRECTION ( 'NONE',  ( -0.000000000000000000, -0.000000000000000000, -1.000000000000000000 ) ) ;
#52775 = ORIENTED_EDGE ( 'NONE', *, *, #51503, .T. ) ;
#52776 = EDGE_CURVE ( 'NONE', #74522, #84400, #87084, .T. ) ;
#52778 = VERTEX_POINT ( 'NONE', #108080 ) ;
#52777 = AXIS2_PLACEMENT_3D ( 'NONE', #71335, #140835, #93788 ) ;
#52779 = CARTESIAN_POINT ( 'NONE',  ( -17.99999999999987210, -8.731860332648849976, -2.120594902707582108 ) ) ;
#52780 = ORIENTED_EDGE ( 'NONE', *, *, #26235, .F. ) ;
#52781 = DIRECTION ( 'NONE',  ( -0.7071067811865486830, 0.7071067811865464625, 0.000000000000000000 ) ) ;
#52782 = SURFACE_SIDE_STYLE ('',( #53528 ) ) ;
#52783 = DIRECTION ( 'NONE',  ( -0.000000000000000000, 0.3543493200069153248, 0.9351131265310292928 ) ) ;
#52784 = ORIENTED_EDGE ( 'NONE', *, *, #13700, .F. ) ;
#52785 = CARTESIAN_POINT ( 'NONE',  ( 31.92500000000001492, -7.729999999999995985, 3.180000000000000160 ) ) ;
#52786 = DIRECTION ( 'NONE',  ( -0.7071067811865487940, 0.7071067811865463515, -0.000000000000000000 ) ) ;
#52787 = FILL_AREA_STYLE_COLOUR ( '', #5449 ) ;
#52789 = ORIENTED_EDGE ( 'NONE', *, *, #118915, .F. ) ;
#52788 = DIRECTION ( 'NONE',  ( -0.000000000000000000, 0.000000000000000000, 1.000000000000000000 ) ) ;
#52790 = CARTESIAN_POINT ( 'NONE',  ( 39.79166666666665719, 3.975000000000003642, -6.884901960086285300 ) ) ;
#52791 = CARTESIAN_POINT ( 'NONE',  ( 70.56250000000000000, -5.819803920172573086, -5.819803920172573974 ) ) ;
#52792 = CARTESIAN_POINT ( 'NONE',  ( 84.29974487139159578, -27.71228299555264840, 4.000000000000000000 ) ) ;
#52793 = DIRECTION ( 'NONE',  ( 0.000000000000000000, -1.000000000000000000, 0.000000000000000000 ) ) ;
#52794 = CARTESIAN_POINT ( 'NONE',  ( 57.48282408945818389, -47.13357697190487983, 36.34567044386079715 ) ) ;
#52795 = EDGE_LOOP ( 'NONE', ( #15410, #38424, #26263, #135073, #38387 ) ) ;
#52796 = ORIENTED_EDGE ( 'NONE', *, *, #56857, .T. ) ;
#52797 = VERTEX_POINT ( 'NONE', #141467 ) ;
#52798 = EDGE_CURVE ( 'NONE', #38188, #46353, #74812, .T. ) ;
#52799 = CARTESIAN_POINT ( 'NONE',  ( 103.8337635252314328, 6.110000000000001208, 1.122388791418549305E-15 ) ) ;
#52800 = ORIENTED_EDGE ( 'NONE', *, *, #13040, .F. ) ;
#52801 = EDGE_CURVE ( 'NONE', #58810, #49145, #8747, .T. ) ;
#52802 = CARTESIAN_POINT ( 'NONE',  ( 126.6671759105294939, -47.13357697190737383, 36.34567044387055290 ) ) ;
#52803 = EDGE_CURVE ( 'NONE', #95099, #136867, #76210, .T. ) ;
#52804 = CARTESIAN_POINT ( 'NONE',  ( 84.51669371712955581, 7.950000000000000178, -2.130196079827421318 ) ) ;
#52805 = ORIENTED_EDGE ( 'NONE', *, *, #84750, .F. ) ;
#52806 = EDGE_CURVE ( 'NONE', #18405, #83571, #42172, .T. ) ;
#52807 = DIRECTION ( 'NONE',  ( 0.000000000000000000, 1.000000000000000000, 0.000000000000000000 ) ) ;
#52808 = FACE_OUTER_BOUND ( 'NONE', #131106, .T. ) ;
#52809 = CARTESIAN_POINT ( 'NONE',  ( 97.32876352523145158, 0.000000000000000000, -6.109999999999998543 ) ) ;
#52810 = ORIENTED_EDGE ( 'NONE', *, *, #61812, .T. ) ;
#52811 = LINE ( 'NONE', #8565, #9468 ) ;
#52812 = CARTESIAN_POINT ( 'NONE',  ( 18.29974487139159223, -27.71228299555219010, 4.000000000000000000 ) ) ;
#52813 = CARTESIAN_POINT ( 'NONE',  ( 3.183988606268992161, 28.73617430169789699, 5.000000000000000000 ) ) ;
#52814 = LINE ( 'NONE', #8569, #6840 ) ;
#52815 = VERTEX_POINT ( 'NONE', #120374 ) ;
#52816 = ORIENTED_EDGE ( 'NONE', *, *, #60056, .F. ) ;
#52817 = VECTOR ( 'NONE', #73559, 1000.000000000000000 ) ;
#52818 = EDGE_CURVE ( 'NONE', #53423, #26730, #73371, .T. ) ;
#52819 = ORIENTED_EDGE ( 'NONE', *, *, #38986, .F. ) ;
#52820 = CARTESIAN_POINT ( 'NONE',  ( -23.70025512860841133, -27.71228299555189523, 4.000000000000000000 ) ) ;
#52821 = ADVANCED_FACE ( 'NONE', ( #41776 ), #77291, .F. ) ;
#52822 = LINE ( 'NONE', #120950, #50160 ) ;
#52823 = CARTESIAN_POINT ( 'NONE',  ( 20.48373647476854842, -5.808823158059035485, -5.808823158059033709 ) ) ;
#52824 = VECTOR ( 'NONE', #19014, 1000.000000000000000 ) ;
#52825 = VECTOR ( 'NONE', #49167, 1000.000000000000114 ) ;
#52826 = DIRECTION ( 'NONE',  ( 0.3543493200069162685, -0.000000000000000000, -0.9351131265310288487 ) ) ;
#52827 = EDGE_CURVE ( 'NONE', #6574, #85157, #19304, .T. ) ;
#52828 = DIRECTION ( 'NONE',  ( 0.000000000000000000, 0.000000000000000000, 1.000000000000000000 ) ) ;
#52829 = ORIENTED_EDGE ( 'NONE', *, *, #137133, .T. ) ;
#52830 = ORIENTED_EDGE ( 'NONE', *, *, #56498, .F. ) ;
#52831 = CARTESIAN_POINT ( 'NONE',  ( 36.47336096364193736, -5.240707523384221744, 16.25846745537504034 ) ) ;
#52832 = EDGE_LOOP ( 'NONE', ( #16384, #117866, #102042, #127253 ) ) ;
#52833 = ORIENTED_EDGE ( 'NONE', *, *, #28110, .T. ) ;
#52834 = EDGE_CURVE ( 'NONE', #41149, #16173, #53352, .T. ) ;
#52835 = STYLED_ITEM ( 'NONE', ( #122650 ), #46908 ) ;
#52836 = CARTESIAN_POINT ( 'NONE',  ( 17.79166666666666785, -3.047499999999994547, 5.278424836066145431 ) ) ;
#52837 = LINE ( 'NONE', #32552, #77532 ) ;
#52838 = VERTEX_POINT ( 'NONE', #54114 ) ;
#52839 = DIRECTION ( 'NONE',  ( -0.7071067811865486830, -0.7071067811865464625, -0.000000000000000000 ) ) ;
#52840 = SURFACE_SIDE_STYLE ('',( #118830 ) ) ;
#52841 = DIRECTION ( 'NONE',  ( 0.6830127018922180770, -0.6830127018922204085, -0.2588190451025213501 ) ) ;
#52842 = EDGE_CURVE ( 'NONE', #140745, #117806, #63560, .T. ) ;
#52843 = CARTESIAN_POINT ( 'NONE',  ( 21.43680103220816591, -12.74070752338415247, 9.898150129686325016 ) ) ;
#52844 = ORIENTED_EDGE ( 'NONE', *, *, #67548, .F. ) ;
#52845 = VECTOR ( 'NONE', #97305, 1000.000000000000000 ) ;
#52846 = PRESENTATION_STYLE_ASSIGNMENT (( #76060 ) ) ;
#52847 = CONICAL_SURFACE ( 'NONE', #48324, 2.552699999999994418, 1.029744258676651869 ) ;
#52848 = ORIENTED_EDGE ( 'NONE', *, *, #95616, .F. ) ;
#52849 = CARTESIAN_POINT ( 'NONE',  ( 25.39999999999999503, 5.312365556086702689, -5.908453331706006395 ) ) ;
#52850 = DIRECTION ( 'NONE',  ( 0.7071067811865487940, 0.7071067811865463515, -0.000000000000000000 ) ) ;
#52851 = ORIENTED_EDGE ( 'NONE', *, *, #73633, .F. ) ;
#52852 = FACE_OUTER_BOUND ( 'NONE', #54849, .T. ) ;
#52853 = VERTEX_POINT ( 'NONE', #380 ) ;
#52854 = CARTESIAN_POINT ( 'NONE',  ( 32.99999999999976552, -18.41253812416056945, 4.000000000000000000 ) ) ;
#52855 = EDGE_LOOP ( 'NONE', ( #96053, #122600, #72149, #111706 ) ) ;
#52856 = VERTEX_POINT ( 'NONE', #87428 ) ;
#52857 = VERTEX_POINT ( 'NONE', #130223 ) ;
#52858 = ADVANCED_FACE ( 'NONE', ( #98987 ), #132386, .T. ) ;
#52859 = CARTESIAN_POINT ( 'NONE',  ( 32.14126352523144448, 4.472830434245835818, 4.472830434245840259 ) ) ;
#52860 = CARTESIAN_POINT ( 'NONE',  ( 1.171830600776465392, 0.7592924766157086447, 4.000000000000000000 ) ) ;
#52861 = CARTESIAN_POINT ( 'NONE',  ( 34.92499999999998295, 8.947904407527573767, 10.03118784388415463 ) ) ;
#52862 = CARTESIAN_POINT ( 'NONE',  ( 124.1045968585647756, 1.637169565754164946, -6.109999999999999432 ) ) ;
#52863 = DIRECTION ( 'NONE',  ( -0.7071067811865486830, 0.7071067811865464625, 0.000000000000000000 ) ) ;
#52864 = DIRECTION ( 'NONE',  ( -0.000000000000000000, -0.3543493200069152693, 0.9351131265310292928 ) ) ;
#52865 = DIRECTION ( 'NONE',  ( 0.6830127018922181881, 0.6830127018922202975, -0.2588190451025214056 ) ) ;
#52866 = VECTOR ( 'NONE', #85496, 1000.000000000000000 ) ;
#52867 = CARTESIAN_POINT ( 'NONE',  ( -11.99451991528749417, 28.92564299267946382, 4.000000000000000000 ) ) ;
#52868 = FACE_OUTER_BOUND ( 'NONE', #99802, .T. ) ;
#52869 = CARTESIAN_POINT ( 'NONE',  ( 29.99999999999980460, -3.412538124160717778, 4.000000000000000000 ) ) ;
#52870 = LINE ( 'NONE', #97065, #93377 ) ;
#52871 = EDGE_CURVE ( 'NONE', #69590, #60184, #118606, .T. ) ;
#52872 = ORIENTED_EDGE ( 'NONE', *, *, #42876, .F. ) ;
#52873 = ORIENTED_EDGE ( 'NONE', *, *, #20016, .F. ) ;
#52874 = ORIENTED_EDGE ( 'NONE', *, *, #55806, .F. ) ;
#52875 = ORIENTED_EDGE ( 'NONE', *, *, #67119, .F. ) ;
#52876 = DIRECTION ( 'NONE',  ( 1.000000000000000000, 1.224606353822377258E-16, 0.000000000000000000 ) ) ;
#52877 = ORIENTED_EDGE ( 'NONE', *, *, #43677, .T. ) ;
#52878 = VERTEX_POINT ( 'NONE', #20714 ) ;
#52879 = DIRECTION ( 'NONE',  ( -0.6830127018922181881, 0.6830127018922202975, -0.2588190451025214056 ) ) ;
#52880 = LINE ( 'NONE', #86967, #62020 ) ;
#52881 = EDGE_CURVE ( 'NONE', #45028, #94854, #13820, .T. ) ;
#52882 = LINE ( 'NONE', #97850, #36986 ) ;
#52883 = ORIENTED_EDGE ( 'NONE', *, *, #48234, .F. ) ;
#52884 = CARTESIAN_POINT ( 'NONE',  ( 53.99451991528749062, 28.92564299267975869, 4.000000000000000000 ) ) ;
#52885 = ORIENTED_EDGE ( 'NONE', *, *, #52482, .T. ) ;
#52886 = CARTESIAN_POINT ( 'NONE',  ( 11.99999999999991296, -13.39766691384881803, -10.96608748226468677 ) ) ;
#52887 = CARTESIAN_POINT ( 'NONE',  ( 6.775403141435218934, -2.126176841940958351, -7.934999999999989839 ) ) ;
#52888 = VERTEX_POINT ( 'NONE', #109162 ) ;
#52889 = CARTESIAN_POINT ( 'NONE',  ( 90.18293019189809456, -1.637169565754159173, -6.109999999999999432 ) ) ;
#52890 = CARTESIAN_POINT ( 'NONE',  ( -21.18398860626899349, 28.73617430169802134, 5.000000000000000000 ) ) ;
#52891 = PLANE ( 'NONE',  #9660 ) ;
#52892 = CARTESIAN_POINT ( 'NONE',  ( 10.82816939922345156, 21.75929247661549581, 4.000000000000000000 ) ) ;
#52893 = ORIENTED_EDGE ( 'NONE', *, *, #236, .T. ) ;
#52894 = ORIENTED_EDGE ( 'NONE', *, *, #115466, .T. ) ;
#52895 = PLANE ( 'NONE',  #125935 ) ;
#52896 = VERTEX_POINT ( 'NONE', #19996 ) ;
#52897 = DIRECTION ( 'NONE',  ( -0.3543493200069162685, -0.000000000000000000, -0.9351131265310288487 ) ) ;
#52898 = CARTESIAN_POINT ( 'NONE',  ( -31.92499999999997584, 1.196650378695321315, -30.59010235425025215 ) ) ;
#52899 = CARTESIAN_POINT ( 'NONE',  ( -34.47516574401891631, -13.50948238788424938, 4.998110765256835286 ) ) ;
#52900 = LINE ( 'NONE', #65267, #93520 ) ;
#52901 = EDGE_LOOP ( 'NONE', ( #48557, #36617, #54894, #66743, #111542 ) ) ;
#52902 = PLANE ( 'NONE',  #83160 ) ;
#52903 = VECTOR ( 'NONE', #6518, 1000.000000000000227 ) ;
#52904 = EDGE_CURVE ( 'NONE', #20428, #62928, #64242, .T. ) ;
#52906 = EDGE_CURVE ( 'NONE', #79378, #85671, #65714, .T. ) ;
#52905 = DIRECTION ( 'NONE',  ( 1.224646799147353207E-16, 0.000000000000000000, -1.000000000000000000 ) ) ;
#52907 = LINE ( 'NONE', #29736, #132516 ) ;
#52908 = ORIENTED_EDGE ( 'NONE', *, *, #69367, .T. ) ;
#52909 = CARTESIAN_POINT ( 'NONE',  ( -12.20000000000000817, -1.670812611072399357E-15, -0.5000000000000000000 ) ) ;
#52910 = VECTOR ( 'NONE', #21672, 1000.000000000000000 ) ;
#52911 = VECTOR ( 'NONE', #98406, 999.9999999999998863 ) ;
#52912 = VECTOR ( 'NONE', #139191, 1000.000000000000227 ) ;
#52913 = PLANE ( 'NONE',  #61041 ) ;
#52914 = ORIENTED_EDGE ( 'NONE', *, *, #83986, .T. ) ;
#52915 = VECTOR ( 'NONE', #126327, 1000.000000000000227 ) ;
#52916 = ADVANCED_FACE ( 'NONE', ( #42514 ), #31615, .F. ) ;
#52918 = ORIENTED_EDGE ( 'NONE', *, *, #57658, .T. ) ;
#52917 = CARTESIAN_POINT ( 'NONE',  ( 0.5457257104438988371, -52.10338527932239572, -40.45859298138255866 ) ) ;
#52919 = EDGE_LOOP ( 'NONE', ( #103500, #39234, #8859, #142174 ) ) ;
#52920 = EDGE_CURVE ( 'NONE', #31963, #141805, #110564, .T. ) ;
#52921 = CARTESIAN_POINT ( 'NONE',  ( -18.18398860626898994, 28.73617430169800002, 5.000000000000000000 ) ) ;
#52922 = DIRECTION ( 'NONE',  ( 0.6830127018922180770, -0.6830127018922204085, -0.2588190451025213501 ) ) ;
#52923 = VECTOR ( 'NONE', #137786, 1000.000000000000000 ) ;
#52924 = ORIENTED_EDGE ( 'NONE', *, *, #120053, .F. ) ;
#52925 = CARTESIAN_POINT ( 'NONE',  ( -7.499999999999944045, 19.46639925780207392, 5.000000000000000000 ) ) ;
#52926 = VECTOR ( 'NONE', #61890, 999.9999999999998863 ) ;
#52927 = CARTESIAN_POINT ( 'NONE',  ( -19.49999999999985789, -7.420205493532915142, -2.617629953481298788 ) ) ;
#52928 = CARTESIAN_POINT ( 'NONE',  ( -24.46160355370555806, -9.740707523384173783, 17.74957260769605227 ) ) ;
#52929 = EDGE_CURVE ( 'NONE', #105140, #6561, #4503, .T. ) ;
#52930 = LINE ( 'NONE', #97131, #115542 ) ;
#52931 = DIRECTION ( 'NONE',  ( 0.3543493200069163795, -9.265275131829747941E-33, -0.9351131265310288487 ) ) ;
#52932 = DIRECTION ( 'NONE',  ( -0.000000000000000000, 1.301042606982605074E-16, -1.000000000000000000 ) ) ;
#52933 = DIRECTION ( 'NONE',  ( -1.000000000000000000, -3.560121055573109579E-15, 0.000000000000000000 ) ) ;
#52934 = CARTESIAN_POINT ( 'NONE',  ( 0.000000000000000000, 0.000000000000000000, 0.000000000000000000 ) ) ;
#52935 = DIRECTION ( 'NONE',  ( -0.6830127018922180770, -0.6830127018922204085, -0.2588190451025213501 ) ) ;
#52937 = VECTOR ( 'NONE', #76883, 1000.000000000000000 ) ;
#52936 = CARTESIAN_POINT ( 'NONE',  ( 0.4892135623730947680, -27.52281430457055578, 5.000000000000000000 ) ) ;
#52938 = DIRECTION ( 'NONE',  ( 0.7071067811865487940, -0.7071067811865463515, 0.000000000000000000 ) ) ;
#52939 = CARTESIAN_POINT ( 'NONE',  ( 54.29974487139159578, -27.71228299555243879, 4.000000000000000000 ) ) ;
#52940 = DIRECTION ( 'NONE',  ( -0.7071067811865486830, -0.7071067811865464625, -0.000000000000000000 ) ) ;
#52941 = ORIENTED_EDGE ( 'NONE', *, *, #34237, .T. ) ;
#52942 = EDGE_CURVE ( 'NONE', #23280, #2318, #88867, .T. ) ;
#52943 =( BOUNDED_CURVE ( )  B_SPLINE_CURVE ( 3, ( #141431, #68891, #2136, #34112 ),
 .UNSPECIFIED., .F., .F. ) 
 B_SPLINE_CURVE_WITH_KNOTS ( ( 4, 4 ),
 ( 2.356194490192346613, 2.506762762968578695 ),
 .UNSPECIFIED. ) 
 CURVE ( )  GEOMETRIC_REPRESENTATION_ITEM ( )  RATIONAL_B_SPLINE_CURVE ( ( 1.000000000000000000, 0.9981116584018945304, 0.9981116584018945304, 1.000000000000000000 ) ) 
 REPRESENTATION_ITEM ( '' )  );
#52944 = VERTEX_POINT ( 'NONE', #109877 ) ;
#52945 = ORIENTED_EDGE ( 'NONE', *, *, #105650, .F. ) ;
#52946 = CARTESIAN_POINT ( 'NONE',  ( 112.8541666666666572, -2.130196079827425315, -7.950000000000001066 ) ) ;
#52947 = AXIS2_PLACEMENT_3D ( 'NONE', #82408, #18529, #103408 ) ;
#52948 = ORIENTED_EDGE ( 'NONE', *, *, #56043, .F. ) ;
#52949 = ORIENTED_EDGE ( 'NONE', *, *, #58748, .F. ) ;
#52950 = EDGE_LOOP ( 'NONE', ( #66363, #1716, #74333, #24895 ) ) ;
#52951 = LINE ( 'NONE', #120330, #61836 ) ;
#52952 = VECTOR ( 'NONE', #39251, 1000.000000000000000 ) ;
#52953 = CARTESIAN_POINT ( 'NONE',  ( 8.292893218813400580, 8.259292476615630818, 5.000000000000000000 ) ) ;
#52954 = ORIENTED_EDGE ( 'NONE', *, *, #52586, .F. ) ;
#52955 = CIRCLE ( 'NONE', #134010, 0.5000000000000000000 ) ;
#52956 =( BOUNDED_CURVE ( )  B_SPLINE_CURVE ( 3, ( #89072, #141277, #19504, #131133 ),
 .UNSPECIFIED., .F., .T. ) 
 B_SPLINE_CURVE_WITH_KNOTS ( ( 4, 4 ),
 ( 4.712388980384696779, 6.283185307179586232 ),
 .UNSPECIFIED. ) 
 CURVE ( )  GEOMETRIC_REPRESENTATION_ITEM ( )  RATIONAL_B_SPLINE_CURVE ( ( 1.000000000000000000, 0.8047378541243667138, 0.8047378541243667138, 1.000000000000000000 ) ) 
 REPRESENTATION_ITEM ( '' )  );
#52957 = DIRECTION ( 'NONE',  ( -0.7071067811865486830, -0.7071067811865464625, 0.000000000000000000 ) ) ;
#52958 = AXIS2_PLACEMENT_3D ( 'NONE', #41913, #84691, #52753 ) ;
#52959 = LINE ( 'NONE', #30533, #115875 ) ;
#52960 = VECTOR ( 'NONE', #83837, 999.9999999999998863 ) ;
#52961 = FACE_OUTER_BOUND ( 'NONE', #138967, .T. ) ;
#52962 = DIRECTION ( 'NONE',  ( 1.000000000000000000, 0.000000000000000000, 0.000000000000000000 ) ) ;
#52963 = CARTESIAN_POINT ( 'NONE',  ( 101.0629301918980900, 1.637169565754157174, 6.110000000000002984 ) ) ;
#52964 = ORIENTED_EDGE ( 'NONE', *, *, #9230, .T. ) ;
#52965 = CARTESIAN_POINT ( 'NONE',  ( 1.868077901080408498, 12.49629736921268552, -26.81958028572744723 ) ) ;
#52966 = CARTESIAN_POINT ( 'NONE',  ( 27.18398860626900060, 28.73617430169806042, 5.000000000000000000 ) ) ;
#52967 = CARTESIAN_POINT ( 'NONE',  ( -23.67183060077630685, -12.74070752338414891, 4.000000000000000000 ) ) ;
#52968 = VECTOR ( 'NONE', #110704, 1000.000000000000000 ) ;
#52969 = CARTESIAN_POINT ( 'NONE',  ( 22.25000000000000000, 0.000000000000000000, 0.000000000000000000 ) ) ;
#52970 = LINE ( 'NONE', #106626, #26114 ) ;
#52971 = CARTESIAN_POINT ( 'NONE',  ( 0.8681510425102002548, -0.5999999999999994227, -4.444131413071504610 ) ) ;
#52972 = VECTOR ( 'NONE', #94942, 1000.000000000000000 ) ;
#52973 = CARTESIAN_POINT ( 'NONE',  ( 31.43336038379622721, 2.130196079827431532, -7.949999999999997513 ) ) ;
#52974 = CARTESIAN_POINT ( 'NONE',  ( 7.139999999999992575, -35.13237070076360169, 17.62370837922859934 ) ) ;
#52975 = VERTEX_POINT ( 'NONE', #10542 ) ;
#52976 = ORIENTED_EDGE ( 'NONE', *, *, #66984, .T. ) ;
#52977 = ADVANCED_FACE ( 'NONE', ( #54804 ), #88143, .T. ) ;
#52978 = CARTESIAN_POINT ( 'NONE',  ( 26.52083333333332860, 7.949999999999999289, 2.130196079827431532 ) ) ;
#52979 = ORIENTED_EDGE ( 'NONE', *, *, #110348, .T. ) ;
#52980 = LINE ( 'NONE', #76193, #60249 ) ;
#52981 = EDGE_CURVE ( 'NONE', #46699, #133133, #18475, .T. ) ;
#52982 = LINE ( 'NONE', #31269, #36261 ) ;
#52983 = VECTOR ( 'NONE', #95182, 1000.000000000000000 ) ;
#52984 = DIRECTION ( 'NONE',  ( 0.000000000000000000, 0.000000000000000000, 1.000000000000000000 ) ) ;
#52986 = ADVANCED_FACE ( 'NONE', ( #122161 ), #1092, .F. ) ;
#52985 = DIRECTION ( 'NONE',  ( -0.3543493200069163240, 0.000000000000000000, 0.9351131265310288487 ) ) ;
#52987 = EDGE_CURVE ( 'NONE', #118149, #114653, #143514, .T. ) ;
#52988 = PRESENTATION_STYLE_ASSIGNMENT (( #72677 ) ) ;
#52989 = DIRECTION ( 'NONE',  ( 0.3543493200069162685, -0.000000000000000000, -0.9351131265310288487 ) ) ;
#52990 = CARTESIAN_POINT ( 'NONE',  ( 120.5162635252314374, -4.472830434245839371, 4.472830434245839371 ) ) ;
#52991 = ORIENTED_EDGE ( 'NONE', *, *, #58721, .T. ) ;
#52992 = PLANE ( 'NONE',  #22414 ) ;
#52993 = VERTEX_POINT ( 'NONE', #48197 ) ;
#52994 = CARTESIAN_POINT ( 'NONE',  ( -21.18398860626899349, 28.73617430169802134, 5.000000000000000000 ) ) ;
#52995 = LINE ( 'NONE', #66062, #64048 ) ;
#52996 = DIRECTION ( 'NONE',  ( 1.055184596092948005E-16, -1.000000000000000000, 0.000000000000000000 ) ) ;
#52997 = DIRECTION ( 'NONE',  ( 0.7071067811865486830, -0.7071067811865464625, -0.000000000000000000 ) ) ;
#52998 = ORIENTED_EDGE ( 'NONE', *, *, #26100, .T. ) ;
#53000 = EDGE_CURVE ( 'NONE', #103666, #118878, #11979, .T. ) ;
#52999 = CARTESIAN_POINT ( 'NONE',  ( 42.87543019189810423, -5.291415217122920289, -3.055000000000001492 ) ) ;
#53001 = EDGE_LOOP ( 'NONE', ( #22487, #50750, #115854, #51069 ) ) ;
#53002 = DIRECTION ( 'NONE',  ( -0.000000000000000000, 0.000000000000000000, 1.000000000000000000 ) ) ;
#53003 = EDGE_CURVE ( 'NONE', #55692, #46933, #69248, .T. ) ;
#53004 = CARTESIAN_POINT ( 'NONE',  ( -27.18398860626900060, 28.73617430169806042, 5.000000000000000000 ) ) ;
#53005 = DIRECTION ( 'NONE',  ( -0.000000000000000000, -0.3543493200069152693, 0.9351131265310292928 ) ) ;
#53006 = LINE ( 'NONE', #88526, #50765 ) ;
#53007 = EDGE_CURVE ( 'NONE', #16785, #97786, #123644, .T. ) ;
#53008 = CARTESIAN_POINT ( 'NONE',  ( 36.80793019189810167, -6.109999999999998543, 1.637169565754158063 ) ) ;
#53009 = ORIENTED_EDGE ( 'NONE', *, *, #41833, .F. ) ;
#53010 = CARTESIAN_POINT ( 'NONE',  ( -78.18398860626899705, 28.73617430169841924, 5.000000000000000000 ) ) ;
#53011 = ORIENTED_EDGE ( 'NONE', *, *, #63569, .F. ) ;
#53012 = ORIENTED_EDGE ( 'NONE', *, *, #59004, .F. ) ;
#53013 = EDGE_CURVE ( 'NONE', #51392, #70680, #103270, .T. ) ;
#53014 = ORIENTED_EDGE ( 'NONE', *, *, #65616, .F. ) ;
#53015 = VECTOR ( 'NONE', #43490, 1000.000000000000227 ) ;
#53016 = LINE ( 'NONE', #74086, #104695 ) ;
#53017 = EDGE_LOOP ( 'NONE', ( #126749, #107705, #84386, #61066, #72352 ) ) ;
#53018 = DIRECTION ( 'NONE',  ( -0.7071067811865486830, -0.7071067811865464625, 0.000000000000000000 ) ) ;
#53019 = LINE ( 'NONE', #117553, #80368 ) ;
#53020 = EDGE_CURVE ( 'NONE', #132991, #122347, #46081, .T. ) ;
#53021 = CARTESIAN_POINT ( 'NONE',  ( -11.72174548431420149, 8.259292476615637923, 11.78515199841147520 ) ) ;
#53022 = VECTOR ( 'NONE', #85861, 1000.000000000000227 ) ;
#53023 = VECTOR ( 'NONE', #91406, 1000.000000000000000 ) ;
#53024 = VECTOR ( 'NONE', #51790, 999.9999999999998863 ) ;
#53025 = DIRECTION ( 'NONE',  ( -0.6830127018922181881, 0.6830127018922202975, -0.2588190451025214056 ) ) ;
#53026 = VECTOR ( 'NONE', #7183, 1000.000000000000000 ) ;
#53027 = FACE_BOUND ( 'NONE', #96730, .T. ) ;
#53028 = VERTEX_POINT ( 'NONE', #77982 ) ;
#53029 = PLANE ( 'NONE',  #2729 ) ;
#53030 = PLANE ( 'NONE',  #11531 ) ;
#53031 = ORIENTED_EDGE ( 'NONE', *, *, #10429, .T. ) ;
#53032 = CARTESIAN_POINT ( 'NONE',  ( 21.18398860626899349, 28.73617430169802134, 5.000000000000000000 ) ) ;
#53033 = ORIENTED_EDGE ( 'NONE', *, *, #114547, .T. ) ;
#53034 = ADVANCED_FACE ( 'NONE', ( #111289 ), #45376, .F. ) ;
#53035 = VERTEX_POINT ( 'NONE', #14119 ) ;
#53036 = VECTOR ( 'NONE', #76887, 1000.000000000000227 ) ;
#53037 = DIRECTION ( 'NONE',  ( -0.7071067811865486830, -0.7071067811865464625, 0.000000000000000000 ) ) ;
#53038 = ORIENTED_EDGE ( 'NONE', *, *, #49505, .F. ) ;
#53039 = ADVANCED_FACE ( 'NONE', ( #68543 ), #56960, .F. ) ;
#53040 = CARTESIAN_POINT ( 'NONE',  ( 59.12043019189810877, 3.055000000000001936, -5.291415217122916737 ) ) ;
#53041 = ORIENTED_EDGE ( 'NONE', *, *, #67312, .T. ) ;
#53042 = DIRECTION ( 'NONE',  ( -0.000000000000000000, 1.000000000000000000, -0.000000000000000000 ) ) ;
#53043 = DIRECTION ( 'NONE',  ( 0.7071067811865486830, -0.7071067811865464625, -0.000000000000000000 ) ) ;
#53044 = ORIENTED_EDGE ( 'NONE', *, *, #49078, .F. ) ;
#53045 = DIRECTION ( 'NONE',  ( -0.000000000000000000, -0.3543493200069152693, 0.9351131265310292928 ) ) ;
#53046 = VECTOR ( 'NONE', #47661, 1000.000000000000000 ) ;
#53047 = VECTOR ( 'NONE', #45192, 999.9999999999998863 ) ;
#53048 = VECTOR ( 'NONE', #40869, 1000.000000000000000 ) ;
#53049 = DIRECTION ( 'NONE',  ( -0.7071067811865487940, 0.7071067811865463515, 0.000000000000000000 ) ) ;
#53050 = DIRECTION ( 'NONE',  ( 1.000000000000000000, -0.000000000000000000, 0.000000000000000000 ) ) ;
#53051 = CARTESIAN_POINT ( 'NONE',  ( 0.000000000000000000, -21.72500000000000142, 4.500000000000000888 ) ) ;
#53052 = PLANE ( 'NONE',  #42502 ) ;
#53053 = CARTESIAN_POINT ( 'NONE',  ( 34.42499999999998295, 21.72500000000000142, 0.4999999999999995559 ) ) ;
#53054 = ORIENTED_EDGE ( 'NONE', *, *, #61812, .F. ) ;
#53055 = EDGE_LOOP ( 'NONE', ( #72458, #28490, #103680, #20654 ) ) ;
#53056 = VECTOR ( 'NONE', #112734, 999.9999999999998863 ) ;
#53057 = FACE_OUTER_BOUND ( 'NONE', #123228, .T. ) ;
#53058 = FACE_OUTER_BOUND ( 'NONE', #110253, .T. ) ;
#53059 = VERTEX_POINT ( 'NONE', #91010 ) ;
#53060 = ORIENTED_EDGE ( 'NONE', *, *, #107533, .F. ) ;
#53061 = AXIS2_PLACEMENT_3D ( 'NONE', #108357, #117818, #18506 ) ;
#53062 = ORIENTED_EDGE ( 'NONE', *, *, #50133, .T. ) ;
#53063 = LINE ( 'NONE', #131360, #74512 ) ;
#53064 = CARTESIAN_POINT ( 'NONE',  ( -25.17183060077629975, 12.75929247661559174, 4.000000000000000000 ) ) ;
#53065 = CARTESIAN_POINT ( 'NONE',  ( 48.18398860626899705, 28.73617430169820608, 5.000000000000000000 ) ) ;
#53066 = EDGE_LOOP ( 'NONE', ( #85846, #90043, #4869, #92282 ) ) ;
#53067 = VECTOR ( 'NONE', #76546, 1000.000000000000000 ) ;
#53068 = DIRECTION ( 'NONE',  ( 0.7071067811865487940, 0.7071067811865463515, 0.000000000000000000 ) ) ;
#53069 = CONICAL_SURFACE ( 'NONE', #82908, 2.500000000000000888, 0.9599310885968822538 ) ;
#53070 = LINE ( 'NONE', #66830, #426 ) ;
#53071 = CARTESIAN_POINT ( 'NONE',  ( 15.67123647476855552, 0.000000000000000000, 7.934999999999990727 ) ) ;
#53072 = DIRECTION ( 'NONE',  ( -1.000000000000000000, -0.000000000000000000, -0.000000000000000000 ) ) ;
#53073 = VERTEX_POINT ( 'NONE', #134505 ) ;
#53074 = CARTESIAN_POINT ( 'NONE',  ( 119.2037635252314658, 6.109999999999999432, 1.122388791418549108E-15 ) ) ;
#53076 = EDGE_CURVE ( 'NONE', #130333, #109240, #89550, .T. ) ;
#53075 = PLANE ( 'NONE',  #106722 ) ;
#53077 = LINE ( 'NONE', #98038, #19430 ) ;
#53079 = VERTEX_POINT ( 'NONE', #102593 ) ;
#53078 = FACE_OUTER_BOUND ( 'NONE', #40680, .T. ) ;
#53080 = DIRECTION ( 'NONE',  ( -1.000000000000000000, -0.000000000000000000, -0.000000000000000000 ) ) ;
#53081 = VERTEX_POINT ( 'NONE', #47531 ) ;
#53082 = CARTESIAN_POINT ( 'NONE',  ( -72.18398860626899705, 28.73617430169837661, 5.000000000000000000 ) ) ;
#53083 = LINE ( 'NONE', #130692, #123424 ) ;
#53084 = DIRECTION ( 'NONE',  ( 0.7071067811865486830, -0.7071067811865464625, -0.000000000000000000 ) ) ;
#53085 = VERTEX_POINT ( 'NONE', #91691 ) ;
#53086 = EDGE_CURVE ( 'NONE', #111174, #64090, #135916, .T. ) ;
#53087 = FACE_OUTER_BOUND ( 'NONE', #13572, .T. ) ;
#53088 = DIRECTION ( 'NONE',  ( 1.000000000000000000, 1.224606353822377258E-16, 0.000000000000000000 ) ) ;
#53089 = ORIENTED_EDGE ( 'NONE', *, *, #133532, .F. ) ;
#53090 = LINE ( 'NONE', #99444, #2200 ) ;
#53091 = CARTESIAN_POINT ( 'NONE',  ( -3.005480084712505828, 28.92564299267936079, 4.000000000000000000 ) ) ;
#53092 = ORIENTED_EDGE ( 'NONE', *, *, #64744, .F. ) ;
#53093 = CARTESIAN_POINT ( 'NONE',  ( 3.791666666666666963, -3.047499999999994547, 5.278424836066145431 ) ) ;
#53094 = DIRECTION ( 'NONE',  ( 0.6830127018922181881, 0.6830127018922202975, -0.2588190451025214056 ) ) ;
#53095 = EDGE_CURVE ( 'NONE', #9707, #70234, #128950, .T. ) ;
#53096 = ORIENTED_EDGE ( 'NONE', *, *, #62026, .F. ) ;
#53097 = APPLICATION_CONTEXT ( 'automotive_design' ) ;
#53099 = ORIENTED_EDGE ( 'NONE', *, *, #84317, .T. ) ;
#53098 = EDGE_CURVE ( 'NONE', #130142, #139208, #13393, .T. ) ;
#53100 = CARTESIAN_POINT ( 'NONE',  ( 0.2569208697893817228, -2.055000000000000160, 0.000000000000000000 ) ) ;
#53101 = DIRECTION ( 'NONE',  ( -0.000000000000000000, 0.3543493200069153248, 0.9351131265310292928 ) ) ;
#53102 = ADVANCED_FACE ( 'NONE', ( #23580 ), #112037, .F. ) ;
#53103 = CARTESIAN_POINT ( 'NONE',  ( 15.58290314143522082, 3.967499999999992699, -6.871911579029513994 ) ) ;
#53104 =( LENGTH_UNIT ( ) NAMED_UNIT ( * ) SI_UNIT ( .MILLI., .METRE. ) );
#53105 = DIRECTION ( 'NONE',  ( -1.000000000000000000, -1.224606353822377258E-16, -0.000000000000000000 ) ) ;
#53106 = CARTESIAN_POINT ( 'NONE',  ( 150.3000000000000114, 5.817072295949924468E-16, -4.749999999999997335 ) ) ;
#53107 = ORIENTED_EDGE ( 'NONE', *, *, #6623, .T. ) ;
#53108 = EDGE_CURVE ( 'NONE', #17366, #18293, #79448, .T. ) ;
#53109 = FILL_AREA_STYLE ('',( #85746 ) ) ;
#53110 = CARTESIAN_POINT ( 'NONE',  ( -84.18398860626899705, 28.73617430169846187, 5.000000000000000000 ) ) ;
#53111 = CARTESIAN_POINT ( 'NONE',  ( 6.316639616203773677, -1.633150327867691765, -6.094999999999989093 ) ) ;
#53112 = CARTESIAN_POINT ( 'NONE',  ( -17.81601139373099940, 28.73617430169775133, 5.000000000000000000 ) ) ;
#53113 = CARTESIAN_POINT ( 'NONE',  ( 34.03709685856478018, -3.054999999999999272, -5.291415217122919401 ) ) ;
#53114 = CARTESIAN_POINT ( 'NONE',  ( -21.78162688292479388, 21.74787736706805674, 4.999607392498049308 ) ) ;
#53115 = EDGE_CURVE ( 'NONE', #21869, #127158, #29285, .T. ) ;
#53116 = EDGE_LOOP ( 'NONE', ( #102474, #92107, #94062, #80866, #98508 ) ) ;
#53117 = LINE ( 'NONE', #74186, #16316 ) ;
#53118 = ORIENTED_EDGE ( 'NONE', *, *, #92692, .T. ) ;
#53119 = ORIENTED_EDGE ( 'NONE', *, *, #2997, .F. ) ;
#53120 = AXIS2_PLACEMENT_3D ( 'NONE', #95461, #84607, #73715 ) ;
#53121 = DIRECTION ( 'NONE',  ( -0.3543493200069163240, -0.000000000000000000, -0.9351131265310288487 ) ) ;
#53122 = DIRECTION ( 'NONE',  ( -0.000000000000000000, 0.3543493200069153248, 0.9351131265310292928 ) ) ;
#53124 = EDGE_CURVE ( 'NONE', #4075, #87580, #93833, .T. ) ;
#53123 = AXIS2_PLACEMENT_3D ( 'NONE', #60427, #93737, #38648 ) ;
#53125 = AXIS2_PLACEMENT_3D ( 'NONE', #12438, #135669, #69720 ) ;
#53126 = ORIENTED_EDGE ( 'NONE', *, *, #139102, .T. ) ;
#53127 =( NAMED_UNIT ( * ) PLANE_ANGLE_UNIT ( ) SI_UNIT ( $, .RADIAN. ) );
#53128 = DIRECTION ( 'NONE',  ( 0.7071067811865487940, 0.7071067811865463515, 0.000000000000000000 ) ) ;
#53129 = VECTOR ( 'NONE', #125092, 1000.000000000000000 ) ;
#53130 = CARTESIAN_POINT ( 'NONE',  ( -8.526639036357797963, -5.240707523384225297, 16.25846745537493732 ) ) ;
#53131 = DIRECTION ( 'NONE',  ( -0.7071067811865486830, 0.7071067811865464625, 0.000000000000000000 ) ) ;
#53132 = LINE ( 'NONE', #8185, #24582 ) ;
#53133 = ORIENTED_EDGE ( 'NONE', *, *, #113226, .F. ) ;
#53134 = CARTESIAN_POINT ( 'NONE',  ( -12.81246187583938401, -22.22500000000000142, 4.000000000000000000 ) ) ;
#53135 = CARTESIAN_POINT ( 'NONE',  ( 19.27928215921719612, -2.789594763390444321, 4.000000000000000000 ) ) ;
#53136 = EDGE_CURVE ( 'NONE', #106976, #50763, #138061, .T. ) ;
#53137 = CARTESIAN_POINT ( 'NONE',  ( 79.45833333333332860, 3.974999999999997424, 6.884901960086288852 ) ) ;
#53138 = AXIS2_PLACEMENT_3D ( 'NONE', #102005, #57103, #113577 ) ;
#53139 = CARTESIAN_POINT ( 'NONE',  ( 2.994519915287485734, 28.92564299267940342, 4.000000000000000000 ) ) ;
#53140 = CARTESIAN_POINT ( 'NONE',  ( 69.48921356237309510, -27.52281430457103895, 5.000000000000000000 ) ) ;
#53141 =( BOUNDED_SURFACE ( )  B_SPLINE_SURFACE ( 1, 2, ( 
 ( #126203, #124769, #60254, #103698, #91444, #116013, #4344, #48648, #26880, #58134, #127636, #27582, #36346, #68984, #58863, #92845, #137808, #2979, #94274, #3662, #137081, #39197, #104430, #38483, #14581, #26183, #60996, #37783, #113163, #113893, #13837, #80574, #47273, #25440, #82706, #37044, #5091, #81292, #15962, #49392, #93575, #126885, #69710, #102331, #103023, #47959, #92123, #125496, #7237, #107977, #28329, #85522, #50784, #117431, #62390, #64510, #97858, #73965, #61683, #52887, #18106, #86974, #108685, #17426, #84159, #142097, #30461, #75398, #7962, #40634, #118142, #116745, #39940, #107291, #119573, #9372, #130504, #52201, #118883, #20269, #18849, #73267, #53647, #96390, #141350, #139956, #31183, #42783, #63116, #6503, #105844, #72590, #19571, #94972, #84837, #129044, #86280, #139245, #8650, #63815, #140628, #128358, #29030, #41314, #106553, #51512, #97090, #95704, #42066, #29716, #129760, #74702, #33357, #122442, #11519, #67392, #134062, #99246, #98558, #45646, #78259, #32616, #65976, #666, #131922, #2063, #66665, #121725, #110133, #77555, #112312, #22401, #110829, #54383, #10813, #20991, #55076, #31884, #55800, #57238, #76848, #23107, #68134, #34044, #111581, #46374, #78988, #12260, #121023, #100002, #21722, #143488, #123196, #133352, #56547, #131197, #12961, #76105, #23869, #44209, #101412, #120274, #100718, #142785, #1363, #10122, #88425, #65254, #132665, #44957, #89820, #109437, #43476, #34751, #87688, #89134, #14413, #4174, #27403, #82529, #126046, #16528, #69535, #26712, #93399, #115109, #48465, #3501, #58695, #135496, #124600, #70954, #103535, #81118, #115824, #79727, #47105, #102864, #47793, #37605, #114432, #136904, #125321, #92665, #15780, #57958, #91966, #25275, #60817, #136186, #123910, #36864, #102153, #15100, #91291, #60076, #104245, #81852, #4910, #126717, #49208, #137636, #113724, #2808, #134797, #36180, #71658, #35494, #38314, #80410, #104979, #26010, #5645, #70276, #90560, #24568, #59378, #68824, #112997, #13664, #75242 ),
 ( #119401, #95523, #83241, #74525, #39759, #108513, #86097, #39018, #105671, #20097, #52043, #96925, #29550, #62216, #139790, #138337, #61523, #128871, #141168, #130327, #8480, #73790, #140461, #41883, #40470, #94794, #31017, #117960, #19401, #17940, #52732, #64344, #84668, #28148, #127447, #49917, #41152, #72408, #106371, #7054, #107816, #94095, #129578, #85359, #18663, #116577, #6333, #62939, #17260, #50611, #30278, #139055, #83987, #118708, #51335, #128189, #28864, #73102, #117258, #107114, #7790, #63653, #96219, #88242, #99077, #88969, #54217, #22934, #45475, #34575, #76672, #10642, #22231, #65077, #484, #54907, #31711, #12083, #44025, #143320, #66496, #141928, #67958, #111395, #75933, #9190, #142620, #132494, #78084, #86816, #89653, #87522, #33181, #133882, #44778, #122263, #98403, #109973, #56367, #77393, #123010, #43311, #100546, #120107, #131032, #20817, #67199, #120845, #133190, #21552, #11342, #121559, #110660, #55617, #109266, #78796, #131749, #99819, #23686, #33867, #1194, #9945, #32435, #42619, #65814, #53465, #97674, #38152, #13495, #4014, #49031, #14937, #92493, #27239, #59903, #136720, #112830, #136013, #2630, #36018, #104072, #114263, #48294, #112143, #93226, #12791, #4727, #124425, #137459, #82371, #59214, #35313, #37433, #134616, #101963, #101242, #57778, #113534, #103362, #126550, #57065, #125876, #26548, #68645, #80239, #25825, #1881, #46193, #81672, #90367, #91114, #70789, #114935, #15613, #70100, #25097, #69356, #46928, #135332, #79553, #125136, #102692, #123742, #24398, #14235, #58520, #3338, #47624, #36695, #91789, #80941, #73625, #140305, #38852, #39585, #105510, #41707, #117104, #60649, #83820, #83075, #95361, #27975, #40995, #96066, #18488, #85194, #63494, #129415, #7623, #6174, #127273, #115653, #17101, #107664, #16346, #30103, #61367, #141002, #50451, #19239, #138896, #85920, #51888, #74352, #8322, #118540, #72245, #17779, #62763, #139629, #52572, #96753, #128027, #116413, #130160, #106950, #94637, #28707, #84517, #72952 ) ),
 .UNSPECIFIED., .F., .F., .F. ) 
 B_SPLINE_SURFACE_WITH_KNOTS ( ( 2, 2 ),
 ( 3, 2, 2, 2, 2, 2, 2, 2, 2, 2, 2, 2, 2, 2, 2, 2, 2, 2, 2, 2, 2, 2, 2, 2, 2, 2, 2, 2, 2, 2, 2, 2, 2, 2, 2, 2, 2, 2, 2, 2, 2, 2, 2, 2, 2, 2, 2, 2, 2, 2, 2, 2, 2, 2, 2, 2, 2, 2, 2, 2, 2, 2, 2, 2, 2, 2, 2, 2, 2, 2, 2, 2, 2, 2, 2, 2, 2, 2, 2, 2, 2, 2, 2, 2, 2, 2, 2, 2, 2, 2, 2, 2, 2, 2, 2, 2, 2, 2, 2, 2, 2, 2, 2, 2, 2, 2, 2, 2, 2, 2, 2, 2, 2, 2, 2, 2, 2, 2, 2, 2, 3 ),
 ( 0.000000000000000000, 1.000000000000000000 ),
 ( 0.000000000000000000, 0.008333333333333333218, 0.01666666666666666644, 0.02500000000000000139, 0.03333333333333333287, 0.04166666666666666435, 0.05000000000000000278, 0.05833333333333333426, 0.06666666666666666574, 0.07499999999999999722, 0.08333333333333332871, 0.09166666666666666019, 0.1000000000000000056, 0.1083333333333333370, 0.1166666666666666685, 0.1250000000000000000, 0.1333333333333333315, 0.1416666666666666630, 0.1499999999999999944, 0.1583333333333333259, 0.1666666666666666574, 0.1749999999999999889, 0.1833333333333333204, 0.1916666666666666796, 0.2000000000000000111, 0.2083333333333333426, 0.2166666666666666741, 0.2250000000000000056, 0.2333333333333333370, 0.2416666666666666685, 0.2500000000000000000, 0.2583333333333333592, 0.2666666666666666630, 0.2750000000000000222, 0.2833333333333333259, 0.2916666666666666852, 0.2999999999999999889, 0.3083333333333333481, 0.3166666666666666519, 0.3250000000000000111, 0.3333333333333333148, 0.3416666666666666741, 0.3499999999999999778, 0.3583333333333333370, 0.3666666666666666408, 0.3750000000000000000, 0.3833333333333333592, 0.3916666666666666630, 0.4000000000000000222, 0.4083333333333333259, 0.4166666666666666852, 0.4249999999999999889, 0.4333333333333333481, 0.4416666666666666519, 0.4500000000000000111, 0.4583333333333333148, 0.4666666666666666741, 0.4749999999999999778, 0.4833333333333333370, 0.4916666666666666408, 0.5000000000000000000, 0.5083333333333333037, 0.5166666666666667185, 0.5250000000000000222, 0.5333333333333333259, 0.5416666666666666297, 0.5500000000000000444, 0.5583333333333333481, 0.5666666666666666519, 0.5749999999999999556, 0.5833333333333333703, 0.5916666666666666741, 0.5999999999999999778, 0.6083333333333332815, 0.6166666666666666963, 0.6250000000000000000, 0.6333333333333333037, 0.6416666666666667185, 0.6500000000000000222, 0.6583333333333333259, 0.6666666666666666297, 0.6750000000000000444, 0.6833333333333333481, 0.6916666666666666519, 0.6999999999999999556, 0.7083333333333333703, 0.7166666666666666741, 0.7249999999999999778, 0.7333333333333332815, 0.7416666666666666963, 0.7500000000000000000, 0.7583333333333333037, 0.7666666666666667185, 0.7750000000000000222, 0.7833333333333333259, 0.7916666666666666297, 0.8000000000000000444, 0.8083333333333333481, 0.8166666666666666519, 0.8249999999999999556, 0.8333333333333333703, 0.8416666666666666741, 0.8499999999999999778, 0.8583333333333332815, 0.8666666666666666963, 0.8750000000000000000, 0.8833333333333333037, 0.8916666666666667185, 0.9000000000000000222, 0.9083333333333333259, 0.9166666666666666297, 0.9250000000000000444, 0.9333333333333333481, 0.9416666666666666519, 0.9499999999999999556, 0.9583333333333333703, 0.9666666666666666741, 0.9749999999999999778, 0.9833333333333332815, 0.9916666666666666963, 1.000000000000000000 ),
 .UNSPECIFIED. ) 
 GEOMETRIC_REPRESENTATION_ITEM ( )  RATIONAL_B_SPLINE_SURFACE ( (
 ( 1.000000000000000000, 0.9659258262890683122, 1.000000000000000000, 0.9659258262890683122, 1.000000000000000000, 0.9659258262890683122, 1.000000000000000000, 0.9659258262890683122, 1.000000000000000000, 0.9659258262890683122, 1.000000000000000000, 0.9659258262890683122, 1.000000000000000000, 0.9659258262890683122, 1.000000000000000000, 0.9659258262890683122, 1.000000000000000000, 0.9659258262890683122, 1.000000000000000000, 0.9659258262890683122, 1.000000000000000000, 0.9659258262890683122, 1.000000000000000000, 0.9659258262890683122, 1.000000000000000000, 0.9659258262890683122, 1.000000000000000000, 0.9659258262890683122, 1.000000000000000000, 0.9659258262890683122, 1.000000000000000000, 0.9659258262890683122, 1.000000000000000000, 0.9659258262890683122, 1.000000000000000000, 0.9659258262890683122, 1.000000000000000000, 0.9659258262890683122, 1.000000000000000000, 0.9659258262890683122, 1.000000000000000000, 0.9659258262890683122, 1.000000000000000000, 0.9659258262890683122, 1.000000000000000000, 0.9659258262890683122, 1.000000000000000000, 0.9659258262890683122, 1.000000000000000000, 0.9659258262890683122, 1.000000000000000000, 0.9659258262890683122, 1.000000000000000000, 0.9659258262890683122, 1.000000000000000000, 0.9659258262890683122, 1.000000000000000000, 0.9659258262890683122, 1.000000000000000000, 0.9659258262890683122, 1.000000000000000000, 0.9659258262890683122, 1.000000000000000000, 0.9659258262890683122, 1.000000000000000000, 0.9659258262890683122, 1.000000000000000000, 0.9659258262890683122, 1.000000000000000000, 0.9659258262890683122, 1.000000000000000000, 0.9659258262890683122, 1.000000000000000000, 0.9659258262890683122, 1.000000000000000000, 0.9659258262890683122, 1.000000000000000000, 0.9659258262890683122, 1.000000000000000000, 0.9659258262890683122, 1.000000000000000000, 0.9659258262890683122, 1.000000000000000000, 0.9659258262890683122, 1.000000000000000000, 0.9659258262890683122, 1.000000000000000000, 0.9659258262890683122, 1.000000000000000000, 0.9659258262890683122, 1.000000000000000000, 0.9659258262890683122, 1.000000000000000000, 0.9659258262890683122, 1.000000000000000000, 0.9659258262890683122, 1.000000000000000000, 0.9659258262890683122, 1.000000000000000000, 0.9659258262890683122, 1.000000000000000000, 0.9659258262890683122, 1.000000000000000000, 0.9659258262890683122, 1.000000000000000000, 0.9659258262890683122, 1.000000000000000000, 0.9659258262890683122, 1.000000000000000000, 0.9659258262890683122, 1.000000000000000000, 0.9659258262890683122, 1.000000000000000000, 0.9659258262890683122, 1.000000000000000000, 0.9659258262890683122, 1.000000000000000000, 0.9659258262890683122, 1.000000000000000000, 0.9659258262890683122, 1.000000000000000000, 0.9659258262890683122, 1.000000000000000000, 0.9659258262890683122, 1.000000000000000000, 0.9659258262890683122, 1.000000000000000000, 0.9659258262890683122, 1.000000000000000000, 0.9659258262890683122, 1.000000000000000000, 0.9659258262890683122, 1.000000000000000000, 0.9659258262890683122, 1.000000000000000000, 0.9659258262890683122, 1.000000000000000000, 0.9659258262890683122, 1.000000000000000000, 0.9659258262890683122, 1.000000000000000000, 0.9659258262890683122, 1.000000000000000000, 0.9659258262890683122, 1.000000000000000000, 0.9659258262890683122, 1.000000000000000000, 0.9659258262890683122, 1.000000000000000000, 0.9659258262890683122, 1.000000000000000000, 0.9659258262890683122, 1.000000000000000000, 0.9659258262890683122, 1.000000000000000000, 0.9659258262890683122, 1.000000000000000000, 0.9659258262890683122, 1.000000000000000000, 0.9659258262890683122, 1.000000000000000000, 0.9659258262890683122, 1.000000000000000000, 0.9659258262890683122, 1.000000000000000000, 0.9659258262890683122, 1.000000000000000000, 0.9659258262890683122, 1.000000000000000000, 0.9659258262890683122, 1.000000000000000000, 0.9659258262890683122, 1.000000000000000000, 0.9659258262890683122, 1.000000000000000000, 0.9659258262890683122, 1.000000000000000000, 0.9659258262890683122, 1.000000000000000000, 0.9659258262890683122, 1.000000000000000000, 0.9659258262890683122, 1.000000000000000000, 0.9659258262890683122, 1.000000000000000000, 0.9659258262890683122, 1.000000000000000000, 0.9659258262890683122, 1.000000000000000000, 0.9659258262890683122, 1.000000000000000000, 0.9659258262890683122, 1.000000000000000000, 0.9659258262890683122, 1.000000000000000000, 0.9659258262890683122, 1.000000000000000000, 0.9659258262890683122, 1.000000000000000000, 0.9659258262890683122, 1.000000000000000000, 0.9659258262890683122, 1.000000000000000000, 0.9659258262890683122, 1.000000000000000000, 0.9659258262890683122, 1.000000000000000000, 0.9659258262890683122, 1.000000000000000000, 0.9659258262890683122, 1.000000000000000000, 0.9659258262890683122, 1.000000000000000000, 0.9659258262890683122, 1.000000000000000000, 0.9659258262890683122, 1.000000000000000000, 0.9659258262890683122, 1.000000000000000000, 0.9659258262890683122, 1.000000000000000000, 0.9659258262890683122, 1.000000000000000000, 0.9659258262890683122, 1.000000000000000000, 0.9659258262890683122, 1.000000000000000000, 0.9659258262890683122, 1.000000000000000000, 0.9659258262890683122, 1.000000000000000000, 0.9659258262890683122, 1.000000000000000000, 0.9659258262890683122, 1.000000000000000000, 0.9659258262890683122, 1.000000000000000000, 0.9659258262890683122, 1.000000000000000000, 0.9659258262890683122, 1.000000000000000000),
 ( 1.000000000000000000, 0.9659258262890683122, 1.000000000000000000, 0.9659258262890683122, 1.000000000000000000, 0.9659258262890683122, 1.000000000000000000, 0.9659258262890683122, 1.000000000000000000, 0.9659258262890683122, 1.000000000000000000, 0.9659258262890683122, 1.000000000000000000, 0.9659258262890683122, 1.000000000000000000, 0.9659258262890683122, 1.000000000000000000, 0.9659258262890683122, 1.000000000000000000, 0.9659258262890683122, 1.000000000000000000, 0.9659258262890683122, 1.000000000000000000, 0.9659258262890683122, 1.000000000000000000, 0.9659258262890683122, 1.000000000000000000, 0.9659258262890683122, 1.000000000000000000, 0.9659258262890683122, 1.000000000000000000, 0.9659258262890683122, 1.000000000000000000, 0.9659258262890683122, 1.000000000000000000, 0.9659258262890683122, 1.000000000000000000, 0.9659258262890683122, 1.000000000000000000, 0.9659258262890683122, 1.000000000000000000, 0.9659258262890683122, 1.000000000000000000, 0.9659258262890683122, 1.000000000000000000, 0.9659258262890683122, 1.000000000000000000, 0.9659258262890683122, 1.000000000000000000, 0.9659258262890683122, 1.000000000000000000, 0.9659258262890683122, 1.000000000000000000, 0.9659258262890683122, 1.000000000000000000, 0.9659258262890683122, 1.000000000000000000, 0.9659258262890683122, 1.000000000000000000, 0.9659258262890683122, 1.000000000000000000, 0.9659258262890683122, 1.000000000000000000, 0.9659258262890683122, 1.000000000000000000, 0.9659258262890683122, 1.000000000000000000, 0.9659258262890683122, 1.000000000000000000, 0.9659258262890683122, 1.000000000000000000, 0.9659258262890683122, 1.000000000000000000, 0.9659258262890683122, 1.000000000000000000, 0.9659258262890683122, 1.000000000000000000, 0.9659258262890683122, 1.000000000000000000, 0.9659258262890683122, 1.000000000000000000, 0.9659258262890683122, 1.000000000000000000, 0.9659258262890683122, 1.000000000000000000, 0.9659258262890683122, 1.000000000000000000, 0.9659258262890683122, 1.000000000000000000, 0.9659258262890683122, 1.000000000000000000, 0.9659258262890683122, 1.000000000000000000, 0.9659258262890683122, 1.000000000000000000, 0.9659258262890683122, 1.000000000000000000, 0.9659258262890683122, 1.000000000000000000, 0.9659258262890683122, 1.000000000000000000, 0.9659258262890683122, 1.000000000000000000, 0.9659258262890683122, 1.000000000000000000, 0.9659258262890683122, 1.000000000000000000, 0.9659258262890683122, 1.000000000000000000, 0.9659258262890683122, 1.000000000000000000, 0.9659258262890683122, 1.000000000000000000, 0.9659258262890683122, 1.000000000000000000, 0.9659258262890683122, 1.000000000000000000, 0.9659258262890683122, 1.000000000000000000, 0.9659258262890683122, 1.000000000000000000, 0.9659258262890683122, 1.000000000000000000, 0.9659258262890683122, 1.000000000000000000, 0.9659258262890683122, 1.000000000000000000, 0.9659258262890683122, 1.000000000000000000, 0.9659258262890683122, 1.000000000000000000, 0.9659258262890683122, 1.000000000000000000, 0.9659258262890683122, 1.000000000000000000, 0.9659258262890683122, 1.000000000000000000, 0.9659258262890683122, 1.000000000000000000, 0.9659258262890683122, 1.000000000000000000, 0.9659258262890683122, 1.000000000000000000, 0.9659258262890683122, 1.000000000000000000, 0.9659258262890683122, 1.000000000000000000, 0.9659258262890683122, 1.000000000000000000, 0.9659258262890683122, 1.000000000000000000, 0.9659258262890683122, 1.000000000000000000, 0.9659258262890683122, 1.000000000000000000, 0.9659258262890683122, 1.000000000000000000, 0.9659258262890683122, 1.000000000000000000, 0.9659258262890683122, 1.000000000000000000, 0.9659258262890683122, 1.000000000000000000, 0.9659258262890683122, 1.000000000000000000, 0.9659258262890683122, 1.000000000000000000, 0.9659258262890683122, 1.000000000000000000, 0.9659258262890683122, 1.000000000000000000, 0.9659258262890683122, 1.000000000000000000, 0.9659258262890683122, 1.000000000000000000, 0.9659258262890683122, 1.000000000000000000, 0.9659258262890683122, 1.000000000000000000, 0.9659258262890683122, 1.000000000000000000, 0.9659258262890683122, 1.000000000000000000, 0.9659258262890683122, 1.000000000000000000, 0.9659258262890683122, 1.000000000000000000, 0.9659258262890683122, 1.000000000000000000, 0.9659258262890683122, 1.000000000000000000, 0.9659258262890683122, 1.000000000000000000, 0.9659258262890683122, 1.000000000000000000, 0.9659258262890683122, 1.000000000000000000, 0.9659258262890683122, 1.000000000000000000, 0.9659258262890683122, 1.000000000000000000, 0.9659258262890683122, 1.000000000000000000, 0.9659258262890683122, 1.000000000000000000, 0.9659258262890683122, 1.000000000000000000, 0.9659258262890683122, 1.000000000000000000, 0.9659258262890683122, 1.000000000000000000, 0.9659258262890683122, 1.000000000000000000, 0.9659258262890683122, 1.000000000000000000, 0.9659258262890683122, 1.000000000000000000, 0.9659258262890683122, 1.000000000000000000, 0.9659258262890683122, 1.000000000000000000, 0.9659258262890683122, 1.000000000000000000, 0.9659258262890683122, 1.000000000000000000, 0.9659258262890683122, 1.000000000000000000, 0.9659258262890683122, 1.000000000000000000, 0.9659258262890683122, 1.000000000000000000, 0.9659258262890683122, 1.000000000000000000, 0.9659258262890683122, 1.000000000000000000, 0.9659258262890683122, 1.000000000000000000, 0.9659258262890683122, 1.000000000000000000, 0.9659258262890683122, 1.000000000000000000) ) ) 
 REPRESENTATION_ITEM ( '' )  SURFACE ( )  );
#53142 = DIRECTION ( 'NONE',  ( -0.6830127018922180770, -0.6830127018922204085, -0.2588190451025213501 ) ) ;
#53143 = CARTESIAN_POINT ( 'NONE',  ( 54.76669371712954870, -7.949999999999999289, 2.130196079827424427 ) ) ;
#53144 = DIRECTION ( 'NONE',  ( 0.7071067811865487940, 0.7071067811865463515, 0.000000000000000000 ) ) ;
#53145 = VECTOR ( 'NONE', #116231, 1000.000000000000000 ) ;
#53146 = VERTEX_POINT ( 'NONE', #117009 ) ;
#53147 = ORIENTED_EDGE ( 'NONE', *, *, #138670, .T. ) ;
#53148 = CARTESIAN_POINT ( 'NONE',  ( 56.85416666666666430, -2.130196079827425315, -7.950000000000001066 ) ) ;
#53149 = CARTESIAN_POINT ( 'NONE',  ( -29.67183060077626422, -6.740707523384212863, 4.000000000000000000 ) ) ;
#53150 = DIRECTION ( 'NONE',  ( -1.000000000000000000, 0.000000000000000000, -0.000000000000000000 ) ) ;
#53151 = EDGE_CURVE ( 'NONE', #143140, #123173, #105409, .T. ) ;
#53152 = VECTOR ( 'NONE', #25130, 1000.000000000000000 ) ;
#53153 = PLANE ( 'NONE',  #32279 ) ;
#53154 = ORIENTED_EDGE ( 'NONE', *, *, #82042, .T. ) ;
#53156 = EDGE_CURVE ( 'NONE', #143522, #4786, #4611, .T. ) ;
#53155 = LINE ( 'NONE', #108954, #123221 ) ;
#53157 = EDGE_CURVE ( 'NONE', #129470, #111735, #73528, .T. ) ;
#53158 = CARTESIAN_POINT ( 'NONE',  ( 44.77126352523143282, 4.472830434245839371, 4.472830434245842035 ) ) ;
#53159 = VERTEX_POINT ( 'NONE', #38746 ) ;
#53160 = DIRECTION ( 'NONE',  ( 0.7071067811865486830, -0.7071067811865464625, -0.000000000000000000 ) ) ;
#53161 = VERTEX_POINT ( 'NONE', #114843 ) ;
#53162 = VERTEX_POINT ( 'NONE', #138789 ) ;
#53163 = CARTESIAN_POINT ( 'NONE',  ( 11.99999999999990941, -13.06887692260767686, 4.000000000000000000 ) ) ;
#53164 = CONICAL_SURFACE ( 'NONE', #48529, 2.500000000000000888, 0.9599310885968822538 ) ;
#53166 = EDGE_CURVE ( 'NONE', #52039, #121499, #48925, .T. ) ;
#53165 = VECTOR ( 'NONE', #7308, 1000.000000000000114 ) ;
#53167 = CARTESIAN_POINT ( 'NONE',  ( 80.43336038379622721, 2.130196079827431532, -7.949999999999996625 ) ) ;
#53168 = CARTESIAN_POINT ( 'NONE',  ( -10.49999999999993250, -14.70932175296478839, -11.46312253303834794 ) ) ;
#53169 = VECTOR ( 'NONE', #141210, 1000.000000000000114 ) ;
#53170 = DIRECTION ( 'NONE',  ( 0.7071067811865487940, 0.7071067811865463515, 0.000000000000000000 ) ) ;
#53171 = EDGE_LOOP ( 'NONE', ( #37069, #21842, #119234, #29876 ) ) ;
#53172 = EDGE_CURVE ( 'NONE', #62444, #9144, #139524, .T. ) ;
#53173 = CARTESIAN_POINT ( 'NONE',  ( 5.999999999999974243, -19.44781430457062754, 5.000000000000000000 ) ) ;
#53174 = DIRECTION ( 'NONE',  ( 0.000000000000000000, -1.000000000000000000, 0.000000000000000000 ) ) ;
#53176 = ORIENTED_EDGE ( 'NONE', *, *, #2078, .F. ) ;
#53175 = CARTESIAN_POINT ( 'NONE',  ( 8.504139616203772789, -3.047499999999994547, 5.278424836066145431 ) ) ;
#53177 = VECTOR ( 'NONE', #126061, 999.9999999999998863 ) ;
#53178 = CARTESIAN_POINT ( 'NONE',  ( 83.12543019189810423, 5.291415217122919401, 3.055000000000002824 ) ) ;
#53179 = VECTOR ( 'NONE', #26975, 1000.000000000000227 ) ;
#53180 = CARTESIAN_POINT ( 'NONE',  ( 15.31250000000000000, -4.461849672132299993, -4.461849672132299105 ) ) ;
#53181 = CARTESIAN_POINT ( 'NONE',  ( -8.994519915287490619, 28.92564299267944250, 4.000000000000000000 ) ) ;
#53182 = DIRECTION ( 'NONE',  ( -0.7071067811865487940, 0.7071067811865463515, 0.000000000000000000 ) ) ;
#53183 = AXIS2_PLACEMENT_3D ( 'NONE', #74955, #108948, #29974 ) ;
#53184 = CARTESIAN_POINT ( 'NONE',  ( 56.99451991528749062, 28.92564299267978001, 4.000000000000000000 ) ) ;
#53185 = ORIENTED_EDGE ( 'NONE', *, *, #53858, .F. ) ;
#53186 = ADVANCED_FACE ( 'NONE', ( #28597 ), #125771, .F. ) ;
#53187 = CARTESIAN_POINT ( 'NONE',  ( 88.45419371712957002, 6.884901960086283523, 3.975000000000002753 ) ) ;
#53188 = CARTESIAN_POINT ( 'NONE',  ( 64.07876352523145158, -7.482591942790325086E-16, 6.109999999999998543 ) ) ;
#53189 = DIRECTION ( 'NONE',  ( 0.000000000000000000, -1.000000000000000000, 0.000000000000000000 ) ) ;
#53190 = CARTESIAN_POINT ( 'NONE',  ( -24.69524342170288023, 1.235879655689124501, 4.000000000000000000 ) ) ;
#53191 = ORIENTED_EDGE ( 'NONE', *, *, #76877, .F. ) ;
#53192 = ORIENTED_EDGE ( 'NONE', *, *, #85267, .F. ) ;
#53193 = AXIS2_PLACEMENT_3D ( 'NONE', #54334, #76796, #21673 ) ;
#53194 = PLANE ( 'NONE',  #28369 ) ;
#53196 = EDGE_CURVE ( 'NONE', #33900, #17266, #40208, .T. ) ;
#53195 = DIRECTION ( 'NONE',  ( 1.000000000000000000, 0.000000000000000000, 0.000000000000000000 ) ) ;
#53197 = EDGE_LOOP ( 'NONE', ( #131674, #7987, #98706, #4283, #128010, #29545, #35796, #138869 ) ) ;
#53198 = ORIENTED_EDGE ( 'NONE', *, *, #28679, .T. ) ;
#53199 = CARTESIAN_POINT ( 'NONE',  ( 9.981552653643248618, 18.75929247661552424, 20.33588619593440683 ) ) ;
#53200 = ORIENTED_EDGE ( 'NONE', *, *, #88027, .F. ) ;
#53201 = LINE ( 'NONE', #86577, #97827 ) ;
#53202 = CARTESIAN_POINT ( 'NONE',  ( 39.48921356237310221, -27.52281430457082934, 5.000000000000000000 ) ) ;
#53203 = AXIS2_PLACEMENT_3D ( 'NONE', #89287, #13122, #90736 ) ;
#53204 = FACE_OUTER_BOUND ( 'NONE', #35189, .T. ) ;
#53205 = FACE_BOUND ( 'NONE', #50132, .T. ) ;
#53206 = PLANE ( 'NONE',  #8482 ) ;
#53207 = DIRECTION ( 'NONE',  ( -0.9659258262890677571, 3.169619151431787128E-17, -0.2588190451025225713 ) ) ;
#53208 = CARTESIAN_POINT ( 'NONE',  ( 18.63425672184678916, -2.500000000000000444, 3.061616997868384127E-16 ) ) ;
#53210 = ORIENTED_EDGE ( 'NONE', *, *, #9786, .F. ) ;
#53209 = DIRECTION ( 'NONE',  ( 0.000000000000000000, 0.000000000000000000, 1.000000000000000000 ) ) ;
#53211 = ITEM_DEFINED_TRANSFORMATION ( 'NONE', 'NONE', #135029,  #127880 ) ;
#53212 = ORIENTED_EDGE ( 'NONE', *, *, #78359, .F. ) ;
#53213 = EDGE_CURVE ( 'NONE', #115415, #88391, #116299, .T. ) ;
#53214 = ORIENTED_EDGE ( 'NONE', *, *, #104179, .F. ) ;
#53215 = CARTESIAN_POINT ( 'NONE',  ( 81.14126352523143737, 4.472830434245835818, 4.472830434245840259 ) ) ;
#53216 = ORIENTED_EDGE ( 'NONE', *, *, #113633, .T. ) ;
#53217 = DIRECTION ( 'NONE',  ( 0.7071067811865487940, -0.7071067811865463515, 0.000000000000000000 ) ) ;
#53218 = EDGE_LOOP ( 'NONE', ( #69987, #17926, #123850, #83739 ) ) ;
#53219 = CARTESIAN_POINT ( 'NONE',  ( 3.183988606268992161, 28.73617430169789699, 5.000000000000000000 ) ) ;
#53220 = LINE ( 'NONE', #88010, #12394 ) ;
#53221 = DIRECTION ( 'NONE',  ( 0.3543493200069162685, -0.000000000000000000, -0.9351131265310288487 ) ) ;
#53222 = AXIS2_PLACEMENT_3D ( 'NONE', #123734, #13484, #101957 ) ;
#53223 = LINE ( 'NONE', #120611, #17616 ) ;
#53224 = DIRECTION ( 'NONE',  ( 0.7071067811865487940, 0.7071067811865463515, 0.000000000000000000 ) ) ;
#53225 = CARTESIAN_POINT ( 'NONE',  ( -24.79333936457829779, 21.75929247661549581, 4.998822639870701856 ) ) ;
#53226 = CARTESIAN_POINT ( 'NONE',  ( -21.48921356237309155, -27.52281430457070499, 5.000000000000000000 ) ) ;
#53228 = VERTEX_POINT ( 'NONE', #26444 ) ;
#53227 = CIRCLE ( 'NONE', #104228, 28.00000000000003197 ) ;
#53229 = VECTOR ( 'NONE', #94265, 1000.000000000000000 ) ;
#53230 = VECTOR ( 'NONE', #94298, 1000.000000000000000 ) ;
#53231 = STYLED_ITEM ( 'NONE', ( #126896 ), #63692 ) ;
#53232 = ORIENTED_EDGE ( 'NONE', *, *, #46304, .T. ) ;
#53233 = DIRECTION ( 'NONE',  ( -0.7071067811865486830, -0.7071067811865464625, 0.000000000000000000 ) ) ;
#53234 = FACE_OUTER_BOUND ( 'NONE', #93906, .T. ) ;
#53235 = VECTOR ( 'NONE', #24889, 1000.000000000000227 ) ;
#53236 = EDGE_LOOP ( 'NONE', ( #89570, #51222, #38446 ) ) ;
#53237 = ORIENTED_EDGE ( 'NONE', *, *, #93878, .T. ) ;
#53238 = ORIENTED_EDGE ( 'NONE', *, *, #110348, .F. ) ;
#53239 = CARTESIAN_POINT ( 'NONE',  ( 38.64626352523143993, -4.472830434245840259, 4.472830434245838482 ) ) ;
#53240 = VERTEX_POINT ( 'NONE', #18380 ) ;
#53241 = AXIS2_PLACEMENT_3D ( 'NONE', #61744, #18172, #116085 ) ;
#53242 = DIRECTION ( 'NONE',  ( 0.7071067811865486830, -0.7071067811865464625, -0.000000000000000000 ) ) ;
#53243 = CARTESIAN_POINT ( 'NONE',  ( 28.92080628287044064, 3.047499999999997655, 5.278424836066143655 ) ) ;
#53244 = CARTESIAN_POINT ( 'NONE',  ( 3.657803576507369314, 12.22753933337904009, -27.06132802995527697 ) ) ;
#53245 = VERTEX_POINT ( 'NONE', #137357 ) ;
#53246 = CARTESIAN_POINT ( 'NONE',  ( -63.48921356237309510, -27.52281430457099631, 5.000000000000000000 ) ) ;
#53247 = ORIENTED_EDGE ( 'NONE', *, *, #42945, .T. ) ;
#53248 = CARTESIAN_POINT ( 'NONE',  ( -25.39999999999996305, 3.061616997868383141E-16, -2.500000000000000000 ) ) ;
#53249 = VECTOR ( 'NONE', #61740, 1000.000000000000000 ) ;
#53250 = AXIS2_PLACEMENT_3D ( 'NONE', #67263, #123798, #91175 ) ;
#53251 = LINE ( 'NONE', #119915, #116914 ) ;
#53253 = ORIENTED_EDGE ( 'NONE', *, *, #21019, .F. ) ;
#53252 = PLANE ( 'NONE',  #65626 ) ;
#53254 = ORIENTED_EDGE ( 'NONE', *, *, #101427, .F. ) ;
#53255 = PLANE ( 'NONE',  #16811 ) ;
#53256 = FACE_OUTER_BOUND ( 'NONE', #70421, .T. ) ;
#53257 = ORIENTED_EDGE ( 'NONE', *, *, #5215, .F. ) ;
#53258 = VECTOR ( 'NONE', #46822, 1000.000000000000000 ) ;
#53259 = CARTESIAN_POINT ( 'NONE',  ( -20.29289321881330821, -6.740707523384214639, 5.000000000000000000 ) ) ;
#53260 = ORIENTED_EDGE ( 'NONE', *, *, #94378, .T. ) ;
#53261 = ORIENTED_EDGE ( 'NONE', *, *, #68231, .T. ) ;
#53262 = ORIENTED_EDGE ( 'NONE', *, *, #73143, .T. ) ;
#53264 = DIRECTION ( 'NONE',  ( 0.7071067811865487940, -0.7071067811865463515, -0.000000000000000000 ) ) ;
#53263 = STYLED_ITEM ( 'NONE', ( #75114 ), #83137 ) ;
#53265 = DIRECTION ( 'NONE',  ( 0.000000000000000000, -1.000000000000000000, 0.000000000000000000 ) ) ;
#53266 = VECTOR ( 'NONE', #108039, 1000.000000000000000 ) ;
#53267 = CARTESIAN_POINT ( 'NONE',  ( -53.99451991528749062, 28.92564299267975869, 4.000000000000000000 ) ) ;
#53268 = ADVANCED_FACE ( 'NONE', ( #127917 ), #92383, .F. ) ;
#53269 = LINE ( 'NONE', #33004, #91074 ) ;
#53270 = DIRECTION ( 'NONE',  ( 0.000000000000000000, -1.000000000000000000, 0.000000000000000000 ) ) ;
#53271 = ADVANCED_FACE ( 'NONE', ( #106841 ), #136614, .F. ) ;
#53273 = EDGE_LOOP ( 'NONE', ( #114796, #64433, #96710, #118732 ) ) ;
#53272 = EDGE_CURVE ( 'NONE', #136399, #89877, #27861, .T. ) ;
#53274 = VECTOR ( 'NONE', #83827, 1000.000000000000000 ) ;
#53275 = CARTESIAN_POINT ( 'NONE',  ( 97.64169371712954160, -2.130196079827424871, -7.949999999999998401 ) ) ;
#53276 = VERTEX_POINT ( 'NONE', #16235 ) ;
#53277 = VECTOR ( 'NONE', #50868, 1000.000000000000000 ) ;
#53278 = DIRECTION ( 'NONE',  ( -0.7071067811865486830, -0.7071067811865464625, 0.000000000000000000 ) ) ;
#53279 = EDGE_CURVE ( 'NONE', #27100, #138721, #104707, .T. ) ;
#53280 = EDGE_CURVE ( 'NONE', #34606, #109090, #16995, .T. ) ;
#53281 = DIRECTION ( 'NONE',  ( 0.7071067811865486830, -0.7071067811865464625, -0.000000000000000000 ) ) ;
#53282 = ORIENTED_EDGE ( 'NONE', *, *, #107521, .T. ) ;
#53283 = AXIS2_PLACEMENT_3D ( 'NONE', #93162, #60575, #125807 ) ;
#53284 = CARTESIAN_POINT ( 'NONE',  ( -16.49999999999988276, 12.43112307739205313, 4.000000000000000000 ) ) ;
#53285 = CARTESIAN_POINT ( 'NONE',  ( -34.42500000000001137, -19.45860074219779534, 5.000000000000000000 ) ) ;
#53286 = ORIENTED_EDGE ( 'NONE', *, *, #96748, .T. ) ;
#53287 = VERTEX_POINT ( 'NONE', #61267 ) ;
#53288 = EDGE_CURVE ( 'NONE', #89845, #118518, #83713, .T. ) ;
#53289 = CARTESIAN_POINT ( 'NONE',  ( -14.99451991528749595, 28.92564299267948513, 4.000000000000000000 ) ) ;
#53290 = DIRECTION ( 'NONE',  ( -0.3543493200069162685, -0.000000000000000000, -0.9351131265310288487 ) ) ;
#53291 = UNCERTAINTY_MEASURE_WITH_UNIT (LENGTH_MEASURE( 1.000000000000000082E-05 ), #101351, 'distance_accuracy_value', 'NONE');
#53292 = VECTOR ( 'NONE', #84219, 1000.000000000000000 ) ;
#53293 = LINE ( 'NONE', #8332, #134940 ) ;
#53294 = CARTESIAN_POINT ( 'NONE',  ( 57.18398860626899705, 28.73617430169827358, 5.000000000000000000 ) ) ;
#53295 = CARTESIAN_POINT ( 'NONE',  ( 22.82900182742193351, 7.795401085224272109, 5.000000000000000000 ) ) ;
#53296 = CARTESIAN_POINT ( 'NONE',  ( 65.68293019189810877, -1.637169565754159173, -6.109999999999999432 ) ) ;
#53297 = DIRECTION ( 'NONE',  ( -0.000000000000000000, 0.3543493200069153248, 0.9351131265310292928 ) ) ;
#53298 = EDGE_CURVE ( 'NONE', #138500, #99466, #74295, .T. ) ;
#53299 =( LENGTH_UNIT ( ) NAMED_UNIT ( * ) SI_UNIT ( .MILLI., .METRE. ) );
#53300 = DIRECTION ( 'NONE',  ( -0.7071067811865487940, 0.7071067811865463515, 0.000000000000000000 ) ) ;
#53301 = ADVANCED_BREP_SHAPE_REPRESENTATION ( '', ( #42351, #127880 ), #95551 ) ;
#53302 = CARTESIAN_POINT ( 'NONE',  ( 83.97916666666665719, -7.950000000000000178, 2.130196079827424427 ) ) ;
#53303 = VERTEX_POINT ( 'NONE', #97374 ) ;
#53304 = ORIENTED_EDGE ( 'NONE', *, *, #15070, .F. ) ;
#53305 = AXIS2_PLACEMENT_3D ( 'NONE', #131537, #108310, #118505 ) ;
#53306 = PLANE ( 'NONE',  #135810 ) ;
#53307 =( LENGTH_UNIT ( ) NAMED_UNIT ( * ) SI_UNIT ( .MILLI., .METRE. ) );
#53308 = ORIENTED_EDGE ( 'NONE', *, *, #134826, .T. ) ;
#53309 = CARTESIAN_POINT ( 'NONE',  ( 32.91508676806217437, -12.74070752338415957, 18.74364270924361975 ) ) ;
#53311 = EDGE_LOOP ( 'NONE', ( #36479, #13594, #30358, #135483 ) ) ;
#53310 = FACE_OUTER_BOUND ( 'NONE', #106450, .T. ) ;
#53312 = PLANE ( 'NONE',  #136497 ) ;
#53313 = CARTESIAN_POINT ( 'NONE',  ( 2.999999999999981792, -15.41253812416060143, 4.000000000000000000 ) ) ;
#53314 = PLANE ( 'NONE',  #6026 ) ;
#53315 = ORIENTED_EDGE ( 'NONE', *, *, #30094, .F. ) ;
#53316 = EDGE_LOOP ( 'NONE', ( #14687, #105839, #42546, #128339 ) ) ;
#53317 = DIRECTION ( 'NONE',  ( 0.000000000000000000, -1.000000000000000000, 0.000000000000000000 ) ) ;
#53318 = CARTESIAN_POINT ( 'NONE',  ( -23.99999999999982947, -8.731860332648864187, -2.120594902707593654 ) ) ;
#53319 = EDGE_CURVE ( 'NONE', #49422, #105592, #131473, .T. ) ;
#53320 = VECTOR ( 'NONE', #102560, 1000.000000000000000 ) ;
#53321 = DIRECTION ( 'NONE',  ( -0.7071067811865486830, -0.7071067811865464625, -0.000000000000000000 ) ) ;
#53322 = CARTESIAN_POINT ( 'NONE',  ( -24.18398860626899705, 28.73617430169804265, 5.000000000000000000 ) ) ;
#53323 = CARTESIAN_POINT ( 'NONE',  ( 87.14169371712958423, -2.130196079827424871, -7.949999999999999289 ) ) ;
#53324 = PLANE ( 'NONE',  #16175 ) ;
#53325 = DIRECTION ( 'NONE',  ( -0.7071067811865487940, 0.7071067811865463515, 0.000000000000000000 ) ) ;
#53326 = ORIENTED_EDGE ( 'NONE', *, *, #90651, .F. ) ;
#53327 = CARTESIAN_POINT ( 'NONE',  ( 19.49999999999987566, 19.46639925780206326, 5.000000000000000000 ) ) ;
#53328 = CARTESIAN_POINT ( 'NONE',  ( 5.999999999999967137, 5.966399257802200040, 5.000000000000000000 ) ) ;
#53329 = CARTESIAN_POINT ( 'NONE',  ( 30.91666666666666785, 5.278424836066147208, 3.047499999999990550 ) ) ;
#53330 = ADVANCED_FACE ( 'NONE', ( #19830 ), #142356, .F. ) ;
#53331 = ORIENTED_EDGE ( 'NONE', *, *, #23507, .T. ) ;
#53332 = VECTOR ( 'NONE', #121575, 1000.000000000000000 ) ;
#53333 = CARTESIAN_POINT ( 'NONE',  ( 4.499999999999970690, -15.29013452822854013, 0.3645803511610444803 ) ) ;
#53335 = EDGE_CURVE ( 'NONE', #66606, #96111, #28032, .T. ) ;
#53334 = VECTOR ( 'NONE', #65927, 999.9999999999998863 ) ;
#53336 = ORIENTED_EDGE ( 'NONE', *, *, #74906, .T. ) ;
#53337 = VECTOR ( 'NONE', #56097, 1000.000000000000227 ) ;
#53338 = CARTESIAN_POINT ( 'NONE',  ( 75.97959685856477563, 6.109999999999999432, 1.637169565754164280 ) ) ;
#53339 = ADVANCED_FACE ( 'NONE', ( #118430 ), #37239, .T. ) ;
#53340 = DIRECTION ( 'NONE',  ( 0.7071067811865486830, -0.7071067811865464625, -0.000000000000000000 ) ) ;
#53341 = FACE_OUTER_BOUND ( 'NONE', #61455, .T. ) ;
#53342 = ORIENTED_EDGE ( 'NONE', *, *, #87391, .T. ) ;
#53343 = VECTOR ( 'NONE', #134057, 1000.000000000000000 ) ;
#53344 = VECTOR ( 'NONE', #70128, 1000.000000000000227 ) ;
#53345 = AXIS2_PLACEMENT_3D ( 'NONE', #99828, #101971, #57786 ) ;
#53346 = CONICAL_SURFACE ( 'NONE', #65286, 2.055000000000000604, 0.9599310885968764806 ) ;
#53347 = PLANE ( 'NONE',  #7208 ) ;
#53348 = EDGE_CURVE ( 'NONE', #141092, #43222, #52459, .T. ) ;
#53349 = AXIS2_PLACEMENT_3D ( 'NONE', #7026, #108487, #97648 ) ;
#53350 = CARTESIAN_POINT ( 'NONE',  ( 11.70025512860841133, -27.71228299555198049, 4.000000000000000000 ) ) ;
#53351 = DIRECTION ( 'NONE',  ( -0.7071067811865487940, 0.7071067811865463515, -0.000000000000000000 ) ) ;
#53352 = LINE ( 'NONE', #97565, #43980 ) ;
#53354 = ORIENTED_EDGE ( 'NONE', *, *, #56366, .F. ) ;
#53353 = FACE_OUTER_BOUND ( 'NONE', #55456, .T. ) ;
#53355 = CARTESIAN_POINT ( 'NONE',  ( 128.8635666761577738, -49.19207878845100623, -41.22112633374977975 ) ) ;
#53356 = LINE ( 'NONE', #21455, #140304 ) ;
#53357 = CARTESIAN_POINT ( 'NONE',  ( 33.79289321881321939, 6.759292476615653023, 5.000000000000000000 ) ) ;
#53358 = VECTOR ( 'NONE', #89882, 1000.000000000000000 ) ;
#53359 = EDGE_CURVE ( 'NONE', #95686, #122429, #65535, .T. ) ;
#53360 = CYLINDRICAL_SURFACE ( 'NONE', #99369, 6.094999999999989093 ) ;
#53361 = ORIENTED_EDGE ( 'NONE', *, *, #49910, .F. ) ;
#53362 = VERTEX_POINT ( 'NONE', #107558 ) ;
#53363 = CARTESIAN_POINT ( 'NONE',  ( 61.54209685856476852, 5.291415217122923842, -3.054999999999996163 ) ) ;
#53364 = EDGE_LOOP ( 'NONE', ( #3086, #45607, #6224, #63262 ) ) ;
#53365 = EDGE_CURVE ( 'NONE', #141369, #51675, #42338, .T. ) ;
#53366 = CARTESIAN_POINT ( 'NONE',  ( -9.134995737516172554, 3.759292476615678336, 15.36553568819728355 ) ) ;
#53367 = CARTESIAN_POINT ( 'NONE',  ( 11.99999999999991296, -7.068876922607741697, 4.000000000000000000 ) ) ;
#53368 = VECTOR ( 'NONE', #139078, 999.9999999999998863 ) ;
#53369 = FACE_OUTER_BOUND ( 'NONE', #106537, .T. ) ;
#53370 = LINE ( 'NONE', #9101, #38580 ) ;
#53371 = EDGE_LOOP ( 'NONE', ( #26338, #85282, #59623, #87310 ) ) ;
#53372 = CARTESIAN_POINT ( 'NONE',  ( 4.499999999999972466, 10.08746187583913922, 4.000000000000000000 ) ) ;
#53374 =( BOUNDED_CURVE ( )  B_SPLINE_CURVE ( 3, ( #33977, #66604, #11461, #65191 ),
 .UNSPECIFIED., .F., .F. ) 
 B_SPLINE_CURVE_WITH_KNOTS ( ( 4, 4 ),
 ( 1.570796326794896558, 3.141592653589793560 ),
 .UNSPECIFIED. ) 
 CURVE ( )  GEOMETRIC_REPRESENTATION_ITEM ( )  RATIONAL_B_SPLINE_CURVE ( ( 1.000000000000000000, 0.8047378541243649375, 0.8047378541243649375, 1.000000000000000000 ) ) 
 REPRESENTATION_ITEM ( '' )  );
#53373 = CYLINDRICAL_SURFACE ( 'NONE', #30490, 3.000000000000002665 ) ;
#53375 = VECTOR ( 'NONE', #55345, 1000.000000000000000 ) ;
#53376 = EDGE_LOOP ( 'NONE', ( #132601, #12071, #46103, #82765 ) ) ;
#53377 = AXIS2_PLACEMENT_3D ( 'NONE', #128496, #17560, #16873 ) ;
#53378 = DIRECTION ( 'NONE',  ( 0.7071067811865487940, 0.7071067811865463515, -0.000000000000000000 ) ) ;
#53379 = VECTOR ( 'NONE', #67639, 999.9999999999998863 ) ;
#53380 = LINE ( 'NONE', #97587, #105803 ) ;
#53381 = CARTESIAN_POINT ( 'NONE',  ( -42.18398860626899705, 28.73617430169816700, 5.000000000000000000 ) ) ;
#53382 = VECTOR ( 'NONE', #43874, 1000.000000000000000 ) ;
#53383 = ORIENTED_EDGE ( 'NONE', *, *, #79749, .F. ) ;
#53384 = ORIENTED_EDGE ( 'NONE', *, *, #12367, .T. ) ;
#53385 = EDGE_CURVE ( 'NONE', #42960, #45983, #140204, .T. ) ;
#53386 = FACE_BOUND ( 'NONE', #96237, .T. ) ;
#53387 = VECTOR ( 'NONE', #30861, 1000.000000000000227 ) ;
#53388 = DIRECTION ( 'NONE',  ( -0.7071067811865487940, 0.7071067811865463515, -0.000000000000000000 ) ) ;
#53389 = EDGE_CURVE ( 'NONE', #140659, #13117, #132199, .T. ) ;
#53390 = CARTESIAN_POINT ( 'NONE',  ( 127.2844355792472584, -1.701477371938903360, 6.349999999999264233 ) ) ;
#53391 = FACE_OUTER_BOUND ( 'NONE', #26260, .T. ) ;
#53392 = CARTESIAN_POINT ( 'NONE',  ( -10.49999999999992895, 16.77039438581778796, 0.4657186855307983153 ) ) ;
#53393 =( LENGTH_UNIT ( ) NAMED_UNIT ( * ) SI_UNIT ( .MILLI., .METRE. ) );
#53394 = VERTEX_POINT ( 'NONE', #120547 ) ;
#53395 = EDGE_CURVE ( 'NONE', #102321, #137557, #130044, .T. ) ;
#53396 = VECTOR ( 'NONE', #84537, 1000.000000000000000 ) ;
#53397 = VERTEX_POINT ( 'NONE', #21975 ) ;
#53398 = CARTESIAN_POINT ( 'NONE',  ( 109.5787635252314516, -7.482591942790325086E-16, 6.109999999999998543 ) ) ;
#53399 = EDGE_LOOP ( 'NONE', ( #82352, #51217, #102971, #12507 ) ) ;
#53400 = EDGE_CURVE ( 'NONE', #87047, #53796, #66224, .T. ) ;
#53401 = ORIENTED_EDGE ( 'NONE', *, *, #117092, .T. ) ;
#53402 = AXIS2_PLACEMENT_3D ( 'NONE', #105731, #39084, #39830 ) ;
#53403 = DIRECTION ( 'NONE',  ( -0.000000000000000000, 0.3543493200069153248, 0.9351131265310292928 ) ) ;
#53404 = EDGE_CURVE ( 'NONE', #127403, #19828, #130780, .T. ) ;
#53405 = DIRECTION ( 'NONE',  ( -8.817971600062198362E-18, -0.3543493200069152693, 0.9351131265310292928 ) ) ;
#53407 = EDGE_CURVE ( 'NONE', #103883, #33542, #110397, .T. ) ;
#53406 = CARTESIAN_POINT ( 'NONE',  ( -21.18398860626899349, 28.73617430169802134, 5.000000000000000000 ) ) ;
#53408 = ORIENTED_EDGE ( 'NONE', *, *, #93759, .T. ) ;
#53409 = LINE ( 'NONE', #130991, #103818 ) ;
#53410 = CARTESIAN_POINT ( 'NONE',  ( -33.29974487139158867, -27.71228299555229313, 4.000000000000000000 ) ) ;
#53411 = CARTESIAN_POINT ( 'NONE',  ( 26.27718569542921401, -21.72499999999999432, 5.000000000000000000 ) ) ;
#53412 = LINE ( 'NONE', #109219, #27685 ) ;
#53413 = AXIS2_PLACEMENT_3D ( 'NONE', #40628, #86275, #62384 ) ;
#53414 = CARTESIAN_POINT ( 'NONE',  ( 0.000000000000000000, -4.870000000000014317, -10.00000000000000178 ) ) ;
#53415 = ORIENTED_EDGE ( 'NONE', *, *, #10969, .T. ) ;
#53416 = PLANE ( 'NONE',  #70477 ) ;
#53417 = CARTESIAN_POINT ( 'NONE',  ( 0.07735795229993523703, -0.4000000000000003553, 2.152165010376130727 ) ) ;
#53418 = VERTEX_POINT ( 'NONE', #85098 ) ;
#53419 = CARTESIAN_POINT ( 'NONE',  ( -34.92500000000001137, 20.81665438641021382, 4.500000000000000888 ) ) ;
#53420 = VERTEX_POINT ( 'NONE', #129304 ) ;
#53422 = EDGE_LOOP ( 'NONE', ( #35821, #26605, #69273, #143306 ) ) ;
#53421 = ADVANCED_FACE ( 'NONE', ( #41589 ), #29995, .F. ) ;
#53423 = VERTEX_POINT ( 'NONE', #74974 ) ;
#53424 = CARTESIAN_POINT ( 'NONE',  ( 60.08376352523143993, -6.110000000000001208, -3.741295971395164515E-16 ) ) ;
#53426 = EDGE_LOOP ( 'NONE', ( #60534, #50947, #77247, #82423 ) ) ;
#53425 = AXIS2_PLACEMENT_3D ( 'NONE', #109669, #95219, #30711 ) ;
#53427 = ORIENTED_EDGE ( 'NONE', *, *, #79843, .T. ) ;
#53428 = DIRECTION ( 'NONE',  ( 0.000000000000000000, -1.000000000000000000, 0.000000000000000000 ) ) ;
#53429 = DIRECTION ( 'NONE',  ( 0.7071067811865486830, -0.7071067811865464625, -0.000000000000000000 ) ) ;
#53430 = CARTESIAN_POINT ( 'NONE',  ( 96.39626352523141861, 4.472830434245840259, -4.472830434245838482 ) ) ;
#53431 = CARTESIAN_POINT ( 'NONE',  ( -20.70025512860841133, -27.71228299555191654, 4.000000000000000000 ) ) ;
#53432 = CARTESIAN_POINT ( 'NONE',  ( -48.18398860626899705, 28.73617430169820608, 5.000000000000000000 ) ) ;
#53433 = ORIENTED_EDGE ( 'NONE', *, *, #52063, .F. ) ;
#53434 = DIRECTION ( 'NONE',  ( -0.000000000000000000, -0.3543493200069152693, 0.9351131265310292928 ) ) ;
#53435 = VECTOR ( 'NONE', #34417, 1000.000000000000227 ) ;
#53436 = PLANE ( 'NONE',  #86398 ) ;
#53437 = CARTESIAN_POINT ( 'NONE',  ( 91.41666666666667140, -6.884901960086287076, -3.975000000000000977 ) ) ;
#53439 = PLANE ( 'NONE',  #8128 ) ;
#53438 = CIRCLE ( 'NONE', #21041, 2.500000000000000888 ) ;
#53441 = ORIENTED_EDGE ( 'NONE', *, *, #82804, .T. ) ;
#53440 = AXIS2_PLACEMENT_3D ( 'NONE', #115385, #94383, #28441 ) ;
#53442 = CARTESIAN_POINT ( 'NONE',  ( 41.99451991528749062, 28.92564299267967343, 4.000000000000000000 ) ) ;
#53443 = ORIENTED_EDGE ( 'NONE', *, *, #8506, .T. ) ;
#53444 = ORIENTED_EDGE ( 'NONE', *, *, #76936, .T. ) ;
#53445 = EDGE_LOOP ( 'NONE', ( #43294, #15096, #8904, #129294 ) ) ;
#53446 = CARTESIAN_POINT ( 'NONE',  ( 123.7245968585647660, -1.637169565754160949, 6.109999999999997655 ) ) ;
#53447 = ADVANCED_FACE ( 'NONE', ( #119146 ), #64071, .F. ) ;
#53448 = CIRCLE ( 'NONE', #72011, 4.000000000000000000 ) ;
#53449 = AXIS2_PLACEMENT_3D ( 'NONE', #112169, #114288, #25124 ) ;
#53450 = ORIENTED_EDGE ( 'NONE', *, *, #90615, .T. ) ;
#53451 = VECTOR ( 'NONE', #116777, 1000.000000000000000 ) ;
#53452 = STYLED_ITEM ( 'NONE', ( #142872 ), #142559 ) ;
#53453 = AXIS2_PLACEMENT_3D ( 'NONE', #131547, #99603, #34374 ) ;
#53454 = DIRECTION ( 'NONE',  ( -0.000000000000000000, 0.000000000000000000, 1.000000000000000000 ) ) ;
#53455 = LINE ( 'NONE', #41145, #103365 ) ;
#53456 = DIRECTION ( 'NONE',  ( -0.7071067811865487940, 0.7071067811865463515, -0.000000000000000000 ) ) ;
#53457 = EDGE_CURVE ( 'NONE', #57200, #65937, #134334, .T. ) ;
#53458 = ORIENTED_EDGE ( 'NONE', *, *, #30466, .F. ) ;
#53459 = DIRECTION ( 'NONE',  ( -0.6830127018922181881, 0.6830127018922202975, -0.2588190451025214056 ) ) ;
#53461 = ORIENTED_EDGE ( 'NONE', *, *, #79742, .T. ) ;
#53460 = VECTOR ( 'NONE', #31613, 999.9999999999998863 ) ;
#53462 = EDGE_CURVE ( 'NONE', #39389, #14857, #5006, .T. ) ;
#53463 = ADVANCED_FACE ( 'NONE', ( #38401 ), #55347, .T. ) ;
#53464 = EDGE_CURVE ( 'NONE', #1086, #118931, #78519, .T. ) ;
#53465 = CARTESIAN_POINT ( 'NONE',  ( 17.77040314143522082, -7.934999999999989839, 2.126176841940957907 ) ) ;
#53466 = DIRECTION ( 'NONE',  ( 0.7071067811865487940, 0.7071067811865463515, -0.000000000000000000 ) ) ;
#53467 = EDGE_CURVE ( 'NONE', #65462, #92329, #2341, .T. ) ;
#53468 = DIRECTION ( 'NONE',  ( -0.7071067811865486830, -0.7071067811865464625, 0.000000000000000000 ) ) ;
#53469 = CIRCLE ( 'NONE', #130174, 2.500000000000000888 ) ;
#53470 = LINE ( 'NONE', #29554, #79140 ) ;
#53471 = ORIENTED_EDGE ( 'NONE', *, *, #40849, .T. ) ;
#53472 = ORIENTED_EDGE ( 'NONE', *, *, #74815, .T. ) ;
#53473 = EDGE_CURVE ( 'NONE', #138697, #41182, #126812, .T. ) ;
#53474 = VERTEX_POINT ( 'NONE', #27495 ) ;
#53476 = CIRCLE ( 'NONE', #37227, 4.749999999999997335 ) ;
#53475 = DIRECTION ( 'NONE',  ( -0.6830127018922180770, -0.6830127018922204085, -0.2588190451025213501 ) ) ;
#53477 = SURFACE_STYLE_FILL_AREA ( #9954 ) ;
#53478 = ADVANCED_FACE ( 'NONE', ( #56806 ), #45905, .F. ) ;
#53479 = DIRECTION ( 'NONE',  ( 0.7071067811865487940, 0.7071067811865463515, 0.000000000000000000 ) ) ;
#53480 = PLANE ( 'NONE',  #85318 ) ;
#53481 = LINE ( 'NONE', #131042, #68859 ) ;
#53482 = VECTOR ( 'NONE', #98848, 1000.000000000000227 ) ;
#53483 = EDGE_CURVE ( 'NONE', #86990, #35713, #89386, .T. ) ;
#53484 = AXIS2_PLACEMENT_3D ( 'NONE', #111865, #68387, #121991 ) ;
#53485 = LINE ( 'NONE', #54230, #20571 ) ;
#53486 = CARTESIAN_POINT ( 'NONE',  ( 30.04209685856476497, 5.291415217122923842, -3.054999999999996163 ) ) ;
#53487 =( LENGTH_UNIT ( ) NAMED_UNIT ( * ) SI_UNIT ( .MILLI., .METRE. ) );
#53488 = AXIS2_PLACEMENT_3D ( 'NONE', #42589, #22905, #120815 ) ;
#53489 = EDGE_LOOP ( 'NONE', ( #58774, #35975, #131126, #77004 ) ) ;
#53490 = LINE ( 'NONE', #122281, #122918 ) ;
#53491 = ORIENTED_EDGE ( 'NONE', *, *, #39800, .F. ) ;
#53493 = AXIS2_PLACEMENT_3D ( 'NONE', #79043, #34092, #131976 ) ;
#53492 = DIRECTION ( 'NONE',  ( 1.000000000000000000, -0.000000000000000000, -0.000000000000000000 ) ) ;
#53494 = ORIENTED_EDGE ( 'NONE', *, *, #21425, .F. ) ;
#53495 = EDGE_CURVE ( 'NONE', #16426, #85226, #69086, .T. ) ;
#53496 = DIRECTION ( 'NONE',  ( -0.7071067811865487940, 0.7071067811865463515, -0.000000000000000000 ) ) ;
#53498 = ORIENTED_EDGE ( 'NONE', *, *, #36775, .T. ) ;
#53497 = DIRECTION ( 'NONE',  ( 0.7071067811865487940, -0.7071067811865463515, 0.000000000000000000 ) ) ;
#53499 = LINE ( 'NONE', #142646, #530 ) ;
#53500 = ORIENTED_EDGE ( 'NONE', *, *, #2035, .F. ) ;
#53501 = LINE ( 'NONE', #9221, #13614 ) ;
#53502 = ORIENTED_EDGE ( 'NONE', *, *, #61422, .F. ) ;
#53503 = LINE ( 'NONE', #43342, #4973 ) ;
#53504 = UNCERTAINTY_MEASURE_WITH_UNIT (LENGTH_MEASURE( 1.000000000000000082E-05 ), #69572, 'distance_accuracy_value', 'NONE');
#53505 = VERTEX_POINT ( 'NONE', #135074 ) ;
#53506 = ADVANCED_FACE ( 'NONE', ( #49305 ), #24840, .T. ) ;
#53507 = CARTESIAN_POINT ( 'NONE',  ( 20.99451991528748707, 28.92564299267952777, 4.000000000000000000 ) ) ;
#53508 = CARTESIAN_POINT ( 'NONE',  ( 111.9333603837962272, 2.130196079827431532, -7.949999999999997513 ) ) ;
#53509 = CARTESIAN_POINT ( 'NONE',  ( -4.499999999999962697, -20.53675388469230967, 2.352720554255882224 ) ) ;
#53510 = AXIS2_PLACEMENT_3D ( 'NONE', #89586, #77333, #46864 ) ;
#53511 = SURFACE_STYLE_FILL_AREA ( #110700 ) ;
#53512 = CARTESIAN_POINT ( 'NONE',  ( 0.000000000000000000, -30.18000000000009564, -15.92500000000064375 ) ) ;
#53513 = DIRECTION ( 'NONE',  ( -1.000000000000000000, 0.000000000000000000, -0.000000000000000000 ) ) ;
#53514 = DIRECTION ( 'NONE',  ( 0.7071067811865486830, -0.7071067811865464625, -0.000000000000000000 ) ) ;
#53516 = AXIS2_PLACEMENT_3D ( 'NONE', #29444, #73682, #140360 ) ;
#53515 = CARTESIAN_POINT ( 'NONE',  ( 3.937500000000000000, -4.461849672132299105, 4.461849672132299993 ) ) ;
#53517 = CARTESIAN_POINT ( 'NONE',  ( 18.64540314143522082, -2.126176841940958351, -7.934999999999988951 ) ) ;
#53519 = MECHANICAL_DESIGN_GEOMETRIC_PRESENTATION_REPRESENTATION (  '', ( #97470 ), #102165 ) ;
#53518 = FILL_AREA_STYLE ('',( #75980 ) ) ;
#53520 = CARTESIAN_POINT ( 'NONE',  ( 24.84463820744543838, 1.742823668393624903, 4.000000000000000000 ) ) ;
#53521 = EDGE_LOOP ( 'NONE', ( #23742, #61328, #140865, #116073 ) ) ;
#53522 = ORIENTED_EDGE ( 'NONE', *, *, #105533, .F. ) ;
#53523 = LINE ( 'NONE', #142670, #16592 ) ;
#53524 = ORIENTED_EDGE ( 'NONE', *, *, #131921, .T. ) ;
#53525 = VECTOR ( 'NONE', #96897, 1000.000000000000000 ) ;
#53526 = EDGE_CURVE ( 'NONE', #75102, #33478, #90088, .T. ) ;
#53527 = DIRECTION ( 'NONE',  ( -0.7071067811865487940, 0.7071067811865463515, 0.000000000000000000 ) ) ;
#53528 = SURFACE_STYLE_FILL_AREA ( #119459 ) ;
#53529 = VECTOR ( 'NONE', #47101, 1000.000000000000000 ) ;
#53530 = ORIENTED_EDGE ( 'NONE', *, *, #58232, .F. ) ;
#53531 = CARTESIAN_POINT ( 'NONE',  ( -30.75860074219774631, 21.72500000000000142, 5.000000000000000000 ) ) ;
#53532 = DIRECTION ( 'NONE',  ( -0.7071067811865487940, -0.7071067811865463515, -0.000000000000000000 ) ) ;
#53533 = EDGE_CURVE ( 'NONE', #32425, #79691, #111107, .T. ) ;
#53534 = LINE ( 'NONE', #141989, #83602 ) ;
#53535 = CYLINDRICAL_SURFACE ( 'NONE', #121165, 7.950000000000000178 ) ;
#53537 = ORIENTED_EDGE ( 'NONE', *, *, #119154, .T. ) ;
#53536 = CARTESIAN_POINT ( 'NONE',  ( -6.005480084712508493, 28.92564299267933947, 4.000000000000000000 ) ) ;
#53538 = CARTESIAN_POINT ( 'NONE',  ( 66.18398860626901126, 28.73617430169833753, 5.000000000000000000 ) ) ;
#53539 = DIRECTION ( 'NONE',  ( -0.7071067811865486830, -0.7071067811865464625, -0.000000000000000000 ) ) ;
#53540 = AXIS2_PLACEMENT_3D ( 'NONE', #88128, #116639, #6394 ) ;
#53541 = CARTESIAN_POINT ( 'NONE',  ( -4.499999999999968914, -2.173586137069142499, -4.605770156576121543 ) ) ;
#53542 = CARTESIAN_POINT ( 'NONE',  ( 7.499999999999947597, 14.14708470758592007, -0.5283514160166723483 ) ) ;
#53543 = EDGE_CURVE ( 'NONE', #105369, #136234, #44493, .T. ) ;
#53544 = CARTESIAN_POINT ( 'NONE',  ( -13.62823445044376491, -8.240707523384200428, 11.38925528200755721 ) ) ;
#53545 = VERTEX_POINT ( 'NONE', #123481 ) ;
#53546 = ORIENTED_EDGE ( 'NONE', *, *, #142827, .F. ) ;
#53547 = ORIENTED_EDGE ( 'NONE', *, *, #73138, .T. ) ;
#53548 = CARTESIAN_POINT ( 'NONE',  ( 92.45876352523144703, 0.000000000000000000, -6.110000000000001208 ) ) ;
#53549 =( BOUNDED_CURVE ( )  B_SPLINE_CURVE ( 3, ( #11991, #34481, #122916, #112746 ),
 .UNSPECIFIED., .F., .T. ) 
 B_SPLINE_CURVE_WITH_KNOTS ( ( 4, 4 ),
 ( 1.864375635226932282, 1.933014472006540752 ),
 .UNSPECIFIED. ) 
 CURVE ( )  GEOMETRIC_REPRESENTATION_ITEM ( )  RATIONAL_B_SPLINE_CURVE ( ( 1.000000000000000000, 0.9996074310407765395, 0.9996074310407765395, 1.000000000000000000 ) ) 
 REPRESENTATION_ITEM ( '' )  );
#53550 = VERTEX_POINT ( 'NONE', #112568 ) ;
#53551 = EDGE_CURVE ( 'NONE', #141006, #17257, #23401, .T. ) ;
#53552 = CARTESIAN_POINT ( 'NONE',  ( 129.9042113015468374, -47.96374157527412763, 37.32649486623389379 ) ) ;
#53553 = DIRECTION ( 'NONE',  ( -1.000000000000000000, -1.224606353822377258E-16, -0.000000000000000000 ) ) ;
#53554 = ORIENTED_EDGE ( 'NONE', *, *, #18063, .T. ) ;
#53555 = AXIS2_PLACEMENT_3D ( 'NONE', #123915, #47108, #36185 ) ;
#53556 = CARTESIAN_POINT ( 'NONE',  ( 184.1499999999998352, -50.24077216217763464, 35.40405119785170029 ) ) ;
#53557 = CARTESIAN_POINT ( 'NONE',  ( -25.39999999999996305, 0.000000000000000000, 2.500000000000000000 ) ) ;
#53558 = MECHANICAL_DESIGN_GEOMETRIC_PRESENTATION_REPRESENTATION (  '', ( #116148 ), #53668 ) ;
#53559 = VECTOR ( 'NONE', #143086, 999.9999999999998863 ) ;
#53560 = CARTESIAN_POINT ( 'NONE',  ( 93.39126352523143737, -4.472830434245839371, -4.472830434245839371 ) ) ;
#53561 = EDGE_LOOP ( 'NONE', ( #74697, #21930, #399, #89825 ) ) ;
#53562 = CARTESIAN_POINT ( 'NONE',  ( 0.02893550784256476716, 0.5999999999999988676, -3.399425482353704453 ) ) ;
#53563 = VECTOR ( 'NONE', #38329, 1000.000000000000114 ) ;
#53564 = VECTOR ( 'NONE', #103235, 1000.000000000000227 ) ;
#53565 = CARTESIAN_POINT ( 'NONE',  ( -27.48921356237309155, -27.52281430457074762, 5.000000000000000000 ) ) ;
#53566 = COLOUR_RGB ( '', 0.72549020, 0.75294118, 0.79215686) ;
#53567 = AXIS2_PLACEMENT_3D ( 'NONE', #45570, #47717, #25189 ) ;
#53568 = AXIS2_PLACEMENT_3D ( 'NONE', #112644, #135146, #35840 ) ;
#53569 = EDGE_LOOP ( 'NONE', ( #58590, #91661, #76066, #1388 ) ) ;
#53570 = ORIENTED_EDGE ( 'NONE', *, *, #137772, .F. ) ;
#53571 = EDGE_CURVE ( 'NONE', #2765, #85157, #24137, .T. ) ;
#53572 = EDGE_LOOP ( 'NONE', ( #89817, #124928, #70544, #100703 ) ) ;
#53573 = FACE_OUTER_BOUND ( 'NONE', #73312, .T. ) ;
#53574 = EDGE_CURVE ( 'NONE', #43296, #68456, #101684, .T. ) ;
#53575 = CARTESIAN_POINT ( 'NONE',  ( 151.4000000000000057, -17.48000000000005016, 12.69999999999954454 ) ) ;
#53576 = CARTESIAN_POINT ( 'NONE',  ( 13.62956980810188767, -3.967499999999998028, -6.871911579029511330 ) ) ;
#53577 = FACE_OUTER_BOUND ( 'NONE', #54343, .T. ) ;
#53578 = AXIS2_PLACEMENT_3D ( 'NONE', #82269, #126446, #5372 ) ;
#53579 = CARTESIAN_POINT ( 'NONE',  ( 163.5342603869775076, 26.96999999999993847, 34.56026864331079196 ) ) ;
#53580 = PLANE ( 'NONE',  #23232 ) ;
#53581 =( NAMED_UNIT ( * ) PLANE_ANGLE_UNIT ( ) SI_UNIT ( $, .RADIAN. ) );
#53582 = VERTEX_POINT ( 'NONE', #77808 ) ;
#53583 = ORIENTED_EDGE ( 'NONE', *, *, #67790, .T. ) ;
#53584 = VECTOR ( 'NONE', #84463, 1000.000000000000000 ) ;
#53585 = EDGE_CURVE ( 'NONE', #108392, #40720, #66930, .T. ) ;
#53586 = CARTESIAN_POINT ( 'NONE',  ( -45.29974487139158867, -27.71228299555237840, 4.000000000000000000 ) ) ;
#53587 = ORIENTED_EDGE ( 'NONE', *, *, #52012, .T. ) ;
#53588 = ORIENTED_EDGE ( 'NONE', *, *, #80356, .T. ) ;
#53589 = EDGE_CURVE ( 'NONE', #140226, #97836, #90845, .T. ) ;
#53590 = EDGE_CURVE ( 'NONE', #114247, #68937, #52811, .T. ) ;
#53591 = STYLED_ITEM ( 'NONE', ( #51459 ), #99140 ) ;
#53592 = VECTOR ( 'NONE', #28951, 1000.000000000000227 ) ;
#53594 = EDGE_CURVE ( 'NONE', #141614, #125764, #50004, .T. ) ;
#53593 = DIRECTION ( 'NONE',  ( 0.7071067811865487940, 0.7071067811865463515, 0.000000000000000000 ) ) ;
#53595 = ORIENTED_EDGE ( 'NONE', *, *, #96986, .F. ) ;
#53596 = CARTESIAN_POINT ( 'NONE',  ( -34.92500000000001137, -22.22500000000000142, 4.000000000000000000 ) ) ;
#53597 = DIRECTION ( 'NONE',  ( -1.000000000000000000, -1.224606353822377258E-16, -0.000000000000000000 ) ) ;
#53598 = AXIS2_PLACEMENT_3D ( 'NONE', #75900, #20790, #9916 ) ;
#53599 = CARTESIAN_POINT ( 'NONE',  ( 8.187538124160473885, -22.22500000000000142, 4.000000000000000000 ) ) ;
#53600 = CARTESIAN_POINT ( 'NONE',  ( -45.48921356237309510, -27.52281430457087197, 5.000000000000000000 ) ) ;
#53601 = AXIS2_PLACEMENT_3D ( 'NONE', #91164, #37488, #26597 ) ;
#53602 = CARTESIAN_POINT ( 'NONE',  ( 65.99451991528749772, 28.92564299267984396, 4.000000000000000000 ) ) ;
#53603 = ORIENTED_EDGE ( 'NONE', *, *, #102486, .F. ) ;
#53604 = EDGE_LOOP ( 'NONE', ( #54936, #26911, #61804, #44400 ) ) ;
#53605 = CARTESIAN_POINT ( 'NONE',  ( 25.40000000000004476, 7.048307320969255052, -3.667349112489660001 ) ) ;
#53606 = CARTESIAN_POINT ( 'NONE',  ( -8.207106781186485733, 0.7592924766157138627, 5.000000000000000000 ) ) ;
#53607 = ORIENTED_EDGE ( 'NONE', *, *, #142669, .F. ) ;
#53608 = AXIS2_PLACEMENT_3D ( 'NONE', #124099, #11736, #133559 ) ;
#53609 = CARTESIAN_POINT ( 'NONE',  ( -14.99451991528749595, 28.92564299267948513, 4.000000000000000000 ) ) ;
#53610 = EDGE_CURVE ( 'NONE', #136709, #115243, #94891, .T. ) ;
#53611 = EDGE_LOOP ( 'NONE', ( #41281, #28934, #34252, #77028, #24757 ) ) ;
#53612 = DIRECTION ( 'NONE',  ( -0.000000000000000000, -0.3543493200069152693, 0.9351131265310292928 ) ) ;
#53613 = ORIENTED_EDGE ( 'NONE', *, *, #142016, .T. ) ;
#53614 = ORIENTED_EDGE ( 'NONE', *, *, #34279, .F. ) ;
#53615 = ORIENTED_EDGE ( 'NONE', *, *, #85879, .F. ) ;
#53616 =( BOUNDED_CURVE ( )  B_SPLINE_CURVE ( 3, ( #23504, #25643, #70631, #68478 ),
 .UNSPECIFIED., .F., .T. ) 
 B_SPLINE_CURVE_WITH_KNOTS ( ( 4, 4 ),
 ( 4.350170835173026163, 4.500739107949217832 ),
 .UNSPECIFIED. ) 
 CURVE ( )  GEOMETRIC_REPRESENTATION_ITEM ( )  RATIONAL_B_SPLINE_CURVE ( ( 1.000000000000000000, 0.9981116584018955296, 0.9981116584018955296, 1.000000000000000000 ) ) 
 REPRESENTATION_ITEM ( '' )  );
#53617 = DIRECTION ( 'NONE',  ( -0.000000000000000000, 0.000000000000000000, 1.000000000000000000 ) ) ;
#53618 = LINE ( 'NONE', #118853, #62323 ) ;
#53619 = CARTESIAN_POINT ( 'NONE',  ( 0.000000000000000000, 0.000000000000000000, 5.000000000000000000 ) ) ;
#53620 = CARTESIAN_POINT ( 'NONE',  ( -34.49999999999975131, -4.535744391599457082, 4.994342998332168548 ) ) ;
#53621 = DIRECTION ( 'NONE',  ( 0.6830127018922181881, 0.6830127018922202975, -0.2588190451025214056 ) ) ;
#53622 = DIRECTION ( 'NONE',  ( 0.3543493200069163240, 0.000000000000000000, 0.9351131265310288487 ) ) ;
#53624 = LINE ( 'NONE', #7209, #66660 ) ;
#53623 = AXIS2_PLACEMENT_3D ( 'NONE', #21082, #132010, #1449 ) ;
#53625 = VECTOR ( 'NONE', #61722, 1000.000000000000000 ) ;
#53626 = DIRECTION ( 'NONE',  ( -0.7071067811865486830, -0.7071067811865464625, -0.000000000000000000 ) ) ;
#53627 = DIRECTION ( 'NONE',  ( -0.000000000000000000, -0.3543493200069152693, 0.9351131265310292928 ) ) ;
#53628 = LINE ( 'NONE', #131897, #38983 ) ;
#53629 = LINE ( 'NONE', #43455, #130441 ) ;
#53630 = ORIENTED_EDGE ( 'NONE', *, *, #57757, .F. ) ;
#53631 = VERTEX_POINT ( 'NONE', #106464 ) ;
#53632 = ORIENTED_EDGE ( 'NONE', *, *, #66655, .T. ) ;
#53633 = VECTOR ( 'NONE', #137104, 1000.000000000000000 ) ;
#53634 = ORIENTED_EDGE ( 'NONE', *, *, #47782, .T. ) ;
#53635 = CARTESIAN_POINT ( 'NONE',  ( 21.46453280170069888, 2.055000000000001048, 0.000000000000000000 ) ) ;
#53636 = ORIENTED_EDGE ( 'NONE', *, *, #105398, .F. ) ;
#53637 = ORIENTED_EDGE ( 'NONE', *, *, #101009, .F. ) ;
#53638 = CARTESIAN_POINT ( 'NONE',  ( -12.29974487139158512, -27.71228299555214747, 4.000000000000000000 ) ) ;
#53639 = DIRECTION ( 'NONE',  ( 1.000000000000000000, 0.000000000000000000, 0.000000000000000000 ) ) ;
#53640 = VERTEX_POINT ( 'NONE', #97009 ) ;
#53641 = LINE ( 'NONE', #97852, #129783 ) ;
#53642 = AXIS2_PLACEMENT_3D ( 'NONE', #50123, #94319, #107338 ) ;
#53643 = ORIENTED_EDGE ( 'NONE', *, *, #78554, .F. ) ;
#53644 = PLANE ( 'NONE',  #86252 ) ;
#53645 = FACE_OUTER_BOUND ( 'NONE', #47211, .T. ) ;
#53646 = EDGE_CURVE ( 'NONE', #101759, #113128, #109150, .T. ) ;
#53647 = CARTESIAN_POINT ( 'NONE',  ( 10.12956980810188767, -3.967499999999998028, -6.871911579029511330 ) ) ;
#53648 = ORIENTED_EDGE ( 'NONE', *, *, #127836, .T. ) ;
#53649 = CARTESIAN_POINT ( 'NONE',  ( 90.76626352523146579, 4.472830434245839371, -4.472830434245839371 ) ) ;
#53650 = EDGE_CURVE ( 'NONE', #62423, #138332, #60911, .T. ) ;
#53651 = CARTESIAN_POINT ( 'NONE',  ( 7.437137942570125837, -8.911461087268691017, 3.298467410628505014 ) ) ;
#53652 = EDGE_CURVE ( 'NONE', #117341, #3772, #84756, .T. ) ;
#53653 = CARTESIAN_POINT ( 'NONE',  ( 36.48921356237310221, -27.52281430457080802, 5.000000000000000000 ) ) ;
#53654 = CARTESIAN_POINT ( 'NONE',  ( -27.71757738642548574, -21.73023691814493574, 5.000000000000000888 ) ) ;
#53655 = ORIENTED_EDGE ( 'NONE', *, *, #81151, .F. ) ;
#53656 = EDGE_LOOP ( 'NONE', ( #64472, #126685, #67031, #41532 ) ) ;
#53657 = ADVANCED_FACE ( 'NONE', ( #17348 ), #130418, .F. ) ;
#53658 = CARTESIAN_POINT ( 'NONE',  ( -7.499999999999942268, -1.533600742197722910, 5.000000000000000000 ) ) ;
#53659 = ORIENTED_EDGE ( 'NONE', *, *, #105014, .T. ) ;
#53660 = DIRECTION ( 'NONE',  ( -0.7071067811865486830, 0.7071067811865464625, 0.000000000000000000 ) ) ;
#53661 = CARTESIAN_POINT ( 'NONE',  ( 28.82816939922333432, -17.24070752338409918, 4.000000000000000000 ) ) ;
#53662 = AXIS2_PLACEMENT_3D ( 'NONE', #60653, #104075, #25829 ) ;
#53664 = DIRECTION ( 'NONE',  ( 0.000000000000000000, 0.000000000000000000, -1.000000000000000000 ) ) ;
#53663 = VECTOR ( 'NONE', #94970, 1000.000000000000000 ) ;
#53665 = EDGE_CURVE ( 'NONE', #1213, #42638, #108583, .T. ) ;
#53666 = PLANE ( 'NONE',  #42634 ) ;
#53667 = VERTEX_POINT ( 'NONE', #39856 ) ;
#53668 =( GEOMETRIC_REPRESENTATION_CONTEXT ( 3 ) GLOBAL_UNCERTAINTY_ASSIGNED_CONTEXT ( ( #25835 ) ) GLOBAL_UNIT_ASSIGNED_CONTEXT ( ( #68450, #23471, #45272 ) ) REPRESENTATION_CONTEXT ( 'NONE', 'WORKASPACE' ) );
#53669 = DIRECTION ( 'NONE',  ( 0.3543493200069162685, -0.000000000000000000, -0.9351131265310288487 ) ) ;
#53670 = CIRCLE ( 'NONE', #9648, 1.898649999999993065 ) ;
#53671 = EDGE_CURVE ( 'NONE', #58614, #99505, #7148, .T. ) ;
#53672 = CARTESIAN_POINT ( 'NONE',  ( -10.49999999999993250, 3.653845994658382779, -4.504631822206345504 ) ) ;
#53673 = CARTESIAN_POINT ( 'NONE',  ( -34.49999999999975842, -7.535744391599424219, 4.994342998332167660 ) ) ;
#53674 = EDGE_LOOP ( 'NONE', ( #32195, #94305, #87038, #20451 ) ) ;
#53675 = CARTESIAN_POINT ( 'NONE',  ( -48.18398860626899705, 28.73617430169820608, 5.000000000000000000 ) ) ;
#53676 = VECTOR ( 'NONE', #1899, 1000.000000000000000 ) ;
#53677 = VECTOR ( 'NONE', #98446, 1000.000000000000227 ) ;
#53678 = VECTOR ( 'NONE', #14970, 1000.000000000000000 ) ;
#53679 = VECTOR ( 'NONE', #117874, 1000.000000000000000 ) ;
#53680 = CARTESIAN_POINT ( 'NONE',  ( -13.29703526515639567, -22.22500000000000142, 13.19564433381002466 ) ) ;
#53682 = VERTEX_POINT ( 'NONE', #5735 ) ;
#53681 = VECTOR ( 'NONE', #83373, 999.9999999999998863 ) ;
#53683 = EDGE_CURVE ( 'NONE', #63651, #64860, #84076, .T. ) ;
#53685 = ORIENTED_EDGE ( 'NONE', *, *, #29664, .T. ) ;
#53684 = FACE_OUTER_BOUND ( 'NONE', #71153, .T. ) ;
#53686 = ORIENTED_EDGE ( 'NONE', *, *, #100375, .T. ) ;
#53687 = ADVANCED_FACE ( 'NONE', ( #138428 ), #62305, .F. ) ;
#53688 = CARTESIAN_POINT ( 'NONE',  ( -4.828169399223495084, -8.240707523384198652, 4.000000000000000000 ) ) ;
#53689 = LINE ( 'NONE', #117465, #129425 ) ;
#53690 = VERTEX_POINT ( 'NONE', #116663 ) ;
#53691 = DIRECTION ( 'NONE',  ( 0.6830127018922180770, 0.6830127018922202975, -0.2588190451025213501 ) ) ;
#53692 = EDGE_CURVE ( 'NONE', #80743, #108597, #25843, .T. ) ;
#53693 = DIRECTION ( 'NONE',  ( -0.000000000000000000, -0.3543493200069152693, 0.9351131265310292928 ) ) ;
#53694 = CARTESIAN_POINT ( 'NONE',  ( 57.18398860626899705, 28.73617430169827358, 5.000000000000000000 ) ) ;
#53695 = CARTESIAN_POINT ( 'NONE',  ( 0.1600000000000003919, -1.341267888597242441, -7.849467545898021648 ) ) ;
#53696 = CARTESIAN_POINT ( 'NONE',  ( 0.000000000000000000, -0.3999999999999997446, -2.500000000000000000 ) ) ;
#53697 = LINE ( 'NONE', #131969, #14751 ) ;
#53698 = CARTESIAN_POINT ( 'NONE',  ( 5.816011393731002066, 28.73617430169783304, 5.000000000000000000 ) ) ;
#53699 = EDGE_CURVE ( 'NONE', #90846, #17453, #29637, .T. ) ;
#53700 = DIRECTION ( 'NONE',  ( 0.7071067811865486830, -0.7071067811865464625, -0.000000000000000000 ) ) ;
#53701 = CARTESIAN_POINT ( 'NONE',  ( -21.29974487139158512, -27.71228299555221142, 4.000000000000000000 ) ) ;
#53702 = CARTESIAN_POINT ( 'NONE',  ( -15.18398860626900237, 28.73617430169797871, 5.000000000000000000 ) ) ;
#53703 = FACE_OUTER_BOUND ( 'NONE', #50714, .T. ) ;
#53704 = DIRECTION ( 'NONE',  ( -0.000000000000000000, 0.000000000000000000, 1.000000000000000000 ) ) ;
#53705 = ORIENTED_EDGE ( 'NONE', *, *, #69563, .T. ) ;
#53706 = VECTOR ( 'NONE', #24520, 1000.000000000000000 ) ;
#53707 = ORIENTED_EDGE ( 'NONE', *, *, #27435, .T. ) ;
#53708 = ORIENTED_EDGE ( 'NONE', *, *, #82333, .F. ) ;
#53709 = CARTESIAN_POINT ( 'NONE',  ( 98.85416666666664298, -2.130196079827425315, -7.950000000000001066 ) ) ;
#53710 = ORIENTED_EDGE ( 'NONE', *, *, #112206, .T. ) ;
#53711 = ORIENTED_EDGE ( 'NONE', *, *, #22225, .T. ) ;
#53712 = VECTOR ( 'NONE', #39751, 1000.000000000000000 ) ;
#53713 = ORIENTED_EDGE ( 'NONE', *, *, #91441, .F. ) ;
#53714 = ADVANCED_FACE ( 'NONE', ( #73882 ), #18760, .T. ) ;
#53715 = PLANE ( 'NONE',  #92019 ) ;
#53716 = FACE_OUTER_BOUND ( 'NONE', #137962, .T. ) ;
#53717 = AXIS2_PLACEMENT_3D ( 'NONE', #132174, #11046, #69059 ) ;
#53718 = ORIENTED_EDGE ( 'NONE', *, *, #33154, .F. ) ;
#53719 = DIRECTION ( 'NONE',  ( -1.000000000000000000, -0.000000000000000000, -0.000000000000000000 ) ) ;
#53720 = CARTESIAN_POINT ( 'NONE',  ( 32.99999999999977263, 19.55218569542897100, 5.000000000000000000 ) ) ;
#53721 = FACE_OUTER_BOUND ( 'NONE', #108666, .T. ) ;
#53722 = DIRECTION ( 'NONE',  ( -0.7071067811865486830, -0.7071067811865464625, -0.000000000000000000 ) ) ;
#53723 = EDGE_LOOP ( 'NONE', ( #101941, #123544, #123939, #38160 ) ) ;
#53724 = CARTESIAN_POINT ( 'NONE',  ( 3.716138108416388253, 12.21541996048661183, -27.07211710725142950 ) ) ;
#53725 = DIRECTION ( 'NONE',  ( -0.7071067811865486830, 0.7071067811865464625, 0.000000000000000000 ) ) ;
#53726 = CARTESIAN_POINT ( 'NONE',  ( 39.29974487139159578, -27.71228299555233576, 4.000000000000000000 ) ) ;
#53728 = AXIS2_PLACEMENT_3D ( 'NONE', #125650, #137233, #26328 ) ;
#53727 = DIRECTION ( 'NONE',  ( -1.000000000000000000, -1.224606353822377258E-16, -0.000000000000000000 ) ) ;
#53729 = CARTESIAN_POINT ( 'NONE',  ( 24.20833333333333570, 3.047499999999997655, 5.278424836066143655 ) ) ;
#53730 = CARTESIAN_POINT ( 'NONE',  ( 71.99451991528749772, 28.92564299267988304, 4.000000000000000000 ) ) ;
#53731 = CARTESIAN_POINT ( 'NONE',  ( 31.72502705046288796, 5.819803920172573086, -5.819803920172572198 ) ) ;
#53732 = EDGE_CURVE ( 'NONE', #15939, #9981, #139155, .T. ) ;
#53733 = FACE_OUTER_BOUND ( 'NONE', #108904, .T. ) ;
#53734 = ORIENTED_EDGE ( 'NONE', *, *, #56518, .T. ) ;
#53735 = ORIENTED_EDGE ( 'NONE', *, *, #79193, .T. ) ;
#53736 = CARTESIAN_POINT ( 'NONE',  ( 29.72916666666665009, 7.950000000000001954, -2.130196079827421762 ) ) ;
#53737 = ORIENTED_EDGE ( 'NONE', *, *, #35829, .F. ) ;
#53738 = PLANE ( 'NONE',  #71841 ) ;
#53739 = EDGE_CURVE ( 'NONE', #48205, #332, #51429, .T. ) ;
#53740 = VECTOR ( 'NONE', #76015, 1000.000000000000000 ) ;
#53741 = CARTESIAN_POINT ( 'NONE',  ( 151.4000000000000057, -18.48000000000005372, 33.92499999999998295 ) ) ;
#53742 = CONICAL_SURFACE ( 'NONE', #88508, 2.500000000000000444, 0.9599310885968830309 ) ;
#53743 = FACE_OUTER_BOUND ( 'NONE', #19578, .T. ) ;
#53744 = DIRECTION ( 'NONE',  ( -0.7071067811865487940, 0.7071067811865463515, 0.000000000000000000 ) ) ;
#53745 = DIRECTION ( 'NONE',  ( 1.000000000000000000, -0.000000000000000000, -0.000000000000000000 ) ) ;
#53746 = CARTESIAN_POINT ( 'NONE',  ( -26.38161509397988169, -2.240707523384264377, 13.37739548510245235 ) ) ;
#53747 = CARTESIAN_POINT ( 'NONE',  ( 126.9329301918981088, 1.637169565754156508, 6.110000000000000320 ) ) ;
#53748 = ORIENTED_EDGE ( 'NONE', *, *, #53590, .T. ) ;
#53749 = ADVANCED_FACE ( 'NONE', ( #73189 ), #117352, .F. ) ;
#53750 = ORIENTED_EDGE ( 'NONE', *, *, #75621, .F. ) ;
#53751 = VECTOR ( 'NONE', #20458, 1000.000000000000227 ) ;
#53752 = LINE ( 'NONE', #43564, #78656 ) ;
#53753 = FACE_OUTER_BOUND ( 'NONE', #4893, .T. ) ;
#53754 = DIRECTION ( 'NONE',  ( 0.000000000000000000, -1.000000000000000000, 0.000000000000000000 ) ) ;
#53755 = PLANE ( 'NONE',  #92787 ) ;
#53756 = ORIENTED_EDGE ( 'NONE', *, *, #109268, .T. ) ;
#53757 = CARTESIAN_POINT ( 'NONE',  ( 49.29209685856476852, -5.291415217122921177, 3.054999999999999272 ) ) ;
#53758 = EDGE_CURVE ( 'NONE', #38491, #19628, #581, .T. ) ;
#53759 = VERTEX_POINT ( 'NONE', #133282 ) ;
#53760 = DIRECTION ( 'NONE',  ( 1.000000000000000000, 0.000000000000000000, 0.000000000000000000 ) ) ;
#53761 = CARTESIAN_POINT ( 'NONE',  ( 12.35051985313232237, -2.500000000000000000, 3.061616997868383634E-16 ) ) ;
#53762 = CARTESIAN_POINT ( 'NONE',  ( -34.49999999999976552, -8.945670655168967755, 4.994342998332164996 ) ) ;
#53763 = FACE_OUTER_BOUND ( 'NONE', #35173, .T. ) ;
#53764 = AXIS2_PLACEMENT_3D ( 'NONE', #103415, #37487, #16396 ) ;
#53765 = CARTESIAN_POINT ( 'NONE',  ( 35.05793019189811588, 6.110000000000000320, -1.637169565754156064 ) ) ;
#53766 = EDGE_LOOP ( 'NONE', ( #29627, #18421, #72324, #140589, #29025 ) ) ;
#53767 = CARTESIAN_POINT ( 'NONE',  ( -33.70710678118631165, -9.740707523384180888, 5.000000000000000000 ) ) ;
#53768 = ORIENTED_EDGE ( 'NONE', *, *, #40527, .F. ) ;
#53769 = ORIENTED_EDGE ( 'NONE', *, *, #142550, .F. ) ;
#53770 = VECTOR ( 'NONE', #137300, 1000.000000000000000 ) ;
#53771 = ORIENTED_EDGE ( 'NONE', *, *, #110966, .F. ) ;
#53772 = AXIS2_PLACEMENT_3D ( 'NONE', #143420, #23796, #88352 ) ;
#53773 = AXIS2_PLACEMENT_3D ( 'NONE', #66479, #14208, #56351 ) ;
#53774 = VECTOR ( 'NONE', #75525, 999.9999999999998863 ) ;
#53775 = CARTESIAN_POINT ( 'NONE',  ( 79.12086038379622721, -6.884901960086286188, 3.974999999999997424 ) ) ;
#53776 = EDGE_CURVE ( 'NONE', #114717, #11535, #65171, .T. ) ;
#53777 = EDGE_LOOP ( 'NONE', ( #28010, #20485, #112257, #16756 ) ) ;
#53778 = CARTESIAN_POINT ( 'NONE',  ( 24.18398860626899705, 28.73617430169804265, 5.000000000000000000 ) ) ;
#53780 = CARTESIAN_POINT ( 'NONE',  ( 6.299744871391586898, -27.71228299555210484, 4.000000000000000000 ) ) ;
#53779 = AXIS2_PLACEMENT_3D ( 'NONE', #61937, #5361, #7507 ) ;
#53781 = MECHANICAL_DESIGN_GEOMETRIC_PRESENTATION_REPRESENTATION (  '', ( #2831 ), #102429 ) ;
#53782 = COLOUR_RGB ( '', 0.08235294, 0.09019608, 0.10196078) ;
#53783 = FACE_OUTER_BOUND ( 'NONE', #41743, .T. ) ;
#53784 = LINE ( 'NONE', #56665, #5001 ) ;
#53785 = EDGE_CURVE ( 'NONE', #21943, #12779, #75325, .T. ) ;
#53786 = FACE_BOUND ( 'NONE', #55206, .T. ) ;
#53787 = EDGE_LOOP ( 'NONE', ( #71510, #59624, #104890, #99403, #42316 ) ) ;
#53788 = DIRECTION ( 'NONE',  ( 1.000000000000000000, -0.000000000000000000, -0.000000000000000000 ) ) ;
#53789 = CARTESIAN_POINT ( 'NONE',  ( 9.489213562373095101, -27.52281430457062328, 5.000000000000000000 ) ) ;
#53790 = EDGE_CURVE ( 'NONE', #7267, #60163, #20906, .T. ) ;
#53791 = ORIENTED_EDGE ( 'NONE', *, *, #109907, .T. ) ;
#53792 = FACE_OUTER_BOUND ( 'NONE', #21991, .T. ) ;
#53793 = EDGE_LOOP ( 'NONE', ( #76245, #120339, #111435, #71526 ) ) ;
#53794 = ORIENTED_EDGE ( 'NONE', *, *, #12810, .F. ) ;
#53795 = DIRECTION ( 'NONE',  ( -1.000000000000000000, -1.224606353822377258E-16, -0.000000000000000000 ) ) ;
#53796 = VERTEX_POINT ( 'NONE', #33964 ) ;
#53797 = CARTESIAN_POINT ( 'NONE',  ( 58.68293019189811588, -1.637169565754158951, -6.109999999999998543 ) ) ;
#53798 = ORIENTED_EDGE ( 'NONE', *, *, #32765, .T. ) ;
#53799 = CARTESIAN_POINT ( 'NONE',  ( 21.48921356237309155, -27.52281430457070499, 5.000000000000000000 ) ) ;
#53800 = VERTEX_POINT ( 'NONE', #119491 ) ;
#53801 = DIRECTION ( 'NONE',  ( 1.000000000000000000, 0.000000000000000000, 0.000000000000000000 ) ) ;
#53802 = EDGE_LOOP ( 'NONE', ( #124849, #84673, #48390, #89280 ) ) ;
#53803 = LINE ( 'NONE', #85676, #58417 ) ;
#53804 = DIRECTION ( 'NONE',  ( -0.7071067811865486830, -0.7071067811865464625, 0.000000000000000000 ) ) ;
#53805 = EDGE_CURVE ( 'NONE', #68252, #51146, #67303, .T. ) ;
#53806 = VECTOR ( 'NONE', #59518, 1000.000000000000227 ) ;
#53807 = LINE ( 'NONE', #117575, #117255 ) ;
#53808 = DIRECTION ( 'NONE',  ( 0.7071067811865487940, -0.7071067811865463515, 0.000000000000000000 ) ) ;
#53809 = DIRECTION ( 'NONE',  ( -0.7071067811865487940, 0.7071067811865463515, 0.000000000000000000 ) ) ;
#53810 = VECTOR ( 'NONE', #95354, 1000.000000000000227 ) ;
#53811 = DIRECTION ( 'NONE',  ( -0.6830127018922181881, 0.6830127018922202975, -0.2588190451025214056 ) ) ;
#53812 = CARTESIAN_POINT ( 'NONE',  ( 24.48921356237309510, -27.52281430457072631, 5.000000000000000000 ) ) ;
#53813 = ORIENTED_EDGE ( 'NONE', *, *, #11518, .F. ) ;
#53814 = ORIENTED_EDGE ( 'NONE', *, *, #27130, .F. ) ;
#53815 = ORIENTED_EDGE ( 'NONE', *, *, #42029, .F. ) ;
#53816 = CIRCLE ( 'NONE', #118565, 0.5000000000000004441 ) ;
#53817 = CARTESIAN_POINT ( 'NONE',  ( 19.87913961620377279, -5.278424836066145431, -3.047499999999993658 ) ) ;
#53818 = DIRECTION ( 'NONE',  ( -0.7071067811865486830, -0.7071067811865464625, 0.000000000000000000 ) ) ;
#53819 = ORIENTED_EDGE ( 'NONE', *, *, #19738, .F. ) ;
#53820 = ORIENTED_EDGE ( 'NONE', *, *, #3721, .T. ) ;
#53821 = DIRECTION ( 'NONE',  ( 0.7071067811865486830, -0.7071067811865464625, -0.000000000000000000 ) ) ;
#53822 = FACE_OUTER_BOUND ( 'NONE', #106688, .T. ) ;
#53823 = CARTESIAN_POINT ( 'NONE',  ( 33.18398860626899705, 28.73617430169810305, 5.000000000000000000 ) ) ;
#53824 = VERTEX_POINT ( 'NONE', #142708 ) ;
#53825 = DIRECTION ( 'NONE',  ( 0.7071067811865487940, 0.7071067811865463515, -0.000000000000000000 ) ) ;
#53826 = VECTOR ( 'NONE', #112448, 1000.000000000000000 ) ;
#53827 = DIRECTION ( 'NONE',  ( -0.7071067811865486830, -0.7071067811865464625, 0.000000000000000000 ) ) ;
#53828 = CARTESIAN_POINT ( 'NONE',  ( 18.29623647476855197, 7.934999999999990727, -1.457635852685135314E-15 ) ) ;
#53829 = EDGE_CURVE ( 'NONE', #115943, #51894, #78178, .T. ) ;
#53830 = CARTESIAN_POINT ( 'NONE',  ( -11.99999999999992006, -10.77435723561696435, -9.972017380717201007 ) ) ;
#53831 = VERTEX_POINT ( 'NONE', #100643 ) ;
#53832 = CARTESIAN_POINT ( 'NONE',  ( 119.9329301918981230, 1.637169565754156730, 6.110000000000001208 ) ) ;
#53833 = EDGE_CURVE ( 'NONE', #73333, #128893, #89061, .T. ) ;
#53834 = CARTESIAN_POINT ( 'NONE',  ( -21.48921356237309155, -27.52281430457070499, 5.000000000000000000 ) ) ;
#53835 = VECTOR ( 'NONE', #31466, 999.9999999999998863 ) ;
#53836 = FACE_OUTER_BOUND ( 'NONE', #21774, .T. ) ;
#53838 = VERTEX_POINT ( 'NONE', #98484 ) ;
#53837 = DIRECTION ( 'NONE',  ( -0.6830127018922180770, -0.6830127018922204085, -0.2588190451025213501 ) ) ;
#53840 = MECHANICAL_DESIGN_GEOMETRIC_PRESENTATION_REPRESENTATION (  '', ( #2786 ), #86326 ) ;
#53839 = LINE ( 'NONE', #98042, #120259 ) ;
#53841 = ORIENTED_EDGE ( 'NONE', *, *, #740, .F. ) ;
#53842 = CARTESIAN_POINT ( 'NONE',  ( -17.81601139373099940, 28.73617430169775133, 5.000000000000000000 ) ) ;
#53843 = DIRECTION ( 'NONE',  ( -0.6830127018922181881, 0.6830127018922202975, -0.2588190451025214056 ) ) ;
#53844 = ADVANCED_FACE ( 'NONE', ( #88342 ), #99914, .F. ) ;
#53845 = EDGE_CURVE ( 'NONE', #28815, #122724, #122355, .T. ) ;
#53846 = CARTESIAN_POINT ( 'NONE',  ( -31.06996025486389712, -0.7407075233842735917, 13.87443053587618458 ) ) ;
#53848 = EDGE_LOOP ( 'NONE', ( #22871, #141548, #88049, #49243 ) ) ;
#53847 =( BOUNDED_CURVE ( )  B_SPLINE_CURVE ( 3, ( #124384, #36649, #137412, #2578 ),
 .UNSPECIFIED., .F., .F. ) 
 B_SPLINE_CURVE_WITH_KNOTS ( ( 4, 4 ),
 ( 1.975938068165228767, 2.025325302527091420 ),
 .UNSPECIFIED. ) 
 CURVE ( )  GEOMETRIC_REPRESENTATION_ITEM ( )  RATIONAL_B_SPLINE_CURVE ( ( 1.000000000000000000, 0.9997967520851089862, 0.9997967520851089862, 1.000000000000000000 ) ) 
 REPRESENTATION_ITEM ( '' )  );
#53849 = DIRECTION ( 'NONE',  ( -1.000000000000000000, -0.000000000000000000, -0.000000000000000000 ) ) ;
#53850 = LINE ( 'NONE', #42972, #53751 ) ;
#53851 = ORIENTED_EDGE ( 'NONE', *, *, #71808, .T. ) ;
#53852 = VECTOR ( 'NONE', #76390, 1000.000000000000000 ) ;
#53853 = PLANE ( 'NONE',  #99496 ) ;
#53854 =( BOUNDED_CURVE ( )  B_SPLINE_CURVE ( 3, ( #103770, #60326, #48717, #71923 ),
 .UNSPECIFIED., .F., .T. ) 
 B_SPLINE_CURVE_WITH_KNOTS ( ( 4, 4 ),
 ( 5.043186909253412509, 5.074607125596364732 ),
 .UNSPECIFIED. ) 
 CURVE ( )  GEOMETRIC_REPRESENTATION_ITEM ( )  RATIONAL_B_SPLINE_CURVE ( ( 1.000000000000000000, 0.9999177325257868620, 0.9999177325257868620, 1.000000000000000000 ) ) 
 REPRESENTATION_ITEM ( '' )  );
#53855 = CARTESIAN_POINT ( 'NONE',  ( -29.67183060077625711, 2.259292476615694323, 4.000000000000000000 ) ) ;
#53856 = ORIENTED_EDGE ( 'NONE', *, *, #15251, .F. ) ;
#53857 = CARTESIAN_POINT ( 'NONE',  ( -9.489213562373095101, -27.52281430457062328, 5.000000000000000000 ) ) ;
#53858 = EDGE_CURVE ( 'NONE', #37853, #27739, #120942, .T. ) ;
#53859 = CARTESIAN_POINT ( 'NONE',  ( -13.43359823057990354, 1.153863645259229909, 4.000000000000000000 ) ) ;
#53860 = VERTEX_POINT ( 'NONE', #21646 ) ;
#53861 = EDGE_CURVE ( 'NONE', #13100, #67034, #89748, .T. ) ;
#53862 = ORIENTED_EDGE ( 'NONE', *, *, #107279, .F. ) ;
#53863 = AXIS2_PLACEMENT_3D ( 'NONE', #107367, #17498, #6581 ) ;
#53864 = LINE ( 'NONE', #7450, #72786 ) ;
#53865 = CARTESIAN_POINT ( 'NONE',  ( 34.92499999999998295, 18.66246187583882588, 4.000000000000000000 ) ) ;
#53866 = EDGE_CURVE ( 'NONE', #13798, #127597, #20181, .T. ) ;
#53867 = CARTESIAN_POINT ( 'NONE',  ( -23.20710678118638626, -11.24070752338416312, 5.000000000000000000 ) ) ;
#53868 = LINE ( 'NONE', #119089, #32264 ) ;
#53869 = DIRECTION ( 'NONE',  ( -0.7071067811865486830, -0.7071067811865464625, 0.000000000000000000 ) ) ;
#53870 = ORIENTED_EDGE ( 'NONE', *, *, #119442, .F. ) ;
#53871 = CARTESIAN_POINT ( 'NONE',  ( -12.45006917115538947, -22.22500000000000142, 13.51659144808220425 ) ) ;
#53872 = CARTESIAN_POINT ( 'NONE',  ( -37.25154412867552622, -11.24070752338416490, 10.39518518046017981 ) ) ;
#53873 = CARTESIAN_POINT ( 'NONE',  ( -2.700255128608413990, -27.71228299555204089, 4.000000000000000000 ) ) ;
#53875 = EDGE_CURVE ( 'NONE', #25399, #96412, #110055, .T. ) ;
#53874 = AXIS2_PLACEMENT_3D ( 'NONE', #9978, #31046, #65844 ) ;
#53876 = VECTOR ( 'NONE', #20462, 1000.000000000000000 ) ;
#53877 = VECTOR ( 'NONE', #16446, 1000.000000000000000 ) ;
#53878 = CARTESIAN_POINT ( 'NONE',  ( 33.18398860626899705, 28.73617430169810305, 5.000000000000000000 ) ) ;
#53879 = CARTESIAN_POINT ( 'NONE',  ( 37.82876352523144448, 0.000000000000000000, -6.109999999999999432 ) ) ;
#53880 = CARTESIAN_POINT ( 'NONE',  ( 31.88982677111766506, -22.22500000000000142, 4.785647885939354751 ) ) ;
#53881 = VECTOR ( 'NONE', #43831, 1000.000000000000000 ) ;
#53882 = VECTOR ( 'NONE', #15221, 1000.000000000000000 ) ;
#53883 = ORIENTED_EDGE ( 'NONE', *, *, #94515, .T. ) ;
#53884 = ORIENTED_EDGE ( 'NONE', *, *, #42105, .T. ) ;
#53885 = CARTESIAN_POINT ( 'NONE',  ( 3.792893218813436551, -8.240707523384196875, 5.000000000000000000 ) ) ;
#53886 = VERTEX_POINT ( 'NONE', #77479 ) ;
#53887 = ORIENTED_EDGE ( 'NONE', *, *, #110063, .F. ) ;
#53888 = AXIS2_PLACEMENT_3D ( 'NONE', #107381, #141447, #42156 ) ;
#53889 = EDGE_CURVE ( 'NONE', #38971, #133114, #95683, .T. ) ;
#53890 = VECTOR ( 'NONE', #116091, 1000.000000000000000 ) ;
#53891 = DIRECTION ( 'NONE',  ( 1.000000000000000000, 0.000000000000000000, 0.000000000000000000 ) ) ;
#53892 = CARTESIAN_POINT ( 'NONE',  ( 32.28242261357411280, -21.73023691814492508, 5.000000000000000888 ) ) ;
#53893 = ORIENTED_EDGE ( 'NONE', *, *, #13336, .T. ) ;
#53894 = CARTESIAN_POINT ( 'NONE',  ( -25.49999999999982236, -16.91253812416058366, 4.000000000000000000 ) ) ;
#53895 = DIRECTION ( 'NONE',  ( 0.7071067811865487940, 0.7071067811865463515, -0.000000000000000000 ) ) ;
#53896 = DIRECTION ( 'NONE',  ( 0.000000000000000000, -1.000000000000000000, 0.000000000000000000 ) ) ;
#53897 = LINE ( 'NONE', #74198, #34923 ) ;
#53898 = CARTESIAN_POINT ( 'NONE',  ( 131.7497271886881549, -49.14999999999999147, 40.57187971032495000 ) ) ;
#53899 = ORIENTED_EDGE ( 'NONE', *, *, #62336, .T. ) ;
#53900 = EDGE_CURVE ( 'NONE', #119311, #19621, #58296, .T. ) ;
#53901 = CARTESIAN_POINT ( 'NONE',  ( 20.99065804761471199, -2.500000000000000444, 3.061616997868384127E-16 ) ) ;
#53902 = CARTESIAN_POINT ( 'NONE',  ( -6.989119713460464567, -22.02621442084248216, 4.990779571109223767 ) ) ;
#53903 = ADVANCED_FACE ( 'NONE', ( #25193 ), #115033, .F. ) ;
#53904 = DIRECTION ( 'NONE',  ( -0.000000000000000000, 0.3543493200069153248, 0.9351131265310292928 ) ) ;
#53905 = DIRECTION ( 'NONE',  ( 0.7071067811865487940, 0.7071067811865463515, 0.000000000000000000 ) ) ;
#53906 = CARTESIAN_POINT ( 'NONE',  ( 29.99999999999980105, -16.44781430457066662, 5.000000000000000000 ) ) ;
#53907 = FACE_OUTER_BOUND ( 'NONE', #85596, .T. ) ;
#53908 = DIRECTION ( 'NONE',  ( -0.7071067811865486830, -0.7071067811865464625, 0.000000000000000000 ) ) ;
#53909 = CARTESIAN_POINT ( 'NONE',  ( 55.93336038379622011, 2.130196079827431532, -7.949999999999997513 ) ) ;
#53910 = EDGE_CURVE ( 'NONE', #88704, #116329, #3430, .T. ) ;
#53912 = FACE_OUTER_BOUND ( 'NONE', #143018, .T. ) ;
#53911 = VECTOR ( 'NONE', #51174, 1000.000000000000000 ) ;
#53913 = VERTEX_POINT ( 'NONE', #102058 ) ;
#53914 = ORIENTED_EDGE ( 'NONE', *, *, #127986, .F. ) ;
#53915 = CARTESIAN_POINT ( 'NONE',  ( 59.18749999999997868, -5.819803920172573086, 5.819803920172572198 ) ) ;
#53916 = CARTESIAN_POINT ( 'NONE',  ( 21.71238017851529989, 8.518175273744143183, 4.330735335516821216 ) ) ;
#53917 = CARTESIAN_POINT ( 'NONE',  ( 14.20710678118645376, -2.240707523384257716, 5.000000000000000000 ) ) ;
#53918 = DIRECTION ( 'NONE',  ( -0.6830127018922180770, -0.6830127018922204085, -0.2588190451025213501 ) ) ;
#53919 = VERTEX_POINT ( 'NONE', #46288 ) ;
#53920 = CARTESIAN_POINT ( 'NONE',  ( -75.48921356237309510, -27.52281430457107803, 5.000000000000000000 ) ) ;
#53921 = AXIS2_PLACEMENT_3D ( 'NONE', #50057, #94249, #138489 ) ;
#53922 = CARTESIAN_POINT ( 'NONE',  ( 72.18398860626899705, 28.73617430169837661, 5.000000000000000000 ) ) ;
#53923 = CARTESIAN_POINT ( 'NONE',  ( 48.70876352523144703, -7.482591942790329030E-16, 6.110000000000001208 ) ) ;
#53924 = VECTOR ( 'NONE', #69920, 1000.000000000000000 ) ;
#53925 = ORIENTED_EDGE ( 'NONE', *, *, #10418, .F. ) ;
#53926 = ORIENTED_EDGE ( 'NONE', *, *, #5682, .T. ) ;
#53927 = ORIENTED_EDGE ( 'NONE', *, *, #40918, .F. ) ;
#53928 = AXIS2_PLACEMENT_3D ( 'NONE', #8213, #6769, #95251 ) ;
#53929 = AXIS2_PLACEMENT_3D ( 'NONE', #115721, #36089, #93301 ) ;
#53930 = DIRECTION ( 'NONE',  ( -0.7071067811865486830, 0.7071067811865464625, 0.000000000000000000 ) ) ;
#53931 = CARTESIAN_POINT ( 'NONE',  ( 4.499999999999979572, 6.052185695429108669, 5.000000000000000000 ) ) ;
#53932 = CARTESIAN_POINT ( 'NONE',  ( 78.29974487139158157, -27.71228299555260577, 4.000000000000000000 ) ) ;
#53933 = LINE ( 'NONE', #98126, #76480 ) ;
#53934 = ORIENTED_EDGE ( 'NONE', *, *, #50225, .F. ) ;
#53935 = DIRECTION ( 'NONE',  ( 0.6830127018922181881, 0.6830127018922202975, -0.2588190451025214056 ) ) ;
#53937 = ORIENTED_EDGE ( 'NONE', *, *, #142724, .T. ) ;
#53936 = FACE_OUTER_BOUND ( 'NONE', #24365, .T. ) ;
#53938 = CARTESIAN_POINT ( 'NONE',  ( 84.00043019189810423, -3.055000000000002380, 5.291415217122920289 ) ) ;
#53939 = LINE ( 'NONE', #76388, #67061 ) ;
#53940 = DIRECTION ( 'NONE',  ( -0.000000000000000000, -0.3543493200069152693, 0.9351131265310292928 ) ) ;
#53941 = CARTESIAN_POINT ( 'NONE',  ( 19.21071296386495675, 9.141836041257182188, 4.000000000000000000 ) ) ;
#53942 = DIRECTION ( 'NONE',  ( -0.7071067811865487940, 0.7071067811865463515, -0.000000000000000000 ) ) ;
#53943 = CARTESIAN_POINT ( 'NONE',  ( 0.000000000000000000, 0.000000000000000000, 5.000000000000000000 ) ) ;
#53944 = VECTOR ( 'NONE', #121051, 1000.000000000000000 ) ;
#53945 = ORIENTED_EDGE ( 'NONE', *, *, #75869, .T. ) ;
#53946 =( NAMED_UNIT ( * ) SI_UNIT ( $, .STERADIAN. ) SOLID_ANGLE_UNIT ( ) );
#53947 = CARTESIAN_POINT ( 'NONE',  ( 63.49543019189811588, 5.291415217122916737, 3.055000000000001936 ) ) ;
#53948 = CARTESIAN_POINT ( 'NONE',  ( 36.18398860626899705, 28.73617430169812437, 5.000000000000000000 ) ) ;
#53949 = EDGE_CURVE ( 'NONE', #100985, #46950, #35414, .T. ) ;
#53950 = PLANE ( 'NONE',  #12996 ) ;
#53951 = ORIENTED_EDGE ( 'NONE', *, *, #30948, .T. ) ;
#53952 = ORIENTED_EDGE ( 'NONE', *, *, #53998, .F. ) ;
#53953 = CIRCLE ( 'NONE', #9924, 0.5000000000000004441 ) ;
#53954 = DIRECTION ( 'NONE',  ( -1.000000000000000000, -0.000000000000000000, -0.000000000000000000 ) ) ;
#53955 = DIRECTION ( 'NONE',  ( -0.7071067811865486830, -0.7071067811865464625, -0.000000000000000000 ) ) ;
#53956 = ORIENTED_EDGE ( 'NONE', *, *, #87489, .F. ) ;
#53957 = VERTEX_POINT ( 'NONE', #90472 ) ;
#53958 = LINE ( 'NONE', #120575, #76903 ) ;
#53959 = ORIENTED_EDGE ( 'NONE', *, *, #103380, .T. ) ;
#53960 = FACE_OUTER_BOUND ( 'NONE', #111330, .T. ) ;
#53961 = DIRECTION ( 'NONE',  ( 0.7071067811865487940, -0.7071067811865463515, 0.000000000000000000 ) ) ;
#53962 = VECTOR ( 'NONE', #136108, 1000.000000000000000 ) ;
#53963 = CARTESIAN_POINT ( 'NONE',  ( 0.000000000000000000, -7.600000000000055600, -31.92499999999998650 ) ) ;
#53964 = EDGE_CURVE ( 'NONE', #19920, #45152, #59305, .T. ) ;
#53965 = FACE_BOUND ( 'NONE', #40978, .T. ) ;
#53966 = PLANE ( 'NONE',  #34009 ) ;
#53967 = FACE_OUTER_BOUND ( 'NONE', #68921, .T. ) ;
#53968 = ADVANCED_FACE ( 'NONE', ( #124526 ), #26636, .F. ) ;
#53969 = CIRCLE ( 'NONE', #79453, 25.00000000000002842 ) ;
#53970 = CARTESIAN_POINT ( 'NONE',  ( 12.03892749862900402, -2.055000000000000160, 0.000000000000000000 ) ) ;
#53972 = ORIENTED_EDGE ( 'NONE', *, *, #17388, .F. ) ;
#53971 = PLANE ( 'NONE',  #136140 ) ;
#53973 = CONTEXT_DEPENDENT_SHAPE_REPRESENTATION ( #77294, #37670 ) ;
#53974 = ORIENTED_EDGE ( 'NONE', *, *, #125199, .F. ) ;
#53975 = ORIENTED_EDGE ( 'NONE', *, *, #88898, .F. ) ;
#53976 = CARTESIAN_POINT ( 'NONE',  ( 85.37043019189812298, -3.055000000000001492, 5.291415217122917625 ) ) ;
#53977 = ORIENTED_EDGE ( 'NONE', *, *, #67997, .T. ) ;
#53978 = EDGE_CURVE ( 'NONE', #130020, #55512, #123487, .T. ) ;
#53979 = DIRECTION ( 'NONE',  ( 0.6830127018922180770, -0.6830127018922204085, -0.2588190451025213501 ) ) ;
#53980 = ORIENTED_EDGE ( 'NONE', *, *, #14020, .F. ) ;
#53981 = CARTESIAN_POINT ( 'NONE',  ( 28.63753812416078048, 22.22499999999999432, 4.000000000000000000 ) ) ;
#53982 = VECTOR ( 'NONE', #68157, 1000.000000000000000 ) ;
#53983 = AXIS2_PLACEMENT_3D ( 'NONE', #72602, #116756, #39952 ) ;
#53984 = EDGE_CURVE ( 'NONE', #48060, #95984, #125962, .T. ) ;
#53985 = AXIS2_PLACEMENT_3D ( 'NONE', #100329, #90148, #57554 ) ;
#53986 = CARTESIAN_POINT ( 'NONE',  ( 30.08314806772912320, 21.75929247661549581, 7.311836541448121451 ) ) ;
#53987 = CARTESIAN_POINT ( 'NONE',  ( 20.66989781452722141, 17.25929247661553845, 19.83885114516066750 ) ) ;
#53988 = DIRECTION ( 'NONE',  ( -0.7071067811865487940, 0.7071067811865463515, -0.000000000000000000 ) ) ;
#53989 = CARTESIAN_POINT ( 'NONE',  ( 6.852250093007166143, 2.500000000000000444, 0.000000000000000000 ) ) ;
#53990 = LINE ( 'NONE', #141694, #112089 ) ;
#53991 = LINE ( 'NONE', #54690, #95544 ) ;
#53992 = FACE_OUTER_BOUND ( 'NONE', #76653, .T. ) ;
#53993 = ORIENTED_EDGE ( 'NONE', *, *, #29549, .T. ) ;
#53994 = AXIS2_PLACEMENT_3D ( 'NONE', #80053, #103871, #125670 ) ;
#53995 = AXIS2_PLACEMENT_3D ( 'NONE', #23619, #67892, #91728 ) ;
#53996 = EDGE_CURVE ( 'NONE', #46307, #120604, #78906, .T. ) ;
#53997 = SURFACE_STYLE_USAGE ( .BOTH. , #119205 ) ;
#53998 = EDGE_CURVE ( 'NONE', #59677, #27437, #136820, .T. ) ;
#53999 = ORIENTED_EDGE ( 'NONE', *, *, #82807, .T. ) ;
#54000 = CARTESIAN_POINT ( 'NONE',  ( 7.139999999999956160, -60.26999999999998892, -8.278119684037271497 ) ) ;
#54001 = DIRECTION ( 'NONE',  ( 0.000000000000000000, -0.3543493200069153248, 0.9351131265310292928 ) ) ;
#54002 = ORIENTED_EDGE ( 'NONE', *, *, #34020, .T. ) ;
#54003 = ORIENTED_EDGE ( 'NONE', *, *, #138817, .T. ) ;
#54004 = CARTESIAN_POINT ( 'NONE',  ( 33.97959685856477563, 6.109999999999999432, 1.637169565754164280 ) ) ;
#54005 = VERTEX_POINT ( 'NONE', #47028 ) ;
#54006 = CARTESIAN_POINT ( 'NONE',  ( 32.50183651486023706, -17.24070752338409918, 8.407044977365149663 ) ) ;
#54007 = LINE ( 'NONE', #111186, #107138 ) ;
#54008 = CIRCLE ( 'NONE', #135049, 3.000000000000000000 ) ;
#54009 = CARTESIAN_POINT ( 'NONE',  ( 29.06663961620377279, 1.633150327867695095, 6.094999999999988205 ) ) ;
#54010 = CARTESIAN_POINT ( 'NONE',  ( -7.412718841549110316, 12.49264501416213946, -25.30319893193128777 ) ) ;
#54011 = ORIENTED_EDGE ( 'NONE', *, *, #54253, .T. ) ;
#54012 = EDGE_CURVE ( 'NONE', #72227, #11858, #9517, .T. ) ;
#54013 = ORIENTED_EDGE ( 'NONE', *, *, #104200, .T. ) ;
#54014 = SURFACE_STYLE_USAGE ( .BOTH. , #31522 ) ;
#54015 = CARTESIAN_POINT ( 'NONE',  ( -39.48921356237310221, -27.52281430457082934, 5.000000000000000000 ) ) ;
#54017 = EDGE_LOOP ( 'NONE', ( #69020, #64772, #126262, #133854 ) ) ;
#54016 = LINE ( 'NONE', #10458, #51728 ) ;
#54018 = VERTEX_POINT ( 'NONE', #15028 ) ;
#54019 = LINE ( 'NONE', #130862, #12504 ) ;
#54020 = LINE ( 'NONE', #43128, #95447 ) ;
#54021 = AXIS2_PLACEMENT_3D ( 'NONE', #142605, #120822, #43291 ) ;
#54022 = EDGE_CURVE ( 'NONE', #42968, #93122, #69451, .T. ) ;
#54023 = EDGE_CURVE ( 'NONE', #57857, #124559, #92584, .T. ) ;
#54024 = DIRECTION ( 'NONE',  ( -0.6830127018922180770, -0.6830127018922204085, -0.2588190451025213501 ) ) ;
#54025 = EDGE_LOOP ( 'NONE', ( #36240, #45863, #29602 ) ) ;
#54026 = DIRECTION ( 'NONE',  ( -1.000000000000000000, -1.224606353822377258E-16, -0.000000000000000000 ) ) ;
#54027 = VERTEX_POINT ( 'NONE', #14328 ) ;
#54028 = PRODUCT ( '1.3 Jaw Plate', '1.3 Jaw Plate', '', ( #15554 ) ) ;
#54029 = ORIENTED_EDGE ( 'NONE', *, *, #118122, .F. ) ;
#54030 = AXIS2_PLACEMENT_3D ( 'NONE', #40126, #84341, #94455 ) ;
#54031 = VERTEX_POINT ( 'NONE', #103461 ) ;
#54032 = DIRECTION ( 'NONE',  ( -1.000000000000000000, -1.224606353822377258E-16, -0.000000000000000000 ) ) ;
#54033 = LINE ( 'NONE', #32249, #32456 ) ;
#54034 = DIRECTION ( 'NONE',  ( -0.7071067811865486830, -0.7071067811865464625, -0.000000000000000000 ) ) ;
#54035 = EDGE_CURVE ( 'NONE', #29880, #71067, #123834, .T. ) ;
#54036 = DIRECTION ( 'NONE',  ( 0.000000000000000000, -1.000000000000000000, 0.000000000000000000 ) ) ;
#54038 = VECTOR ( 'NONE', #37250, 1000.000000000000000 ) ;
#54037 = CARTESIAN_POINT ( 'NONE',  ( 12.03892749862900402, -2.055000000000000160, 2.789133085058097101E-16 ) ) ;
#54039 = CARTESIAN_POINT ( 'NONE',  ( 8.700255128608413102, -27.71228299555199825, 4.000000000000000000 ) ) ;
#54040 = ADVANCED_FACE ( 'NONE', ( #57165 ), #135428, .F. ) ;
#54041 = DIRECTION ( 'NONE',  ( -0.7071067811865486830, 0.7071067811865464625, 0.000000000000000000 ) ) ;
#54042 = ORIENTED_EDGE ( 'NONE', *, *, #18884, .F. ) ;
#54043 = EDGE_CURVE ( 'NONE', #31547, #92519, #25928, .T. ) ;
#54044 = CARTESIAN_POINT ( 'NONE',  ( 97.78752705046289861, 0.000000000000000000, -7.949999999999998401 ) ) ;
#54045 = ORIENTED_EDGE ( 'NONE', *, *, #95666, .F. ) ;
#54046 = DIRECTION ( 'NONE',  ( -0.3543493200069162685, -0.000000000000000000, -0.9351131265310288487 ) ) ;
#54047 =( BOUNDED_CURVE ( )  B_SPLINE_CURVE ( 3, ( #121417, #122125, #67808, #101813 ),
 .UNSPECIFIED., .F., .T. ) 
 B_SPLINE_CURVE_WITH_KNOTS ( ( 4, 4 ),
 ( 1.864375635226937389, 1.933014472006547635 ),
 .UNSPECIFIED. ) 
 CURVE ( )  GEOMETRIC_REPRESENTATION_ITEM ( )  RATIONAL_B_SPLINE_CURVE ( ( 1.000000000000000000, 0.9996074310407765395, 0.9996074310407765395, 1.000000000000000000 ) ) 
 REPRESENTATION_ITEM ( '' )  );
#54048 = AXIS2_PLACEMENT_3D ( 'NONE', #122213, #113480, #67150 ) ;
#54049 = DIRECTION ( 'NONE',  ( -0.7071067811865486830, 0.7071067811865464625, 0.000000000000000000 ) ) ;
#54051 = ORIENTED_EDGE ( 'NONE', *, *, #16288, .T. ) ;
#54050 = VECTOR ( 'NONE', #107661, 1000.000000000000227 ) ;
#54052 = FACE_OUTER_BOUND ( 'NONE', #30006, .T. ) ;
#54053 = DIRECTION ( 'NONE',  ( -0.000000000000000000, 0.000000000000000000, 1.000000000000000000 ) ) ;
#54054 = ADVANCED_FACE ( 'NONE', ( #80336 ), #138257, .F. ) ;
#54055 = FILL_AREA_STYLE ('',( #128716 ) ) ;
#54056 = EDGE_LOOP ( 'NONE', ( #119334, #142786, #109330, #14121 ) ) ;
#54057 = EDGE_LOOP ( 'NONE', ( #6625, #81416, #35237, #10949 ) ) ;
#54058 = CARTESIAN_POINT ( 'NONE',  ( -8.994519915287490619, 28.92564299267944250, 4.000000000000000000 ) ) ;
#54059 = LINE ( 'NONE', #121403, #141417 ) ;
#54060 = LINE ( 'NONE', #128723, #102537 ) ;
#54061 = CIRCLE ( 'NONE', #26298, 4.999999999999998224 ) ;
#54062 = EDGE_CURVE ( 'NONE', #114666, #105677, #105594, .T. ) ;
#54063 = LINE ( 'NONE', #11924, #138490 ) ;
#54064 = CARTESIAN_POINT ( 'NONE',  ( 69.91209685856478018, 5.291415217122922066, -3.054999999999995275 ) ) ;
#54065 = DIRECTION ( 'NONE',  ( 0.000000000000000000, 1.000000000000000000, -0.000000000000000000 ) ) ;
#54066 = CARTESIAN_POINT ( 'NONE',  ( 26.99999999999981526, -0.2811185226894025169, -5.995736974527575924 ) ) ;
#54067 = FACE_OUTER_BOUND ( 'NONE', #55760, .T. ) ;
#54068 = CARTESIAN_POINT ( 'NONE',  ( 84.85416666666667140, -2.130196079827463507, -7.949999999999979750 ) ) ;
#54069 = EDGE_LOOP ( 'NONE', ( #78544, #90509, #105367, #89212 ) ) ;
#54070 = DIRECTION ( 'NONE',  ( 0.7071067811865487940, 0.7071067811865463515, 0.000000000000000000 ) ) ;
#54071 = VERTEX_POINT ( 'NONE', #51258 ) ;
#54072 =( GEOMETRIC_REPRESENTATION_CONTEXT ( 3 ) GLOBAL_UNCERTAINTY_ASSIGNED_CONTEXT ( ( #80812 ) ) GLOBAL_UNIT_ASSIGNED_CONTEXT ( ( #12780, #57057, #103356 ) ) REPRESENTATION_CONTEXT ( 'NONE', 'WORKASPACE' ) );
#54073 = FACE_OUTER_BOUND ( 'NONE', #20558, .T. ) ;
#54074 = DIRECTION ( 'NONE',  ( -0.000000000000000000, -0.3543493200069152693, 0.9351131265310292928 ) ) ;
#54075 = ORIENTED_EDGE ( 'NONE', *, *, #79207, .T. ) ;
#54076 = DIRECTION ( 'NONE',  ( 0.000000000000000000, -1.000000000000000000, 0.000000000000000000 ) ) ;
#54078 = ORIENTED_EDGE ( 'NONE', *, *, #102272, .F. ) ;
#54077 = CARTESIAN_POINT ( 'NONE',  ( 8.999999999999944933, -4.447814304570779420, 5.000000000000000000 ) ) ;
#54079 = CARTESIAN_POINT ( 'NONE',  ( 107.6041666666666714, 2.130196079827441746, 7.949999999999992184 ) ) ;
#54080 = CARTESIAN_POINT ( 'NONE',  ( -34.92500000000001137, 22.22500000000000142, 4.000000000000000000 ) ) ;
#54081 = DIRECTION ( 'NONE',  ( -0.7071067811865486830, -0.7071067811865464625, -0.000000000000000000 ) ) ;
#54082 = ORIENTED_EDGE ( 'NONE', *, *, #28185, .F. ) ;
#54084 = VERTEX_POINT ( 'NONE', #38942 ) ;
#54083 = COLOUR_RGB ( '', 0.09019608, 0.27058824, 0.51372549) ;
#54085 = DIRECTION ( 'NONE',  ( 0.3543493200069162685, -0.000000000000000000, -0.9351131265310288487 ) ) ;
#54086 = CARTESIAN_POINT ( 'NONE',  ( 24.39999999999999858, -5.520864266206504263E-14, 33.92499999999998295 ) ) ;
#54087 = EDGE_CURVE ( 'NONE', #95860, #12218, #72332, .T. ) ;
#54088 = DIRECTION ( 'NONE',  ( -0.000000000000000000, 0.3543493200069153248, 0.9351131265310292928 ) ) ;
#54090 = ADVANCED_FACE ( 'NONE', ( #29473 ), #7717, .F. ) ;
#54089 = CARTESIAN_POINT ( 'NONE',  ( -0.7228143045705931469, -21.72500000000000142, 5.000000000000000000 ) ) ;
#54091 = CARTESIAN_POINT ( 'NONE',  ( 84.37086038379624142, 6.884901960086289741, -3.974999999999993427 ) ) ;
#54093 = EDGE_CURVE ( 'NONE', #75982, #9218, #39195, .T. ) ;
#54092 = PLANE ( 'NONE',  #125069 ) ;
#54094 = VECTOR ( 'NONE', #11314, 1000.000000000000227 ) ;
#54095 = LINE ( 'NONE', #43193, #113181 ) ;
#54096 = ORIENTED_EDGE ( 'NONE', *, *, #35124, .T. ) ;
#54097 = CARTESIAN_POINT ( 'NONE',  ( 87.33333333333332860, -6.884901960086287964, 3.974999999999998312 ) ) ;
#54098 = DIRECTION ( 'NONE',  ( 0.7071067811865487940, 0.7071067811865463515, 0.000000000000000000 ) ) ;
#54099 = DIRECTION ( 'NONE',  ( -0.7071067811865486830, 0.7071067811865464625, 0.000000000000000000 ) ) ;
#54100 = CARTESIAN_POINT ( 'NONE',  ( 32.52083333333333570, -6.094999999999989981, -1.633150327867689100 ) ) ;
#54101 = ORIENTED_EDGE ( 'NONE', *, *, #70704, .F. ) ;
#54102 = EDGE_CURVE ( 'NONE', #19820, #42524, #18578, .T. ) ;
#54103 = VECTOR ( 'NONE', #120250, 1000.000000000000227 ) ;
#54104 = FACE_OUTER_BOUND ( 'NONE', #71088, .T. ) ;
#54105 = ORIENTED_EDGE ( 'NONE', *, *, #29621, .T. ) ;
#54106 = CARTESIAN_POINT ( 'NONE',  ( 71.75043019189811844, 3.055000000000002824, -5.291415217122919401 ) ) ;
#54108 = CARTESIAN_POINT ( 'NONE',  ( -29.95341186370437825, 14.25929247661557042, 18.84478104361334871 ) ) ;
#54107 = VECTOR ( 'NONE', #89752, 999.9999999999998863 ) ;
#54109 = EDGE_CURVE ( 'NONE', #12173, #103754, #104666, .T. ) ;
#54110 = VERTEX_POINT ( 'NONE', #40393 ) ;
#54111 = CARTESIAN_POINT ( 'NONE',  ( 15.75860074219783513, 21.72499999999999432, 5.000000000000000000 ) ) ;
#54112 = CARTESIAN_POINT ( 'NONE',  ( 8.510786437626906675, -27.52281430457049183, 5.000000000000000000 ) ) ;
#54113 = CARTESIAN_POINT ( 'NONE',  ( 9.046588136295392601, 14.25929247661557042, 18.84478104361325634 ) ) ;
#54114 = CARTESIAN_POINT ( 'NONE',  ( 11.29289321881338104, -9.740707523384184441, 5.000000000000000000 ) ) ;
#54116 = ORIENTED_EDGE ( 'NONE', *, *, #46548, .T. ) ;
#54115 = LINE ( 'NONE', #33082, #8193 ) ;
#54117 = CARTESIAN_POINT ( 'NONE',  ( 128.6786164994711612, -49.14501756083436135, -40.36361034346619903 ) ) ;
#54118 = LINE ( 'NONE', #107018, #33749 ) ;
#54119 = FACE_OUTER_BOUND ( 'NONE', #72053, .T. ) ;
#54120 = CIRCLE ( 'NONE', #135139, 3.378199999999994319 ) ;
#54121 = CARTESIAN_POINT ( 'NONE',  ( -12.70710678118645909, 11.25929247661560773, 5.000000000000000000 ) ) ;
#54122 = ORIENTED_EDGE ( 'NONE', *, *, #61176, .T. ) ;
#54123 = ORIENTED_EDGE ( 'NONE', *, *, #101258, .T. ) ;
#54124 = CARTESIAN_POINT ( 'NONE',  ( 60.66709685856477563, -3.055000000000000160, -5.291415217122921177 ) ) ;
#54125 = VECTOR ( 'NONE', #99291, 1000.000000000000227 ) ;
#54126 = ORIENTED_EDGE ( 'NONE', *, *, #36818, .T. ) ;
#54127 = CARTESIAN_POINT ( 'NONE',  ( 15.18398860626900237, 28.73617430169797871, 5.000000000000000000 ) ) ;
#54128 = CARTESIAN_POINT ( 'NONE',  ( 2.816011393730999401, 28.73617430169785436, 5.000000000000000000 ) ) ;
#54129 = EDGE_CURVE ( 'NONE', #117239, #58140, #96148, .T. ) ;
#54130 = EDGE_CURVE ( 'NONE', #62418, #59656, #17864, .T. ) ;
#54131 = CARTESIAN_POINT ( 'NONE',  ( -69.18398860626899705, 28.73617430169835529, 5.000000000000000000 ) ) ;
#54132 = LINE ( 'NONE', #97581, #20024 ) ;
#54133 = EDGE_LOOP ( 'NONE', ( #121548, #104422, #121667, #73401 ) ) ;
#54134 = VERTEX_POINT ( 'NONE', #118632 ) ;
#54135 = DIRECTION ( 'NONE',  ( -0.7071067811865486830, -0.7071067811865464625, -0.000000000000000000 ) ) ;
#54136 = CIRCLE ( 'NONE', #128198, 2.500000000000000888 ) ;
#54137 = ORIENTED_EDGE ( 'NONE', *, *, #34327, .T. ) ;
#54138 = CIRCLE ( 'NONE', #35718, 2.500000000000000888 ) ;
#54139 = DIRECTION ( 'NONE',  ( 0.7071067811865487940, 0.7071067811865463515, 0.000000000000000000 ) ) ;
#54140 = CARTESIAN_POINT ( 'NONE',  ( -7.889826771117836479, -22.22499999999999787, 4.785647885939353863 ) ) ;
#54141 = ORIENTED_EDGE ( 'NONE', *, *, #23950, .F. ) ;
#54142 = VECTOR ( 'NONE', #50994, 1000.000000000000000 ) ;
#54143 = EDGE_CURVE ( 'NONE', #107847, #73688, #94716, .T. ) ;
#54144 = EDGE_CURVE ( 'NONE', #70620, #60930, #6971, .T. ) ;
#54145 = ADVANCED_FACE ( 'NONE', ( #28793 ), #62857, .T. ) ;
#54146 = FACE_BOUND ( 'NONE', #102817, .T. ) ;
#54147 = CARTESIAN_POINT ( 'NONE',  ( 180.6620941962883933, -49.11927476322659913, 40.22110306067540364 ) ) ;
#54148 = FACE_OUTER_BOUND ( 'NONE', #65209, .T. ) ;
#54149 = CARTESIAN_POINT ( 'NONE',  ( 61.22916666666666430, 7.950000000000001954, -2.130196079827421762 ) ) ;
#54150 = CARTESIAN_POINT ( 'NONE',  ( -21.29974487139158512, -27.71228299555221142, 4.000000000000000000 ) ) ;
#54152 = EDGE_CURVE ( 'NONE', #15997, #133006, #82456, .T. ) ;
#54151 = VECTOR ( 'NONE', #20045, 1000.000000000000000 ) ;
#54153 = EDGE_CURVE ( 'NONE', #42862, #31655, #61094, .T. ) ;
#54154 = DIRECTION ( 'NONE',  ( -0.000000000000000000, -0.3543493200069152693, 0.9351131265310292928 ) ) ;
#54155 = CARTESIAN_POINT ( 'NONE',  ( 0.000000000000000000, 0.000000000000000000, 0.000000000000000000 ) ) ;
#54156 = ORIENTED_EDGE ( 'NONE', *, *, #87663, .F. ) ;
#54157 = VECTOR ( 'NONE', #59528, 1000.000000000000000 ) ;
#54158 = VERTEX_POINT ( 'NONE', #17189 ) ;
#54159 = CARTESIAN_POINT ( 'NONE',  ( 111.0370968585647944, -3.054999999999998828, -5.291415217122919401 ) ) ;
#54160 = EDGE_LOOP ( 'NONE', ( #135936, #121030, #13963, #139206 ) ) ;
#54161 = EDGE_CURVE ( 'NONE', #72846, #123539, #115739, .T. ) ;
#54162 = ORIENTED_EDGE ( 'NONE', *, *, #45574, .T. ) ;
#54163 = AXIS2_PLACEMENT_3D ( 'NONE', #67988, #112857, #133912 ) ;
#54164 = CARTESIAN_POINT ( 'NONE',  ( 184.0821179325846799, -51.13011358081449487, 36.94363806876470591 ) ) ;
#54165 = CARTESIAN_POINT ( 'NONE',  ( 19.17183060077634238, -14.24070752338414003, 4.000000000000000000 ) ) ;
#54166 = EDGE_CURVE ( 'NONE', #63821, #42862, #83161, .T. ) ;
#54167 = DIRECTION ( 'NONE',  ( 0.7071067811865486830, 0.7071067811865463515, 0.000000000000000000 ) ) ;
#54168 = ORIENTED_EDGE ( 'NONE', *, *, #44872, .F. ) ;
#54169 = CARTESIAN_POINT ( 'NONE',  ( -25.39999999999996305, 0.000000000000000000, 0.000000000000000000 ) ) ;
#54170 = DIRECTION ( 'NONE',  ( -0.7071067811865487940, 0.7071067811865463515, -0.000000000000000000 ) ) ;
#54172 = LINE ( 'NONE', #22190, #96548 ) ;
#54171 = FACE_OUTER_BOUND ( 'NONE', #107085, .T. ) ;
#54173 = LINE ( 'NONE', #44737, #32258 ) ;
#54174 = AXIS2_PLACEMENT_3D ( 'NONE', #48846, #93763, #38671 ) ;
#54175 = EDGE_CURVE ( 'NONE', #103024, #79108, #43240, .T. ) ;
#54176 = DIRECTION ( 'NONE',  ( 1.000000000000000000, 0.000000000000000000, 0.000000000000000000 ) ) ;
#54177 = ORIENTED_EDGE ( 'NONE', *, *, #60749, .F. ) ;
#54178 = CARTESIAN_POINT ( 'NONE',  ( 60.18398860626900415, 28.73617430169829490, 5.000000000000000000 ) ) ;
#54179 = LINE ( 'NONE', #98366, #115915 ) ;
#54180 = ORIENTED_EDGE ( 'NONE', *, *, #41560, .F. ) ;
#54181 = ORIENTED_EDGE ( 'NONE', *, *, #123583, .T. ) ;
#54182 = EDGE_LOOP ( 'NONE', ( #142535, #34199, #111271, #73068 ) ) ;
#54183 = CARTESIAN_POINT ( 'NONE',  ( 63.29209685856476852, -5.291415217122921177, 3.054999999999999272 ) ) ;
#54184 = EDGE_CURVE ( 'NONE', #98472, #43787, #131671, .T. ) ;
#54185 = EDGE_LOOP ( 'NONE', ( #61077, #84217, #81256, #35093 ) ) ;
#54186 = CARTESIAN_POINT ( 'NONE',  ( 69.29974487139159578, -27.71228299555254537, 4.000000000000000000 ) ) ;
#54187 = VECTOR ( 'NONE', #91282, 1000.000000000000227 ) ;
#54188 = CARTESIAN_POINT ( 'NONE',  ( -0.9750270504628943957, -4.461849672132299993, -4.461849672132299105 ) ) ;
#54189 = CARTESIAN_POINT ( 'NONE',  ( 103.3962635252314470, 4.472830434245840259, -4.472830434245838482 ) ) ;
#54190 = CARTESIAN_POINT ( 'NONE',  ( 34.92499999999998295, 6.759292476615656575, 4.255531930566160526 ) ) ;
#54192 = CARTESIAN_POINT ( 'NONE',  ( -22.49999999999984013, -14.56887692260766087, 4.000000000000000000 ) ) ;
#54191 = CARTESIAN_POINT ( 'NONE',  ( -26.99999999999981526, -19.22509904557638549, 1.855685503482115584 ) ) ;
#54193 = EDGE_CURVE ( 'NONE', #79114, #106843, #67123, .T. ) ;
#54194 = EDGE_LOOP ( 'NONE', ( #52028, #115560, #140251 ) ) ;
#54195 = DIRECTION ( 'NONE',  ( -0.6830127018922181881, 0.6830127018922202975, -0.2588190451025214056 ) ) ;
#54196 = CARTESIAN_POINT ( 'NONE',  ( 30.79289321881324781, -17.24070752338410628, 5.000000000000000000 ) ) ;
#54197 = VECTOR ( 'NONE', #19357, 1000.000000000000000 ) ;
#54198 = DIRECTION ( 'NONE',  ( 0.7071067811865487940, 0.7071067811865463515, -0.000000000000000000 ) ) ;
#54200 = EDGE_CURVE ( 'NONE', #47328, #118264, #65739, .T. ) ;
#54199 = PLANE ( 'NONE',  #15074 ) ;
#54201 = EDGE_LOOP ( 'NONE', ( #95166, #135508, #7117 ) ) ;
#54202 = LINE ( 'NONE', #52026, #92050 ) ;
#54203 = ORIENTED_EDGE ( 'NONE', *, *, #138746, .T. ) ;
#54204 = ADVANCED_FACE ( 'NONE', ( #55539 ), #10566, .F. ) ;
#54205 = ORIENTED_EDGE ( 'NONE', *, *, #7853, .F. ) ;
#54206 = EDGE_LOOP ( 'NONE', ( #112118, #123161, #17844, #37922 ) ) ;
#54207 = CARTESIAN_POINT ( 'NONE',  ( 124.0162635252314516, -4.472830434245838482, 4.472830434245838482 ) ) ;
#54208 = VERTEX_POINT ( 'NONE', #43943 ) ;
#54209 = EDGE_CURVE ( 'NONE', #37150, #22300, #64997, .T. ) ;
#54210 = CARTESIAN_POINT ( 'NONE',  ( -11.99451991528749417, 28.92564299267946382, 4.000000000000000000 ) ) ;
#54211 = CARTESIAN_POINT ( 'NONE',  ( 34.49999999999975131, 13.46425560840035196, 4.994342998332160555 ) ) ;
#54212 = ORIENTED_EDGE ( 'NONE', *, *, #73856, .T. ) ;
#54213 = DIRECTION ( 'NONE',  ( 0.7071067811865486830, -0.7071067811865464625, -0.000000000000000000 ) ) ;
#54214 = ORIENTED_EDGE ( 'NONE', *, *, #44765, .F. ) ;
#54215 = VECTOR ( 'NONE', #41112, 1000.000000000000000 ) ;
#54216 = VECTOR ( 'NONE', #27654, 1000.000000000000114 ) ;
#54217 = CARTESIAN_POINT ( 'NONE',  ( 9.166236474768552966, 7.934999999999990727, -1.457635852685135314E-15 ) ) ;
#54218 = DIRECTION ( 'NONE',  ( -0.7071067811865486830, -0.7071067811865464625, 0.000000000000000000 ) ) ;
#54219 = FACE_OUTER_BOUND ( 'NONE', #97111, .T. ) ;
#54220 = EDGE_CURVE ( 'NONE', #88566, #69745, #404, .T. ) ;
#54221 = CARTESIAN_POINT ( 'NONE',  ( 11.47472276569333083, -8.505968740979792386, -4.231148911907932408 ) ) ;
#54222 = ORIENTED_EDGE ( 'NONE', *, *, #141115, .T. ) ;
#54223 = ORIENTED_EDGE ( 'NONE', *, *, #129485, .T. ) ;
#54224 = ORIENTED_EDGE ( 'NONE', *, *, #119597, .F. ) ;
#54225 = CARTESIAN_POINT ( 'NONE',  ( 20.56249999999999645, 4.461849672132300881, 4.461849672132299105 ) ) ;
#54226 = DIRECTION ( 'NONE',  ( -0.000000000000000000, 0.000000000000000000, 1.000000000000000000 ) ) ;
#54227 = LINE ( 'NONE', #44035, #24191 ) ;
#54228 = EDGE_CURVE ( 'NONE', #1839, #140728, #41799, .T. ) ;
#54229 = CARTESIAN_POINT ( 'NONE',  ( 31.49999999999979039, 6.052185695429111334, 5.000000000000000000 ) ) ;
#54230 = CARTESIAN_POINT ( 'NONE',  ( 34.92499999999998295, 22.22500000000000142, 4.500000000000000888 ) ) ;
#54231 = AXIS2_PLACEMENT_3D ( 'NONE', #12274, #76863, #1375 ) ;
#54232 = CARTESIAN_POINT ( 'NONE',  ( 29.31293019189811133, -1.637169565754159617, -6.110000000000001208 ) ) ;
#54233 = LINE ( 'NONE', #101262, #53676 ) ;
#54234 = LINE ( 'NONE', #133900, #39674 ) ;
#54235 = ORIENTED_EDGE ( 'NONE', *, *, #105688, .F. ) ;
#54236 = CARTESIAN_POINT ( 'NONE',  ( 4.000000000000000000, 8.616843969807042924, 0.000000000000000000 ) ) ;
#54237 = EDGE_LOOP ( 'NONE', ( #101968, #41793, #128995, #115744, #57521 ) ) ;
#54238 = CARTESIAN_POINT ( 'NONE',  ( 22.42819999999999681, 3.174999999999997158, 0.000000000000000000 ) ) ;
#54239 = ORIENTED_EDGE ( 'NONE', *, *, #46964, .F. ) ;
#54240 = CIRCLE ( 'NONE', #109771, 2.055000000000001048 ) ;
#54241 = CARTESIAN_POINT ( 'NONE',  ( 18.56663961620377279, 1.633150327867675555, 6.094999999999998863 ) ) ;
#54243 = ORIENTED_EDGE ( 'NONE', *, *, #34279, .T. ) ;
#54242 = CARTESIAN_POINT ( 'NONE',  ( 8.031592354503320763, 2.500000000000001332, 0.000000000000000000 ) ) ;
#54244 = VECTOR ( 'NONE', #108153, 1000.000000000000000 ) ;
#54245 = CARTESIAN_POINT ( 'NONE',  ( -19.41009064519819916, 9.759292476615618384, 11.28811694763774298 ) ) ;
#54246 = EDGE_CURVE ( 'NONE', #117563, #5082, #42540, .T. ) ;
#54247 = ORIENTED_EDGE ( 'NONE', *, *, #97396, .F. ) ;
#54248 = CARTESIAN_POINT ( 'NONE',  ( 22.49999999999984013, -4.216083040037233332, -7.486842126848710421 ) ) ;
#54249 = ORIENTED_EDGE ( 'NONE', *, *, #131278, .F. ) ;
#54250 = PLANE ( 'NONE',  #39710 ) ;
#54251 = VERTEX_POINT ( 'NONE', #32352 ) ;
#54252 = VECTOR ( 'NONE', #140255, 1000.000000000000000 ) ;
#54253 = EDGE_CURVE ( 'NONE', #110463, #98003, #33796, .T. ) ;
#54254 = CARTESIAN_POINT ( 'NONE',  ( 116.4541937171295558, 6.884901960086283523, 3.975000000000002753 ) ) ;
#54256 = VECTOR ( 'NONE', #136526, 1000.000000000000000 ) ;
#54255 = CARTESIAN_POINT ( 'NONE',  ( 48.78752705046289151, 0.000000000000000000, -7.949999999999998401 ) ) ;
#54257 = CARTESIAN_POINT ( 'NONE',  ( 14.70025512860841133, -27.71228299555195917, 4.000000000000000000 ) ) ;
#54258 = CARTESIAN_POINT ( 'NONE',  ( 0.000000000000000000, 0.000000000000000000, 5.000000000000000000 ) ) ;
#54259 = CARTESIAN_POINT ( 'NONE',  ( -8.999999999999932498, 14.96639925780211478, 5.000000000000000000 ) ) ;
#54260 = CARTESIAN_POINT ( 'NONE',  ( 6.416666666666666963, 5.278424836066147208, 3.047499999999990550 ) ) ;
#54261 = CARTESIAN_POINT ( 'NONE',  ( 20.83290314143522082, -3.967499999999994476, 6.871911579029513106 ) ) ;
#54262 = LINE ( 'NONE', #11386, #141562 ) ;
#54263 = DIRECTION ( 'NONE',  ( -0.6830127018922181881, 0.6830127018922202975, -0.2588190451025214056 ) ) ;
#54264 = EDGE_LOOP ( 'NONE', ( #12124, #117482, #55300, #54224 ) ) ;
#54266 = ADVANCED_FACE ( 'NONE', ( #54830 ), #99735, .F. ) ;
#54265 = SHAPE_REPRESENTATION ( 'parallel pin unhardened_iso_ISO 2338 - 2.5 m6 x 8 - St', ( #127880 ), #33203 ) ;
#54267 = ORIENTED_EDGE ( 'NONE', *, *, #75838, .F. ) ;
#54268 = EDGE_CURVE ( 'NONE', #72412, #79859, #75861, .T. ) ;
#54269 = LINE ( 'NONE', #54963, #23540 ) ;
#54270 = VERTEX_POINT ( 'NONE', #9107 ) ;
#54271 = CARTESIAN_POINT ( 'NONE',  ( 54.18398860626899705, 28.73617430169825226, 5.000000000000000000 ) ) ;
#54272 = DIRECTION ( 'NONE',  ( -0.3543493200069162685, -0.000000000000000000, -0.9351131265310288487 ) ) ;
#54273 = VECTOR ( 'NONE', #34053, 1000.000000000000000 ) ;
#54274 = LINE ( 'NONE', #110026, #8515 ) ;
#54275 = VERTEX_POINT ( 'NONE', #88167 ) ;
#54276 = CARTESIAN_POINT ( 'NONE',  ( -15.00548008471250228, 28.92564299267927552, 4.000000000000000000 ) ) ;
#54277 = LINE ( 'NONE', #143383, #44217 ) ;
#54278 = DIRECTION ( 'NONE',  ( 0.7071067811865487940, 0.7071067811865463515, -0.000000000000000000 ) ) ;
#54279 = EDGE_CURVE ( 'NONE', #44877, #15280, #9869, .T. ) ;
#54280 = DIRECTION ( 'NONE',  ( -0.7071067811865486830, -0.7071067811865464625, 0.000000000000000000 ) ) ;
#54281 = DIRECTION ( 'NONE',  ( 0.000000000000000000, 1.000000000000000000, -4.625929269271485322E-15 ) ) ;
#54283 = ORIENTED_EDGE ( 'NONE', *, *, #46495, .T. ) ;
#54282 = DIRECTION ( 'NONE',  ( 0.000000000000000000, 1.000000000000000000, 0.000000000000000000 ) ) ;
#54284 = LINE ( 'NONE', #97749, #90580 ) ;
#54285 = LINE ( 'NONE', #140526, #133186 ) ;
#54286 = PRESENTATION_STYLE_ASSIGNMENT (( #133260 ) ) ;
#54287 = DIRECTION ( 'NONE',  ( -0.6830127018922180770, -0.6830127018922204085, -0.2588190451025213501 ) ) ;
#54288 = DIRECTION ( 'NONE',  ( -0.7071067811865486830, -0.7071067811865464625, 0.000000000000000000 ) ) ;
#54289 = ORIENTED_EDGE ( 'NONE', *, *, #70056, .T. ) ;
#54290 = VERTEX_POINT ( 'NONE', #141086 ) ;
#54291 = VERTEX_POINT ( 'NONE', #120025 ) ;
#54292 = CARTESIAN_POINT ( 'NONE',  ( 93.91709685856477563, 3.054999999999998828, 5.291415217122922066 ) ) ;
#54293 = EDGE_LOOP ( 'NONE', ( #23538, #126315, #2273, #31935 ) ) ;
#54294 = CARTESIAN_POINT ( 'NONE',  ( -19.05000000000000071, 3.174999999999997158, 1.444000000000000394 ) ) ;
#54295 = CARTESIAN_POINT ( 'NONE',  ( 84.95419371712955581, 6.884901960086283523, 3.975000000000002753 ) ) ;
#54296 = EDGE_LOOP ( 'NONE', ( #58951, #74508, #7648, #71304, #74729, #65160, #70960 ) ) ;
#54297 = CARTESIAN_POINT ( 'NONE',  ( 34.92499999999998295, -14.99387692260787652, 4.000000000000000000 ) ) ;
#54299 = VECTOR ( 'NONE', #45788, 1000.000000000000000 ) ;
#54298 = DIRECTION ( 'NONE',  ( -0.000000000000000000, 0.000000000000000000, 1.000000000000000000 ) ) ;
#54300 = CARTESIAN_POINT ( 'NONE',  ( 90.18293019189809456, -1.637169565754158951, -6.109999999999998543 ) ) ;
#54301 = VERTEX_POINT ( 'NONE', #86011 ) ;
#54302 = CARTESIAN_POINT ( 'NONE',  ( -29.99999999999979039, 18.08204922493370503, 0.9627537363045557406 ) ) ;
#54303 = EDGE_CURVE ( 'NONE', #127190, #121732, #68856, .T. ) ;
#54304 = DIRECTION ( 'NONE',  ( -0.3543493200069162685, -0.000000000000000000, -0.9351131265310288487 ) ) ;
#54305 = ORIENTED_EDGE ( 'NONE', *, *, #112450, .F. ) ;
#54306 = EDGE_LOOP ( 'NONE', ( #65215, #57029, #70334, #140365 ) ) ;
#54307 = ORIENTED_EDGE ( 'NONE', *, *, #133980, .F. ) ;
#54308 = CARTESIAN_POINT ( 'NONE',  ( 23.99999999999982947, 2.342191155542475034, -5.001666872980140788 ) ) ;
#54309 = ADVANCED_FACE ( 'NONE', ( #30939 ), #75171, .F. ) ;
#54310 = EDGE_CURVE ( 'NONE', #112531, #64780, #119330, .T. ) ;
#54311 = DIRECTION ( 'NONE',  ( -0.7071067811865487940, 0.7071067811865463515, 0.000000000000000000 ) ) ;
#54312 = CARTESIAN_POINT ( 'NONE',  ( 14.21290314143522160, 3.967499999999992699, -6.871911579029513994 ) ) ;
#54313 = CARTESIAN_POINT ( 'NONE',  ( -17.99451991528748351, 28.92564299267950645, 4.000000000000000000 ) ) ;
#54314 = CIRCLE ( 'NONE', #135329, 2.999999999999992450 ) ;
#54315 = LINE ( 'NONE', #10742, #133580 ) ;
#54316 = CARTESIAN_POINT ( 'NONE',  ( 34.47516574401890921, 12.02806734111568687, 4.998110765256834398 ) ) ;
#54317 = EDGE_CURVE ( 'NONE', #102292, #47660, #24324, .T. ) ;
#54318 = ADVANCED_FACE ( 'NONE', ( #35946 ), #101160, .T. ) ;
#54319 = VECTOR ( 'NONE', #58760, 1000.000000000000114 ) ;
#54320 = EDGE_CURVE ( 'NONE', #42461, #119756, #101409, .T. ) ;
#54321 = ORIENTED_EDGE ( 'NONE', *, *, #96129, .F. ) ;
#54322 = ORIENTED_EDGE ( 'NONE', *, *, #62147, .T. ) ;
#54323 = VECTOR ( 'NONE', #48170, 1000.000000000000000 ) ;
#54325 = EDGE_CURVE ( 'NONE', #38343, #135502, #45398, .T. ) ;
#54324 = DIRECTION ( 'NONE',  ( 1.000000000000000000, 0.000000000000000000, 0.000000000000000000 ) ) ;
#54326 = ORIENTED_EDGE ( 'NONE', *, *, #53866, .F. ) ;
#54327 = EDGE_LOOP ( 'NONE', ( #73506, #126197, #10842, #83667 ) ) ;
#54328 = EDGE_CURVE ( 'NONE', #33187, #133473, #2542, .T. ) ;
#54329 = ADVANCED_FACE ( 'NONE', ( #46104 ), #132478, .T. ) ;
#54330 = DIRECTION ( 'NONE',  ( 0.7071067811865487940, 0.7071067811865463515, -0.000000000000000000 ) ) ;
#54331 = ORIENTED_EDGE ( 'NONE', *, *, #25118, .T. ) ;
#54332 = AXIS2_PLACEMENT_3D ( 'NONE', #19411, #117273, #30290 ) ;
#54333 = CARTESIAN_POINT ( 'NONE',  ( -41.99451991528749062, 28.92564299267967343, 4.000000000000000000 ) ) ;
#54334 = CARTESIAN_POINT ( 'NONE',  ( 0.000000000000000000, 0.000000000000000000, 6.750000000000000888 ) ) ;
#54335 = LINE ( 'NONE', #86224, #57195 ) ;
#54336 = CARTESIAN_POINT ( 'NONE',  ( -27.48921356237309155, -27.52281430457074762, 5.000000000000000000 ) ) ;
#54337 = CARTESIAN_POINT ( 'NONE',  ( 118.9791666666666430, -7.950000000000000178, 2.130196079827424427 ) ) ;
#54338 = ORIENTED_EDGE ( 'NONE', *, *, #29534, .F. ) ;
#54339 = EDGE_CURVE ( 'NONE', #119913, #14862, #122929, .T. ) ;
#54340 = LINE ( 'NONE', #142741, #78928 ) ;
#54341 = ORIENTED_EDGE ( 'NONE', *, *, #76951, .T. ) ;
#54342 = DIRECTION ( 'NONE',  ( -0.000000000000000000, 0.3543493200069153248, 0.9351131265310292928 ) ) ;
#54343 = EDGE_LOOP ( 'NONE', ( #133265, #48706, #77176, #140648 ) ) ;
#54344 = FACE_OUTER_BOUND ( 'NONE', #46382, .T. ) ;
#54345 = ORIENTED_EDGE ( 'NONE', *, *, #4204, .F. ) ;
#54346 = FACE_OUTER_BOUND ( 'NONE', #36577, .T. ) ;
#54347 = VERTEX_POINT ( 'NONE', #124351 ) ;
#54348 = ORIENTED_EDGE ( 'NONE', *, *, #66163, .T. ) ;
#54349 = ADVANCED_FACE ( 'NONE', ( #46850 ), #14144, .F. ) ;
#54350 = VERTEX_POINT ( 'NONE', #70719 ) ;
#54351 = AXIS2_PLACEMENT_3D ( 'NONE', #116549, #61495, #50580 ) ;
#54352 = LINE ( 'NONE', #21690, #16406 ) ;
#54353 = COLOUR_RGB ( '', 0.66274510, 0.83137255, 0.94901961) ;
#54354 = VECTOR ( 'NONE', #129055, 1000.000000000000000 ) ;
#54355 = CARTESIAN_POINT ( 'NONE',  ( 75.18398860626899705, 28.73617430169839793, 5.000000000000000000 ) ) ;
#54356 = CARTESIAN_POINT ( 'NONE',  ( 10.49999999999993605, -17.94781430457064531, 5.000000000000000000 ) ) ;
#54357 = PRESENTATION_STYLE_ASSIGNMENT (( #131887 ) ) ;
#54358 = DIRECTION ( 'NONE',  ( -0.7071067811865486830, 0.7071067811865464625, 0.000000000000000000 ) ) ;
#54359 = CARTESIAN_POINT ( 'NONE',  ( -12.32816939922344268, 8.259292476615630818, 4.000000000000000000 ) ) ;
#54360 = LINE ( 'NONE', #120993, #80638 ) ;
#54361 = CARTESIAN_POINT ( 'NONE',  ( 34.42499999999998295, 0.000000000000000000, 4.500000000000000888 ) ) ;
#54362 = VECTOR ( 'NONE', #136674, 999.9999999999998863 ) ;
#54364 = EDGE_CURVE ( 'NONE', #131796, #135826, #90281, .T. ) ;
#54363 = LINE ( 'NONE', #43453, #108403 ) ;
#54365 = LINE ( 'NONE', #107953, #82978 ) ;
#54366 = CARTESIAN_POINT ( 'NONE',  ( -25.39999999999996305, 3.061616997868383141E-16, -2.500000000000000000 ) ) ;
#54367 = EDGE_LOOP ( 'NONE', ( #50380, #20086, #89901 ) ) ;
#54368 = EDGE_CURVE ( 'NONE', #127835, #139877, #56289, .T. ) ;
#54369 = VERTEX_POINT ( 'NONE', #133804 ) ;
#54370 = VERTEX_POINT ( 'NONE', #34491 ) ;
#54371 = DIRECTION ( 'NONE',  ( -0.7071067811865486830, -0.7071067811865464625, 0.000000000000000000 ) ) ;
#54372 = ORIENTED_EDGE ( 'NONE', *, *, #105529, .T. ) ;
#54373 = EDGE_CURVE ( 'NONE', #8795, #110134, #78710, .T. ) ;
#54374 = ORIENTED_EDGE ( 'NONE', *, *, #89328, .T. ) ;
#54375 = DIRECTION ( 'NONE',  ( -0.7071067811865487940, 0.7071067811865463515, 0.000000000000000000 ) ) ;
#54376 = FILL_AREA_STYLE_COLOUR ( '', #43475 ) ;
#54377 = CARTESIAN_POINT ( 'NONE',  ( -30.18398860626900060, 28.73617430169808173, 5.000000000000000000 ) ) ;
#54378 = VERTEX_POINT ( 'NONE', #58437 ) ;
#54379 = CARTESIAN_POINT ( 'NONE',  ( 6.299744871391586898, -27.71228299555210484, 4.000000000000000000 ) ) ;
#54380 = ORIENTED_EDGE ( 'NONE', *, *, #48628, .F. ) ;
#54381 = PRESENTATION_STYLE_ASSIGNMENT (( #97088 ) ) ;
#54382 = DIRECTION ( 'NONE',  ( -0.7071067811865487940, 0.7071067811865463515, -0.000000000000000000 ) ) ;
#54383 = CARTESIAN_POINT ( 'NONE',  ( 17.56706980810188767, 2.126176841940952134, -7.934999999999993392 ) ) ;
#54384 = ORIENTED_EDGE ( 'NONE', *, *, #16345, .T. ) ;
#54385 = CARTESIAN_POINT ( 'NONE',  ( 90.32876352523145158, 0.000000000000000000, -6.109999999999999432 ) ) ;
#54386 = DIRECTION ( 'NONE',  ( -0.000000000000000000, -0.3543493200069152693, 0.9351131265310292928 ) ) ;
#54388 = ADVANCED_FACE ( 'NONE', ( #72156 ), #49678, .F. ) ;
#54387 = CARTESIAN_POINT ( 'NONE',  ( -24.29974487139158867, -27.71228299555223273, 4.000000000000000000 ) ) ;
#54389 = DIRECTION ( 'NONE',  ( -1.000000000000000000, -1.224606353822377258E-16, -0.000000000000000000 ) ) ;
#54390 = ORIENTED_EDGE ( 'NONE', *, *, #106320, .T. ) ;
#54391 = CARTESIAN_POINT ( 'NONE',  ( 0.000000000000000000, 0.000000000000000000, 0.000000000000000000 ) ) ;
#54392 = VERTEX_POINT ( 'NONE', #27166 ) ;
#54393 = ORIENTED_EDGE ( 'NONE', *, *, #59446, .F. ) ;
#54394 = LINE ( 'NONE', #141364, #99582 ) ;
#54395 = DIRECTION ( 'NONE',  ( -1.000000000000000000, -1.224606353822377258E-16, -0.000000000000000000 ) ) ;
#54396 = CARTESIAN_POINT ( 'NONE',  ( -3.770042794577900924, 21.73644205237997085, 5.000000000000000888 ) ) ;
#54397 = DIRECTION ( 'NONE',  ( -0.000000000000000000, 0.000000000000000000, 1.000000000000000000 ) ) ;
#54399 = ORIENTED_EDGE ( 'NONE', *, *, #94602, .F. ) ;
#54398 = VECTOR ( 'NONE', #10781, 1000.000000000000000 ) ;
#54400 = FACE_OUTER_BOUND ( 'NONE', #114612, .T. ) ;
#54401 = ADVANCED_FACE ( 'NONE', ( #128637 ), #62678, .T. ) ;
#54402 = DIRECTION ( 'NONE',  ( -0.000000000000000000, -1.000000000000000000, -0.000000000000000000 ) ) ;
#54403 = ORIENTED_EDGE ( 'NONE', *, *, #135838, .F. ) ;
#54404 = FACE_OUTER_BOUND ( 'NONE', #116325, .T. ) ;
#54405 = FACE_OUTER_BOUND ( 'NONE', #51545, .T. ) ;
#54406 = ORIENTED_EDGE ( 'NONE', *, *, #84533, .T. ) ;
#54409 = ADVANCED_FACE ( 'NONE', ( #27888 ), #93856, .F. ) ;
#54408 = ORIENTED_EDGE ( 'NONE', *, *, #64594, .F. ) ;
#54407 = LINE ( 'NONE', #44235, #60315 ) ;
#54410 = ORIENTED_EDGE ( 'NONE', *, *, #24166, .F. ) ;
#54411 = CARTESIAN_POINT ( 'NONE',  ( -5.510786437626906675, -27.52281430457051314, 5.000000000000000000 ) ) ;
#54412 = FACE_OUTER_BOUND ( 'NONE', #82498, .T. ) ;
#54413 = EDGE_LOOP ( 'NONE', ( #47853, #48927, #14496, #73902, #50181 ) ) ;
#54414 = LINE ( 'NONE', #20301, #11827 ) ;
#54415 = DIRECTION ( 'NONE',  ( 0.7071067811865486830, -0.7071067811865464625, -0.000000000000000000 ) ) ;
#54416 = CIRCLE ( 'NONE', #66007, 0.5000000000000004441 ) ;
#54417 = EDGE_CURVE ( 'NONE', #63482, #73550, #105435, .T. ) ;
#54418 =( BOUNDED_CURVE ( )  B_SPLINE_CURVE ( 3, ( #16589, #60879, #39075, #83301 ),
 .UNSPECIFIED., .F., .T. ) 
 B_SPLINE_CURVE_WITH_KNOTS ( ( 4, 4 ),
 ( 5.043186909253417838, 5.074607125596330093 ),
 .UNSPECIFIED. ) 
 CURVE ( )  GEOMETRIC_REPRESENTATION_ITEM ( )  RATIONAL_B_SPLINE_CURVE ( ( 1.000000000000000000, 0.9999177325257870841, 0.9999177325257870841, 1.000000000000000000 ) ) 
 REPRESENTATION_ITEM ( '' )  );
#54419 = DIRECTION ( 'NONE',  ( 0.7071067811865487940, 0.7071067811865463515, 0.000000000000000000 ) ) ;
#54421 = CARTESIAN_POINT ( 'NONE',  ( 33.18398860626899705, 28.73617430169810305, 5.000000000000000000 ) ) ;
#54420 = VECTOR ( 'NONE', #26948, 1000.000000000000000 ) ;
#54422 = FACE_OUTER_BOUND ( 'NONE', #115582, .T. ) ;
#54423 = CARTESIAN_POINT ( 'NONE',  ( -34.92500000000001137, -8.337538124160923658, 4.000000000000000000 ) ) ;
#54424 = CARTESIAN_POINT ( 'NONE',  ( -3.156123077392388065, -22.22500000000000142, 4.000000000000000000 ) ) ;
#54425 = FACE_OUTER_BOUND ( 'NONE', #75210, .T. ) ;
#54426 = DIRECTION ( 'NONE',  ( -0.000000000000000000, 0.3543493200069153248, 0.9351131265310292928 ) ) ;
#54427 = CARTESIAN_POINT ( 'NONE',  ( 11.51078643762690490, -27.52281430457047406, 5.000000000000000000 ) ) ;
#54428 = DIRECTION ( 'NONE',  ( 0.000000000000000000, 0.000000000000000000, -1.000000000000000000 ) ) ;
#54429 = CARTESIAN_POINT ( 'NONE',  ( 19.78501580275798588, -3.740707523384238176, 15.76143240460128503 ) ) ;
#54430 = ORIENTED_EDGE ( 'NONE', *, *, #68754, .F. ) ;
#54431 = ADVANCED_FACE ( 'NONE', ( #38072 ), #137382, .T. ) ;
#54432 = ORIENTED_EDGE ( 'NONE', *, *, #114682, .T. ) ;
#54433 = CARTESIAN_POINT ( 'NONE',  ( 97.39583333333334281, -2.130196079827427091, 7.949999999999999289 ) ) ;
#54434 = ADVANCED_FACE ( 'NONE', ( #126473 ), #6091, .F. ) ;
#54435 = VERTEX_POINT ( 'NONE', #61972 ) ;
#54436 = AXIS2_PLACEMENT_3D ( 'NONE', #108352, #141764, #64194 ) ;
#54437 = ORIENTED_EDGE ( 'NONE', *, *, #101720, .T. ) ;
#54438 = ORIENTED_EDGE ( 'NONE', *, *, #127837, .F. ) ;
#54439 = PLANE ( 'NONE',  #114957 ) ;
#54440 = DIRECTION ( 'NONE',  ( -0.7071067811865487940, 0.7071067811865463515, 0.000000000000000000 ) ) ;
#54441 = ORIENTED_EDGE ( 'NONE', *, *, #106437, .T. ) ;
#54442 = DIRECTION ( 'NONE',  ( 0.7071067811865487940, -0.7071067811865463515, 0.000000000000000000 ) ) ;
#54443 = DIRECTION ( 'NONE',  ( -0.000000000000000000, -0.000000000000000000, -1.000000000000000000 ) ) ;
#54444 = DIRECTION ( 'NONE',  ( -0.6830127018922181881, 0.6830127018922202975, -0.2588190451025214056 ) ) ;
#54445 = CARTESIAN_POINT ( 'NONE',  ( -34.92500000000001137, -7.487538124160419528, 4.000000000000000000 ) ) ;
#54446 = ORIENTED_EDGE ( 'NONE', *, *, #20971, .F. ) ;
#54447 = EDGE_CURVE ( 'NONE', #75313, #81350, #117716, .T. ) ;
#54448 = CARTESIAN_POINT ( 'NONE',  ( 14.93213401340503310, 4.189643424786883230, -32.27832594409215261 ) ) ;
#54449 = CARTESIAN_POINT ( 'NONE',  ( 0.000000000000000000, 0.000000000000000000, 5.000000000000000000 ) ) ;
#54450 = DIRECTION ( 'NONE',  ( 0.7071067811865487940, 0.7071067811865463515, 0.000000000000000000 ) ) ;
#54451 = PLANE ( 'NONE',  #137155 ) ;
#54452 = CARTESIAN_POINT ( 'NONE',  ( 0.000000000000000000, -0.5999999999999994227, -3.054668707061620747 ) ) ;
#54453 = CARTESIAN_POINT ( 'NONE',  ( 27.35002705046288085, -5.819803920172572198, -5.819803920172572198 ) ) ;
#54454 = VECTOR ( 'NONE', #49641, 1000.000000000000227 ) ;
#54455 = LINE ( 'NONE', #32693, #100164 ) ;
#54456 = AXIS2_PLACEMENT_3D ( 'NONE', #5981, #61859, #103187 ) ;
#54457 = EDGE_LOOP ( 'NONE', ( #72443, #71643, #36860, #68650 ) ) ;
#54458 = EDGE_LOOP ( 'NONE', ( #25464, #8016, #95300, #614 ) ) ;
#54459 = CARTESIAN_POINT ( 'NONE',  ( 116.6670968585647756, -3.055000000000000160, -5.291415217122921177 ) ) ;
#54460 = ORIENTED_EDGE ( 'NONE', *, *, #62500, .F. ) ;
#54461 = VECTOR ( 'NONE', #134030, 1000.000000000000000 ) ;
#54462 = CARTESIAN_POINT ( 'NONE',  ( -63.48921356237309510, -27.52281430457099631, 5.000000000000000000 ) ) ;
#54463 = DIRECTION ( 'NONE',  ( -0.7071067811865486830, -0.7071067811865464625, -0.000000000000000000 ) ) ;
#54464 = CARTESIAN_POINT ( 'NONE',  ( -3.489213562373097322, -27.52281430457057709, 5.000000000000000000 ) ) ;
#54465 = FACE_OUTER_BOUND ( 'NONE', #105236, .T. ) ;
#54466 = CARTESIAN_POINT ( 'NONE',  ( -5.207106781186508826, 6.759292476615651246, 5.000000000000000000 ) ) ;
#54467 = DIRECTION ( 'NONE',  ( -0.7071067811865486830, -0.7071067811865464625, -0.000000000000000000 ) ) ;
#54468 = CARTESIAN_POINT ( 'NONE',  ( 122.7037635252314516, 6.109999999999998543, 1.122388791418548911E-15 ) ) ;
#54469 = ORIENTED_EDGE ( 'NONE', *, *, #42566, .F. ) ;
#54470 = EDGE_CURVE ( 'NONE', #138219, #75105, #6806, .T. ) ;
#54471 = ORIENTED_EDGE ( 'NONE', *, *, #48932, .T. ) ;
#54472 = LINE ( 'NONE', #30566, #26991 ) ;
#54473 = ORIENTED_EDGE ( 'NONE', *, *, #129278, .F. ) ;
#54474 = CARTESIAN_POINT ( 'NONE',  ( 36.45876352523143282, 0.000000000000000000, -6.110000000000001208 ) ) ;
#54475 = ORIENTED_EDGE ( 'NONE', *, *, #39453, .T. ) ;
#54476 = DIRECTION ( 'NONE',  ( -0.7071067811865486830, 0.7071067811865464625, 0.000000000000000000 ) ) ;
#54477 = EDGE_CURVE ( 'NONE', #2768, #139894, #106863, .T. ) ;
#54478 = DIRECTION ( 'NONE',  ( -0.7071067811865486830, 0.7071067811865464625, 0.000000000000000000 ) ) ;
#54479 = FACE_OUTER_BOUND ( 'NONE', #51123, .T. ) ;
#54480 = EDGE_CURVE ( 'NONE', #83105, #46795, #60559, .T. ) ;
#54481 = CARTESIAN_POINT ( 'NONE',  ( 42.49543019189810877, 5.291415217122916737, 3.055000000000001936 ) ) ;
#54482 = EDGE_CURVE ( 'NONE', #861, #43029, #104732, .T. ) ;
#54483 = EDGE_LOOP ( 'NONE', ( #108260, #88620, #32507, #91843 ) ) ;
#54485 = EDGE_CURVE ( 'NONE', #9764, #113899, #95990, .T. ) ;
#54484 = FACE_OUTER_BOUND ( 'NONE', #14959, .T. ) ;
#54486 = ORIENTED_EDGE ( 'NONE', *, *, #116851, .T. ) ;
#54487 = ORIENTED_EDGE ( 'NONE', *, *, #41429, .T. ) ;
#54488 = ORIENTED_EDGE ( 'NONE', *, *, #13415, .F. ) ;
#54489 = EDGE_CURVE ( 'NONE', #96477, #60654, #23514, .T. ) ;
#54490 = FACE_OUTER_BOUND ( 'NONE', #34708, .T. ) ;
#54491 = EDGE_LOOP ( 'NONE', ( #142098, #24696, #48580, #38010 ) ) ;
#54492 = FACE_OUTER_BOUND ( 'NONE', #51895, .T. ) ;
#54493 = EDGE_CURVE ( 'NONE', #106679, #106612, #40916, .T. ) ;
#54494 = DIRECTION ( 'NONE',  ( -0.3543493200069162685, -0.000000000000000000, -0.9351131265310288487 ) ) ;
#54495 = FACE_OUTER_BOUND ( 'NONE', #60555, .T. ) ;
#54496 = PLANE ( 'NONE',  #111522 ) ;
#54497 = EDGE_CURVE ( 'NONE', #32541, #23207, #15541, .T. ) ;
#54498 = FACE_BOUND ( 'NONE', #98266, .T. ) ;
#54499 = ORIENTED_EDGE ( 'NONE', *, *, #4962, .T. ) ;
#54500 = EDGE_CURVE ( 'NONE', #129291, #12567, #126392, .T. ) ;
#54501 = PLANE ( 'NONE',  #24970 ) ;
#54502 = PLANE ( 'NONE',  #5069 ) ;
#54503 = CARTESIAN_POINT ( 'NONE',  ( -34.92500000000001137, -22.22500000000000142, 4.500000000000000888 ) ) ;
#54504 = ORIENTED_EDGE ( 'NONE', *, *, #143448, .F. ) ;
#54505 = FACE_OUTER_BOUND ( 'NONE', #27098, .T. ) ;
#54506 = ORIENTED_EDGE ( 'NONE', *, *, #87304, .T. ) ;
#54507 = ORIENTED_EDGE ( 'NONE', *, *, #37672, .F. ) ;
#54508 = EDGE_CURVE ( 'NONE', #118046, #62746, #82295, .T. ) ;
#54509 = EDGE_LOOP ( 'NONE', ( #65495, #1415, #101898, #130119, #35721 ) ) ;
#54510 = CIRCLE ( 'NONE', #140182, 2.999999999999999112 ) ;
#54511 = CARTESIAN_POINT ( 'NONE',  ( 45.12043019189810877, 3.055000000000001936, -5.291415217122916737 ) ) ;
#54512 = ORIENTED_EDGE ( 'NONE', *, *, #89962, .T. ) ;
#54513 = DIRECTION ( 'NONE',  ( -0.000000000000000000, -0.3543493200069152693, 0.9351131265310292928 ) ) ;
#54514 = VECTOR ( 'NONE', #108420, 1000.000000000000000 ) ;
#54515 = SURFACE_STYLE_FILL_AREA ( #77687 ) ;
#54516 = LINE ( 'NONE', #98696, #106593 ) ;
#54517 = VERTEX_POINT ( 'NONE', #87982 ) ;
#54518 = DIRECTION ( 'NONE',  ( 0.000000000000000000, 0.000000000000000000, -1.000000000000000000 ) ) ;
#54519 = LINE ( 'NONE', #72191, #27308 ) ;
#54520 = LINE ( 'NONE', #63276, #43310 ) ;
#54521 = VECTOR ( 'NONE', #26745, 1000.000000000000000 ) ;
#54522 = LINE ( 'NONE', #52349, #140764 ) ;
#54523 = FACE_OUTER_BOUND ( 'NONE', #89642, .T. ) ;
#54524 = CARTESIAN_POINT ( 'NONE',  ( -66.18398860626901126, 28.73617430169833753, 5.000000000000000000 ) ) ;
#54525 = LINE ( 'NONE', #129922, #20843 ) ;
#54526 = EDGE_LOOP ( 'NONE', ( #118448, #96179, #41637, #64716 ) ) ;
#54527 = EDGE_CURVE ( 'NONE', #27902, #40406, #39852, .T. ) ;
#54528 = ORIENTED_EDGE ( 'NONE', *, *, #95744, .T. ) ;
#54529 = ORIENTED_EDGE ( 'NONE', *, *, #96512, .F. ) ;
#54530 = CARTESIAN_POINT ( 'NONE',  ( 0.7071067811865406894, -12.74070752338415780, 5.000000000000000000 ) ) ;
#54531 = CARTESIAN_POINT ( 'NONE',  ( 3.398789304146614398, -2.055000000000000160, 2.789133085058097101E-16 ) ) ;
#54532 = ORIENTED_EDGE ( 'NONE', *, *, #134427, .F. ) ;
#54533 = ORIENTED_EDGE ( 'NONE', *, *, #40467, .F. ) ;
#54534 = DIRECTION ( 'NONE',  ( 0.3543493200069162685, -0.000000000000000000, -0.9351131265310288487 ) ) ;
#54535 = DIRECTION ( 'NONE',  ( -0.3543493200069162685, -0.000000000000000000, -0.9351131265310288487 ) ) ;
#54536 = CARTESIAN_POINT ( 'NONE',  ( 45.48921356237309510, -27.52281430457087197, 5.000000000000000000 ) ) ;
#54537 = ORIENTED_EDGE ( 'NONE', *, *, #13794, .T. ) ;
#54538 = DIRECTION ( 'NONE',  ( -0.000000000000000000, -0.3543493200069152693, 0.9351131265310292928 ) ) ;
#54539 = EDGE_CURVE ( 'NONE', #39432, #59763, #42363, .T. ) ;
#54540 = VECTOR ( 'NONE', #79796, 1000.000000000000000 ) ;
#54541 = CARTESIAN_POINT ( 'NONE',  ( 1.180000000000000826, -6.391994993740215847, 6.750000000000000888 ) ) ;
#54542 = CARTESIAN_POINT ( 'NONE',  ( 14.94206980810188590, 7.934999999999993392, 2.126176841940951689 ) ) ;
#54543 = VECTOR ( 'NONE', #28930, 1000.000000000000000 ) ;
#54544 = DIRECTION ( 'NONE',  ( 1.000000000000000000, 0.000000000000000000, 0.000000000000000000 ) ) ;
#54545 = EDGE_LOOP ( 'NONE', ( #125056, #74122, #65238, #67233 ) ) ;
#54546 = CARTESIAN_POINT ( 'NONE',  ( 117.7454301918981230, -5.291415217122919401, -3.055000000000000604 ) ) ;
#54547 = AXIS2_PLACEMENT_3D ( 'NONE', #64115, #117738, #141682 ) ;
#54549 = EDGE_CURVE ( 'NONE', #7898, #4663, #131496, .T. ) ;
#54548 = PLANE ( 'NONE',  #41985 ) ;
#54550 = DIRECTION ( 'NONE',  ( 0.7071067811865487940, 0.7071067811865463515, 0.000000000000000000 ) ) ;
#54552 = VERTEX_POINT ( 'NONE', #132229 ) ;
#54551 = LINE ( 'NONE', #8137, #118967 ) ;
#54553 = LINE ( 'NONE', #10985, #78612 ) ;
#54554 = ORIENTED_EDGE ( 'NONE', *, *, #90285, .T. ) ;
#54555 = PRESENTATION_LAYER_ASSIGNMENT (  '', '', ( #128632 ) ) ;
#54556 = CARTESIAN_POINT ( 'NONE',  ( 76.20419371712955581, -6.884901960086285300, -3.975000000000000089 ) ) ;
#54557 = CARTESIAN_POINT ( 'NONE',  ( -5.994519915287488843, 28.92564299267942118, 4.000000000000000000 ) ) ;
#54558 = DIRECTION ( 'NONE',  ( -0.000000000000000000, 0.000000000000000000, 1.000000000000000000 ) ) ;
#54559 = EDGE_LOOP ( 'NONE', ( #54473, #129776, #15539, #123962, #112203 ) ) ;
#54560 = EDGE_CURVE ( 'NONE', #38115, #123554, #121316, .T. ) ;
#54561 = LINE ( 'NONE', #98049, #141415 ) ;
#54562 = CARTESIAN_POINT ( 'NONE',  ( -19.66071175273273752, -1.129697928112111116, -31.75000930624208451 ) ) ;
#54563 = VERTEX_POINT ( 'NONE', #66248 ) ;
#54564 = DIRECTION ( 'NONE',  ( 0.7071067811865487940, 0.7071067811865463515, 0.000000000000000000 ) ) ;
#54565 = CARTESIAN_POINT ( 'NONE',  ( -6.792893218813409462, 0.7592924766157086447, 5.000000000000000000 ) ) ;
#54566 = ORIENTED_EDGE ( 'NONE', *, *, #53462, .T. ) ;
#54567 = LINE ( 'NONE', #132128, #43795 ) ;
#54570 = EDGE_CURVE ( 'NONE', #9775, #10888, #140919, .T. ) ;
#54569 = ORIENTED_EDGE ( 'NONE', *, *, #2512, .F. ) ;
#54568 = DIRECTION ( 'NONE',  ( 0.7071067811865487940, 0.7071067811865463515, 0.000000000000000000 ) ) ;
#54571 = ORIENTED_EDGE ( 'NONE', *, *, #35830, .F. ) ;
#54572 = CARTESIAN_POINT ( 'NONE',  ( 17.51078643762690845, -27.52281430457043143, 5.000000000000000000 ) ) ;
#54573 = FACE_OUTER_BOUND ( 'NONE', #47897, .T. ) ;
#54574 = VERTEX_POINT ( 'NONE', #20562 ) ;
#54575 = CARTESIAN_POINT ( 'NONE',  ( 15.18398860626900237, 28.73617430169797871, 5.000000000000000000 ) ) ;
#54576 = DIRECTION ( 'NONE',  ( 0.000000000000000000, 0.000000000000000000, -1.000000000000000000 ) ) ;
#54577 = PLANE ( 'NONE',  #70039 ) ;
#54578 = ORIENTED_EDGE ( 'NONE', *, *, #138110, .F. ) ;
#54579 = DIRECTION ( 'NONE',  ( -0.7071067811865486830, -0.7071067811865464625, 0.000000000000000000 ) ) ;
#54580 = CARTESIAN_POINT ( 'NONE',  ( -21.18398860626899349, 28.73617430169802134, 5.000000000000000000 ) ) ;
#54581 = SURFACE_SIDE_STYLE ('',( #86493 ) ) ;
#54582 = CARTESIAN_POINT ( 'NONE',  ( 42.20376352523144448, 6.109999999999999432, 1.122388791418549108E-15 ) ) ;
#54583 = LINE ( 'NONE', #43688, #23358 ) ;
#54584 = EDGE_CURVE ( 'NONE', #13816, #52329, #98843, .T. ) ;
#54585 = ORIENTED_EDGE ( 'NONE', *, *, #1747, .F. ) ;
#54586 = ORIENTED_EDGE ( 'NONE', *, *, #95666, .T. ) ;
#54587 =( NAMED_UNIT ( * ) PLANE_ANGLE_UNIT ( ) SI_UNIT ( $, .RADIAN. ) );
#54588 = ADVANCED_FACE ( 'NONE', ( #10402 ), #8242, .F. ) ;
#54589 = VERTEX_POINT ( 'NONE', #32922 ) ;
#54590 = ORIENTED_EDGE ( 'NONE', *, *, #117441, .T. ) ;
#54591 = CARTESIAN_POINT ( 'NONE',  ( -17.99451991528748351, 28.92564299267950645, 4.000000000000000000 ) ) ;
#54592 = CARTESIAN_POINT ( 'NONE',  ( 20.51159235450331764, 3.061616997868380183E-16, -2.500000000000001332 ) ) ;
#54593 = EDGE_LOOP ( 'NONE', ( #140138, #141733, #107081, #143390 ) ) ;
#54594 = DIRECTION ( 'NONE',  ( 0.000000000000000000, 0.000000000000000000, -1.000000000000000000 ) ) ;
#54595 = DIRECTION ( 'NONE',  ( -0.6830127018922180770, -0.6830127018922204085, -0.2588190451025213501 ) ) ;
#54596 = EDGE_CURVE ( 'NONE', #18390, #128893, #53958, .T. ) ;
#54597 = DIRECTION ( 'NONE',  ( -0.6830127018922181881, 0.6830127018922202975, -0.2588190451025214056 ) ) ;
#54598 = CARTESIAN_POINT ( 'NONE',  ( 123.8129301918981184, -1.637169565754159617, -6.110000000000001208 ) ) ;
#54599 = ORIENTED_EDGE ( 'NONE', *, *, #103315, .F. ) ;
#54600 = EDGE_CURVE ( 'NONE', #64063, #54084, #77144, .T. ) ;
#54601 = CARTESIAN_POINT ( 'NONE',  ( -34.75611968250422024, 7.705650698523992759, 4.955485411084894487 ) ) ;
#54602 = DIRECTION ( 'NONE',  ( -0.6830127018922180770, -0.6830127018922204085, -0.2588190451025213501 ) ) ;
#54603 = FACE_OUTER_BOUND ( 'NONE', #106398, .T. ) ;
#54604 = CARTESIAN_POINT ( 'NONE',  ( -66.29974487139159578, -27.71228299555252406, 4.000000000000000000 ) ) ;
#54605 = LINE ( 'NONE', #98786, #83888 ) ;
#54606 = FACE_OUTER_BOUND ( 'NONE', #30982, .T. ) ;
#54607 = CARTESIAN_POINT ( 'NONE',  ( 60.89169371712955581, 2.130196079827421762, 7.950000000000001066 ) ) ;
#54608 = VECTOR ( 'NONE', #83084, 1000.000000000000227 ) ;
#54609 = CARTESIAN_POINT ( 'NONE',  ( 20.56494995367816614, -2.598550695876024275, 5.000000000000000000 ) ) ;
#54610 = DIRECTION ( 'NONE',  ( -1.000000000000000000, -0.000000000000000000, 0.000000000000000000 ) ) ;
#54611 = ORIENTED_EDGE ( 'NONE', *, *, #4033, .T. ) ;
#54612 = ORIENTED_EDGE ( 'NONE', *, *, #97689, .F. ) ;
#54613 = CARTESIAN_POINT ( 'NONE',  ( 44.02083333333333570, 7.949999999999999289, 2.130196079827431532 ) ) ;
#54614 = VECTOR ( 'NONE', #12539, 999.9999999999998863 ) ;
#54615 = CARTESIAN_POINT ( 'NONE',  ( 27.48921356237309155, -27.52281430457074762, 5.000000000000000000 ) ) ;
#54616 = PLANE ( 'NONE',  #34549 ) ;
#54617 = ORIENTED_EDGE ( 'NONE', *, *, #18015, .F. ) ;
#54618 = DIRECTION ( 'NONE',  ( 0.000000000000000000, -1.000000000000000000, 0.000000000000000000 ) ) ;
#54619 = EDGE_CURVE ( 'NONE', #142915, #114801, #52488, .T. ) ;
#54620 = CARTESIAN_POINT ( 'NONE',  ( -19.05000000000000071, 3.174999999999997158, 5.000000000000000000 ) ) ;
#54621 = CARTESIAN_POINT ( 'NONE',  ( 49.58376352523144703, -6.110000000000001208, -3.741295971395164515E-16 ) ) ;
#54622 = ORIENTED_EDGE ( 'NONE', *, *, #111222, .T. ) ;
#54623 = DIRECTION ( 'NONE',  ( -1.000000000000000000, 0.000000000000000000, 0.000000000000000000 ) ) ;
#54624 = ORIENTED_EDGE ( 'NONE', *, *, #39296, .F. ) ;
#54625 = EDGE_LOOP ( 'NONE', ( #87885, #85019, #90843, #84316 ) ) ;
#54626 = DIRECTION ( 'NONE',  ( -0.7071067811865486830, 0.7071067811865464625, 0.000000000000000000 ) ) ;
#54627 = CARTESIAN_POINT ( 'NONE',  ( 12.29974487139158512, -27.71228299555214747, 4.000000000000000000 ) ) ;
#54628 = PLANE ( 'NONE',  #4873 ) ;
#54629 = DIRECTION ( 'NONE',  ( 0.7071067811865487940, 0.7071067811865463515, 0.000000000000000000 ) ) ;
#54630 = ORIENTED_EDGE ( 'NONE', *, *, #18379, .T. ) ;
#54631 = DIRECTION ( 'NONE',  ( -0.000000000000000000, -0.3543493200069152693, 0.9351131265310292928 ) ) ;
#54633 = VERTEX_POINT ( 'NONE', #142383 ) ;
#54632 = DIRECTION ( 'NONE',  ( 0.000000000000000000, -1.000000000000000000, 0.000000000000000000 ) ) ;
#54634 = CARTESIAN_POINT ( 'NONE',  ( 78.60459685856477563, 1.637169565754164946, -6.109999999999999432 ) ) ;
#54635 = CARTESIAN_POINT ( 'NONE',  ( 14.14583333333333748, -1.633150327867709528, 6.094999999999979323 ) ) ;
#54636 =( NAMED_UNIT ( * ) PLANE_ANGLE_UNIT ( ) SI_UNIT ( $, .RADIAN. ) );
#54637 = PRESENTATION_STYLE_ASSIGNMENT (( #74240 ) ) ;
#54638 = FACE_OUTER_BOUND ( 'NONE', #103054, .T. ) ;
#54639 = AXIS2_PLACEMENT_3D ( 'NONE', #25723, #83717, #127921 ) ;
#54641 = EDGE_CURVE ( 'NONE', #57507, #82848, #43768, .T. ) ;
#54640 = AXIS2_PLACEMENT_3D ( 'NONE', #122717, #13223, #69081 ) ;
#54642 = ORIENTED_EDGE ( 'NONE', *, *, #141730, .T. ) ;
#54643 = CIRCLE ( 'NONE', #140035, 2.500000000000000444 ) ;
#54644 = CARTESIAN_POINT ( 'NONE',  ( -0.2997448713915885632, -27.71228299555206220, 4.000000000000000000 ) ) ;
#54645 = CARTESIAN_POINT ( 'NONE',  ( 65.97459685856479439, 1.637169565754164058, -6.109999999999996767 ) ) ;
#54646 = EDGE_CURVE ( 'NONE', #37506, #13547, #21996, .T. ) ;
#54647 = VECTOR ( 'NONE', #74775, 1000.000000000000227 ) ;
#54648 = CARTESIAN_POINT ( 'NONE',  ( -8.277185695429338352, -21.72500000000000142, 5.000000000000000000 ) ) ;
#54649 = DIRECTION ( 'NONE',  ( 0.7071067811865487940, 0.7071067811865463515, 0.000000000000000000 ) ) ;
#54650 = CARTESIAN_POINT ( 'NONE',  ( 9.328169399223463998, -9.740707523384180888, 4.000000000000000000 ) ) ;
#54651 = ORIENTED_EDGE ( 'NONE', *, *, #94554, .T. ) ;
#54652 = VERTEX_POINT ( 'NONE', #11094 ) ;
#54653 = CIRCLE ( 'NONE', #135671, 0.5000000000000000000 ) ;
#54654 = CARTESIAN_POINT ( 'NONE',  ( 11.15159235450332176, -2.500000000000000444, 3.061616997868384620E-16 ) ) ;
#54655 = CARTESIAN_POINT ( 'NONE',  ( 17.02886364525924989, -2.441401769420105339, 4.000000000000000000 ) ) ;
#54656 = ORIENTED_EDGE ( 'NONE', *, *, #53732, .F. ) ;
#54657 = EDGE_CURVE ( 'NONE', #16746, #143518, #97402, .T. ) ;
#54658 = EDGE_CURVE ( 'NONE', #33564, #92017, #19858, .T. ) ;
#54659 = ORIENTED_EDGE ( 'NONE', *, *, #23459, .F. ) ;
#54660 = DIRECTION ( 'NONE',  ( -0.3543493200069162685, -0.000000000000000000, -0.9351131265310288487 ) ) ;
#54661 = ORIENTED_EDGE ( 'NONE', *, *, #44972, .T. ) ;
#54662 = CARTESIAN_POINT ( 'NONE',  ( 26.91508676806222411, -12.74070752338414536, 18.74364270924360198 ) ) ;
#54663 = LINE ( 'NONE', #98846, #13195 ) ;
#54664 = CARTESIAN_POINT ( 'NONE',  ( 20.68342038867197630, -6.740707523384219968, 11.88629033278119174 ) ) ;
#54665 = ADVANCED_FACE ( 'NONE', ( #99546 ), #30769, .T. ) ;
#54666 = FACE_BOUND ( 'NONE', #95170, .T. ) ;
#54667 = EDGE_CURVE ( 'NONE', #20647, #121702, #132952, .T. ) ;
#54668 = CARTESIAN_POINT ( 'NONE',  ( 25.04515773336651208, -21.74070752338405654, 21.72585301388590295 ) ) ;
#54669 = CARTESIAN_POINT ( 'NONE',  ( 41.20419371712954870, -6.884901960086285300, -3.975000000000000089 ) ) ;
#54670 = DIRECTION ( 'NONE',  ( -0.000000000000000000, 0.3543493200069153248, 0.9351131265310292928 ) ) ;
#54672 = VERTEX_POINT ( 'NONE', #108261 ) ;
#54671 = DIRECTION ( 'NONE',  ( 3.469446951953611033E-15, 0.000000000000000000, 1.000000000000000000 ) ) ;
#54673 = CARTESIAN_POINT ( 'NONE',  ( 75.48921356237309510, -27.52281430457107803, 5.000000000000000000 ) ) ;
#54675 = EDGE_CURVE ( 'NONE', #98477, #53957, #90759, .T. ) ;
#54674 = CONTEXT_DEPENDENT_SHAPE_REPRESENTATION ( #25373, #19223 ) ;
#54676 = ORIENTED_EDGE ( 'NONE', *, *, #14808, .F. ) ;
#54677 = EDGE_LOOP ( 'NONE', ( #8446, #3847, #37235, #57498 ) ) ;
#54678 = CARTESIAN_POINT ( 'NONE',  ( 77.78709685856478018, 3.054999999999997495, 5.291415217122919401 ) ) ;
#54679 = VERTEX_POINT ( 'NONE', #3779 ) ;
#54680 = LINE ( 'NONE', #45950, #59218 ) ;
#54681 = CARTESIAN_POINT ( 'NONE',  ( 11.30840764549667554, 9.139736423841732040E-16, 0.000000000000000000 ) ) ;
#54682 = ORIENTED_EDGE ( 'NONE', *, *, #78201, .T. ) ;
#54683 = DIRECTION ( 'NONE',  ( 0.7071067811865486830, -0.7071067811865464625, -0.000000000000000000 ) ) ;
#54684 = ADVANCED_FACE ( 'NONE', ( #113286 ), #90862, .F. ) ;
#54685 = CARTESIAN_POINT ( 'NONE',  ( -11.81601139373100651, 28.73617430169779041, 5.000000000000000000 ) ) ;
#54686 = DIRECTION ( 'NONE',  ( 0.7071067811865487940, 0.7071067811865463515, 0.000000000000000000 ) ) ;
#54687 = DIRECTION ( 'NONE',  ( 0.7071067811865487940, 0.7071067811865463515, 0.000000000000000000 ) ) ;
#54688 = DIRECTION ( 'NONE',  ( -0.6830127018922180770, -0.6830127018922204085, -0.2588190451025213501 ) ) ;
#54689 = CARTESIAN_POINT ( 'NONE',  ( -4.499999999999966249, -10.53360074219763298, 5.000000000000000000 ) ) ;
#54690 = CARTESIAN_POINT ( 'NONE',  ( -14.81601139373099585, 28.73617430169776910, 5.000000000000000000 ) ) ;
#54691 = CARTESIAN_POINT ( 'NONE',  ( 60.18398860626900415, 28.73617430169829490, 5.000000000000000000 ) ) ;
#54692 = VERTEX_POINT ( 'NONE', #100297 ) ;
#54693 = EDGE_CURVE ( 'NONE', #129495, #55173, #80692, .T. ) ;
#54694 = DIRECTION ( 'NONE',  ( 0.000000000000000000, -0.000000000000000000, -1.000000000000000000 ) ) ;
#54695 = EDGE_LOOP ( 'NONE', ( #100534, #63410, #42478, #12314 ) ) ;
#54696 = CARTESIAN_POINT ( 'NONE',  ( 26.29289321881327623, 5.259292476615663681, 5.000000000000000000 ) ) ;
#54697 =( BOUNDED_CURVE ( )  B_SPLINE_CURVE ( 3, ( #28632, #61975, #117038, #17704 ),
 .UNSPECIFIED., .F., .T. ) 
 B_SPLINE_CURVE_WITH_KNOTS ( ( 4, 4 ),
 ( 2.779374508378133601, 4.199602562396782091 ),
 .UNSPECIFIED. ) 
 CURVE ( )  GEOMETRIC_REPRESENTATION_ITEM ( )  RATIONAL_B_SPLINE_CURVE ( ( 1.000000000000000000, 0.8388583629366748173, 0.8388583629366748173, 1.000000000000000000 ) ) 
 REPRESENTATION_ITEM ( '' )  );
#54698 = DIRECTION ( 'NONE',  ( 0.7071067811865486830, -0.7071067811865464625, -0.000000000000000000 ) ) ;
#54699 = VERTEX_POINT ( 'NONE', #135095 ) ;
#54700 = ORIENTED_EDGE ( 'NONE', *, *, #71175, .F. ) ;
#54701 = EDGE_CURVE ( 'NONE', #27623, #39127, #56829, .T. ) ;
#54702 = CARTESIAN_POINT ( 'NONE',  ( 38.50043019189809712, -3.055000000000002380, 5.291415217122920289 ) ) ;
#54703 = EDGE_CURVE ( 'NONE', #72776, #97358, #73119, .T. ) ;
#54704 = ORIENTED_EDGE ( 'NONE', *, *, #33903, .T. ) ;
#54705 = CARTESIAN_POINT ( 'NONE',  ( 2.000000000000008882, 0.000000000000000000, 0.000000000000000000 ) ) ;
#54706 = ADVANCED_FACE ( 'NONE', ( #123502 ), #3103, .F. ) ;
#54707 = AXIS2_PLACEMENT_3D ( 'NONE', #116358, #38803, #137406 ) ;
#54708 = CYLINDRICAL_SURFACE ( 'NONE', #70160, 1.000000000000000888 ) ;
#54709 = CARTESIAN_POINT ( 'NONE',  ( 27.17080628287044064, -3.047499999999997211, -5.278424836066143655 ) ) ;
#54710 = CARTESIAN_POINT ( 'NONE',  ( 9.971754739210105356, 9.503873597802957818, -27.24537889701776905 ) ) ;
#54711 = ORIENTED_EDGE ( 'NONE', *, *, #99595, .F. ) ;
#54712 = AXIS2_PLACEMENT_3D ( 'NONE', #26642, #49851, #71588 ) ;
#54713 = CARTESIAN_POINT ( 'NONE',  ( -5.671830600776434750, 5.259292476615662792, 4.000000000000000000 ) ) ;
#54714 = ORIENTED_EDGE ( 'NONE', *, *, #135034, .F. ) ;
#54715 = DIRECTION ( 'NONE',  ( 0.000000000000000000, -1.000000000000000000, 0.000000000000000000 ) ) ;
#54716 = DIRECTION ( 'NONE',  ( -0.7071067811865486830, 0.7071067811865464625, 0.000000000000000000 ) ) ;
#54718 = ORIENTED_EDGE ( 'NONE', *, *, #36069, .T. ) ;
#54717 = CARTESIAN_POINT ( 'NONE',  ( 23.99451991528749062, 28.92564299267954908, 4.000000000000000000 ) ) ;
#54719 = ORIENTED_EDGE ( 'NONE', *, *, #28322, .F. ) ;
#54720 = LINE ( 'NONE', #94084, #5560 ) ;
#54721 = CARTESIAN_POINT ( 'NONE',  ( 31.49999999999977973, 10.08746187583915344, 4.000000000000000000 ) ) ;
#54722 = DIRECTION ( 'NONE',  ( 0.7071067811865487940, -0.7071067811865463515, 0.000000000000000000 ) ) ;
#54723 = VERTEX_POINT ( 'NONE', #134359 ) ;
#54724 = LINE ( 'NONE', #43131, #143080 ) ;
#54725 = ORIENTED_EDGE ( 'NONE', *, *, #72173, .F. ) ;
#54726 = ORIENTED_EDGE ( 'NONE', *, *, #52543, .F. ) ;
#54727 = ADVANCED_FACE ( 'NONE', ( #35785 ), #35057, .F. ) ;
#54728 = DIRECTION ( 'NONE',  ( -0.000000000000000000, 0.3543493200069153248, 0.9351131265310292928 ) ) ;
#54729 = CARTESIAN_POINT ( 'NONE',  ( -23.67183060077630685, 14.25929247661557397, 4.000000000000000000 ) ) ;
#54730 = DIRECTION ( 'NONE',  ( 0.7071067811865486830, -0.7071067811865464625, -0.000000000000000000 ) ) ;
#54731 = CARTESIAN_POINT ( 'NONE',  ( -34.92500000000001137, 21.72500000000000142, 4.165035510187084178 ) ) ;
#54732 = LINE ( 'NONE', #41698, #109885 ) ;
#54733 = VECTOR ( 'NONE', #8558, 1000.000000000000000 ) ;
#54734 = LINE ( 'NONE', #76493, #66875 ) ;
#54736 = EDGE_CURVE ( 'NONE', #33185, #93058, #45233, .T. ) ;
#54735 = ORIENTED_EDGE ( 'NONE', *, *, #51404, .F. ) ;
#54737 = CARTESIAN_POINT ( 'NONE',  ( 96.32919371712955581, -3.975000000000001865, 6.884901960086284411 ) ) ;
#54738 = VERTEX_POINT ( 'NONE', #135773 ) ;
#54739 = DIRECTION ( 'NONE',  ( 0.000000000000000000, 1.000000000000000000, 0.000000000000000000 ) ) ;
#54740 = VECTOR ( 'NONE', #74239, 1000.000000000000000 ) ;
#54741 = VECTOR ( 'NONE', #80856, 1000.000000000000000 ) ;
#54742 = DIRECTION ( 'NONE',  ( 0.6830127018922181881, 0.6830127018922202975, -0.2588190451025214056 ) ) ;
#54743 = DIRECTION ( 'NONE',  ( 0.000000000000000000, 1.000000000000000000, 0.000000000000000000 ) ) ;
#54744 = VECTOR ( 'NONE', #71765, 1000.000000000000000 ) ;
#54745 = EDGE_LOOP ( 'NONE', ( #80390, #57710, #115265 ) ) ;
#54746 = CARTESIAN_POINT ( 'NONE',  ( 16.45742106731621135, 0.9613713492673626737, -33.49048331797055766 ) ) ;
#54747 = CARTESIAN_POINT ( 'NONE',  ( -11.67183060077639567, 8.259292476615641476, 4.000000000000000000 ) ) ;
#54748 = VERTEX_POINT ( 'NONE', #34316 ) ;
#54749 = ORIENTED_EDGE ( 'NONE', *, *, #130710, .F. ) ;
#54750 = DIRECTION ( 'NONE',  ( -0.000000000000000000, 0.000000000000000000, 1.000000000000000000 ) ) ;
#54751 = CARTESIAN_POINT ( 'NONE',  ( 0.000000000000000000, 0.000000000000000000, 5.000000000000000000 ) ) ;
#54752 = EDGE_CURVE ( 'NONE', #45511, #41681, #36463, .T. ) ;
#54753 = CARTESIAN_POINT ( 'NONE',  ( 17.54840764549667398, 9.139736423841732040E-16, 0.000000000000000000 ) ) ;
#54754 = CARTESIAN_POINT ( 'NONE',  ( 52.91666666666666430, -6.884901960086287076, -3.975000000000000977 ) ) ;
#54755 = CARTESIAN_POINT ( 'NONE',  ( -27.32816939922333077, 2.259292476615697876, 4.000000000000000000 ) ) ;
#54756 = CARTESIAN_POINT ( 'NONE',  ( 69.76626352523143737, 4.472830434245839371, -4.472830434245839371 ) ) ;
#54757 = DIRECTION ( 'NONE',  ( 0.7071067811865487940, 0.7071067811865463515, -0.000000000000000000 ) ) ;
#54758 = CARTESIAN_POINT ( 'NONE',  ( -12.20000000000000817, -1.670812611072399357E-15, 0.000000000000000000 ) ) ;
#54759 = CARTESIAN_POINT ( 'NONE',  ( -66.29974487139159578, -27.71228299555252406, 4.000000000000000000 ) ) ;
#54760 = DIRECTION ( 'NONE',  ( -0.000000000000000000, 0.3543493200069153248, 0.9351131265310292928 ) ) ;
#54761 = EDGE_CURVE ( 'NONE', #86742, #83926, #124893, .T. ) ;
#54762 = ORIENTED_EDGE ( 'NONE', *, *, #71866, .F. ) ;
#54763 = LINE ( 'NONE', #130180, #134524 ) ;
#54764 = ORIENTED_EDGE ( 'NONE', *, *, #136019, .F. ) ;
#54765 = CARTESIAN_POINT ( 'NONE',  ( 20.20519093902540320, 4.584330080086930965E-16, 0.000000000000000000 ) ) ;
#54766 = CARTESIAN_POINT ( 'NONE',  ( -34.49999999999975842, 21.05432934483072671, 4.994342998332167660 ) ) ;
#54767 = DIRECTION ( 'NONE',  ( 0.000000000000000000, 0.000000000000000000, 1.000000000000000000 ) ) ;
#54768 = DIRECTION ( 'NONE',  ( -0.000000000000000000, 0.3543493200069153248, 0.9351131265310292928 ) ) ;
#54769 = LINE ( 'NONE', #1052, #57896 ) ;
#54770 = ADVANCED_FACE ( 'NONE', ( #57520 ), #25567, .F. ) ;
#54771 = DIRECTION ( 'NONE',  ( 0.7071067811865487940, 0.7071067811865463515, -0.000000000000000000 ) ) ;
#54772 = DIRECTION ( 'NONE',  ( 0.000000000000000000, 0.000000000000000000, 1.000000000000000000 ) ) ;
#54773 = ORIENTED_EDGE ( 'NONE', *, *, #16315, .F. ) ;
#54774 = ADVANCED_FACE ( 'NONE', ( #67700 ), #4467, .F. ) ;
#54775 = VERTEX_POINT ( 'NONE', #6624 ) ;
#54776 = CARTESIAN_POINT ( 'NONE',  ( 32.99999999999976552, 7.931123077392109977, 4.000000000000000000 ) ) ;
#54777 =( NAMED_UNIT ( * ) PLANE_ANGLE_UNIT ( ) SI_UNIT ( $, .RADIAN. ) );
#54778 = UNCERTAINTY_MEASURE_WITH_UNIT (LENGTH_MEASURE( 1.000000000000000082E-05 ), #16091, 'distance_accuracy_value', 'NONE');
#54779 = CARTESIAN_POINT ( 'NONE',  ( 6.436801032208253837, -12.74070752338415247, 9.898150129686360543 ) ) ;
#54780 = LINE ( 'NONE', #98957, #41136 ) ;
#54781 = CARTESIAN_POINT ( 'NONE',  ( 82.91252705046289861, -7.949999999999998401, -4.867971026610728450E-16 ) ) ;
#54782 = CARTESIAN_POINT ( 'NONE',  ( -34.92500000000001137, -10.19990548397269059, 4.759050581649336920 ) ) ;
#54783 = VECTOR ( 'NONE', #74518, 1000.000000000000000 ) ;
#54784 = CARTESIAN_POINT ( 'NONE',  ( -32.95560648933506798, 22.22500000000000142, 5.746276820986322420 ) ) ;
#54785 = ORIENTED_EDGE ( 'NONE', *, *, #46483, .T. ) ;
#54786 = CARTESIAN_POINT ( 'NONE',  ( 81.49999999999998579, 0.000000000000000000, -7.950000000000000178 ) ) ;
#54787 = EDGE_CURVE ( 'NONE', #46869, #115536, #18228, .T. ) ;
#54788 = CARTESIAN_POINT ( 'NONE',  ( 0.000000000000000000, 0.000000000000000000, 5.000000000000000000 ) ) ;
#54789 = LINE ( 'NONE', #109862, #71626 ) ;
#54790 = DIRECTION ( 'NONE',  ( 0.000000000000000000, 0.000000000000000000, 1.000000000000000000 ) ) ;
#54791 = VECTOR ( 'NONE', #93485, 1000.000000000000000 ) ;
#54792 = ORIENTED_EDGE ( 'NONE', *, *, #512, .T. ) ;
#54793 = EDGE_CURVE ( 'NONE', #103321, #89661, #16084, .T. ) ;
#54794 = CARTESIAN_POINT ( 'NONE',  ( -27.18398860626900060, 28.73617430169806042, 5.000000000000000000 ) ) ;
#54795 = ORIENTED_EDGE ( 'NONE', *, *, #49969, .F. ) ;
#54796 = CARTESIAN_POINT ( 'NONE',  ( 55.45418156660451103, -52.10373894832327579, -40.45955814675560447 ) ) ;
#54797 = CARTESIAN_POINT ( 'NONE',  ( 76.85459685856477563, -1.637169565754161615, 6.110000000000000320 ) ) ;
#54798 = CARTESIAN_POINT ( 'NONE',  ( 18.79289321881332953, -20.24070752338407431, 5.000000000000000000 ) ) ;
#54799 = EDGE_LOOP ( 'NONE', ( #33127, #61181, #66740 ) ) ;
#54800 = DIRECTION ( 'NONE',  ( -1.000000000000000000, 0.000000000000000000, -0.000000000000000000 ) ) ;
#54801 = CARTESIAN_POINT ( 'NONE',  ( -9.299744871391588674, -27.71228299555212971, 4.000000000000000000 ) ) ;
#54802 = PLANE ( 'NONE',  #115938 ) ;
#54803 = DIRECTION ( 'NONE',  ( -0.7071067811865486830, -0.7071067811865464625, -0.000000000000000000 ) ) ;
#54804 = FACE_OUTER_BOUND ( 'NONE', #17936, .T. ) ;
#54806 = ORIENTED_EDGE ( 'NONE', *, *, #101794, .F. ) ;
#54805 = PLANE ( 'NONE',  #98468 ) ;
#54807 = DIRECTION ( 'NONE',  ( 0.7071067811865487940, 0.7071067811865463515, -0.000000000000000000 ) ) ;
#54808 = DIRECTION ( 'NONE',  ( 0.7071067811865487940, 0.7071067811865463515, 0.000000000000000000 ) ) ;
#54809 = DIRECTION ( 'NONE',  ( 0.3543493200069162685, -0.000000000000000000, -0.9351131265310288487 ) ) ;
#54810 = DIRECTION ( 'NONE',  ( 0.7071067811865487940, 0.7071067811865463515, 0.000000000000000000 ) ) ;
#54811 = ORIENTED_EDGE ( 'NONE', *, *, #142379, .F. ) ;
#54812 = VECTOR ( 'NONE', #53049, 1000.000000000000000 ) ;
#54813 = EDGE_LOOP ( 'NONE', ( #39547, #86065, #75557, #107284 ) ) ;
#54814 = CARTESIAN_POINT ( 'NONE',  ( 66.35459685856476142, -1.637169565754161615, 6.110000000000000320 ) ) ;
#54815 = EDGE_CURVE ( 'NONE', #138021, #86498, #7368, .T. ) ;
#54816 = ORIENTED_EDGE ( 'NONE', *, *, #19179, .T. ) ;
#54817 = AXIS2_PLACEMENT_3D ( 'NONE', #25028, #113464, #36624 ) ;
#54818 = PLANE ( 'NONE',  #93903 ) ;
#54819 = EDGE_CURVE ( 'NONE', #12889, #94959, #62509, .T. ) ;
#54820 = FACE_OUTER_BOUND ( 'NONE', #62268, .T. ) ;
#54821 = CARTESIAN_POINT ( 'NONE',  ( 125.3500270504628844, -5.819803920172573086, -5.819803920172573086 ) ) ;
#54822 = FACE_OUTER_BOUND ( 'NONE', #91215, .T. ) ;
#54823 = EDGE_LOOP ( 'NONE', ( #126469, #82650, #99852, #41320 ) ) ;
#54824 = ORIENTED_EDGE ( 'NONE', *, *, #14548, .T. ) ;
#54825 = DIRECTION ( 'NONE',  ( -0.000000000000000000, 0.000000000000000000, 1.000000000000000000 ) ) ;
#54826 = FILL_AREA_STYLE_COLOUR ( '', #113784 ) ;
#54827 = ADVANCED_FACE ( 'NONE', ( #39330 ), #127013, .F. ) ;
#54828 = ADVANCED_FACE ( 'NONE', ( #84279 ), #42216, .T. ) ;
#54829 = ORIENTED_EDGE ( 'NONE', *, *, #26658, .F. ) ;
#54830 = FACE_OUTER_BOUND ( 'NONE', #110258, .T. ) ;
#54831 = DIRECTION ( 'NONE',  ( 1.000000000000000000, 0.000000000000000000, 0.000000000000000000 ) ) ;
#54832 = DIRECTION ( 'NONE',  ( -0.7071067811865487940, 0.7071067811865463515, -0.000000000000000000 ) ) ;
#54833 = EDGE_CURVE ( 'NONE', #77128, #88053, #83553, .T. ) ;
#54834 = ORIENTED_EDGE ( 'NONE', *, *, #4622, .F. ) ;
#54835 = VECTOR ( 'NONE', #38763, 1000.000000000000227 ) ;
#54836 = EDGE_CURVE ( 'NONE', #119600, #100283, #55769, .T. ) ;
#54837 = FACE_BOUND ( 'NONE', #80564, .T. ) ;
#54838 = ADVANCED_FACE ( 'NONE', ( #28451 ), #70561, .T. ) ;
#54839 = CARTESIAN_POINT ( 'NONE',  ( 180.8041599634935608, -49.02495722182848681, 39.69341335395905190 ) ) ;
#54840 = DIRECTION ( 'NONE',  ( 1.000000000000000000, 1.224606353822377258E-16, 0.000000000000000000 ) ) ;
#54841 = DIRECTION ( 'NONE',  ( -0.7071067811865486830, -0.7071067811865464625, 0.000000000000000000 ) ) ;
#54842 = VECTOR ( 'NONE', #40048, 1000.000000000000000 ) ;
#54843 = CIRCLE ( 'NONE', #135858, 2.500000000000000888 ) ;
#54844 = DIRECTION ( 'NONE',  ( -0.000000000000000000, 0.000000000000000000, 1.000000000000000000 ) ) ;
#54845 =( NAMED_UNIT ( * ) PLANE_ANGLE_UNIT ( ) SI_UNIT ( $, .RADIAN. ) );
#54846 = ORIENTED_EDGE ( 'NONE', *, *, #122528, .T. ) ;
#54847 = AXIS2_PLACEMENT_3D ( 'NONE', #10362, #12512, #67660 ) ;
#54848 = EDGE_CURVE ( 'NONE', #7244, #135518, #68036, .T. ) ;
#54849 = EDGE_LOOP ( 'NONE', ( #105544, #56234, #11577, #135241 ) ) ;
#54850 = CARTESIAN_POINT ( 'NONE',  ( 116.7245968585647802, -1.637169565754160949, 6.109999999999997655 ) ) ;
#54851 = ORIENTED_EDGE ( 'NONE', *, *, #135510, .F. ) ;
#54852 = ADVANCED_FACE ( 'NONE', ( #37168 ), #103814, .F. ) ;
#54853 = ORIENTED_EDGE ( 'NONE', *, *, #43450, .F. ) ;
#54854 = VECTOR ( 'NONE', #7512, 1000.000000000000000 ) ;
#54855 = DIRECTION ( 'NONE',  ( -0.7071067811865486830, -0.7071067811865464625, 0.000000000000000000 ) ) ;
#54856 = EDGE_CURVE ( 'NONE', #45976, #142614, #49516, .T. ) ;
#54857 = LINE ( 'NONE', #19353, #66316 ) ;
#54858 = CARTESIAN_POINT ( 'NONE',  ( -69.18398860626899705, 28.73617430169835529, 5.000000000000000000 ) ) ;
#54859 = ORIENTED_EDGE ( 'NONE', *, *, #18719, .T. ) ;
#54860 = CARTESIAN_POINT ( 'NONE',  ( 68.76669371712957002, -7.949999999999998401, 2.130196079827423983 ) ) ;
#54861 = PLANE ( 'NONE',  #33406 ) ;
#54862 = CARTESIAN_POINT ( 'NONE',  ( 37.74999999999999289, -9.735942053221458872E-16, 7.950000000000000178 ) ) ;
#54864 = FACE_OUTER_BOUND ( 'NONE', #115759, .T. ) ;
#54863 = CARTESIAN_POINT ( 'NONE',  ( -32.99999999999976552, -16.60178936734451582, 0.8616154019346735637 ) ) ;
#54865 = DIRECTION ( 'NONE',  ( -0.7071067811865486830, -0.7071067811865464625, 0.000000000000000000 ) ) ;
#54866 = ADVANCED_FACE ( 'NONE', ( #60380 ), #94392, .F. ) ;
#54867 = CARTESIAN_POINT ( 'NONE',  ( 32.99451991528749062, 28.92564299267960948, 4.000000000000000000 ) ) ;
#54868 = VERTEX_POINT ( 'NONE', #140072 ) ;
#54869 = DIRECTION ( 'NONE',  ( -0.7071067811865486830, -0.7071067811865464625, 0.000000000000000000 ) ) ;
#54870 = CARTESIAN_POINT ( 'NONE',  ( -12.46160355370563799, -9.740707523384173783, 17.74957260769608069 ) ) ;
#54871 = ORIENTED_EDGE ( 'NONE', *, *, #63681, .T. ) ;
#54872 = ORIENTED_EDGE ( 'NONE', *, *, #17739, .F. ) ;
#54873 = ORIENTED_EDGE ( 'NONE', *, *, #103611, .T. ) ;
#54874 = CARTESIAN_POINT ( 'NONE',  ( 67.22959685856476142, -6.110000000000000320, -1.637169565754161393 ) ) ;
#54876 = EDGE_CURVE ( 'NONE', #89916, #89397, #129887, .T. ) ;
#54875 = AXIS2_PLACEMENT_3D ( 'NONE', #49895, #69506, #47768 ) ;
#54877 = ORIENTED_EDGE ( 'NONE', *, *, #12746, .F. ) ;
#54878 =( BOUNDED_CURVE ( )  B_SPLINE_CURVE ( 2, ( #81872, #51357, #38332, #126065, #28884, #73121, #6352, #26731, #49936, #82548, #126735, #84008, #104998 ),
 .UNSPECIFIED., .F., .T. ) 
 B_SPLINE_CURVE_WITH_KNOTS ( ( 3, 2, 2, 2, 2, 2, 3 ),
 ( 0.5000000000000000000, 0.5027777777777777679, 0.5055555555555555358, 0.5083333333333333037, 0.5111111111111110716, 0.5138888888888888395, 0.5166666666666667185 ),
 .UNSPECIFIED. ) 
 CURVE ( )  GEOMETRIC_REPRESENTATION_ITEM ( )  RATIONAL_B_SPLINE_CURVE ( ( 1.000000000000000000, 0.9659258262890683122, 1.000000000000000000, 0.9659258262890683122, 1.000000000000000000, 0.9659258262890683122, 1.000000000000000000, 0.9659258262890683122, 1.000000000000000000, 0.9659258262890683122, 1.000000000000000000, 0.9659258262890683122, 1.000000000000000000 ) ) 
 REPRESENTATION_ITEM ( '' )  );
#54879 = CARTESIAN_POINT ( 'NONE',  ( -7.499999999999951150, 5.696342897626497148, -7.587980461218414518 ) ) ;
#54880 = ADVANCED_FACE ( 'NONE', ( #54490 ), #21113, .F. ) ;
#54881 = VECTOR ( 'NONE', #12708, 1000.000000000000000 ) ;
#54882 = SURFACE_STYLE_FILL_AREA ( #32408 ) ;
#54883 = CARTESIAN_POINT ( 'NONE',  ( 100.6254301918981042, 5.291415217122919401, 3.055000000000002824 ) ) ;
#54884 = CARTESIAN_POINT ( 'NONE',  ( 20.99451991528748707, 28.92564299267952777, 4.000000000000000000 ) ) ;
#54885 = VERTEX_POINT ( 'NONE', #42186 ) ;
#54886 = CARTESIAN_POINT ( 'NONE',  ( -69.18398860626899705, 28.73617430169835529, 5.000000000000000000 ) ) ;
#54887 = AXIS2_PLACEMENT_3D ( 'NONE', #78622, #90196, #122103 ) ;
#54888 = ADVANCED_FACE ( 'NONE', ( #41436 ), #131315, .F. ) ;
#54889 = FACE_OUTER_BOUND ( 'NONE', #105634, .T. ) ;
#54890 = CARTESIAN_POINT ( 'NONE',  ( 92.00000000000000000, 0.000000000000000000, -7.950000000000000178 ) ) ;
#54891 = DIRECTION ( 'NONE',  ( -0.3543493200069163240, 0.000000000000000000, -0.9351131265310288487 ) ) ;
#54892 = ORIENTED_EDGE ( 'NONE', *, *, #56191, .F. ) ;
#54893 = SURFACE_SIDE_STYLE ('',( #127429 ) ) ;
#54894 = ORIENTED_EDGE ( 'NONE', *, *, #4204, .T. ) ;
#54895 = EDGE_LOOP ( 'NONE', ( #102844, #77550, #48683, #134276 ) ) ;
#54896 = ORIENTED_EDGE ( 'NONE', *, *, #56539, .F. ) ;
#54898 = VECTOR ( 'NONE', #61739, 1000.000000000000000 ) ;
#54897 = CARTESIAN_POINT ( 'NONE',  ( 126.0579301918981230, 6.110000000000000320, -1.637169565754156064 ) ) ;
#54899 = VERTEX_POINT ( 'NONE', #74824 ) ;
#54900 = CARTESIAN_POINT ( 'NONE',  ( 60.18398860626900415, 28.73617430169829490, 5.000000000000000000 ) ) ;
#54901 = VECTOR ( 'NONE', #105965, 1000.000000000000000 ) ;
#54902 = CARTESIAN_POINT ( 'NONE',  ( -2.816011393730999401, 28.73617430169785436, 5.000000000000000000 ) ) ;
#54903 = VERTEX_POINT ( 'NONE', #66078 ) ;
#54904 = CARTESIAN_POINT ( 'NONE',  ( 13.29826936130429260, 3.821174125832445049E-16, 0.000000000000000000 ) ) ;
#54905 = LINE ( 'NONE', #9941, #104416 ) ;
#54906 = ORIENTED_EDGE ( 'NONE', *, *, #111600, .F. ) ;
#54907 = CARTESIAN_POINT ( 'NONE',  ( 10.47873647476855119, -5.808823158059033709, 5.808823158059035485 ) ) ;
#54908 = CARTESIAN_POINT ( 'NONE',  ( 15.18398860626900237, 28.73617430169797871, 5.000000000000000000 ) ) ;
#54909 = CARTESIAN_POINT ( 'NONE',  ( 20.99451991528748707, 28.92564299267952777, 4.000000000000000000 ) ) ;
#54910 = VECTOR ( 'NONE', #49521, 999.9999999999998863 ) ;
#54911 = DIRECTION ( 'NONE',  ( 0.000000000000000000, 0.000000000000000000, -1.000000000000000000 ) ) ;
#54912 = VERTEX_POINT ( 'NONE', #130628 ) ;
#54913 = VERTEX_POINT ( 'NONE', #29838 ) ;
#54914 = EDGE_CURVE ( 'NONE', #111735, #19820, #31997, .T. ) ;
#54915 = EDGE_LOOP ( 'NONE', ( #37940, #27040, #101141, #89871, #19210 ) ) ;
#54916 =( LENGTH_UNIT ( ) NAMED_UNIT ( * ) SI_UNIT ( .MILLI., .METRE. ) );
#54917 = FACE_OUTER_BOUND ( 'NONE', #10398, .T. ) ;
#54918 = UNCERTAINTY_MEASURE_WITH_UNIT (LENGTH_MEASURE( 1.000000000000000082E-05 ), #50873, 'distance_accuracy_value', 'NONE');
#54919 = CARTESIAN_POINT ( 'NONE',  ( -30.48921356237309510, -27.52281430457076894, 5.000000000000000000 ) ) ;
#54920 = CARTESIAN_POINT ( 'NONE',  ( 7.499999999999947597, 21.43112307739195899, 4.000000000000000000 ) ) ;
#54921 = DIRECTION ( 'NONE',  ( 0.000000000000000000, -1.000000000000000000, 0.000000000000000000 ) ) ;
#54922 = CARTESIAN_POINT ( 'NONE',  ( 30.33376352523143993, 6.110000000000001208, 1.122388791418549305E-15 ) ) ;
#54923 = DIRECTION ( 'NONE',  ( 0.7071067811865487940, 0.7071067811865463515, -0.000000000000000000 ) ) ;
#54924 = LINE ( 'NONE', #100568, #4921 ) ;
#54925 = VERTEX_POINT ( 'NONE', #121134 ) ;
#54926 = CARTESIAN_POINT ( 'NONE',  ( -22.17183060077631396, -8.240707523384200428, 4.000000000000000000 ) ) ;
#54927 = ORIENTED_EDGE ( 'NONE', *, *, #36454, .T. ) ;
#54928 = CARTESIAN_POINT ( 'NONE',  ( 128.8886022459138019, 0.000000000000000000, -6.349999999999997868 ) ) ;
#54929 = ORIENTED_EDGE ( 'NONE', *, *, #9064, .T. ) ;
#54930 = DIRECTION ( 'NONE',  ( -0.000000000000000000, -0.3543493200069152693, 0.9351131265310292928 ) ) ;
#54932 = ORIENTED_EDGE ( 'NONE', *, *, #16812, .T. ) ;
#54931 = PLANE ( 'NONE',  #7041 ) ;
#54933 = VECTOR ( 'NONE', #116678, 1000.000000000000000 ) ;
#54934 = EDGE_CURVE ( 'NONE', #81122, #99547, #81556, .T. ) ;
#54935 = DIRECTION ( 'NONE',  ( 0.6830127018922181881, 0.6830127018922202975, -0.2588190451025214056 ) ) ;
#54936 = ORIENTED_EDGE ( 'NONE', *, *, #110594, .F. ) ;
#54937 = CARTESIAN_POINT ( 'NONE',  ( -3.792893218813429002, -20.24070752338408141, 5.000000000000000000 ) ) ;
#54938 = EDGE_LOOP ( 'NONE', ( #32546, #22524, #7411, #124846, #59956, #136505 ) ) ;
#54939 = PLANE ( 'NONE',  #37419 ) ;
#54940 = ORIENTED_EDGE ( 'NONE', *, *, #97338, .F. ) ;
#54941 = AXIS2_PLACEMENT_3D ( 'NONE', #130074, #84446, #131499 ) ;
#54944 = ADVANCED_FACE ( 'NONE', ( #120390 ), #96505, .F. ) ;
#54943 = VECTOR ( 'NONE', #111836, 1000.000000000000114 ) ;
#54942 = CONICAL_SURFACE ( 'NONE', #6239, 2.055000000000001048, 0.9599310885968758145 ) ;
#54945 = EDGE_CURVE ( 'NONE', #46130, #125641, #98669, .T. ) ;
#54946 = DIRECTION ( 'NONE',  ( 0.7071067811865487940, 0.7071067811865463515, 0.000000000000000000 ) ) ;
#54948 = CARTESIAN_POINT ( 'NONE',  ( 114.8500270504628844, -5.819803920172572198, -5.819803920172572198 ) ) ;
#54947 = VECTOR ( 'NONE', #94360, 1000.000000000000000 ) ;
#54949 = CARTESIAN_POINT ( 'NONE',  ( 14.99999999999989875, 7.931123077392104648, 4.000000000000000000 ) ) ;
#54950 = LINE ( 'NONE', #54257, #13511 ) ;
#54951 = EDGE_CURVE ( 'NONE', #21857, #105963, #85648, .T. ) ;
#54952 =( NAMED_UNIT ( * ) SI_UNIT ( $, .STERADIAN. ) SOLID_ANGLE_UNIT ( ) );
#54953 = CARTESIAN_POINT ( 'NONE',  ( 0.000000000000000000, 2.375000000000000000, -4.320000000000002061 ) ) ;
#54954 = CARTESIAN_POINT ( 'NONE',  ( 24.39999999999999858, -1.600000000000086020, -34.92499999999998295 ) ) ;
#54955 = CARTESIAN_POINT ( 'NONE',  ( 13.27083333333333393, 6.094999999999991758, 1.633150327867687102 ) ) ;
#54956 = CARTESIAN_POINT ( 'NONE',  ( 15.14540314143521904, -2.126176841940958351, -7.934999999999988951 ) ) ;
#54957 = VECTOR ( 'NONE', #57864, 1000.000000000000000 ) ;
#54958 = CARTESIAN_POINT ( 'NONE',  ( 0.000000000000000000, 0.9892420537897055333, 14.41609864557725729 ) ) ;
#54959 = DIRECTION ( 'NONE',  ( 0.7071067811865486830, -0.7071067811865464625, -0.000000000000000000 ) ) ;
#54960 = VERTEX_POINT ( 'NONE', #119003 ) ;
#54961 = EDGE_LOOP ( 'NONE', ( #137447, #53999, #107585, #105954 ) ) ;
#54962 = ADVANCED_FACE ( 'NONE', ( #55191 ), #87799, .F. ) ;
#54963 = CARTESIAN_POINT ( 'NONE',  ( 45.29974487139158867, -27.71228299555237840, 4.000000000000000000 ) ) ;
#54964 = EDGE_LOOP ( 'NONE', ( #84063, #38030, #88564, #85011, #126489, #111189 ) ) ;
#54965 = CARTESIAN_POINT ( 'NONE',  ( 0.4892135623730947680, -27.52281430457055578, 5.000000000000000000 ) ) ;
#54966 = CARTESIAN_POINT ( 'NONE',  ( -4.499999999999964473, 15.43112307739203004, 4.000000000000000000 ) ) ;
#54967 = SURFACE_SIDE_STYLE ('',( #65870 ) ) ;
#54968 = ORIENTED_EDGE ( 'NONE', *, *, #122030, .T. ) ;
#54969 = ADVANCED_FACE ( 'NONE', ( #108098 ), #76967, .F. ) ;
#54970 = CARTESIAN_POINT ( 'NONE',  ( 174.7500000000000000, 7.919999999999947526, -16.42230000000009227 ) ) ;
#54971 = CARTESIAN_POINT ( 'NONE',  ( 7.326124847093153925, 2.055000000000001048, 0.000000000000000000 ) ) ;
#54972 = CARTESIAN_POINT ( 'NONE',  ( -5.999999999999958256, 13.93112307739204603, 4.000000000000000000 ) ) ;
#54973 = CARTESIAN_POINT ( 'NONE',  ( -48.29974487139158867, -27.71228299555239971, 4.000000000000000000 ) ) ;
#54974 = CARTESIAN_POINT ( 'NONE',  ( 14.99999999999990052, 10.93112307739207445, 4.000000000000000000 ) ) ;
#54976 = VERTEX_POINT ( 'NONE', #108811 ) ;
#54975 = LINE ( 'NONE', #111472, #5720 ) ;
#54977 = DIRECTION ( 'NONE',  ( 0.7071067811865486830, -0.7071067811865464625, -0.000000000000000000 ) ) ;
#54978 = CIRCLE ( 'NONE', #22530, 2.500000000000000444 ) ;
#54979 = EDGE_CURVE ( 'NONE', #118785, #60140, #53016, .T. ) ;
#54980 = CARTESIAN_POINT ( 'NONE',  ( 70.70833333333332860, -3.974999999999999201, -6.884901960086287964 ) ) ;
#54981 = DIRECTION ( 'NONE',  ( 0.000000000000000000, -1.000000000000000000, 0.000000000000000000 ) ) ;
#54982 = DIRECTION ( 'NONE',  ( 0.7071067811865486830, -0.7071067811865464625, -0.000000000000000000 ) ) ;
#54983 = CARTESIAN_POINT ( 'NONE',  ( 5.510786437626906675, -27.52281430457051314, 5.000000000000000000 ) ) ;
#54984 = ORIENTED_EDGE ( 'NONE', *, *, #127067, .T. ) ;
#54985 = ORIENTED_EDGE ( 'NONE', *, *, #65477, .T. ) ;
#54986 = ORIENTED_EDGE ( 'NONE', *, *, #6004, .T. ) ;
#54987 = CARTESIAN_POINT ( 'NONE',  ( 94.93793019189810423, -6.110000000000001208, 1.637169565754158951 ) ) ;
#54988 = AXIS2_PLACEMENT_3D ( 'NONE', #31727, #41164, #30293 ) ;
#54989 = VERTEX_POINT ( 'NONE', #10923 ) ;
#54990 = EDGE_CURVE ( 'NONE', #34604, #120211, #7830, .T. ) ;
#54991 = CARTESIAN_POINT ( 'NONE',  ( 14.99451991528749595, 28.92564299267948513, 4.000000000000000000 ) ) ;
#54992 = VECTOR ( 'NONE', #23594, 1000.000000000000000 ) ;
#54993 = CARTESIAN_POINT ( 'NONE',  ( -26.67183060077628198, -9.740707523384187994, 4.000000000000000000 ) ) ;
#54994 = EDGE_LOOP ( 'NONE', ( #94955, #53118, #31821, #107779 ) ) ;
#54995 = DIRECTION ( 'NONE',  ( 0.000000000000000000, -1.000000000000000000, 0.000000000000000000 ) ) ;
#54996 = PLANE ( 'NONE',  #28097 ) ;
#54997 = ADVANCED_FACE ( 'NONE', ( #66776 ), #22515, .F. ) ;
#54998 = EDGE_CURVE ( 'NONE', #28039, #24388, #110948, .T. ) ;
#54999 = CARTESIAN_POINT ( 'NONE',  ( 82.45376352523145158, -6.109999999999998543, -3.741295971395162543E-16 ) ) ;
#55000 = ORIENTED_EDGE ( 'NONE', *, *, #71779, .F. ) ;
#55001 = CARTESIAN_POINT ( 'NONE',  ( 0.2265654810057258217, 0.5999999999999987566, -3.877828006771851133 ) ) ;
#55002 = VECTOR ( 'NONE', #2118, 1000.000000000000227 ) ;
#55003 = CARTESIAN_POINT ( 'NONE',  ( 11.91508676806230582, -12.74070752338415602, 18.74364270924357001 ) ) ;
#55004 = EDGE_CURVE ( 'NONE', #66852, #98615, #121833, .T. ) ;
#55005 = VERTEX_POINT ( 'NONE', #1474 ) ;
#55006 = ORIENTED_EDGE ( 'NONE', *, *, #75247, .F. ) ;
#55007 = AXIS2_PLACEMENT_3D ( 'NONE', #39706, #73731, #83938 ) ;
#55008 = EDGE_LOOP ( 'NONE', ( #108280, #138800, #56601, #28226 ) ) ;
#55009 = LINE ( 'NONE', #110061, #28299 ) ;
#55010 = EDGE_CURVE ( 'NONE', #129972, #103979, #91398, .T. ) ;
#55011 = LINE ( 'NONE', #589, #43227 ) ;
#55012 = CARTESIAN_POINT ( 'NONE',  ( 19.17123647476855197, 0.000000000000000000, 7.934999999999990727 ) ) ;
#55013 = CARTESIAN_POINT ( 'NONE',  ( 0.000000000000000000, 0.000000000000000000, 5.000000000000000000 ) ) ;
#55014 = CARTESIAN_POINT ( 'NONE',  ( 3.345840036506314785, -49.02495722182847970, -39.69341335395904480 ) ) ;
#55015 = DIRECTION ( 'NONE',  ( 0.7071067811865486830, -0.7071067811865464625, -0.000000000000000000 ) ) ;
#55016 = SURFACE_STYLE_USAGE ( .BOTH. , #87625 ) ;
#55017 = ORIENTED_EDGE ( 'NONE', *, *, #60531, .T. ) ;
#55018 = ORIENTED_EDGE ( 'NONE', *, *, #5365, .F. ) ;
#55019 = ADVANCED_FACE ( 'NONE', ( #133463 ), #67514, .F. ) ;
#55020 = CARTESIAN_POINT ( 'NONE',  ( 16.21321903303349643, 12.75929247661559351, 10.29404684609039045 ) ) ;
#55021 = VERTEX_POINT ( 'NONE', #11636 ) ;
#55022 = ORIENTED_EDGE ( 'NONE', *, *, #88392, .F. ) ;
#55023 = EDGE_CURVE ( 'NONE', #49119, #143446, #112420, .T. ) ;
#55024 = VECTOR ( 'NONE', #46800, 1000.000000000000000 ) ;
#55025 = DIRECTION ( 'NONE',  ( 0.7071067811865486830, -0.7071067811865464625, -0.000000000000000000 ) ) ;
#55026 = ORIENTED_EDGE ( 'NONE', *, *, #3860, .F. ) ;
#55027 = DIRECTION ( 'NONE',  ( -0.000000000000000000, 0.3543493200069153248, 0.9351131265310292928 ) ) ;
#55028 = CARTESIAN_POINT ( 'NONE',  ( 13.49999999999990408, -20.53675388469229546, 2.352720554255925300 ) ) ;
#55029 = CARTESIAN_POINT ( 'NONE',  ( -12.48921356237309155, -27.52281430457064104, 5.000000000000000000 ) ) ;
#55030 = FACE_OUTER_BOUND ( 'NONE', #125830, .T. ) ;
#55031 = DIRECTION ( 'NONE',  ( 1.000000000000000000, 0.000000000000000000, 0.000000000000000000 ) ) ;
#55032 = ORIENTED_EDGE ( 'NONE', *, *, #73202, .F. ) ;
#55033 = CARTESIAN_POINT ( 'NONE',  ( 25.37176554955600238, -8.240707523384196875, 11.38925528200746662 ) ) ;
#55034 = AXIS2_PLACEMENT_3D ( 'NONE', #16452, #118647, #5585 ) ;
#55035 = VERTEX_POINT ( 'NONE', #45066 ) ;
#55036 = CARTESIAN_POINT ( 'NONE',  ( 19.39745846707657151, 0.5627691706057111887, -30.75765991350439421 ) ) ;
#55037 = ORIENTED_EDGE ( 'NONE', *, *, #19563, .F. ) ;
#55038 = CARTESIAN_POINT ( 'NONE',  ( 116.0166937171295700, 7.950000000000000178, -2.130196079827421318 ) ) ;
#55039 = VERTEX_POINT ( 'NONE', #13777 ) ;
#55040 = DIRECTION ( 'NONE',  ( -0.7071067811865486830, -0.7071067811865464625, 0.000000000000000000 ) ) ;
#55041 = VERTEX_POINT ( 'NONE', #102276 ) ;
#55042 = ORIENTED_EDGE ( 'NONE', *, *, #47644, .F. ) ;
#55043 = AXIS2_PLACEMENT_3D ( 'NONE', #112960, #123153, #23824 ) ;
#55044 = ORIENTED_EDGE ( 'NONE', *, *, #91762, .T. ) ;
#55045 = VECTOR ( 'NONE', #118289, 1000.000000000000000 ) ;
#55046 = EDGE_CURVE ( 'NONE', #75268, #16508, #101525, .T. ) ;
#55047 = DIRECTION ( 'NONE',  ( -0.7071067811865486830, -0.7071067811865464625, 0.000000000000000000 ) ) ;
#55048 = CARTESIAN_POINT ( 'NONE',  ( 22.82900182742193351, 7.795401085224272109, 5.000000000000000000 ) ) ;
#55049 = CARTESIAN_POINT ( 'NONE',  ( 0.4892135623730947680, -27.52281430457055578, 5.000000000000000000 ) ) ;
#55050 = DIRECTION ( 'NONE',  ( 0.6830127018922181881, 0.6830127018922202975, -0.2588190451025214056 ) ) ;
#55051 = DIRECTION ( 'NONE',  ( -0.6830127018922181881, 0.6830127018922202975, -0.2588190451025214056 ) ) ;
#55052 = CARTESIAN_POINT ( 'NONE',  ( 18.63999999999999702, 9.521314400968980422E-16, 0.000000000000000000 ) ) ;
#55053 = CARTESIAN_POINT ( 'NONE',  ( -25.26506670282035927, 12.75929247661558286, 18.34774599283961649 ) ) ;
#55054 = DIRECTION ( 'NONE',  ( -0.7071067811865486830, -0.7071067811865464625, 0.000000000000000000 ) ) ;
#55055 = VECTOR ( 'NONE', #1797, 1000.000000000000000 ) ;
#55056 = DIRECTION ( 'NONE',  ( 0.7071067811865486830, -0.7071067811865464625, -0.000000000000000000 ) ) ;
#55057 = DIRECTION ( 'NONE',  ( 0.000000000000000000, -1.000000000000000000, 0.000000000000000000 ) ) ;
#55058 = PLANE ( 'NONE',  #55240 ) ;
#55059 = LINE ( 'NONE', #90541, #137475 ) ;
#55060 = ORIENTED_EDGE ( 'NONE', *, *, #80011, .F. ) ;
#55061 = VERTEX_POINT ( 'NONE', #36291 ) ;
#55062 = ORIENTED_EDGE ( 'NONE', *, *, #28891, .T. ) ;
#55063 = DIRECTION ( 'NONE',  ( -0.000000000000000000, -1.000000000000000000, -0.000000000000000000 ) ) ;
#55064 = EDGE_LOOP ( 'NONE', ( #4684, #136486, #53637, #51771 ) ) ;
#55065 = ORIENTED_EDGE ( 'NONE', *, *, #125704, .T. ) ;
#55066 = CARTESIAN_POINT ( 'NONE',  ( -23.34505516254603208, 5.259292476615669010, 12.77922209995888458 ) ) ;
#55067 = FACE_OUTER_BOUND ( 'NONE', #103496, .T. ) ;
#55068 = DIRECTION ( 'NONE',  ( -0.000000000000000000, 0.3543493200069153248, 0.9351131265310292928 ) ) ;
#55069 = CARTESIAN_POINT ( 'NONE',  ( 0.4892135623730947680, -27.52281430457055578, 5.000000000000000000 ) ) ;
#55070 = DIRECTION ( 'NONE',  ( 0.7071067811865486830, -0.7071067811865464625, -0.000000000000000000 ) ) ;
#55071 = ORIENTED_EDGE ( 'NONE', *, *, #136141, .F. ) ;
#55072 = CIRCLE ( 'NONE', #69052, 2.500000000000000444 ) ;
#55073 = CARTESIAN_POINT ( 'NONE',  ( 36.18398860626899705, 28.73617430169812437, 5.000000000000000000 ) ) ;
#55074 = ORIENTED_EDGE ( 'NONE', *, *, #136320, .F. ) ;
#55075 = DIRECTION ( 'NONE',  ( 0.6830127018922181881, 0.6830127018922202975, -0.2588190451025214056 ) ) ;
#55076 = CARTESIAN_POINT ( 'NONE',  ( 18.00456980810188767, 6.871911579029510442, -3.967499999999998916 ) ) ;
#55077 = ORIENTED_EDGE ( 'NONE', *, *, #124438, .F. ) ;
#55078 = CARTESIAN_POINT ( 'NONE',  ( 81.87043019189812298, -3.055000000000001936, 5.291415217122918513 ) ) ;
#55079 = LINE ( 'NONE', #97861, #117684 ) ;
#55080 = CARTESIAN_POINT ( 'NONE',  ( -16.49999999999987921, -20.56887692260760758, 4.000000000000000000 ) ) ;
#55081 = ORIENTED_EDGE ( 'NONE', *, *, #127793, .F. ) ;
#55082 = ORIENTED_EDGE ( 'NONE', *, *, #132060, .T. ) ;
#55083 = EDGE_LOOP ( 'NONE', ( #127895, #103251, #100531, #67059, #117483 ) ) ;
#55084 = PLANE ( 'NONE',  #33378 ) ;
#55085 = CARTESIAN_POINT ( 'NONE',  ( 22.49999999999985434, 22.22500000000000142, 4.362957392718788796 ) ) ;
#55086 = CARTESIAN_POINT ( 'NONE',  ( 66.18398860626901126, 28.73617430169833753, 5.000000000000000000 ) ) ;
#55087 = CARTESIAN_POINT ( 'NONE',  ( 14.67183060077636725, 17.25929247661554200, 4.000000000000000000 ) ) ;
#55088 = CARTESIAN_POINT ( 'NONE',  ( 11.51078643762690490, -27.52281430457047406, 5.000000000000000000 ) ) ;
#55089 = ORIENTED_EDGE ( 'NONE', *, *, #142889, .T. ) ;
#55090 = LINE ( 'NONE', #42084, #62269 ) ;
#55091 = CARTESIAN_POINT ( 'NONE',  ( 34.49999999999975842, -10.53574439159940113, 4.994342998332163219 ) ) ;
#55093 = EDGE_CURVE ( 'NONE', #34133, #30243, #16392, .T. ) ;
#55092 = DIRECTION ( 'NONE',  ( 0.7071067811865487940, 0.7071067811865463515, 0.000000000000000000 ) ) ;
#55094 = EDGE_CURVE ( 'NONE', #90647, #118382, #132777, .T. ) ;
#55095 = ORIENTED_EDGE ( 'NONE', *, *, #102902, .F. ) ;
#55096 = DIRECTION ( 'NONE',  ( -0.7071067811865486830, -0.7071067811865464625, 0.000000000000000000 ) ) ;
#55097 = DIRECTION ( 'NONE',  ( 0.7071067811865487940, -0.7071067811865463515, 0.000000000000000000 ) ) ;
#55098 = ORIENTED_EDGE ( 'NONE', *, *, #110633, .T. ) ;
#55099 = EDGE_CURVE ( 'NONE', #61244, #124821, #97427, .T. ) ;
#55101 = ORIENTED_EDGE ( 'NONE', *, *, #44319, .F. ) ;
#55100 = DIRECTION ( 'NONE',  ( -1.000000000000000000, -1.224606353822377258E-16, -0.000000000000000000 ) ) ;
#55102 = ORIENTED_EDGE ( 'NONE', *, *, #72000, .T. ) ;
#55103 = EDGE_CURVE ( 'NONE', #69963, #99168, #68940, .T. ) ;
#55104 = EDGE_CURVE ( 'NONE', #7326, #85293, #124716, .T. ) ;
#55105 = FACE_OUTER_BOUND ( 'NONE', #68334, .T. ) ;
#55106 = PLANE ( 'NONE',  #99296 ) ;
#55107 = ORIENTED_EDGE ( 'NONE', *, *, #60643, .F. ) ;
#55108 = DIRECTION ( 'NONE',  ( -0.6830127018922180770, -0.6830127018922204085, -0.2588190451025214056 ) ) ;
#55109 = UNCERTAINTY_MEASURE_WITH_UNIT (LENGTH_MEASURE( 1.000000000000000082E-05 ), #82033, 'distance_accuracy_value', 'NONE');
#55110 = EDGE_CURVE ( 'NONE', #128780, #75355, #122555, .T. ) ;
#55111 = EDGE_CURVE ( 'NONE', #125681, #135809, #100822, .T. ) ;
#55112 = CARTESIAN_POINT ( 'NONE',  ( 69.18398860626899705, 28.73617430169835529, 5.000000000000000000 ) ) ;
#55113 = CARTESIAN_POINT ( 'NONE',  ( 20.99451991528748707, 28.92564299267952777, 4.000000000000000000 ) ) ;
#55114 = CARTESIAN_POINT ( 'NONE',  ( -7.499999999999944045, -2.568876922607786550, 4.000000000000000000 ) ) ;
#55115 = EDGE_CURVE ( 'NONE', #113156, #100573, #118556, .T. ) ;
#55116 = DIRECTION ( 'NONE',  ( -0.3543493200069162685, -0.000000000000000000, -0.9351131265310288487 ) ) ;
#55117 = CARTESIAN_POINT ( 'NONE',  ( 17.14818355038134712, 17.25929247661554555, 8.802941693769241738 ) ) ;
#55118 = CARTESIAN_POINT ( 'NONE',  ( -25.49999999999982592, 12.43112307739206024, 4.000000000000000000 ) ) ;
#55119 = CARTESIAN_POINT ( 'NONE',  ( 18.18398860626898994, 28.73617430169800002, 5.000000000000000000 ) ) ;
#55120 = LINE ( 'NONE', #32656, #113963 ) ;
#55121 = DIRECTION ( 'NONE',  ( 0.7071067811865487940, 0.7071067811865463515, -0.000000000000000000 ) ) ;
#55122 = DIRECTION ( 'NONE',  ( -0.7071067811865486830, 0.7071067811865463515, 0.000000000000000000 ) ) ;
#55123 = DIRECTION ( 'NONE',  ( 0.000000000000000000, 0.000000000000000000, 1.000000000000000000 ) ) ;
#55124 = VERTEX_POINT ( 'NONE', #57350 ) ;
#55125 = VERTEX_POINT ( 'NONE', #2175 ) ;
#55127 = EDGE_CURVE ( 'NONE', #36659, #27842, #53469, .T. ) ;
#55126 = CARTESIAN_POINT ( 'NONE',  ( 104.2500000000000000, -9.735942053221458872E-16, 7.950000000000000178 ) ) ;
#55128 = ORIENTED_EDGE ( 'NONE', *, *, #133066, .T. ) ;
#55129 = ORIENTED_EDGE ( 'NONE', *, *, #32683, .T. ) ;
#55130 = ORIENTED_EDGE ( 'NONE', *, *, #106042, .T. ) ;
#55131 = DIRECTION ( 'NONE',  ( 0.000000000000000000, -1.000000000000000000, 0.000000000000000000 ) ) ;
#55132 = DIRECTION ( 'NONE',  ( 0.5735764363510444941, 0.8191520442889929088, 0.000000000000000000 ) ) ;
#55133 = ORIENTED_EDGE ( 'NONE', *, *, #132747, .T. ) ;
#55134 = AXIS2_PLACEMENT_3D ( 'NONE', #15600, #50435, #127255 ) ;
#55135 = DIRECTION ( 'NONE',  ( -0.7071067811865487940, 0.7071067811865463515, -0.000000000000000000 ) ) ;
#55136 = CARTESIAN_POINT ( 'NONE',  ( 16.22674160717823355, -11.24070752338416490, 18.24660765846986266 ) ) ;
#55137 = CIRCLE ( 'NONE', #122255, 0.5000000000000005551 ) ;
#55138 = CARTESIAN_POINT ( 'NONE',  ( 74.99451991528749772, 28.92564299267990435, 4.000000000000000000 ) ) ;
#55139 = CARTESIAN_POINT ( 'NONE',  ( 34.92499999999998295, -21.72500000000000142, 5.000000000000000000 ) ) ;
#55140 = VERTEX_POINT ( 'NONE', #79838 ) ;
#55141 = CARTESIAN_POINT ( 'NONE',  ( 63.18398860626900415, 28.73617430169831621, 5.000000000000000000 ) ) ;
#55142 = CARTESIAN_POINT ( 'NONE',  ( -10.49999999999992539, 16.18958161055401490, -11.56426086740813730 ) ) ;
#55143 = CARTESIAN_POINT ( 'NONE',  ( 33.48921356237309510, -27.52281430457078670, 5.000000000000000000 ) ) ;
#55144 = EDGE_CURVE ( 'NONE', #66817, #88412, #94918, .T. ) ;
#55146 = CARTESIAN_POINT ( 'NONE',  ( 15.70710678118643777, -18.74070752338409562, 5.000000000000000000 ) ) ;
#55145 = VECTOR ( 'NONE', #142934, 1000.000000000000000 ) ;
#55147 = LINE ( 'NONE', #77623, #12116 ) ;
#55148 = CARTESIAN_POINT ( 'NONE',  ( 10.49999999999993605, -4.912538124160710673, 4.000000000000000000 ) ) ;
#55149 = VECTOR ( 'NONE', #73227, 999.9999999999998863 ) ;
#55150 = DIRECTION ( 'NONE',  ( 0.7071067811865486830, -0.7071067811865464625, -0.000000000000000000 ) ) ;
#55151 = CARTESIAN_POINT ( 'NONE',  ( 32.99451991528749062, 28.92564299267960948, 4.000000000000000000 ) ) ;
#55152 = ORIENTED_EDGE ( 'NONE', *, *, #126470, .F. ) ;
#55153 = ORIENTED_EDGE ( 'NONE', *, *, #5976, .T. ) ;
#55154 = CARTESIAN_POINT ( 'NONE',  ( 123.6670968585647756, -3.055000000000000160, -5.291415217122921177 ) ) ;
#55155 = ORIENTED_EDGE ( 'NONE', *, *, #29833, .F. ) ;
#55156 = CARTESIAN_POINT ( 'NONE',  ( 34.92499999999998295, -16.19990548397266039, 4.759050581649326261 ) ) ;
#55157 = ADVANCED_FACE ( 'NONE', ( #61631 ), #5033, .F. ) ;
#55158 = CARTESIAN_POINT ( 'NONE',  ( 19.63753812416084443, 22.22500000000000142, 4.000000000000000000 ) ) ;
#55159 = LINE ( 'NONE', #99338, #8613 ) ;
#55160 = LINE ( 'NONE', #45734, #67510 ) ;
#55161 = CARTESIAN_POINT ( 'NONE',  ( 24.39999999999999858, -7.600000000000055600, -28.92499999999998650 ) ) ;
#55162 = EDGE_CURVE ( 'NONE', #2927, #89784, #105097, .T. ) ;
#55163 = CARTESIAN_POINT ( 'NONE',  ( 111.9120968585647944, 5.291415217122921177, -3.054999999999994831 ) ) ;
#55164 = ORIENTED_EDGE ( 'NONE', *, *, #43658, .F. ) ;
#55165 = EDGE_CURVE ( 'NONE', #54738, #128151, #127574, .T. ) ;
#55166 = ORIENTED_EDGE ( 'NONE', *, *, #142549, .T. ) ;
#55167 = CARTESIAN_POINT ( 'NONE',  ( 23.27718569542924243, -21.72500000000000142, 5.000000000000000000 ) ) ;
#55168 = FACE_OUTER_BOUND ( 'NONE', #106513, .T. ) ;
#55169 = EDGE_CURVE ( 'NONE', #99905, #125583, #82648, .T. ) ;
#55171 = ADVANCED_FACE ( 'NONE', ( #28268 ), #28977, .T. ) ;
#55170 = VECTOR ( 'NONE', #1029, 1000.000000000000227 ) ;
#55172 = ORIENTED_EDGE ( 'NONE', *, *, #102350, .F. ) ;
#55173 = VERTEX_POINT ( 'NONE', #117373 ) ;
#55174 = CARTESIAN_POINT ( 'NONE',  ( 39.66709685856477563, -3.055000000000000160, -5.291415217122921177 ) ) ;
#55175 = ORIENTED_EDGE ( 'NONE', *, *, #30775, .T. ) ;
#55176 = CARTESIAN_POINT ( 'NONE',  ( 8.999999999999937828, -2.904428200921304271, -6.989807076074965764 ) ) ;
#55177 = CARTESIAN_POINT ( 'NONE',  ( 69.29974487139159578, -27.71228299555254537, 4.000000000000000000 ) ) ;
#55178 = VECTOR ( 'NONE', #12229, 1000.000000000000000 ) ;
#55179 = SURFACE_STYLE_USAGE ( .BOTH. , #87086 ) ;
#55180 = ADVANCED_FACE ( 'NONE', ( #26824 ), #4288, .T. ) ;
#55181 = CARTESIAN_POINT ( 'NONE',  ( 29.80793019189811588, -6.109999999999998543, 1.637169565754158063 ) ) ;
#55182 = VERTEX_POINT ( 'NONE', #73210 ) ;
#55183 = EDGE_CURVE ( 'NONE', #132937, #20628, #71075, .T. ) ;
#55184 = CARTESIAN_POINT ( 'NONE',  ( -2.953411863704541673, 14.25929247661557753, 18.84478104361328832 ) ) ;
#55185 = ORIENTED_EDGE ( 'NONE', *, *, #89250, .T. ) ;
#55186 = ORIENTED_EDGE ( 'NONE', *, *, #3778, .F. ) ;
#55187 = CONICAL_SURFACE ( 'NONE', #138487, 2.500000000000000444, 0.9599310885968830309 ) ;
#55188 = ORIENTED_EDGE ( 'NONE', *, *, #125262, .F. ) ;
#55189 = CIRCLE ( 'NONE', #45895, 2.500000000000000888 ) ;
#55190 =( NAMED_UNIT ( * ) SI_UNIT ( $, .STERADIAN. ) SOLID_ANGLE_UNIT ( ) );
#55191 = FACE_OUTER_BOUND ( 'NONE', #100553, .T. ) ;
#55192 = EDGE_CURVE ( 'NONE', #58171, #126408, #137752, .T. ) ;
#55193 = EDGE_LOOP ( 'NONE', ( #95839, #125568, #42299, #69067, #138683 ) ) ;
#55194 = FACE_OUTER_BOUND ( 'NONE', #53656, .T. ) ;
#55195 = PLANE ( 'NONE',  #117788 ) ;
#55196 = DIRECTION ( 'NONE',  ( 1.000000000000000000, 3.115803279706882722E-16, 0.000000000000000000 ) ) ;
#55197 = EDGE_CURVE ( 'NONE', #124072, #123554, #58809, .T. ) ;
#55198 = FACE_BOUND ( 'NONE', #133958, .T. ) ;
#55199 = ORIENTED_EDGE ( 'NONE', *, *, #132201, .T. ) ;
#55200 = FACE_OUTER_BOUND ( 'NONE', #141503, .T. ) ;
#55201 = LINE ( 'NONE', #122572, #95343 ) ;
#55202 = DIRECTION ( 'NONE',  ( -0.000000000000000000, 0.000000000000000000, 1.000000000000000000 ) ) ;
#55203 = VERTEX_POINT ( 'NONE', #103644 ) ;
#55204 = DIRECTION ( 'NONE',  ( 0.7071067811865487940, 0.7071067811865463515, -0.000000000000000000 ) ) ;
#55205 = ORIENTED_EDGE ( 'NONE', *, *, #108009, .T. ) ;
#55206 = EDGE_LOOP ( 'NONE', ( #26641, #87317, #30096, #34951 ) ) ;
#55207 = VERTEX_POINT ( 'NONE', #39144 ) ;
#55208 = CARTESIAN_POINT ( 'NONE',  ( 43.66209685856478728, -5.291415217122919401, 3.054999999999997939 ) ) ;
#55209 = EDGE_LOOP ( 'NONE', ( #50267, #94370, #82688, #101934 ) ) ;
#55210 = LINE ( 'NONE', #129907, #51011 ) ;
#55211 = CARTESIAN_POINT ( 'NONE',  ( 11.67183060077638856, 17.25929247661554555, 4.000000000000000000 ) ) ;
#55212 = CARTESIAN_POINT ( 'NONE',  ( 45.48921356237309510, -27.52281430457087197, 5.000000000000000000 ) ) ;
#55213 = ORIENTED_EDGE ( 'NONE', *, *, #115258, .T. ) ;
#55214 = CARTESIAN_POINT ( 'NONE',  ( 34.49999999999976552, -4.535744391599457082, 4.994342998332164107 ) ) ;
#55215 = CARTESIAN_POINT ( 'NONE',  ( 20.99451991528748707, 28.92564299267952777, 4.000000000000000000 ) ) ;
#55216 = EDGE_CURVE ( 'NONE', #107904, #138649, #38429, .T. ) ;
#55217 = EDGE_CURVE ( 'NONE', #76456, #114150, #27523, .T. ) ;
#55218 = DIRECTION ( 'NONE',  ( 0.000000000000000000, 0.000000000000000000, 1.000000000000000000 ) ) ;
#55219 = DIRECTION ( 'NONE',  ( -0.7071067811865486830, 0.7071067811865464625, 0.000000000000000000 ) ) ;
#55220 = CARTESIAN_POINT ( 'NONE',  ( -16.49999999999988276, -6.839392718269142080, -8.480912228396045194 ) ) ;
#55221 = DIRECTION ( 'NONE',  ( -0.7071067811865486830, -0.7071067811865464625, 0.000000000000000000 ) ) ;
#55222 = DIRECTION ( 'NONE',  ( -0.000000000000000000, 0.3543493200069153248, 0.9351131265310292928 ) ) ;
#55223 = ORIENTED_EDGE ( 'NONE', *, *, #102951, .T. ) ;
#55224 = ORIENTED_EDGE ( 'NONE', *, *, #26102, .F. ) ;
#55225 = EDGE_LOOP ( 'NONE', ( #114450, #44831, #18648, #10750, #54512 ) ) ;
#55226 = LINE ( 'NONE', #57385, #28831 ) ;
#55227 = VECTOR ( 'NONE', #47057, 1000.000000000000000 ) ;
#55228 = LINE ( 'NONE', #11676, #93079 ) ;
#55229 = ORIENTED_EDGE ( 'NONE', *, *, #76961, .F. ) ;
#55230 = VECTOR ( 'NONE', #82837, 1000.000000000000000 ) ;
#55232 = ORIENTED_EDGE ( 'NONE', *, *, #103146, .T. ) ;
#55231 = AXIS2_PLACEMENT_3D ( 'NONE', #99019, #87463, #66428 ) ;
#55233 = DIRECTION ( 'NONE',  ( 0.000000000000000000, 0.000000000000000000, -1.000000000000000000 ) ) ;
#55234 = DIRECTION ( 'NONE',  ( 0.7071067811865487940, 0.7071067811865463515, -0.000000000000000000 ) ) ;
#55235 = EDGE_CURVE ( 'NONE', #44871, #93122, #102974, .T. ) ;
#55236 = VECTOR ( 'NONE', #110672, 1000.000000000000000 ) ;
#55237 = CARTESIAN_POINT ( 'NONE',  ( 27.48921356237309155, -27.52281430457074762, 5.000000000000000000 ) ) ;
#55238 = ORIENTED_EDGE ( 'NONE', *, *, #13014, .F. ) ;
#55239 = DIRECTION ( 'NONE',  ( -0.000000000000000000, -0.3543493200069152693, 0.9351131265310292928 ) ) ;
#55240 = AXIS2_PLACEMENT_3D ( 'NONE', #76827, #121001, #74678 ) ;
#55241 = VECTOR ( 'NONE', #67795, 1000.000000000000000 ) ;
#55242 = CARTESIAN_POINT ( 'NONE',  ( 19.49999999999986500, -9.462702396500995761, -9.474982329943561155 ) ) ;
#55243 = CARTESIAN_POINT ( 'NONE',  ( 30.25456980810189123, -6.871911579029512218, 3.967499999999996252 ) ) ;
#55244 = DIRECTION ( 'NONE',  ( -0.7071067811865486830, -0.7071067811865464625, -0.000000000000000000 ) ) ;
#55245 = VERTEX_POINT ( 'NONE', #115953 ) ;
#55246 = CARTESIAN_POINT ( 'NONE',  ( 111.3287635252314516, 0.000000000000000000, -6.109999999999999432 ) ) ;
#55247 =( BOUNDED_CURVE ( )  B_SPLINE_CURVE ( 3, ( #104065, #125126, #70783, #34567 ),
 .UNSPECIFIED., .F., .T. ) 
 B_SPLINE_CURVE_WITH_KNOTS ( ( 4, 4 ),
 ( 1.570796326794896558, 3.141592653589793116 ),
 .UNSPECIFIED. ) 
 CURVE ( )  GEOMETRIC_REPRESENTATION_ITEM ( )  RATIONAL_B_SPLINE_CURVE ( ( 1.000000000000000000, 0.8047378541243649375, 0.8047378541243649375, 1.000000000000000000 ) ) 
 REPRESENTATION_ITEM ( '' )  );
#55248 = PLANE ( 'NONE',  #76664 ) ;
#55249 = CARTESIAN_POINT ( 'NONE',  ( 19.49999999999985789, 5.696342897626518464, -7.587980461218352346 ) ) ;
#55251 = ORIENTED_EDGE ( 'NONE', *, *, #52564, .F. ) ;
#55250 = DIRECTION ( 'NONE',  ( 1.000000000000000000, 1.224606353822377258E-16, 0.000000000000000000 ) ) ;
#55252 = CONICAL_SURFACE ( 'NONE', #38995, 2.500000000000000444, 0.9599310885968830309 ) ;
#55253 = CARTESIAN_POINT ( 'NONE',  ( 12.08840764549667668, -2.500000000000000888, 0.000000000000000000 ) ) ;
#55254 = ORIENTED_EDGE ( 'NONE', *, *, #123469, .F. ) ;
#55255 = PLANE ( 'NONE',  #49693 ) ;
#55256 = CARTESIAN_POINT ( 'NONE',  ( 24.83652871126534123, 15.75929247661555443, 9.299976744542977514 ) ) ;
#55257 = DIRECTION ( 'NONE',  ( -0.3543493200069162685, -0.000000000000000000, -0.9351131265310288487 ) ) ;
#55258 = ORIENTED_EDGE ( 'NONE', *, *, #26850, .F. ) ;
#55259 = VECTOR ( 'NONE', #29428, 1000.000000000000000 ) ;
#55260 = EDGE_CURVE ( 'NONE', #117635, #84441, #83361, .T. ) ;
#55261 = CARTESIAN_POINT ( 'NONE',  ( 0.4892135623730947680, -27.52281430457055578, 5.000000000000000000 ) ) ;
#55262 = PLANE ( 'NONE',  #72303 ) ;
#55263 = ORIENTED_EDGE ( 'NONE', *, *, #27776, .T. ) ;
#55264 = ADVANCED_FACE ( 'NONE', ( #5760 ), #50026, .F. ) ;
#55265 = LINE ( 'NONE', #88618, #64762 ) ;
#55267 = VECTOR ( 'NONE', #58547, 1000.000000000000000 ) ;
#55266 = LINE ( 'NONE', #33538, #97826 ) ;
#55268 = ORIENTED_EDGE ( 'NONE', *, *, #7924, .T. ) ;
#55269 = COLOUR_RGB ( '', 0.40784314, 0.44705882, 0.49803922) ;
#55270 = DIRECTION ( 'NONE',  ( -0.6830127018922181881, 0.6830127018922202975, -0.2588190451025214056 ) ) ;
#55272 = ORIENTED_EDGE ( 'NONE', *, *, #94668, .T. ) ;
#55271 = CARTESIAN_POINT ( 'NONE',  ( 18.95159235450331892, 9.902892378096218942E-16, 0.000000000000000000 ) ) ;
#55273 = ADVANCED_FACE ( 'NONE', ( #36979 ), #138455, .F. ) ;
#55274 = ORIENTED_EDGE ( 'NONE', *, *, #99471, .F. ) ;
#55275 = CARTESIAN_POINT ( 'NONE',  ( 13.74720049256562682, 8.866765337654086920, -27.55742918605191960 ) ) ;
#55276 = VECTOR ( 'NONE', #126087, 1000.000000000000000 ) ;
#55277 = LINE ( 'NONE', #99453, #94549 ) ;
#55278 = ORIENTED_EDGE ( 'NONE', *, *, #102518, .T. ) ;
#55279 = VECTOR ( 'NONE', #7203, 1000.000000000000000 ) ;
#55280 = LINE ( 'NONE', #64012, #11131 ) ;
#55281 = EDGE_CURVE ( 'NONE', #46561, #106533, #81965, .T. ) ;
#55282 = EDGE_CURVE ( 'NONE', #10669, #95640, #85469, .T. ) ;
#55283 = LINE ( 'NONE', #129980, #50681 ) ;
#55284 = LINE ( 'NONE', #23333, #42181 ) ;
#55285 = ADVANCED_FACE ( 'NONE', ( #96326 ), #118079, .T. ) ;
#55286 = EDGE_LOOP ( 'NONE', ( #141890, #70780, #116974, #68941 ) ) ;
#55287 = DIRECTION ( 'NONE',  ( 1.000000000000000000, 0.000000000000000000, 0.000000000000000000 ) ) ;
#55288 = EDGE_CURVE ( 'NONE', #65140, #91460, #33812, .T. ) ;
#55289 = CARTESIAN_POINT ( 'NONE',  ( 42.18398860626899705, 28.73617430169816700, 5.000000000000000000 ) ) ;
#55290 = CARTESIAN_POINT ( 'NONE',  ( 17.84878961325748037, 2.500000000000000888, 0.000000000000000000 ) ) ;
#55291 = VECTOR ( 'NONE', #114094, 1000.000000000000227 ) ;
#55292 = FILL_AREA_STYLE ('',( #132868 ) ) ;
#55293 = ADVANCED_FACE ( 'NONE', ( #78031 ), #100492, .T. ) ;
#55294 = CARTESIAN_POINT ( 'NONE',  ( 27.47459685856478018, 1.637169565754164280, -6.109999999999997655 ) ) ;
#55295 = CARTESIAN_POINT ( 'NONE',  ( -33.18398860626899705, 28.73617430169810305, 5.000000000000000000 ) ) ;
#55296 = VERTEX_POINT ( 'NONE', #7177 ) ;
#55297 = EDGE_LOOP ( 'NONE', ( #134422, #44413, #138427, #20326 ) ) ;
#55299 = EDGE_CURVE ( 'NONE', #79224, #117585, #30402, .T. ) ;
#55298 = LINE ( 'NONE', #99469, #104398 ) ;
#55300 = ORIENTED_EDGE ( 'NONE', *, *, #103777, .T. ) ;
#55301 = ORIENTED_EDGE ( 'NONE', *, *, #120026, .F. ) ;
#55302 = DIRECTION ( 'NONE',  ( -1.000000000000000000, 5.303853817486469551E-15, 0.000000000000000000 ) ) ;
#55303 = CARTESIAN_POINT ( 'NONE',  ( 32.28769006033950006, -21.73547319004780931, 4.999917730833664642 ) ) ;
#55304 = ORIENTED_EDGE ( 'NONE', *, *, #97632, .F. ) ;
#55305 = DIRECTION ( 'NONE',  ( 0.7071067811865487940, -0.7071067811865463515, 0.000000000000000000 ) ) ;
#55306 = LINE ( 'NONE', #122676, #123117 ) ;
#55307 = EDGE_CURVE ( 'NONE', #81467, #83442, #9306, .T. ) ;
#55308 = LINE ( 'NONE', #152, #120419 ) ;
#55309 = ADVANCED_FACE ( 'NONE', ( #74637 ), #19516, .T. ) ;
#55310 = DIRECTION ( 'NONE',  ( 0.000000000000000000, 1.000000000000000000, 0.000000000000000000 ) ) ;
#55311 = CARTESIAN_POINT ( 'NONE',  ( 125.5629301918981042, 1.637169565754157174, 6.110000000000002984 ) ) ;
#55312 = ORIENTED_EDGE ( 'NONE', *, *, #42696, .T. ) ;
#55313 = LINE ( 'NONE', #33579, #30300 ) ;
#55314 = CARTESIAN_POINT ( 'NONE',  ( -26.20710678118635784, -2.240707523384255939, 5.000000000000000000 ) ) ;
#55315 = CARTESIAN_POINT ( 'NONE',  ( -27.18398860626900060, 28.73617430169806042, 5.000000000000000000 ) ) ;
#55316 = CYLINDRICAL_SURFACE ( 'NONE', #86703, 2.500000000000000000 ) ;
#55317 = ADVANCED_FACE ( 'NONE', ( #73905 ), #111336, .F. ) ;
#55318 = CARTESIAN_POINT ( 'NONE',  ( -9.005480084712511157, 28.92564299267931816, 4.000000000000000000 ) ) ;
#55319 = FACE_OUTER_BOUND ( 'NONE', #29347, .T. ) ;
#55320 = CARTESIAN_POINT ( 'NONE',  ( 59.72502705046289861, 5.819803920172573086, -5.819803920172572198 ) ) ;
#55321 = DIRECTION ( 'NONE',  ( -0.000000000000000000, 0.3543493200069153248, 0.9351131265310292928 ) ) ;
#55322 = CARTESIAN_POINT ( 'NONE',  ( 10.94186803553636977, 3.061616997868383634E-16, -2.500000000000000444 ) ) ;
#55323 = ORIENTED_EDGE ( 'NONE', *, *, #29080, .T. ) ;
#55324 = ORIENTED_EDGE ( 'NONE', *, *, #9092, .F. ) ;
#55325 = CARTESIAN_POINT ( 'NONE',  ( 45.18749999999998579, -5.819803920172573086, 5.819803920172572198 ) ) ;
#55326 = DIRECTION ( 'NONE',  ( -0.7071067811865486830, -0.7071067811865464625, -0.000000000000000000 ) ) ;
#55327 = CARTESIAN_POINT ( 'NONE',  ( -30.29974487139158867, -27.71228299555227537, 4.000000000000000000 ) ) ;
#55328 = ORIENTED_EDGE ( 'NONE', *, *, #17761, .F. ) ;
#55329 = DIRECTION ( 'NONE',  ( -0.7071067811865487940, 0.7071067811865463515, 0.000000000000000000 ) ) ;
#55330 = LINE ( 'NONE', #121280, #90934 ) ;
#55331 = VECTOR ( 'NONE', #53669, 1000.000000000000227 ) ;
#55332 = CARTESIAN_POINT ( 'NONE',  ( 36.16709685856476852, -3.055000000000000160, -5.291415217122921177 ) ) ;
#55333 = ORIENTED_EDGE ( 'NONE', *, *, #9387, .F. ) ;
#55334 = EDGE_CURVE ( 'NONE', #104144, #49412, #135726, .T. ) ;
#55335 = PLANE ( 'NONE',  #80327 ) ;
#55336 = VERTEX_POINT ( 'NONE', #81605 ) ;
#55337 = ORIENTED_EDGE ( 'NONE', *, *, #52906, .F. ) ;
#55338 = DIRECTION ( 'NONE',  ( -0.6830127018922180770, -0.6830127018922204085, -0.2588190451025213501 ) ) ;
#55339 = CIRCLE ( 'NONE', #57626, 2.055000000000001048 ) ;
#55340 = VECTOR ( 'NONE', #17104, 1000.000000000000000 ) ;
#55341 = VECTOR ( 'NONE', #132045, 1000.000000000000000 ) ;
#55342 = CARTESIAN_POINT ( 'NONE',  ( 15.05159235450332034, 9.902892378096218942E-16, 0.000000000000000000 ) ) ;
#55343 = DIRECTION ( 'NONE',  ( -1.000000000000000000, -0.000000000000000000, -0.000000000000000000 ) ) ;
#55344 = VECTOR ( 'NONE', #143437, 1000.000000000000000 ) ;
#55345 = DIRECTION ( 'NONE',  ( -0.7071067811865486830, -0.7071067811865464625, -0.000000000000000000 ) ) ;
#55346 = EDGE_LOOP ( 'NONE', ( #94450, #6313, #111724, #60615 ) ) ;
#55347 = PLANE ( 'NONE',  #78967 ) ;
#55349 = ORIENTED_EDGE ( 'NONE', *, *, #77740, .F. ) ;
#55348 = DIRECTION ( 'NONE',  ( 0.000000000000000000, 0.000000000000000000, -1.000000000000000000 ) ) ;
#55350 = CARTESIAN_POINT ( 'NONE',  ( 86.04209685856477563, 5.291415217122923842, -3.054999999999996163 ) ) ;
#55351 = PLANE ( 'NONE',  #99404 ) ;
#55352 = CARTESIAN_POINT ( 'NONE',  ( -8.773457579940252170E-14, -35.14999999999997726, -39.50000000000000000 ) ) ;
#55353 = DIRECTION ( 'NONE',  ( -0.7071067811865487940, 0.7071067811865463515, 0.000000000000000000 ) ) ;
#55354 = DIRECTION ( 'NONE',  ( -1.000000000000000000, -0.000000000000000000, -0.000000000000000000 ) ) ;
#55355 = AXIS2_PLACEMENT_3D ( 'NONE', #128389, #48682, #137118 ) ;
#55356 = ADVANCED_FACE ( 'NONE', ( #26489 ), #134556, .F. ) ;
#55357 = ORIENTED_EDGE ( 'NONE', *, *, #80448, .F. ) ;
#55358 = CARTESIAN_POINT ( 'NONE',  ( 36.48921356237310221, -27.52281430457080802, 5.000000000000000000 ) ) ;
#55359 = CARTESIAN_POINT ( 'NONE',  ( 65.68293019189810877, -1.637169565754158951, -6.109999999999998543 ) ) ;
#55360 = CARTESIAN_POINT ( 'NONE',  ( 22.82816939922337340, -17.24070752338410273, 4.000000000000000000 ) ) ;
#55361 = EDGE_CURVE ( 'NONE', #76949, #54350, #104008, .T. ) ;
#55362 = DIRECTION ( 'NONE',  ( 0.7071067811865486830, -0.7071067811865464625, -0.000000000000000000 ) ) ;
#55363 = CARTESIAN_POINT ( 'NONE',  ( 12.03892749862900402, 2.055000000000001048, 0.000000000000000000 ) ) ;
#55364 = VERTEX_POINT ( 'NONE', #13434 ) ;
#55365 = EDGE_LOOP ( 'NONE', ( #101900, #64454, #44953, #129974 ) ) ;
#55366 = VECTOR ( 'NONE', #130534, 1000.000000000000000 ) ;
#55367 = DIRECTION ( 'NONE',  ( -0.6830127018922180770, -0.6830127018922204085, -0.2588190451025213501 ) ) ;
#55368 = ORIENTED_EDGE ( 'NONE', *, *, #84415, .F. ) ;
#55369 = ADVANCED_FACE ( 'NONE', ( #69292 ), #125815, .F. ) ;
#55370 = CARTESIAN_POINT ( 'NONE',  ( -14.99451991528749595, 28.92564299267948513, 4.000000000000000000 ) ) ;
#55371 = VERTEX_POINT ( 'NONE', #114883 ) ;
#55372 = CARTESIAN_POINT ( 'NONE',  ( 32.67183060077625356, 2.259292476615704981, 4.000000000000000000 ) ) ;
#55373 = PLANE ( 'NONE',  #112767 ) ;
#55374 = DIRECTION ( 'NONE',  ( -0.000000000000000000, -0.000000000000000000, 1.000000000000000000 ) ) ;
#55375 = CIRCLE ( 'NONE', #32182, 25.00000000000002487 ) ;
#55377 = AXIS2_PLACEMENT_3D ( 'NONE', #92509, #17799, #94652 ) ;
#55376 = CARTESIAN_POINT ( 'NONE',  ( 5.187538124160490760, -22.22500000000000142, 4.000000000000000000 ) ) ;
#55378 = EDGE_CURVE ( 'NONE', #37141, #132971, #48235, .T. ) ;
#55379 = FACE_BOUND ( 'NONE', #52855, .T. ) ;
#55380 = DIRECTION ( 'NONE',  ( -0.000000000000000000, -0.3543493200069152693, 0.9351131265310292928 ) ) ;
#55381 = PLANE ( 'NONE',  #125474 ) ;
#55382 = DIRECTION ( 'NONE',  ( 0.7071067811865487940, 0.7071067811865463515, 0.000000000000000000 ) ) ;
#55384 = ORIENTED_EDGE ( 'NONE', *, *, #67100, .F. ) ;
#55383 = LINE ( 'NONE', #119871, #29645 ) ;
#55385 = VECTOR ( 'NONE', #82412, 1000.000000000000000 ) ;
#55386 = VECTOR ( 'NONE', #78421, 1000.000000000000000 ) ;
#55387 = FACE_OUTER_BOUND ( 'NONE', #117717, .T. ) ;
#55388 = ORIENTED_EDGE ( 'NONE', *, *, #124330, .F. ) ;
#55389 = ORIENTED_EDGE ( 'NONE', *, *, #34243, .T. ) ;
#55390 = CARTESIAN_POINT ( 'NONE',  ( 76.32876352523145158, 0.000000000000000000, -6.109999999999998543 ) ) ;
#55391 = ORIENTED_EDGE ( 'NONE', *, *, #105019, .F. ) ;
#55392 = CARTESIAN_POINT ( 'NONE',  ( 26.99999999999980460, 4.965500833774353140, -4.007596771432718974 ) ) ;
#55393 = CARTESIAN_POINT ( 'NONE',  ( -30.18398860626900060, 28.73617430169808173, 5.000000000000000000 ) ) ;
#55394 = ORIENTED_EDGE ( 'NONE', *, *, #53319, .T. ) ;
#55395 = CARTESIAN_POINT ( 'NONE',  ( -34.92500000000001137, -22.22500000000000142, 4.500000000000000888 ) ) ;
#55396 = AXIS2_PLACEMENT_3D ( 'NONE', #89316, #55270, #99448 ) ;
#55397 = EDGE_CURVE ( 'NONE', #58222, #94758, #46871, .T. ) ;
#55398 = ADVANCED_FACE ( 'NONE', ( #93169 ), #2562, .F. ) ;
#55399 = CARTESIAN_POINT ( 'NONE',  ( 34.42499999999998295, -3.022814304570575761, 5.000000000000000000 ) ) ;
#55400 = DIRECTION ( 'NONE',  ( 0.6830127018922180770, -0.6830127018922204085, -0.2588190451025213501 ) ) ;
#55401 = EDGE_CURVE ( 'NONE', #38121, #74158, #24341, .T. ) ;
#55402 = CARTESIAN_POINT ( 'NONE',  ( -18.48921356237309510, -27.52281430457068367, 5.000000000000000000 ) ) ;
#55403 = CARTESIAN_POINT ( 'NONE',  ( 5.999999999999952927, -13.06887692260767864, 4.000000000000000000 ) ) ;
#55404 = CARTESIAN_POINT ( 'NONE',  ( 19.73159235450332005, 9.902892378096218942E-16, 0.000000000000000000 ) ) ;
#55405 = ORIENTED_EDGE ( 'NONE', *, *, #66655, .F. ) ;
#55406 = EDGE_LOOP ( 'NONE', ( #89001, #5996, #53038, #16049 ) ) ;
#55407 = CARTESIAN_POINT ( 'NONE',  ( 48.18398860626899705, 28.73617430169820608, 5.000000000000000000 ) ) ;
#55408 = DIRECTION ( 'NONE',  ( -0.7071067811865486830, -0.7071067811865464625, 0.000000000000000000 ) ) ;
#55409 = ORIENTED_EDGE ( 'NONE', *, *, #141367, .F. ) ;
#55410 = EDGE_LOOP ( 'NONE', ( #44683, #20464, #34630, #55429 ) ) ;
#55411 = EDGE_CURVE ( 'NONE', #49875, #129576, #135279, .T. ) ;
#55412 = CARTESIAN_POINT ( 'NONE',  ( 27.85459685856476852, -1.637169565754161615, 6.110000000000000320 ) ) ;
#55413 = ORIENTED_EDGE ( 'NONE', *, *, #110907, .F. ) ;
#55414 = CARTESIAN_POINT ( 'NONE',  ( -45.48921356237309510, -27.52281430457087197, 5.000000000000000000 ) ) ;
#55415 = DIRECTION ( 'NONE',  ( -0.6830127018922181881, 0.6830127018922202975, -0.2588190451025214056 ) ) ;
#55416 = CARTESIAN_POINT ( 'NONE',  ( 24.69163961620376924, 6.094999999999988205, -1.633150327867694651 ) ) ;
#55417 = DIRECTION ( 'NONE',  ( 0.3543493200069163240, 0.000000000000000000, 0.9351131265310288487 ) ) ;
#55418 = ORIENTED_EDGE ( 'NONE', *, *, #120799, .T. ) ;
#55419 = DIRECTION ( 'NONE',  ( 0.6830127018922180770, -0.6830127018922204085, -0.2588190451025213501 ) ) ;
#55420 = ORIENTED_EDGE ( 'NONE', *, *, #114977, .T. ) ;
#55421 = CARTESIAN_POINT ( 'NONE',  ( -2.999999999999980016, 7.552185695429095347, 5.000000000000000000 ) ) ;
#55422 = LINE ( 'NONE', #134415, #56846 ) ;
#55424 = VERTEX_POINT ( 'NONE', #103309 ) ;
#55423 = CARTESIAN_POINT ( 'NONE',  ( 0.000000000000000000, 0.000000000000000000, 5.000000000000000000 ) ) ;
#55425 = ORIENTED_EDGE ( 'NONE', *, *, #125707, .F. ) ;
#55426 = CARTESIAN_POINT ( 'NONE',  ( 18.79289321881332597, 12.75929247661559174, 5.000000000000000000 ) ) ;
#55427 = CARTESIAN_POINT ( 'NONE',  ( -34.92500000000001137, -7.298069433178910437, 4.500000000000000888 ) ) ;
#55428 = CARTESIAN_POINT ( 'NONE',  ( -0.005480084712502889671, 28.92564299267938210, 4.000000000000000000 ) ) ;
#55429 = ORIENTED_EDGE ( 'NONE', *, *, #82284, .T. ) ;
#55430 = DIRECTION ( 'NONE',  ( 0.000000000000000000, 0.000000000000000000, -1.000000000000000000 ) ) ;
#55431 = ORIENTED_EDGE ( 'NONE', *, *, #126109, .T. ) ;
#55432 = DIRECTION ( 'NONE',  ( 0.000000000000000000, -1.000000000000000000, 0.000000000000000000 ) ) ;
#55433 = CARTESIAN_POINT ( 'NONE',  ( -29.99999999999979750, -22.06887692260758271, 4.000000000000000000 ) ) ;
#55434 = DIRECTION ( 'NONE',  ( 0.6830127018922181881, 0.6830127018922202975, -0.2588190451025214056 ) ) ;
#55435 = VECTOR ( 'NONE', #95811, 1000.000000000000000 ) ;
#55436 = VECTOR ( 'NONE', #102288, 1000.000000000000000 ) ;
#55437 = AXIS2_PLACEMENT_3D ( 'NONE', #81573, #3248, #125778 ) ;
#55438 = FACE_OUTER_BOUND ( 'NONE', #139481, .T. ) ;
#55439 = DIRECTION ( 'NONE',  ( 0.000000000000000000, 0.000000000000000000, -1.000000000000000000 ) ) ;
#55440 = FACE_OUTER_BOUND ( 'NONE', #63541, .T. ) ;
#55441 = VECTOR ( 'NONE', #33987, 1000.000000000000000 ) ;
#55442 = DIRECTION ( 'NONE',  ( 0.7071067811865487940, -0.7071067811865463515, 0.000000000000000000 ) ) ;
#55443 = LINE ( 'NONE', #111972, #136294 ) ;
#55444 = ORIENTED_EDGE ( 'NONE', *, *, #18560, .T. ) ;
#55445 = CARTESIAN_POINT ( 'NONE',  ( 25.17183060077629975, 6.759292476615649470, 4.000000000000000000 ) ) ;
#55446 = ORIENTED_EDGE ( 'NONE', *, *, #58814, .T. ) ;
#55447 = VECTOR ( 'NONE', #80444, 1000.000000000000000 ) ;
#55448 = CARTESIAN_POINT ( 'NONE',  ( -9.299744871391588674, -27.71228299555212971, 4.000000000000000000 ) ) ;
#55449 = DIRECTION ( 'NONE',  ( 0.7071067811865487940, 0.7071067811865463515, 0.000000000000000000 ) ) ;
#55450 = EDGE_CURVE ( 'NONE', #35713, #7390, #38095, .T. ) ;
#55451 = ORIENTED_EDGE ( 'NONE', *, *, #26724, .F. ) ;
#55452 = CARTESIAN_POINT ( 'NONE',  ( 14.20710678118644310, 15.75929247661555443, 5.000000000000000000 ) ) ;
#55453 = DIRECTION ( 'NONE',  ( -0.7071067811865487940, 0.7071067811865463515, 0.000000000000000000 ) ) ;
#55454 = CARTESIAN_POINT ( 'NONE',  ( -48.18398860626899705, 28.73617430169820608, 5.000000000000000000 ) ) ;
#55455 = EDGE_CURVE ( 'NONE', #127303, #9331, #58457, .T. ) ;
#55456 = EDGE_LOOP ( 'NONE', ( #113702, #73259, #69515, #418 ) ) ;
#55457 = PRESENTATION_STYLE_ASSIGNMENT (( #87369 ) ) ;
#55458 = LINE ( 'NONE', #78633, #16371 ) ;
#55459 = EDGE_CURVE ( 'NONE', #7608, #64278, #3960, .T. ) ;
#55460 = CARTESIAN_POINT ( 'NONE',  ( -20.99999999999985079, -13.39766691384885000, -10.96608748226461039 ) ) ;
#55461 = AXIS2_PLACEMENT_3D ( 'NONE', #130357, #19433, #18695 ) ;
#55462 = AXIS2_PLACEMENT_3D ( 'NONE', #65637, #22062, #9006 ) ;
#55463 = DIRECTION ( 'NONE',  ( 0.7071067811865486830, -0.7071067811865464625, -0.000000000000000000 ) ) ;
#55464 = CARTESIAN_POINT ( 'NONE',  ( 3.489213562373097322, -27.52281430457057709, 5.000000000000000000 ) ) ;
#55465 = EDGE_CURVE ( 'NONE', #115745, #65695, #80184, .T. ) ;
#55466 = CARTESIAN_POINT ( 'NONE',  ( 67.43293019189812298, 1.637169565754156730, 6.110000000000001208 ) ) ;
#55467 = CARTESIAN_POINT ( 'NONE',  ( 184.1500000000000057, -57.15000000000009095, 34.92499999999998295 ) ) ;
#55469 = CARTESIAN_POINT ( 'NONE',  ( 118.2500000000000000, -9.735942053221458872E-16, 7.950000000000000178 ) ) ;
#55468 = AXIS2_PLACEMENT_3D ( 'NONE', #111843, #58217, #90813 ) ;
#55470 = CARTESIAN_POINT ( 'NONE',  ( 32.74586038379622011, 3.974999999999996980, 6.884901960086287964 ) ) ;
#55471 = PLANE ( 'NONE',  #111272 ) ;
#55472 = ORIENTED_EDGE ( 'NONE', *, *, #26830, .F. ) ;
#55473 = DIRECTION ( 'NONE',  ( 0.7071067811865487940, 0.7071067811865463515, 0.000000000000000000 ) ) ;
#55474 = ORIENTED_EDGE ( 'NONE', *, *, #25210, .F. ) ;
#55475 = FACE_OUTER_BOUND ( 'NONE', #75291, .T. ) ;
#55476 = CARTESIAN_POINT ( 'NONE',  ( 3.489213562373097322, -27.52281430457057709, 5.000000000000000000 ) ) ;
#55477 = AXIS2_PLACEMENT_3D ( 'NONE', #94374, #29131, #95088 ) ;
#55478 = AXIS2_PLACEMENT_3D ( 'NONE', #80629, #84218, #105214 ) ;
#55479 = VECTOR ( 'NONE', #66350, 1000.000000000000000 ) ;
#55480 = LINE ( 'NONE', #133055, #46182 ) ;
#55481 = CARTESIAN_POINT ( 'NONE',  ( 13.49159235450332162, 9.902892378096218942E-16, 0.000000000000000000 ) ) ;
#55482 = EDGE_CURVE ( 'NONE', #135742, #140903, #58175, .T. ) ;
#55483 = EDGE_CURVE ( 'NONE', #70680, #136170, #122949, .T. ) ;
#55484 = CARTESIAN_POINT ( 'NONE',  ( 7.499999999999946709, 22.01701374228155572, 2.453858888625611634 ) ) ;
#55485 = LINE ( 'NONE', #69214, #128699 ) ;
#55486 = ORIENTED_EDGE ( 'NONE', *, *, #52529, .F. ) ;
#55487 = AXIS2_PLACEMENT_3D ( 'NONE', #107531, #48893, #18348 ) ;
#55488 = VERTEX_POINT ( 'NONE', #135958 ) ;
#55489 = LINE ( 'NONE', #99671, #101915 ) ;
#55490 = CARTESIAN_POINT ( 'NONE',  ( 26.65943557924714113, -6.350000000000002309, -1.701477371937631045 ) ) ;
#55491 = AXIS2_PLACEMENT_3D ( 'NONE', #24823, #124139, #123463 ) ;
#55492 = LINE ( 'NONE', #43187, #38158 ) ;
#55493 = ADVANCED_FACE ( 'NONE', ( #80884 ), #67898, .F. ) ;
#55494 = DIRECTION ( 'NONE',  ( -0.7071067811865486830, -0.7071067811865464625, 0.000000000000000000 ) ) ;
#55495 = CARTESIAN_POINT ( 'NONE',  ( 81.60002705046289861, 5.819803920172570422, 5.819803920172574863 ) ) ;
#55496 = CARTESIAN_POINT ( 'NONE',  ( -30.18398860626900060, 28.73617430169808173, 5.000000000000000000 ) ) ;
#55497 = LINE ( 'NONE', #45355, #43766 ) ;
#55498 = EDGE_LOOP ( 'NONE', ( #2068, #17184, #87312, #26398 ) ) ;
#55499 = CARTESIAN_POINT ( 'NONE',  ( 75.22916666666665719, 7.950000000000001954, -2.130196079827421762 ) ) ;
#55500 = DIRECTION ( 'NONE',  ( -0.000000000000000000, 0.000000000000000000, 1.000000000000000000 ) ) ;
#55501 = LINE ( 'NONE', #47515, #104069 ) ;
#55502 = CARTESIAN_POINT ( 'NONE',  ( 3.710381658649934078, -2.500000000000000000, 3.061616997868383634E-16 ) ) ;
#55503 = ADVANCED_FACE ( 'NONE', ( #79495 ), #112776, .F. ) ;
#55504 = VECTOR ( 'NONE', #80442, 1000.000000000000000 ) ;
#55505 = EDGE_LOOP ( 'NONE', ( #8999, #135421, #85823, #32093 ) ) ;
#55506 = PLANE ( 'NONE',  #12039 ) ;
#55507 = ORIENTED_EDGE ( 'NONE', *, *, #89308, .T. ) ;
#55508 = CARTESIAN_POINT ( 'NONE',  ( 5.848407645496676466, 9.139736423841732040E-16, 0.000000000000000000 ) ) ;
#55509 = CARTESIAN_POINT ( 'NONE',  ( 70.14626352523143282, -4.472830434245840259, 4.472830434245839371 ) ) ;
#55510 = DIRECTION ( 'NONE',  ( 0.7071067811865487940, 0.7071067811865463515, 0.000000000000000000 ) ) ;
#55511 = EDGE_CURVE ( 'NONE', #78692, #12567, #127961, .T. ) ;
#55512 = VERTEX_POINT ( 'NONE', #93876 ) ;
#55513 = DIRECTION ( 'NONE',  ( -0.000000000000000000, -0.3543493200069152693, 0.9351131265310292928 ) ) ;
#55514 = LINE ( 'NONE', #95603, #63753 ) ;
#55515 = CARTESIAN_POINT ( 'NONE',  ( -34.49999999999975131, 9.054329344830845727, 4.994342998332165884 ) ) ;
#55516 = DIRECTION ( 'NONE',  ( 0.000000000000000000, 0.000000000000000000, 1.000000000000000000 ) ) ;
#55517 = DIRECTION ( 'NONE',  ( 0.3543493200069162685, -0.000000000000000000, -0.9351131265310288487 ) ) ;
#55519 = EDGE_LOOP ( 'NONE', ( #71493, #66023, #80393 ) ) ;
#55518 = LINE ( 'NONE', #76567, #130981 ) ;
#55520 = DIRECTION ( 'NONE',  ( 0.7071067811865487940, 0.7071067811865463515, 0.000000000000000000 ) ) ;
#55521 = CARTESIAN_POINT ( 'NONE',  ( 0.000000000000000000, 0.000000000000000000, 5.000000000000000000 ) ) ;
#55522 = DIRECTION ( 'NONE',  ( -0.7071067811865486830, -0.7071067811865464625, -0.000000000000000000 ) ) ;
#55523 = EDGE_LOOP ( 'NONE', ( #127743, #32711, #62550, #60282, #142153 ) ) ;
#55524 = ADVANCED_FACE ( 'NONE', ( #63437 ), #18423, .F. ) ;
#55525 = ORIENTED_EDGE ( 'NONE', *, *, #53984, .F. ) ;
#55526 = CARTESIAN_POINT ( 'NONE',  ( 59.93793019189809712, -6.110000000000001208, 1.637169565754158951 ) ) ;
#55527 = VERTEX_POINT ( 'NONE', #116347 ) ;
#55528 = DIRECTION ( 'NONE',  ( -0.000000000000000000, -0.3543493200069152693, 0.9351131265310292928 ) ) ;
#55529 = DIRECTION ( 'NONE',  ( -0.000000000000000000, -0.3543493200069152693, 0.9351131265310292928 ) ) ;
#55530 = DIRECTION ( 'NONE',  ( -1.000000000000000000, 0.000000000000000000, -0.000000000000000000 ) ) ;
#55531 = ADVANCED_FACE ( 'NONE', ( #6112 ), #40250, .F. ) ;
#55532 = PLANE ( 'NONE',  #38796 ) ;
#55533 = DIRECTION ( 'NONE',  ( 0.000000000000000000, 1.000000000000000000, 0.000000000000000000 ) ) ;
#55534 = VERTEX_POINT ( 'NONE', #38795 ) ;
#55535 = EDGE_LOOP ( 'NONE', ( #112497, #93498, #79456, #75730 ) ) ;
#55536 = CARTESIAN_POINT ( 'NONE',  ( -24.48921356237309510, -27.52281430457072631, 5.000000000000000000 ) ) ;
#55537 = ORIENTED_EDGE ( 'NONE', *, *, #101078, .F. ) ;
#55538 = EDGE_CURVE ( 'NONE', #9860, #39432, #106737, .T. ) ;
#55539 = FACE_OUTER_BOUND ( 'NONE', #54237, .T. ) ;
#55540 = CARTESIAN_POINT ( 'NONE',  ( 111.9333603837962272, 2.130196079827431532, -7.949999999999996625 ) ) ;
#55541 = PLANE ( 'NONE',  #51572 ) ;
#55542 = AXIS2_PLACEMENT_3D ( 'NONE', #55237, #68290, #33507 ) ;
#55543 = CONICAL_SURFACE ( 'NONE', #134182, 2.055000000000000604, 0.9599310885968764806 ) ;
#55544 = CIRCLE ( 'NONE', #53125, 2.500000000000000444 ) ;
#55545 =( BOUNDED_CURVE ( )  B_SPLINE_CURVE ( 2, ( #20306, #129082, #32651, #75438, #97133, #18894, #141392, #10848, #139996, #31223, #131967, #107332, #76889 ),
 .UNSPECIFIED., .F., .T. ) 
 B_SPLINE_CURVE_WITH_KNOTS ( ( 3, 2, 2, 2, 2, 2, 3 ),
 ( 0.9000000000000001332, 0.9027777777777779011, 0.9055555555555556690, 0.9083333333333334370, 0.9111111111111110938, 0.9138888888888888618, 0.9166666666666666297 ),
 .UNSPECIFIED. ) 
 CURVE ( )  GEOMETRIC_REPRESENTATION_ITEM ( )  RATIONAL_B_SPLINE_CURVE ( ( 0.9999999999999986677, 0.9659258262890696445, 1.000000000000000000, 0.9659258262890683122, 1.000000000000000000, 0.9659258262890683122, 1.000000000000000000, 0.9659258262890683122, 1.000000000000000000, 0.9659258262890683122, 1.000000000000000000, 0.9659258262890683122, 1.000000000000000000 ) ) 
 REPRESENTATION_ITEM ( '' )  );
#55546 = EDGE_LOOP ( 'NONE', ( #142667, #113411, #54571, #77661 ) ) ;
#55547 = AXIS2_PLACEMENT_3D ( 'NONE', #135126, #91587, #3807 ) ;
#55548 = EDGE_CURVE ( 'NONE', #96695, #19121, #7169, .T. ) ;
#55549 = FACE_BOUND ( 'NONE', #85176, .T. ) ;
#55550 = CARTESIAN_POINT ( 'NONE',  ( 30.06011071044001426, -9.740707523384180888, 10.89222023123373795 ) ) ;
#55551 = CARTESIAN_POINT ( 'NONE',  ( 127.7219355792471305, -5.499261314031185677, 3.174999999999998046 ) ) ;
#55552 = CARTESIAN_POINT ( 'NONE',  ( 61.37500000000000000, 7.950000000000000178, 1.460391307983218535E-15 ) ) ;
#55553 = VECTOR ( 'NONE', #30144, 1000.000000000000227 ) ;
#55554 = CARTESIAN_POINT ( 'NONE',  ( -27.48921356237309155, -27.52281430457074762, 5.000000000000000000 ) ) ;
#55555 = SURFACE_SIDE_STYLE ('',( #110602 ) ) ;
#55556 = CARTESIAN_POINT ( 'NONE',  ( -88.78149007701877338, -5.517728913302859347E-14, 1.431893073193702213E-16 ) ) ;
#55557 = VERTEX_POINT ( 'NONE', #117051 ) ;
#55558 = VECTOR ( 'NONE', #137285, 1000.000000000000000 ) ;
#55559 = ORIENTED_EDGE ( 'NONE', *, *, #17999, .F. ) ;
#55560 = CARTESIAN_POINT ( 'NONE',  ( 100.5370968585647802, -3.054999999999998828, -5.291415217122919401 ) ) ;
#55561 = ORIENTED_EDGE ( 'NONE', *, *, #118681, .F. ) ;
#55562 = ORIENTED_EDGE ( 'NONE', *, *, #142023, .F. ) ;
#55563 = AXIS2_PLACEMENT_3D ( 'NONE', #8858, #79232, #90795 ) ;
#55564 = VECTOR ( 'NONE', #69410, 1000.000000000000000 ) ;
#55565 = DIRECTION ( 'NONE',  ( 0.000000000000000000, -1.000000000000000000, 0.000000000000000000 ) ) ;
#55566 = FACE_OUTER_BOUND ( 'NONE', #58126, .T. ) ;
#55567 = CIRCLE ( 'NONE', #131943, 2.552699999999928693 ) ;
#55568 = CARTESIAN_POINT ( 'NONE',  ( -45.29974487139158867, -27.71228299555237840, 4.000000000000000000 ) ) ;
#55569 = ORIENTED_EDGE ( 'NONE', *, *, #12886, .F. ) ;
#55570 = DIRECTION ( 'NONE',  ( 0.6830127018922180770, -0.6830127018922204085, -0.2588190451025213501 ) ) ;
#55571 = DIRECTION ( 'NONE',  ( 0.7071067811865487940, -0.7071067811865463515, 0.000000000000000000 ) ) ;
#55572 = EDGE_CURVE ( 'NONE', #138636, #19628, #62704, .T. ) ;
#55573 = CARTESIAN_POINT ( 'NONE',  ( 156.1500000000000057, -57.14999999999999147, -53.92499999999968452 ) ) ;
#55575 = DIRECTION ( 'NONE',  ( 6.694238229904089514E-15, -0.9647414015272165466, 0.2631995976047492580 ) ) ;
#55574 = CARTESIAN_POINT ( 'NONE',  ( 30.18398860626900060, 28.73617430169808173, 5.000000000000000000 ) ) ;
#55576 = PLANE ( 'NONE',  #11405 ) ;
#55577 = CARTESIAN_POINT ( 'NONE',  ( -4.912274722134691121E-20, 1.320799999999990870, 4.000000000000000000 ) ) ;
#55578 = VERTEX_POINT ( 'NONE', #52511 ) ;
#55579 = VECTOR ( 'NONE', #23177, 1000.000000000000227 ) ;
#55580 = CARTESIAN_POINT ( 'NONE',  ( 86.89583333333335702, -2.130196079827389344, 7.950000000000021494 ) ) ;
#55581 = CARTESIAN_POINT ( 'NONE',  ( -2.999999999999975131, -21.84840872380824450, 2.849755605029599348 ) ) ;
#55582 = VERTEX_POINT ( 'NONE', #72178 ) ;
#55583 = ADVANCED_FACE ( 'NONE', ( #51827 ), #129353, .F. ) ;
#55584 = ORIENTED_EDGE ( 'NONE', *, *, #110633, .F. ) ;
#55585 = VECTOR ( 'NONE', #37626, 1000.000000000000227 ) ;
#55586 = EDGE_CURVE ( 'NONE', #81677, #35253, #106886, .T. ) ;
#55587 = VERTEX_POINT ( 'NONE', #140943 ) ;
#55588 = EDGE_CURVE ( 'NONE', #6599, #20040, #61998, .T. ) ;
#55590 = CONICAL_SURFACE ( 'NONE', #115754, 2.500000000000000888, 0.9599310885968822538 ) ;
#55589 = CARTESIAN_POINT ( 'NONE',  ( 58.33376352523143993, 6.110000000000001208, 1.122388791418549305E-15 ) ) ;
#55591 = ORIENTED_EDGE ( 'NONE', *, *, #30383, .F. ) ;
#55592 = CARTESIAN_POINT ( 'NONE',  ( -15.48921356237309510, -27.52281430457066236, 5.000000000000000000 ) ) ;
#55593 =( GEOMETRIC_REPRESENTATION_CONTEXT ( 3 ) GLOBAL_UNCERTAINTY_ASSIGNED_CONTEXT ( ( #84021 ) ) GLOBAL_UNIT_ASSIGNED_CONTEXT ( ( #127952, #62696, #106878 ) ) REPRESENTATION_CONTEXT ( 'NONE', 'WORKASPACE' ) );
#55594 = CARTESIAN_POINT ( 'NONE',  ( -0.3916937171295608033, 1.633150327867687324, -6.094999999999991758 ) ) ;
#55595 = CARTESIAN_POINT ( 'NONE',  ( 91.72959685856477563, -6.110000000000000320, -1.637169565754161393 ) ) ;
#55596 = CARTESIAN_POINT ( 'NONE',  ( -34.47516574401890210, 19.49051761211541844, 4.998110765256836174 ) ) ;
#55597 = ORIENTED_EDGE ( 'NONE', *, *, #96731, .T. ) ;
#55598 = LINE ( 'NONE', #99787, #125169 ) ;
#55599 = AXIS2_PLACEMENT_3D ( 'NONE', #136576, #80105, #72092 ) ;
#55600 = LINE ( 'NONE', #9170, #19217 ) ;
#55601 = EDGE_CURVE ( 'NONE', #121901, #84862, #117740, .T. ) ;
#55602 = FACE_OUTER_BOUND ( 'NONE', #117868, .T. ) ;
#55603 = ORIENTED_EDGE ( 'NONE', *, *, #6028, .T. ) ;
#55604 = PLANE ( 'NONE',  #52721 ) ;
#55605 = CARTESIAN_POINT ( 'NONE',  ( 48.48921356237309510, -27.52281430457089328, 5.000000000000000000 ) ) ;
#55606 = EDGE_LOOP ( 'NONE', ( #90015, #125379, #122100, #83117 ) ) ;
#55607 = ORIENTED_EDGE ( 'NONE', *, *, #11354, .T. ) ;
#55608 = ORIENTED_EDGE ( 'NONE', *, *, #111181, .T. ) ;
#55609 = CARTESIAN_POINT ( 'NONE',  ( 124.3079301918981230, -6.109999999999998543, 1.637169565754158507 ) ) ;
#55610 = VECTOR ( 'NONE', #1685, 1000.000000000000227 ) ;
#55611 = CARTESIAN_POINT ( 'NONE',  ( -17.99451991528748351, 28.92564299267950645, 4.000000000000000000 ) ) ;
#55612 = CARTESIAN_POINT ( 'NONE',  ( 14.51078643762690490, -27.52281430457045275, 5.000000000000000000 ) ) ;
#55613 = ORIENTED_EDGE ( 'NONE', *, *, #17034, .F. ) ;
#55614 = LINE ( 'NONE', #132491, #46537 ) ;
#55615 = ORIENTED_EDGE ( 'NONE', *, *, #59166, .T. ) ;
#55616 = VECTOR ( 'NONE', #100579, 1000.000000000000000 ) ;
#55617 = CARTESIAN_POINT ( 'NONE',  ( 16.02040314143522082, 7.934999999999989839, -2.126176841940961904 ) ) ;
#55618 = EDGE_CURVE ( 'NONE', #26139, #83438, #5418, .T. ) ;
#55619 = LINE ( 'NONE', #54909, #52911 ) ;
#55620 = DIRECTION ( 'NONE',  ( -0.7071067811865487940, 0.7071067811865463515, 0.000000000000000000 ) ) ;
#55621 = VERTEX_POINT ( 'NONE', #74286 ) ;
#55622 = ADVANCED_FACE ( 'NONE', ( #7565 ), #30039, .F. ) ;
#55623 = ORIENTED_EDGE ( 'NONE', *, *, #88105, .F. ) ;
#55624 = ORIENTED_EDGE ( 'NONE', *, *, #106167, .F. ) ;
#55625 = CARTESIAN_POINT ( 'NONE',  ( 20.85416666666666430, 1.633150327867675555, 6.094999999999998863 ) ) ;
#55626 = PLANE ( 'NONE',  #4650 ) ;
#55627 = LINE ( 'NONE', #133893, #126026 ) ;
#55628 = CARTESIAN_POINT ( 'NONE',  ( -57.18398860626899705, 28.73617430169827358, 5.000000000000000000 ) ) ;
#55629 = EDGE_CURVE ( 'NONE', #30840, #52778, #138105, .T. ) ;
#55630 = ADVANCED_FACE ( 'NONE', ( #29328 ), #73570, .T. ) ;
#55631 = AXIS2_PLACEMENT_3D ( 'NONE', #63648, #88962, #43305 ) ;
#55632 = CARTESIAN_POINT ( 'NONE',  ( 34.82816939922328459, -5.240707523384228850, 4.000000000000000000 ) ) ;
#55633 = LINE ( 'NONE', #57793, #109677 ) ;
#55634 = CARTESIAN_POINT ( 'NONE',  ( 31.49999999999977973, -2.568876922607791879, 4.000000000000000000 ) ) ;
#55635 = DIRECTION ( 'NONE',  ( -0.000000000000000000, -0.000000000000000000, 1.000000000000000000 ) ) ;
#55636 = ORIENTED_EDGE ( 'NONE', *, *, #43042, .F. ) ;
#55637 = CARTESIAN_POINT ( 'NONE',  ( 42.18398860626899705, 28.73617430169816700, 5.000000000000000000 ) ) ;
#55638 = ORIENTED_EDGE ( 'NONE', *, *, #132761, .F. ) ;
#55639 = CIRCLE ( 'NONE', #71909, 2.500000000000000444 ) ;
#55640 = AXIS2_PLACEMENT_3D ( 'NONE', #109468, #110159, #67419 ) ;
#55641 = CARTESIAN_POINT ( 'NONE',  ( 8.816011393731004731, 28.73617430169781173, 5.000000000000000000 ) ) ;
#55642 = ORIENTED_EDGE ( 'NONE', *, *, #109229, .T. ) ;
#55643 = VECTOR ( 'NONE', #49181, 1000.000000000000000 ) ;
#55644 = PLANE ( 'NONE',  #46077 ) ;
#55646 = EDGE_LOOP ( 'NONE', ( #41986, #110789, #109872, #31438 ) ) ;
#55645 = CARTESIAN_POINT ( 'NONE',  ( 42.41666666666665719, -6.884901960086287076, -3.975000000000000977 ) ) ;
#55647 = ADVANCED_FACE ( 'NONE', ( #60581 ), #49698, .F. ) ;
#55648 = EDGE_CURVE ( 'NONE', #141315, #132971, #109022, .T. ) ;
#55649 = DIRECTION ( 'NONE',  ( -0.000000000000000000, 0.000000000000000000, 1.000000000000000000 ) ) ;
#55650 = DIRECTION ( 'NONE',  ( 0.7071067811865487940, 0.7071067811865463515, 0.000000000000000000 ) ) ;
#55651 = ORIENTED_EDGE ( 'NONE', *, *, #46310, .F. ) ;
#55652 = DIRECTION ( 'NONE',  ( 0.7071067811865486830, -0.7071067811865464625, -0.000000000000000000 ) ) ;
#55653 = VERTEX_POINT ( 'NONE', #131517 ) ;
#55654 = CARTESIAN_POINT ( 'NONE',  ( 12.32816939922344623, -21.74070752338406365, 4.000000000000000000 ) ) ;
#55655 = VECTOR ( 'NONE', #128939, 1000.000000000000000 ) ;
#55656 = ORIENTED_EDGE ( 'NONE', *, *, #108416, .T. ) ;
#55657 = DIRECTION ( 'NONE',  ( -0.7071067811865486830, -0.7071067811865464625, -0.000000000000000000 ) ) ;
#55658 = CARTESIAN_POINT ( 'NONE',  ( 112.3708603837962272, 6.884901960086289741, -3.974999999999993427 ) ) ;
#55659 = EDGE_CURVE ( 'NONE', #106208, #55894, #122036, .T. ) ;
#55660 = CARTESIAN_POINT ( 'NONE',  ( 26.99451991528749417, 28.92564299267956685, 4.000000000000000000 ) ) ;
#55661 = DIRECTION ( 'NONE',  ( 0.7071067811865487940, 0.7071067811865463515, 0.000000000000000000 ) ) ;
#55662 = DIRECTION ( 'NONE',  ( 0.000000000000000000, 1.000000000000000000, 0.000000000000000000 ) ) ;
#55663 = LINE ( 'NONE', #54954, #69351 ) ;
#55664 = CARTESIAN_POINT ( 'NONE',  ( 14.43749999999999822, -4.461849672132299105, 4.461849672132299993 ) ) ;
#55666 = VECTOR ( 'NONE', #16549, 1000.000000000000000 ) ;
#55665 = CARTESIAN_POINT ( 'NONE',  ( 23.45790314143522437, 6.871911579029515771, 3.967499999999989146 ) ) ;
#55667 = EDGE_CURVE ( 'NONE', #39610, #14791, #87298, .T. ) ;
#55668 = DIRECTION ( 'NONE',  ( -0.3543493200069162685, -0.000000000000000000, -0.9351131265310288487 ) ) ;
#55669 = CARTESIAN_POINT ( 'NONE',  ( 5.510786437626906675, -27.52281430457051314, 5.000000000000000000 ) ) ;
#55670 = EDGE_LOOP ( 'NONE', ( #73152, #23853, #80217, #84097 ) ) ;
#55671 = ORIENTED_EDGE ( 'NONE', *, *, #79862, .T. ) ;
#55672 = VECTOR ( 'NONE', #108234, 1000.000000000000000 ) ;
#55673 = CARTESIAN_POINT ( 'NONE',  ( -16.49999999999988631, -8.568876922607724822, 4.000000000000000000 ) ) ;
#55674 = VERTEX_POINT ( 'NONE', #9712 ) ;
#55675 = VECTOR ( 'NONE', #105295, 1000.000000000000227 ) ;
#55676 = CARTESIAN_POINT ( 'NONE',  ( 105.1462635252314612, -4.472830434245840259, 4.472830434245839371 ) ) ;
#55677 = VECTOR ( 'NONE', #74203, 1000.000000000000000 ) ;
#55678 = DIRECTION ( 'NONE',  ( 0.3543493200069162685, -0.000000000000000000, -0.9351131265310288487 ) ) ;
#55679 = DIRECTION ( 'NONE',  ( 0.7071067811865486830, -0.7071067811865464625, -0.000000000000000000 ) ) ;
#55680 = EDGE_CURVE ( 'NONE', #48488, #118031, #25828, .T. ) ;
#55681 = LINE ( 'NONE', #99879, #60947 ) ;
#55682 = FILL_AREA_STYLE_COLOUR ( '', #64149 ) ;
#55683 = ORIENTED_EDGE ( 'NONE', *, *, #16193, .F. ) ;
#55684 = VECTOR ( 'NONE', #91648, 1000.000000000000000 ) ;
#55685 = CARTESIAN_POINT ( 'NONE',  ( -21.70710678118638626, -12.74070752338415424, 5.000000000000000000 ) ) ;
#55686 = CARTESIAN_POINT ( 'NONE',  ( 18.95159235450331892, -2.500000000000000000, 3.061616997868384127E-16 ) ) ;
#55687 = DIRECTION ( 'NONE',  ( -0.7071067811865487940, 0.7071067811865463515, 0.000000000000000000 ) ) ;
#55688 = STYLED_ITEM ( 'NONE', ( #22942 ), #81831 ) ;
#55689 = SURFACE_SIDE_STYLE ('',( #23002 ) ) ;
#55692 = VERTEX_POINT ( 'NONE', #76432 ) ;
#55691 = EDGE_CURVE ( 'NONE', #106470, #119037, #43792, .T. ) ;
#55690 = DIRECTION ( 'NONE',  ( 0.7071067811865487940, -0.7071067811865463515, 0.000000000000000000 ) ) ;
#55693 = FACE_OUTER_BOUND ( 'NONE', #41242, .T. ) ;
#55694 = ADVANCED_FACE ( 'NONE', ( #19876 ), #120602, .F. ) ;
#55695 = CARTESIAN_POINT ( 'NONE',  ( 21.18398860626899349, 28.73617430169802134, 5.000000000000000000 ) ) ;
#55696 = DIRECTION ( 'NONE',  ( -8.817971600062198362E-18, -0.3543493200069152693, 0.9351131265310292928 ) ) ;
#55697 = CARTESIAN_POINT ( 'NONE',  ( 11.70025512860841133, -27.71228299555198049, 4.000000000000000000 ) ) ;
#55698 = DIRECTION ( 'NONE',  ( -0.6830127018922181881, 0.6830127018922202975, -0.2588190451025214056 ) ) ;
#55699 = ORIENTED_EDGE ( 'NONE', *, *, #132401, .F. ) ;
#55700 = ADVANCED_FACE ( 'NONE', ( #10424 ), #98174, .F. ) ;
#55701 = ORIENTED_EDGE ( 'NONE', *, *, #73165, .T. ) ;
#55702 = ORIENTED_EDGE ( 'NONE', *, *, #84282, .T. ) ;
#55703 = CARTESIAN_POINT ( 'NONE',  ( 90.27126352523143282, 4.472830434245839371, 4.472830434245842035 ) ) ;
#55704 = VECTOR ( 'NONE', #119102, 1000.000000000000227 ) ;
#55705 = VERTEX_POINT ( 'NONE', #243 ) ;
#55706 = CARTESIAN_POINT ( 'NONE',  ( 1.171830600776462061, -8.240707523384200428, 4.000000000000000000 ) ) ;
#55707 = CARTESIAN_POINT ( 'NONE',  ( 3.005480084712505828, 28.92564299267936079, 4.000000000000000000 ) ) ;
#55708 = CARTESIAN_POINT ( 'NONE',  ( 0.000000000000000000, 0.000000000000000000, 5.000000000000000000 ) ) ;
#55709 = PLANE ( 'NONE',  #121840 ) ;
#55710 = EDGE_LOOP ( 'NONE', ( #35453, #35719, #58700, #48298 ) ) ;
#55711 = CARTESIAN_POINT ( 'NONE',  ( -16.82816939922341248, 15.75929247661555443, 4.000000000000000000 ) ) ;
#55712 = CARTESIAN_POINT ( 'NONE',  ( 49.85416666666665719, -2.130196079827501698, -7.949999999999956657 ) ) ;
#55713 = CARTESIAN_POINT ( 'NONE',  ( 84.49543019189812298, 5.291415217122916737, 3.055000000000001936 ) ) ;
#55714 = ORIENTED_EDGE ( 'NONE', *, *, #41990, .F. ) ;
#55715 = CARTESIAN_POINT ( 'NONE',  ( 34.92499999999998295, 22.22500000000000142, 4.500000000000000888 ) ) ;
#55716 = DIRECTION ( 'NONE',  ( -1.000000000000000000, -0.000000000000000000, -0.000000000000000000 ) ) ;
#55717 = VECTOR ( 'NONE', #13832, 1000.000000000000000 ) ;
#55718 = ORIENTED_EDGE ( 'NONE', *, *, #69315, .F. ) ;
#55719 = VERTEX_POINT ( 'NONE', #88005 ) ;
#55720 = EDGE_LOOP ( 'NONE', ( #69471, #136992, #31825, #75350, #28730, #140338, #26167 ) ) ;
#55721 = PLANE ( 'NONE',  #113980 ) ;
#55722 = LINE ( 'NONE', #53575, #43120 ) ;
#55723 = CARTESIAN_POINT ( 'NONE',  ( 15.08790314143521982, 6.871911579029515771, 3.967499999999989146 ) ) ;
#55724 = CARTESIAN_POINT ( 'NONE',  ( -2.207106781186525701, 0.7592924766157052030, 5.000000000000000000 ) ) ;
#55725 = VECTOR ( 'NONE', #111070, 1000.000000000000000 ) ;
#55726 = VECTOR ( 'NONE', #32628, 1000.000000000000000 ) ;
#55727 = CARTESIAN_POINT ( 'NONE',  ( 165.1810627992761340, 26.96999999999993847, 33.99267764067941755 ) ) ;
#55728 = DIRECTION ( 'NONE',  ( -0.3543493200069162685, -0.000000000000000000, -0.9351131265310288487 ) ) ;
#55729 = CARTESIAN_POINT ( 'NONE',  ( 2.139447441471317379, 3.061616997868383141E-16, -2.500000000000000444 ) ) ;
#55730 = ORIENTED_EDGE ( 'NONE', *, *, #120508, .F. ) ;
#55731 = ORIENTED_EDGE ( 'NONE', *, *, #39218, .T. ) ;
#55732 = FACE_OUTER_BOUND ( 'NONE', #15653, .T. ) ;
#55733 = ORIENTED_EDGE ( 'NONE', *, *, #137999, .T. ) ;
#55734 = EDGE_LOOP ( 'NONE', ( #138827, #103108, #109318, #66045 ) ) ;
#55735 = AXIS2_PLACEMENT_3D ( 'NONE', #133522, #69716, #113167 ) ;
#55736 = COLOUR_RGB ( '', 0.66274510, 0.83137255, 0.94901961) ;
#55737 = AXIS2_PLACEMENT_3D ( 'NONE', #10392, #130795, #74987 ) ;
#55738 = DIRECTION ( 'NONE',  ( -1.000000000000000000, -1.224606353822377258E-16, -0.000000000000000000 ) ) ;
#55739 = ORIENTED_EDGE ( 'NONE', *, *, #103877, .F. ) ;
#55740 = CARTESIAN_POINT ( 'NONE',  ( 57.24586038379622721, 3.974999999999996980, 6.884901960086287964 ) ) ;
#55741 = CARTESIAN_POINT ( 'NONE',  ( -3.707013264293017141, -21.74070752338405299, 4.999753212805222446 ) ) ;
#55742 = FACE_OUTER_BOUND ( 'NONE', #90857, .T. ) ;
#55743 = CARTESIAN_POINT ( 'NONE',  ( 18.00548008471250583, 28.92564299267925776, 4.000000000000000000 ) ) ;
#55744 = CIRCLE ( 'NONE', #2504, 2.500000000000000444 ) ;
#55745 = AXIS2_PLACEMENT_3D ( 'NONE', #74549, #115852, #139084 ) ;
#55746 = VECTOR ( 'NONE', #60825, 1000.000000000000000 ) ;
#55747 = VECTOR ( 'NONE', #127733, 1000.000000000000000 ) ;
#55748 = DIRECTION ( 'NONE',  ( 0.000000000000000000, 1.000000000000000000, 0.000000000000000000 ) ) ;
#55749 = ORIENTED_EDGE ( 'NONE', *, *, #116715, .T. ) ;
#55750 = AXIS2_PLACEMENT_3D ( 'NONE', #78595, #100352, #56167 ) ;
#55751 = SURFACE_STYLE_USAGE ( .BOTH. , #22352 ) ;
#55752 = ORIENTED_EDGE ( 'NONE', *, *, #14030, .T. ) ;
#55753 = EDGE_CURVE ( 'NONE', #38181, #23998, #14238, .T. ) ;
#55754 = CARTESIAN_POINT ( 'NONE',  ( 28.60343192894626441, -14.24070752338413293, 19.24067776001732355 ) ) ;
#55755 = ORIENTED_EDGE ( 'NONE', *, *, #140199, .F. ) ;
#55756 = DIRECTION ( 'NONE',  ( -1.000000000000000000, -1.224606353822377258E-16, -0.000000000000000000 ) ) ;
#55757 = ORIENTED_EDGE ( 'NONE', *, *, #103576, .T. ) ;
#55759 = EDGE_CURVE ( 'NONE', #53631, #131121, #130826, .T. ) ;
#55758 = CARTESIAN_POINT ( 'NONE',  ( 30.18398860626900060, 28.73617430169808173, 5.000000000000000000 ) ) ;
#55760 = EDGE_LOOP ( 'NONE', ( #2660, #11777, #100213, #108739 ) ) ;
#55761 = ORIENTED_EDGE ( 'NONE', *, *, #49765, .T. ) ;
#55762 = VECTOR ( 'NONE', #104132, 999.9999999999998863 ) ;
#55763 = ORIENTED_EDGE ( 'NONE', *, *, #96244, .T. ) ;
#55764 = DIRECTION ( 'NONE',  ( 0.7071067811865486830, -0.7071067811865464625, -0.000000000000000000 ) ) ;
#55765 = CARTESIAN_POINT ( 'NONE',  ( 42.48921356237308800, -27.52281430457085065, 5.000000000000000000 ) ) ;
#55766 = CARTESIAN_POINT ( 'NONE',  ( 156.1499999999997783, -49.14999999999999147, 34.92500000000004690 ) ) ;
#55767 = DIRECTION ( 'NONE',  ( -0.6830127018922181881, 0.6830127018922202975, -0.2588190451025214056 ) ) ;
#55768 = EDGE_CURVE ( 'NONE', #103662, #138649, #121335, .T. ) ;
#55769 = CIRCLE ( 'NONE', #41885, 28.00000000000003197 ) ;
#55770 = CARTESIAN_POINT ( 'NONE',  ( 0.000000000000000000, 0.000000000000000000, 5.000000000000000000 ) ) ;
#55771 = FACE_OUTER_BOUND ( 'NONE', #7370, .T. ) ;
#55772 = AXIS2_PLACEMENT_3D ( 'NONE', #10659, #44043, #142637 ) ;
#55773 = FACE_OUTER_BOUND ( 'NONE', #10441, .T. ) ;
#55774 = ADVANCED_FACE ( 'NONE', ( #119883 ), #22021, .F. ) ;
#55775 = VECTOR ( 'NONE', #48396, 1000.000000000000227 ) ;
#55776 = CARTESIAN_POINT ( 'NONE',  ( -51.48921356237309510, -27.52281430457091460, 5.000000000000000000 ) ) ;
#55777 = VERTEX_POINT ( 'NONE', #66269 ) ;
#55778 = DIRECTION ( 'NONE',  ( 0.6830127018922181881, 0.6830127018922202975, -0.2588190451025214056 ) ) ;
#55779 = DIRECTION ( 'NONE',  ( -0.6830127018922180770, -0.6830127018922204085, -0.2588190451025213501 ) ) ;
#55780 = ORIENTED_EDGE ( 'NONE', *, *, #77263, .T. ) ;
#55781 = VECTOR ( 'NONE', #889, 1000.000000000000227 ) ;
#55782 = ORIENTED_EDGE ( 'NONE', *, *, #88853, .T. ) ;
#55783 = EDGE_LOOP ( 'NONE', ( #140107, #67204, #124750, #79497, #61245, #30876 ) ) ;
#55784 = CARTESIAN_POINT ( 'NONE',  ( 174.7500000000000000, 7.919999999999947526, 16.57230000000005532 ) ) ;
#55785 = EDGE_CURVE ( 'NONE', #19566, #108338, #11117, .T. ) ;
#55786 = VERTEX_POINT ( 'NONE', #44542 ) ;
#55787 = ORIENTED_EDGE ( 'NONE', *, *, #135183, .F. ) ;
#55788 = DIRECTION ( 'NONE',  ( 0.7071067811865487940, 0.7071067811865463515, 0.000000000000000000 ) ) ;
#55789 = CARTESIAN_POINT ( 'NONE',  ( 34.92499999999998295, 22.22500000000000142, 4.000000000000000000 ) ) ;
#55790 = PLANE ( 'NONE',  #34074 ) ;
#55791 = VECTOR ( 'NONE', #71332, 1000.000000000000000 ) ;
#55792 = CARTESIAN_POINT ( 'NONE',  ( -11.21342912940201764, -22.22500000000000142, -3.985200587934857541 ) ) ;
#55793 = CARTESIAN_POINT ( 'NONE',  ( -4.265066702820487166, 12.75929247661558996, 18.34774599283957386 ) ) ;
#55794 = ORIENTED_EDGE ( 'NONE', *, *, #79856, .F. ) ;
#55795 = DIRECTION ( 'NONE',  ( 0.7071067811865487940, 0.7071067811865463515, -0.000000000000000000 ) ) ;
#55796 = EDGE_CURVE ( 'NONE', #40167, #25993, #85854, .T. ) ;
#55797 = ORIENTED_EDGE ( 'NONE', *, *, #118797, .F. ) ;
#55798 = FILL_AREA_STYLE ('',( #142782 ) ) ;
#55799 = VECTOR ( 'NONE', #44442, 1000.000000000000000 ) ;
#55800 = CARTESIAN_POINT ( 'NONE',  ( 18.29623647476855197, 7.934999999999990727, -1.457635852685135314E-15 ) ) ;
#55801 = VERTEX_POINT ( 'NONE', #130091 ) ;
#55802 = CARTESIAN_POINT ( 'NONE',  ( 79.68293019189812298, -1.637169565754159173, -6.109999999999999432 ) ) ;
#55803 = CARTESIAN_POINT ( 'NONE',  ( 10.77958563595370833, 2.500000000000000888, 0.000000000000000000 ) ) ;
#55804 = LINE ( 'NONE', #110833, #95128 ) ;
#55805 = ORIENTED_EDGE ( 'NONE', *, *, #114669, .T. ) ;
#55806 = EDGE_CURVE ( 'NONE', #110443, #65489, #132973, .T. ) ;
#55807 = ORIENTED_EDGE ( 'NONE', *, *, #98234, .F. ) ;
#55808 = MECHANICAL_DESIGN_GEOMETRIC_PRESENTATION_REPRESENTATION (  '', ( #25663 ), #102160 ) ;
#55809 = VERTEX_POINT ( 'NONE', #64118 ) ;
#55810 = CARTESIAN_POINT ( 'NONE',  ( 20.99999999999985079, -5.527737879153171718, -7.983877177622420440 ) ) ;
#55811 = CARTESIAN_POINT ( 'NONE',  ( -10.49999999999992184, 4.466399257802213363, 5.000000000000000000 ) ) ;
#55812 = CARTESIAN_POINT ( 'NONE',  ( 16.96306865584292467, -0.7331570413090292559, -35.15540272813352374 ) ) ;
#55813 = CARTESIAN_POINT ( 'NONE',  ( 34.92499999999998295, -21.72500000000000142, 5.000000000000000000 ) ) ;
#55814 = VECTOR ( 'NONE', #112327, 999.9999999999998863 ) ;
#55815 = LINE ( 'NONE', #100019, #116798 ) ;
#55816 = ORIENTED_EDGE ( 'NONE', *, *, #1767, .F. ) ;
#55817 = EDGE_CURVE ( 'NONE', #72918, #121606, #119193, .T. ) ;
#55818 = EDGE_CURVE ( 'NONE', #52838, #99485, #64837, .T. ) ;
#55819 = DIRECTION ( 'NONE',  ( -0.000000000000000000, -0.000000000000000000, -1.000000000000000000 ) ) ;
#55820 = DIRECTION ( 'NONE',  ( -0.7071067811865486830, -0.7071067811865464625, 0.000000000000000000 ) ) ;
#55821 = ORIENTED_EDGE ( 'NONE', *, *, #140099, .F. ) ;
#55822 = CARTESIAN_POINT ( 'NONE',  ( 25.39999999999999858, -14.29000000000013593, 12.69999999999954632 ) ) ;
#55823 = VECTOR ( 'NONE', #47621, 1000.000000000000000 ) ;
#55825 = ADVANCED_FACE ( 'NONE', ( #90885 ), #70581, .F. ) ;
#55824 = CARTESIAN_POINT ( 'NONE',  ( 25.39999999999999858, -2.600000000000056044, -28.92500000000001492 ) ) ;
#55826 = EDGE_LOOP ( 'NONE', ( #45605, #12712, #141358, #54487 ) ) ;
#55828 = VERTEX_POINT ( 'NONE', #112613 ) ;
#55827 = DIRECTION ( 'NONE',  ( -0.3543493200069162685, -0.000000000000000000, -0.9351131265310288487 ) ) ;
#55830 = ORIENTED_EDGE ( 'NONE', *, *, #34768, .F. ) ;
#55829 = EDGE_CURVE ( 'NONE', #134528, #33663, #35804, .T. ) ;
#55831 = EDGE_CURVE ( 'NONE', #41910, #64188, #114727, .T. ) ;
#55832 = CARTESIAN_POINT ( 'NONE',  ( -48.18398860626899705, 28.73617430169820608, 5.000000000000000000 ) ) ;
#55833 = DIRECTION ( 'NONE',  ( 0.7071067811865487940, -0.7071067811865463515, 0.000000000000000000 ) ) ;
#55835 = ORIENTED_EDGE ( 'NONE', *, *, #67569, .T. ) ;
#55834 = VECTOR ( 'NONE', #53722, 1000.000000000000000 ) ;
#55836 = CARTESIAN_POINT ( 'NONE',  ( 7.939999999999994174, -35.56014942880460694, -10.00000000000000178 ) ) ;
#55837 = PLANE ( 'NONE',  #27696 ) ;
#55838 = EDGE_CURVE ( 'NONE', #20875, #1659, #971, .T. ) ;
#55839 = LINE ( 'NONE', #696, #99409 ) ;
#55840 = DIRECTION ( 'NONE',  ( -0.6830127018922180770, -0.6830127018922204085, -0.2588190451025213501 ) ) ;
#55841 = LINE ( 'NONE', #44250, #70010 ) ;
#55842 = CARTESIAN_POINT ( 'NONE',  ( 72.48921356237309510, -27.52281430457106026, 5.000000000000000000 ) ) ;
#55843 = DIRECTION ( 'NONE',  ( -1.000000000000000000, -0.000000000000000000, -0.000000000000000000 ) ) ;
#55844 = CARTESIAN_POINT ( 'NONE',  ( 20.97873647476855652, -5.808823158059033709, 5.808823158059035485 ) ) ;
#55845 = PLANE ( 'NONE',  #88527 ) ;
#55846 = DIRECTION ( 'NONE',  ( 0.000000000000000000, 0.000000000000000000, -1.000000000000000000 ) ) ;
#55848 = EDGE_CURVE ( 'NONE', #121372, #117339, #51309, .T. ) ;
#55847 = VECTOR ( 'NONE', #37789, 1000.000000000000000 ) ;
#55849 = DIRECTION ( 'NONE',  ( -0.6830127018922180770, -0.6830127018922204085, -0.2588190451025213501 ) ) ;
#55850 = CARTESIAN_POINT ( 'NONE',  ( -34.49999999999976552, 8.900465351122123892, -2.516491619111432154 ) ) ;
#55851 = EDGE_LOOP ( 'NONE', ( #73952, #100512, #53176, #127557 ) ) ;
#55852 = VERTEX_POINT ( 'NONE', #123522 ) ;
#55853 = VECTOR ( 'NONE', #60777, 1000.000000000000000 ) ;
#55854 = CARTESIAN_POINT ( 'NONE',  ( 102.3541666666666714, -2.130196079827425315, -7.950000000000001066 ) ) ;
#55855 = VECTOR ( 'NONE', #71239, 1000.000000000000000 ) ;
#55856 = EDGE_LOOP ( 'NONE', ( #94381, #65888, #44744, #123662 ) ) ;
#55857 = ORIENTED_EDGE ( 'NONE', *, *, #96098, .T. ) ;
#55858 = ORIENTED_EDGE ( 'NONE', *, *, #14695, .T. ) ;
#55859 = FACE_OUTER_BOUND ( 'NONE', #10216, .T. ) ;
#55860 = DIRECTION ( 'NONE',  ( 0.7071067811865487940, 0.7071067811865463515, 0.000000000000000000 ) ) ;
#55861 = MECHANICAL_DESIGN_GEOMETRIC_PRESENTATION_REPRESENTATION (  '', ( #92867 ), #32774 ) ;
#55862 = CIRCLE ( 'NONE', #21050, 0.5000000000000004441 ) ;
#55863 = VECTOR ( 'NONE', #139989, 1000.000000000000227 ) ;
#55864 = VECTOR ( 'NONE', #109355, 1000.000000000000000 ) ;
#55865 = ORIENTED_EDGE ( 'NONE', *, *, #54482, .T. ) ;
#55866 = LINE ( 'NONE', #88485, #18476 ) ;
#55867 = VECTOR ( 'NONE', #127077, 1000.000000000000000 ) ;
#55868 = CARTESIAN_POINT ( 'NONE',  ( 13.10332671766740020, 3.690788593506699300, 4.000000000000000000 ) ) ;
#55869 = CARTESIAN_POINT ( 'NONE',  ( -28.49999999999979750, 1.466399257802248446, 5.000000000000000000 ) ) ;
#55870 = ORIENTED_EDGE ( 'NONE', *, *, #90630, .T. ) ;
#55871 = DIRECTION ( 'NONE',  ( -0.6830127018922181881, 0.6830127018922202975, -0.2588190451025214056 ) ) ;
#55872 = FACE_OUTER_BOUND ( 'NONE', #138437, .T. ) ;
#55873 = AXIS2_PLACEMENT_3D ( 'NONE', #136612, #94527, #70691 ) ;
#55874 = CARTESIAN_POINT ( 'NONE',  ( 34.92499999999998295, 14.71849043720411387, 4.759050581649326261 ) ) ;
#55875 = LINE ( 'NONE', #122515, #61492 ) ;
#55876 = DIRECTION ( 'NONE',  ( 1.000000000000000000, 0.000000000000000000, 0.000000000000000000 ) ) ;
#55877 = CARTESIAN_POINT ( 'NONE',  ( -25.39999999999996305, 0.000000000000000000, 2.500000000000000000 ) ) ;
#55878 = CARTESIAN_POINT ( 'NONE',  ( 85.97502705046289861, -5.819803920172573086, 5.819803920172573086 ) ) ;
#55879 = CARTESIAN_POINT ( 'NONE',  ( -60.18398860626900415, 28.73617430169829490, 5.000000000000000000 ) ) ;
#55880 = EDGE_CURVE ( 'NONE', #42960, #39646, #25586, .T. ) ;
#55881 = EDGE_CURVE ( 'NONE', #131796, #88687, #26324, .T. ) ;
#55882 = ORIENTED_EDGE ( 'NONE', *, *, #25225, .F. ) ;
#55883 = ORIENTED_EDGE ( 'NONE', *, *, #119868, .F. ) ;
#55884 = CARTESIAN_POINT ( 'NONE',  ( 120.6045968585647614, 1.637169565754164946, -6.109999999999999432 ) ) ;
#55885 = ORIENTED_EDGE ( 'NONE', *, *, #99427, .F. ) ;
#55886 = AXIS2_PLACEMENT_3D ( 'NONE', #101180, #1821, #35252 ) ;
#55887 = CARTESIAN_POINT ( 'NONE',  ( -3.183988606268992161, 28.73617430169789699, 5.000000000000000000 ) ) ;
#55888 = CARTESIAN_POINT ( 'NONE',  ( 12.48921356237309155, -27.52281430457064104, 5.000000000000000000 ) ) ;
#55889 = EDGE_CURVE ( 'NONE', #91367, #49119, #134380, .T. ) ;
#55890 = CARTESIAN_POINT ( 'NONE',  ( 42.48921356237308800, -27.52281430457085065, 5.000000000000000000 ) ) ;
#55891 = VECTOR ( 'NONE', #92987, 1000.000000000000227 ) ;
#55892 = AXIS2_PLACEMENT_3D ( 'NONE', #4827, #36108, #58616 ) ;
#55893 = CARTESIAN_POINT ( 'NONE',  ( 110.1620968585647944, -5.291415217122919401, 3.054999999999997939 ) ) ;
#55894 = VERTEX_POINT ( 'NONE', #24181 ) ;
#55895 = VECTOR ( 'NONE', #56511, 1000.000000000000000 ) ;
#55896 = ORIENTED_EDGE ( 'NONE', *, *, #39376, .F. ) ;
#55897 = DIRECTION ( 'NONE',  ( -0.7071067811865486830, -0.7071067811865464625, -0.000000000000000000 ) ) ;
#55898 = LINE ( 'NONE', #100096, #24604 ) ;
#55899 = ORIENTED_EDGE ( 'NONE', *, *, #99142, .T. ) ;
#55900 = ORIENTED_EDGE ( 'NONE', *, *, #23027, .F. ) ;
#55901 = CARTESIAN_POINT ( 'NONE',  ( 36.75043019189811133, 3.055000000000002824, -5.291415217122919401 ) ) ;
#55902 = ORIENTED_EDGE ( 'NONE', *, *, #36949, .T. ) ;
#55903 = VECTOR ( 'NONE', #99289, 1000.000000000000227 ) ;
#55904 = LINE ( 'NONE', #100810, #30589 ) ;
#55905 = FACE_OUTER_BOUND ( 'NONE', #134167, .T. ) ;
#55906 = DIRECTION ( 'NONE',  ( -0.7071067811865486830, -0.7071067811865464625, 0.000000000000000000 ) ) ;
#55907 = CARTESIAN_POINT ( 'NONE',  ( 33.89126352523143737, -4.472830434245839371, -4.472830434245839371 ) ) ;
#55908 = ORIENTED_EDGE ( 'NONE', *, *, #1009, .F. ) ;
#55909 = CARTESIAN_POINT ( 'NONE',  ( 1.499999999999996225, -4.912538124160712449, 4.000000000000000000 ) ) ;
#55911 = EDGE_CURVE ( 'NONE', #6161, #14902, #114033, .T. ) ;
#55910 = VERTEX_POINT ( 'NONE', #15398 ) ;
#55912 = ORIENTED_EDGE ( 'NONE', *, *, #132742, .F. ) ;
#55913 = VECTOR ( 'NONE', #129135, 1000.000000000000000 ) ;
#55914 = ORIENTED_EDGE ( 'NONE', *, *, #99097, .T. ) ;
#55915 = AXIS2_PLACEMENT_3D ( 'NONE', #35331, #79574, #123759 ) ;
#55916 = CARTESIAN_POINT ( 'NONE',  ( -14.99451991528749595, 28.92564299267948513, 4.000000000000000000 ) ) ;
#55917 = ORIENTED_EDGE ( 'NONE', *, *, #793, .F. ) ;
#55918 = CARTESIAN_POINT ( 'NONE',  ( -34.91107144025656339, 21.84219451764876396, 4.000000000000000000 ) ) ;
#55919 = LINE ( 'NONE', #89243, #91818 ) ;
#55920 = VECTOR ( 'NONE', #135681, 1000.000000000000000 ) ;
#55921 =( NAMED_UNIT ( * ) PLANE_ANGLE_UNIT ( ) SI_UNIT ( $, .RADIAN. ) );
#55922 = FACE_OUTER_BOUND ( 'NONE', #126928, .T. ) ;
#55923 = ADVANCED_FACE ( 'NONE', ( #24881 ), #80029, .F. ) ;
#55924 = FACE_BOUND ( 'NONE', #50090, .T. ) ;
#55925 = ORIENTED_EDGE ( 'NONE', *, *, #85267, .T. ) ;
#55926 = CARTESIAN_POINT ( 'NONE',  ( -3.299744871391591339, -27.71228299555208352, 4.000000000000000000 ) ) ;
#55927 = ADVANCED_FACE ( 'NONE', ( #89426 ), #113306, .F. ) ;
#55929 = EDGE_CURVE ( 'NONE', #23492, #27958, #59681, .T. ) ;
#55928 = LINE ( 'NONE', #100832, #55436 ) ;
#55930 = CARTESIAN_POINT ( 'NONE',  ( -34.92500000000001137, 22.22500000000000142, 4.000000000000000000 ) ) ;
#55931 = DIRECTION ( 'NONE',  ( 0.7071067811865486830, -0.7071067811865464625, -0.000000000000000000 ) ) ;
#55932 = EDGE_LOOP ( 'NONE', ( #57464, #130674, #66089, #121781 ) ) ;
#55933 = CARTESIAN_POINT ( 'NONE',  ( 18.48921356237309510, -27.52281430457068367, 5.000000000000000000 ) ) ;
#55934 = ORIENTED_EDGE ( 'NONE', *, *, #57252, .T. ) ;
#55935 = VERTEX_POINT ( 'NONE', #3121 ) ;
#55936 = ORIENTED_EDGE ( 'NONE', *, *, #112084, .F. ) ;
#55937 = EDGE_CURVE ( 'NONE', #77443, #133096, #47411, .T. ) ;
#55938 = EDGE_CURVE ( 'NONE', #64078, #142188, #45257, .T. ) ;
#55939 = CARTESIAN_POINT ( 'NONE',  ( 50.22459685856478018, -1.637169565754160949, 6.109999999999997655 ) ) ;
#55940 = ORIENTED_EDGE ( 'NONE', *, *, #24077, .F. ) ;
#55941 = DIRECTION ( 'NONE',  ( -0.7071067811865486830, -0.7071067811865464625, 0.000000000000000000 ) ) ;
#55942 = ADVANCED_FACE ( 'NONE', ( #34339 ), #103158, .T. ) ;
#55943 = CARTESIAN_POINT ( 'NONE',  ( -32.99451991528749062, 28.92564299267960948, 4.000000000000000000 ) ) ;
#55944 = ORIENTED_EDGE ( 'NONE', *, *, #10881, .T. ) ;
#55945 = CARTESIAN_POINT ( 'NONE',  ( -36.18398860626899705, 28.73617430169812437, 5.000000000000000000 ) ) ;
#55946 = CARTESIAN_POINT ( 'NONE',  ( -11.56319896779163159, -12.74070752338414891, 9.898150129686403176 ) ) ;
#55947 = AXIS2_PLACEMENT_3D ( 'NONE', #67960, #33184, #25100 ) ;
#55948 =( BOUNDED_CURVE ( )  B_SPLINE_CURVE ( 3, ( #111760, #37778, #137079, #48644 ),
 .UNSPECIFIED., .F., .F. ) 
 B_SPLINE_CURVE_WITH_KNOTS ( ( 4, 4 ),
 ( 5.106027341939290309, 6.645403452391243526 ),
 .UNSPECIFIED. ) 
 CURVE ( )  GEOMETRIC_REPRESENTATION_ITEM ( )  RATIONAL_B_SPLINE_CURVE ( ( 1.000000000000000000, 0.8120851936182305053, 0.8120851936182305053, 1.000000000000000000 ) ) 
 REPRESENTATION_ITEM ( '' )  );
#55949 = COLOUR_RGB ( '', 0.66274510, 0.83137255, 0.94901961) ;
#55950 = EDGE_CURVE ( 'NONE', #113151, #36832, #135796, .T. ) ;
#55951 = AXIS2_PLACEMENT_3D ( 'NONE', #6098, #127948, #92418 ) ;
#55952 = CARTESIAN_POINT ( 'NONE',  ( -33.48921356237309510, -27.52281430457078670, 5.000000000000000000 ) ) ;
#55953 = FACE_OUTER_BOUND ( 'NONE', #23582, .T. ) ;
#55954 = DIRECTION ( 'NONE',  ( -0.6830127018922180770, -0.6830127018922204085, -0.2588190451025213501 ) ) ;
#55955 = CARTESIAN_POINT ( 'NONE',  ( -30.29974487139158867, -27.71228299555227537, 4.000000000000000000 ) ) ;
#55956 = SURFACE_STYLE_FILL_AREA ( #11669 ) ;
#55957 = ORIENTED_EDGE ( 'NONE', *, *, #77766, .F. ) ;
#55958 = EDGE_LOOP ( 'NONE', ( #15599, #63726, #124141, #54735 ) ) ;
#55959 = VECTOR ( 'NONE', #87538, 1000.000000000000000 ) ;
#55960 = AXIS2_PLACEMENT_3D ( 'NONE', #33920, #9244, #131797 ) ;
#55961 = EDGE_LOOP ( 'NONE', ( #89387, #137964, #46615 ) ) ;
#55962 = VECTOR ( 'NONE', #143353, 1000.000000000000000 ) ;
#55963 = ORIENTED_EDGE ( 'NONE', *, *, #3303, .F. ) ;
#55964 = STYLED_ITEM ( 'NONE', ( #30189 ), #143366 ) ;
#55965 = LINE ( 'NONE', #22553, #35795 ) ;
#55966 = EDGE_CURVE ( 'NONE', #106022, #135463, #56854, .T. ) ;
#55967 = CARTESIAN_POINT ( 'NONE',  ( 36.53752705046288440, -9.735942053221456900E-16, 7.949999999999998401 ) ) ;
#55968 = VERTEX_POINT ( 'NONE', #93718 ) ;
#55969 = STYLED_ITEM ( 'NONE', ( #5814 ), #116311 ) ;
#55970 = VERTEX_POINT ( 'NONE', #95125 ) ;
#55971 = CARTESIAN_POINT ( 'NONE',  ( -7.140000000000001457, 0.000000000000000000, -40.00000000000000000 ) ) ;
#55972 = CARTESIAN_POINT ( 'NONE',  ( -81.18398860626899705, 28.73617430169844056, 5.000000000000000000 ) ) ;
#55973 = LINE ( 'NONE', #91435, #30049 ) ;
#55974 = ORIENTED_EDGE ( 'NONE', *, *, #72695, .T. ) ;
#55975 =( GEOMETRIC_REPRESENTATION_CONTEXT ( 3 ) GLOBAL_UNCERTAINTY_ASSIGNED_CONTEXT ( ( #112840 ) ) GLOBAL_UNIT_ASSIGNED_CONTEXT ( ( #37146, #14683, #58964 ) ) REPRESENTATION_CONTEXT ( 'NONE', 'WORKASPACE' ) );
#55976 = DIRECTION ( 'NONE',  ( -0.3543493200069162685, -0.000000000000000000, -0.9351131265310288487 ) ) ;
#55977 = ADVANCED_FACE ( 'NONE', ( #49534 ), #106697, .F. ) ;
#55978 = LINE ( 'NONE', #142264, #132440 ) ;
#55979 = CARTESIAN_POINT ( 'NONE',  ( 27.62956980810189123, -3.967499999999998028, -6.871911579029511330 ) ) ;
#55980 = LINE ( 'NONE', #24037, #16003 ) ;
#55981 = VERTEX_POINT ( 'NONE', #82856 ) ;
#55982 = CARTESIAN_POINT ( 'NONE',  ( 115.2662635252314374, 4.472830434245839371, -4.472830434245839371 ) ) ;
#55983 = DIRECTION ( 'NONE',  ( 0.7071067811865487940, 0.7071067811865463515, -0.000000000000000000 ) ) ;
#55984 = ADVANCED_FACE ( 'NONE', ( #84299 ), #5951, .F. ) ;
#55985 = DIRECTION ( 'NONE',  ( 0.7071067811865486830, -0.7071067811865464625, -0.000000000000000000 ) ) ;
#55987 = ORIENTED_EDGE ( 'NONE', *, *, #141959, .F. ) ;
#55986 = DIRECTION ( 'NONE',  ( -0.6830127018922180770, -0.6830127018922204085, -0.2588190451025213501 ) ) ;
#55988 = PLANE ( 'NONE',  #101779 ) ;
#55989 = ORIENTED_EDGE ( 'NONE', *, *, #140213, .T. ) ;
#55990 = CARTESIAN_POINT ( 'NONE',  ( 24.45983838949724998, 18.75929247661552779, 8.305906642995541489 ) ) ;
#55991 = CARTESIAN_POINT ( 'NONE',  ( -36.18398860626899705, 28.73617430169812437, 5.000000000000000000 ) ) ;
#55992 = PLANE ( 'NONE',  #107385 ) ;
#55993 = VERTEX_POINT ( 'NONE', #140093 ) ;
#55994 = VECTOR ( 'NONE', #17381, 1000.000000000000227 ) ;
#55995 = ADVANCED_FACE ( 'NONE', ( #62532 ), #29166, .F. ) ;
#55996 = LINE ( 'NONE', #100195, #96870 ) ;
#55997 = AXIS2_PLACEMENT_3D ( 'NONE', #107584, #86575, #31471 ) ;
#55998 = EDGE_CURVE ( 'NONE', #52228, #18107, #137948, .T. ) ;
#55999 = MECHANICAL_DESIGN_GEOMETRIC_PRESENTATION_REPRESENTATION (  '', ( #90660 ), #28132 ) ;
#56000 = CARTESIAN_POINT ( 'NONE',  ( 0.000000000000000000, 0.000000000000000000, 5.000000000000000000 ) ) ;
#56001 = DIRECTION ( 'NONE',  ( -0.7071067811865486830, 0.7071067811865464625, 0.000000000000000000 ) ) ;
#56002 = ORIENTED_EDGE ( 'NONE', *, *, #37781, .T. ) ;
#56003 = AXIS2_PLACEMENT_3D ( 'NONE', #16039, #60331, #104512 ) ;
#56005 = EDGE_CURVE ( 'NONE', #41034, #15918, #40774, .T. ) ;
#56004 = CARTESIAN_POINT ( 'NONE',  ( -27.79289321881325847, 9.759292476615621936, 5.000000000000000000 ) ) ;
#56006 = VERTEX_POINT ( 'NONE', #19004 ) ;
#56007 = DIRECTION ( 'NONE',  ( 0.7071067811865486830, -0.7071067811865464625, -0.000000000000000000 ) ) ;
#56009 = EDGE_LOOP ( 'NONE', ( #124794, #101011, #142350, #56106 ) ) ;
#56008 = CARTESIAN_POINT ( 'NONE',  ( 3.299744871391591339, -27.71228299555208352, 4.000000000000000000 ) ) ;
#56010 = ORIENTED_EDGE ( 'NONE', *, *, #91930, .T. ) ;
#56011 = LINE ( 'NONE', #56739, #35727 ) ;
#56012 = CARTESIAN_POINT ( 'NONE',  ( -18.79289321881332597, -20.24070752338407431, 5.000000000000000000 ) ) ;
#56013 = AXIS2_PLACEMENT_3D ( 'NONE', #133663, #46706, #23454 ) ;
#56014 = VERTEX_POINT ( 'NONE', #84977 ) ;
#56015 = CARTESIAN_POINT ( 'NONE',  ( 6.005480084712508493, 28.92564299267933947, 4.000000000000000000 ) ) ;
#56016 = CARTESIAN_POINT ( 'NONE',  ( -11.81601139373100651, 28.73617430169779041, 5.000000000000000000 ) ) ;
#56017 = FACE_OUTER_BOUND ( 'NONE', #137414, .T. ) ;
#56018 = ORIENTED_EDGE ( 'NONE', *, *, #45438, .T. ) ;
#56019 = EDGE_CURVE ( 'NONE', #107142, #18858, #129179, .T. ) ;
#56020 = PRODUCT ( 'parallel pin unhardened_iso_ISO 2338 - 2.5 m6 x 8 - St', 'parallel pin unhardened_iso_ISO 2338 - 2.5 m6 x 8 - St', '', ( #71423 ) ) ;
#56021 = CARTESIAN_POINT ( 'NONE',  ( 17.01088028653936135, -22.02621442084248571, 4.990779571109217549 ) ) ;
#56022 = CARTESIAN_POINT ( 'NONE',  ( 7.939999999999994174, -39.93000000000000682, -10.00000000000000178 ) ) ;
#56023 = VECTOR ( 'NONE', #24485, 1000.000000000000000 ) ;
#56024 = DIRECTION ( 'NONE',  ( -0.000000000000000000, -0.3543493200069152693, 0.9351131265310292928 ) ) ;
#56025 = AXIS2_PLACEMENT_3D ( 'NONE', #37083, #104475, #49431 ) ;
#56026 = CARTESIAN_POINT ( 'NONE',  ( 126.9294095003570817, -4.539267423379012456, -4.720787893125737433 ) ) ;
#56027 = CARTESIAN_POINT ( 'NONE',  ( 127.5375270504628986, -9.735942053221456900E-16, 7.949999999999998401 ) ) ;
#56028 = EDGE_CURVE ( 'NONE', #105421, #14025, #7391, .T. ) ;
#56029 = LINE ( 'NONE', #79221, #115961 ) ;
#56030 = ORIENTED_EDGE ( 'NONE', *, *, #15723, .T. ) ;
#56031 = ORIENTED_EDGE ( 'NONE', *, *, #56033, .T. ) ;
#56032 = CARTESIAN_POINT ( 'NONE',  ( 126.5624999999999858, -5.819803920172572198, -5.819803920172573086 ) ) ;
#56033 = EDGE_CURVE ( 'NONE', #133992, #56202, #74107, .T. ) ;
#56034 = ORIENTED_EDGE ( 'NONE', *, *, #90893, .T. ) ;
#56035 = ORIENTED_EDGE ( 'NONE', *, *, #15370, .T. ) ;
#56036 = VECTOR ( 'NONE', #122640, 1000.000000000000000 ) ;
#56037 = CARTESIAN_POINT ( 'NONE',  ( 4.980122250714494214, -17.24070752338410273, 20.23474786156470628 ) ) ;
#56038 = CARTESIAN_POINT ( 'NONE',  ( -7.171830600776411657, -14.24070752338413648, 4.000000000000000000 ) ) ;
#56039 = ORIENTED_EDGE ( 'NONE', *, *, #130402, .T. ) ;
#56040 = LINE ( 'NONE', #100231, #71730 ) ;
#56041 = DIRECTION ( 'NONE',  ( -1.000000000000000000, 0.000000000000000000, 0.000000000000000000 ) ) ;
#56042 = CARTESIAN_POINT ( 'NONE',  ( 0.000000000000000000, -34.64999999999999147, 17.99210858042621908 ) ) ;
#56043 = EDGE_CURVE ( 'NONE', #80281, #63122, #61824, .T. ) ;
#56044 = DIRECTION ( 'NONE',  ( -0.000000000000000000, -0.3543493200069152693, 0.9351131265310292928 ) ) ;
#56045 = CARTESIAN_POINT ( 'NONE',  ( 124.2504301918981184, 3.055000000000002824, -5.291415217122919401 ) ) ;
#56046 = EDGE_LOOP ( 'NONE', ( #56542, #96669, #137540, #32237 ) ) ;
#56047 = ADVANCED_FACE ( 'NONE', ( #71268 ), #118299, .T. ) ;
#56048 = DIRECTION ( 'NONE',  ( 0.3543493200069162685, -0.000000000000000000, -0.9351131265310288487 ) ) ;
#56049 =( NAMED_UNIT ( * ) PLANE_ANGLE_UNIT ( ) SI_UNIT ( $, .RADIAN. ) );
#56051 = VECTOR ( 'NONE', #36063, 1000.000000000000000 ) ;
#56050 = CARTESIAN_POINT ( 'NONE',  ( 5.816011393731002066, 28.73617430169783304, 5.000000000000000000 ) ) ;
#56052 = CARTESIAN_POINT ( 'NONE',  ( 0.9950436184061330902, 5.292275011207155266, 4.751003958219890855 ) ) ;
#56053 = DIRECTION ( 'NONE',  ( -1.000000000000000000, -0.000000000000000000, -0.000000000000000000 ) ) ;
#56054 = CARTESIAN_POINT ( 'NONE',  ( 34.49999999999975842, 6.054329344830883031, 4.994342998332162331 ) ) ;
#56055 = DIRECTION ( 'NONE',  ( 0.7071067811865487940, -0.7071067811865463515, 0.000000000000000000 ) ) ;
#56056 = CARTESIAN_POINT ( 'NONE',  ( 46.01669371712956291, 7.950000000000001066, -2.130196079827421318 ) ) ;
#56057 = DIRECTION ( 'NONE',  ( 0.6830127018922181881, 0.6830127018922202975, -0.2588190451025214056 ) ) ;
#56058 = DIRECTION ( 'NONE',  ( 0.6830127018922181881, 0.6830127018922202975, -0.2588190451025214056 ) ) ;
#56059 = ORIENTED_EDGE ( 'NONE', *, *, #30675, .F. ) ;
#56060 = VERTEX_POINT ( 'NONE', #38626 ) ;
#56061 = CARTESIAN_POINT ( 'NONE',  ( 47.37500000000000000, 7.950000000000000178, 1.460391307983218535E-15 ) ) ;
#56062 = DIRECTION ( 'NONE',  ( 0.7071067811865486830, -0.7071067811865464625, -0.000000000000000000 ) ) ;
#56063 = LINE ( 'NONE', #55327, #60015 ) ;
#56064 = ORIENTED_EDGE ( 'NONE', *, *, #42812, .T. ) ;
#56065 = AXIS2_PLACEMENT_3D ( 'NONE', #85039, #61892, #31382 ) ;
#56066 = VECTOR ( 'NONE', #70443, 1000.000000000000000 ) ;
#56067 = CARTESIAN_POINT ( 'NONE',  ( -19.49999999999985789, 5.696342897626483825, -7.587980461218443828 ) ) ;
#56068 = EDGE_CURVE ( 'NONE', #2946, #53913, #39355, .T. ) ;
#56069 = LINE ( 'NONE', #134321, #127877 ) ;
#56070 = STYLED_ITEM ( 'NONE', ( #57754 ), #118359 ) ;
#56071 = AXIS2_PLACEMENT_3D ( 'NONE', #95112, #48784, #61133 ) ;
#56072 = ADVANCED_FACE ( 'NONE', ( #28474 ), #72736, .F. ) ;
#56073 = CARTESIAN_POINT ( 'NONE',  ( 42.29209685856477563, -5.291415217122921177, 3.054999999999999272 ) ) ;
#56074 = ORIENTED_EDGE ( 'NONE', *, *, #81751, .F. ) ;
#56075 = CARTESIAN_POINT ( 'NONE',  ( 0.1600000000000006695, 2.227659143332861191, -7.636621307949803317 ) ) ;
#56076 = ORIENTED_EDGE ( 'NONE', *, *, #118850, .F. ) ;
#56077 = ORIENTED_EDGE ( 'NONE', *, *, #117320, .F. ) ;
#56078 = AXIS2_PLACEMENT_3D ( 'NONE', #43204, #22126, #10532 ) ;
#56079 = PRESENTATION_LAYER_ASSIGNMENT (  '', '', ( #97620 ) ) ;
#56080 = CARTESIAN_POINT ( 'NONE',  ( -13.49999999999989875, -10.53360074219763121, 5.000000000000000000 ) ) ;
#56081 = PLANE ( 'NONE',  #54640 ) ;
#56082 = DIRECTION ( 'NONE',  ( 0.000000000000000000, 0.000000000000000000, 1.000000000000000000 ) ) ;
#56083 = DIRECTION ( 'NONE',  ( -0.6830127018922180770, -0.6830127018922204085, -0.2588190451025213501 ) ) ;
#56084 = ORIENTED_EDGE ( 'NONE', *, *, #104552, .T. ) ;
#56085 = EDGE_CURVE ( 'NONE', #23517, #115243, #116887, .T. ) ;
#56086 = DIRECTION ( 'NONE',  ( 1.000000000000000000, 0.000000000000000000, 0.000000000000000000 ) ) ;
#56087 = VERTEX_POINT ( 'NONE', #5250 ) ;
#56088 = CARTESIAN_POINT ( 'NONE',  ( -4.499999999999966249, -7.533600742197664069, 5.000000000000000000 ) ) ;
#56089 = FACE_OUTER_BOUND ( 'NONE', #120597, .T. ) ;
#56090 = DIRECTION ( 'NONE',  ( -0.7071067811865486830, 0.7071067811865464625, 0.000000000000000000 ) ) ;
#56091 = CARTESIAN_POINT ( 'NONE',  ( -34.45011844616455221, -20.99769585840582664, 5.000000000000000888 ) ) ;
#56092 = PLANE ( 'NONE',  #48588 ) ;
#56093 = CARTESIAN_POINT ( 'NONE',  ( -15.79289321881334551, 9.759292476615621936, 5.000000000000000000 ) ) ;
#56094 = ORIENTED_EDGE ( 'NONE', *, *, #2628, .T. ) ;
#56095 = LINE ( 'NONE', #123491, #131067 ) ;
#56096 = CARTESIAN_POINT ( 'NONE',  ( 56.64126352523144448, 4.472830434245836706, 4.472830434245840259 ) ) ;
#56097 = DIRECTION ( 'NONE',  ( -0.3543493200069162685, -0.000000000000000000, -0.9351131265310288487 ) ) ;
#56098 = FACE_OUTER_BOUND ( 'NONE', #23169, .T. ) ;
#56099 = PLANE ( 'NONE',  #15545 ) ;
#56100 = EDGE_LOOP ( 'NONE', ( #5074, #129383, #135645, #99938 ) ) ;
#56101 = LINE ( 'NONE', #69832, #88709 ) ;
#56102 = EDGE_LOOP ( 'NONE', ( #118560, #57854, #23354, #26820 ) ) ;
#56103 = AXIS2_PLACEMENT_3D ( 'NONE', #23819, #47747, #79679 ) ;
#56104 = VECTOR ( 'NONE', #117549, 1000.000000000000000 ) ;
#56105 = CARTESIAN_POINT ( 'NONE',  ( 31.92500000000000782, 22.27000000000000313, -14.71147562388301822 ) ) ;
#56106 = ORIENTED_EDGE ( 'NONE', *, *, #114142, .F. ) ;
#56107 = AXIS2_PLACEMENT_3D ( 'NONE', #134788, #66652, #56535 ) ;
#56108 = DIRECTION ( 'NONE',  ( 0.7071067811865487940, 0.7071067811865463515, -0.000000000000000000 ) ) ;
#56109 = CARTESIAN_POINT ( 'NONE',  ( 21.29159235450332233, 9.902892378096218942E-16, 0.000000000000000000 ) ) ;
#56110 = DIRECTION ( 'NONE',  ( 0.7071067811865487940, 0.7071067811865463515, 0.000000000000000000 ) ) ;
#56111 = AXIS2_PLACEMENT_3D ( 'NONE', #79075, #23191, #67476 ) ;
#56112 = DIRECTION ( 'NONE',  ( 0.7071067811865487940, 0.7071067811865463515, 0.000000000000000000 ) ) ;
#56113 = FACE_BOUND ( 'NONE', #89153, .T. ) ;
#56114 = CARTESIAN_POINT ( 'NONE',  ( 26.99999999999981526, -5.527737879153164613, -7.983877177622434651 ) ) ;
#56115 = ADVANCED_FACE ( 'NONE', ( #50935 ), #104587, .F. ) ;
#56116 = EDGE_CURVE ( 'NONE', #45742, #87036, #20407, .T. ) ;
#56117 = DIRECTION ( 'NONE',  ( -0.6830127018922180770, -0.6830127018922204085, -0.2588190451025213501 ) ) ;
#56118 = CARTESIAN_POINT ( 'NONE',  ( -45.29974487139158867, -27.71228299555237840, 4.000000000000000000 ) ) ;
#56120 = EDGE_LOOP ( 'NONE', ( #142056, #28248, #100970, #62695 ) ) ;
#56119 = DIRECTION ( 'NONE',  ( 0.000000000000000000, 0.000000000000000000, -1.000000000000000000 ) ) ;
#56121 = VECTOR ( 'NONE', #102997, 1000.000000000000000 ) ;
#56122 = LINE ( 'NONE', #65575, #99533 ) ;
#56123 = ORIENTED_EDGE ( 'NONE', *, *, #39123, .F. ) ;
#56124 = ADVANCED_FACE ( 'NONE', ( #87828 ), #85673, .F. ) ;
#56125 = EDGE_CURVE ( 'NONE', #135598, #78218, #110270, .T. ) ;
#56126 = ORIENTED_EDGE ( 'NONE', *, *, #23214, .F. ) ;
#56127 = CARTESIAN_POINT ( 'NONE',  ( 76.62043019189812298, 3.055000000000001936, -5.291415217122916737 ) ) ;
#56128 = ORIENTED_EDGE ( 'NONE', *, *, #85740, .F. ) ;
#56129 = CARTESIAN_POINT ( 'NONE',  ( 1.369266385878517678, 0.000000000000000000, 0.000000000000000000 ) ) ;
#56130 = EDGE_CURVE ( 'NONE', #55125, #58070, #52340, .T. ) ;
#56131 = CARTESIAN_POINT ( 'NONE',  ( 0.1839886062690032631, 28.73617430169787568, 5.000000000000000000 ) ) ;
#56132 = ADVANCED_FACE ( 'NONE', ( #96529 ), #74847, .F. ) ;
#56133 = AXIS2_PLACEMENT_3D ( 'NONE', #64088, #44513, #66244 ) ;
#56134 = EDGE_LOOP ( 'NONE', ( #17534, #11987, #124372, #119481, #99330 ) ) ;
#56135 = LINE ( 'NONE', #974, #102364 ) ;
#56136 = CIRCLE ( 'NONE', #32950, 2.247899999999996901 ) ;
#56137 = EDGE_CURVE ( 'NONE', #127061, #70950, #132803, .T. ) ;
#56138 = CARTESIAN_POINT ( 'NONE',  ( 4.499999999999973355, 18.43112307739199451, 4.000000000000000000 ) ) ;
#56139 = DIRECTION ( 'NONE',  ( -1.000000000000000000, -0.000000000000000000, -0.000000000000000000 ) ) ;
#56140 = EDGE_CURVE ( 'NONE', #34231, #129574, #55210, .T. ) ;
#56141 = CARTESIAN_POINT ( 'NONE',  ( -24.61500991739762512, 5.335133370053846136, 4.556819239218478756 ) ) ;
#56142 = LINE ( 'NONE', #47420, #131581 ) ;
#56143 = CARTESIAN_POINT ( 'NONE',  ( -34.49999999999975842, 21.05432934483072671, 4.994342998332167660 ) ) ;
#56144 = DIRECTION ( 'NONE',  ( 0.7071067811865486830, -0.7071067811865464625, -0.000000000000000000 ) ) ;
#56145 = DIRECTION ( 'NONE',  ( 0.7071067811865487940, 0.7071067811865463515, 0.000000000000000000 ) ) ;
#56146 = VERTEX_POINT ( 'NONE', #76992 ) ;
#56147 = AXIS2_PLACEMENT_3D ( 'NONE', #95726, #62409, #65274 ) ;
#56148 = VECTOR ( 'NONE', #84759, 1000.000000000000000 ) ;
#56149 = VERTEX_POINT ( 'NONE', #66099 ) ;
#56150 = DIRECTION ( 'NONE',  ( 0.7071067811865487940, 0.7071067811865463515, -0.000000000000000000 ) ) ;
#56151 = CARTESIAN_POINT ( 'NONE',  ( 36.18398860626899705, 28.73617430169812437, 5.000000000000000000 ) ) ;
#56152 = ORIENTED_EDGE ( 'NONE', *, *, #133178, .T. ) ;
#56153 = ADVANCED_FACE ( 'NONE', ( #41457 ), #76251, .F. ) ;
#56154 = EDGE_LOOP ( 'NONE', ( #100137, #131798, #44565, #43494 ) ) ;
#56155 = ORIENTED_EDGE ( 'NONE', *, *, #136480, .F. ) ;
#56156 = CARTESIAN_POINT ( 'NONE',  ( 25.66709685856477563, -3.055000000000000160, -5.291415217122921177 ) ) ;
#56157 = VECTOR ( 'NONE', #97931, 999.9999999999998863 ) ;
#56158 = ORIENTED_EDGE ( 'NONE', *, *, #136468, .F. ) ;
#56159 = CARTESIAN_POINT ( 'NONE',  ( 34.42499999999998295, 20.97718569542917777, 5.000000000000000000 ) ) ;
#56161 = ADVANCED_FACE ( 'NONE', ( #65399 ), #141504, .F. ) ;
#56160 =( BOUNDED_CURVE ( )  B_SPLINE_CURVE ( 3, ( #135040, #79953, #58930, #103092 ),
 .UNSPECIFIED., .F., .T. ) 
 B_SPLINE_CURVE_WITH_KNOTS ( ( 4, 4 ),
 ( 5.005968288816728951, 5.074607125596344304 ),
 .UNSPECIFIED. ) 
 CURVE ( )  GEOMETRIC_REPRESENTATION_ITEM ( )  RATIONAL_B_SPLINE_CURVE ( ( 1.000000000000000000, 0.9996074310407763175, 0.9996074310407763175, 1.000000000000000000 ) ) 
 REPRESENTATION_ITEM ( '' )  );
#56162 = DIRECTION ( 'NONE',  ( 0.3543493200069162685, -0.000000000000000000, -0.9351131265310288487 ) ) ;
#56163 = CARTESIAN_POINT ( 'NONE',  ( 30.23330628287044419, -6.094999999999989981, -1.633150327867689100 ) ) ;
#56164 = CARTESIAN_POINT ( 'NONE',  ( 18.50044947910937765, 3.007166298682988348, -30.07082962428489381 ) ) ;
#56165 = ORIENTED_EDGE ( 'NONE', *, *, #41196, .F. ) ;
#56166 = CARTESIAN_POINT ( 'NONE',  ( 6.628407645496676714, -3.851859888774471706E-31, 2.500000000000001332 ) ) ;
#56167 = DIRECTION ( 'NONE',  ( -0.7071067811865486830, -0.7071067811865464625, 0.000000000000000000 ) ) ;
#56168 = DIRECTION ( 'NONE',  ( -0.7071067811865487940, 0.7071067811865463515, -0.000000000000000000 ) ) ;
#56169 = VECTOR ( 'NONE', #40497, 1000.000000000000227 ) ;
#56170 = VECTOR ( 'NONE', #65252, 1000.000000000000000 ) ;
#56172 = ORIENTED_EDGE ( 'NONE', *, *, #121168, .F. ) ;
#56171 = CARTESIAN_POINT ( 'NONE',  ( -14.20710678118644132, -5.240707523384227073, 5.000000000000000000 ) ) ;
#56173 = AXIS2_PLACEMENT_3D ( 'NONE', #71770, #115934, #48570 ) ;
#56174 = ORIENTED_EDGE ( 'NONE', *, *, #35715, .T. ) ;
#56175 = CARTESIAN_POINT ( 'NONE',  ( 2.510786437626908008, -27.52281430457053446, 5.000000000000000000 ) ) ;
#56176 = DIRECTION ( 'NONE',  ( -0.000000000000000000, 0.3543493200069153248, 0.9351131265310292928 ) ) ;
#56177 = VECTOR ( 'NONE', #127085, 1000.000000000000000 ) ;
#56178 = LINE ( 'NONE', #24225, #40165 ) ;
#56179 = ORIENTED_EDGE ( 'NONE', *, *, #133295, .T. ) ;
#56180 = DIRECTION ( 'NONE',  ( -0.000000000000000000, -1.000000000000000000, -0.000000000000000000 ) ) ;
#56181 = EDGE_CURVE ( 'NONE', #118712, #80915, #119710, .T. ) ;
#56182 = LINE ( 'NONE', #84661, #138275 ) ;
#56183 = ORIENTED_EDGE ( 'NONE', *, *, #54, .T. ) ;
#56184 = EDGE_CURVE ( 'NONE', #72338, #103200, #119024, .T. ) ;
#56185 = FILL_AREA_STYLE_COLOUR ( '', #33279 ) ;
#56186 = PLANE ( 'NONE',  #107303 ) ;
#56187 = COLOUR_RGB ( '', 0.31764706, 0.68627451, 0.89019608) ;
#56188 = AXIS2_PLACEMENT_3D ( 'NONE', #140176, #7491, #107529 ) ;
#56189 = DIRECTION ( 'NONE',  ( -1.000000000000000000, -0.000000000000000000, -0.000000000000000000 ) ) ;
#56190 = LINE ( 'NONE', #10472, #63250 ) ;
#56191 = EDGE_CURVE ( 'NONE', #100333, #138017, #108836, .T. ) ;
#56192 = DIRECTION ( 'NONE',  ( 0.7071067811865487940, 0.7071067811865463515, 0.000000000000000000 ) ) ;
#56193 = DIRECTION ( 'NONE',  ( 0.3543493200069162685, -0.000000000000000000, -0.9351131265310288487 ) ) ;
#56194 = CARTESIAN_POINT ( 'NONE',  ( -33.18398860626899705, 28.73617430169810305, 5.000000000000000000 ) ) ;
#56195 = ORIENTED_EDGE ( 'NONE', *, *, #137048, .F. ) ;
#56196 = ORIENTED_EDGE ( 'NONE', *, *, #33855, .T. ) ;
#56197 = DIRECTION ( 'NONE',  ( -0.7071067811865486830, -0.7071067811865464625, -0.000000000000000000 ) ) ;
#56198 = LINE ( 'NONE', #1027, #50587 ) ;
#56199 = ADVANCED_FACE ( 'NONE', ( #107436 ), #42207, .T. ) ;
#56200 = CARTESIAN_POINT ( 'NONE',  ( -8.999999999999941380, -4.068876922607777225, 4.000000000000000000 ) ) ;
#56201 = FACE_OUTER_BOUND ( 'NONE', #2282, .T. ) ;
#56202 = VERTEX_POINT ( 'NONE', #86424 ) ;
#56203 = AXIS2_PLACEMENT_3D ( 'NONE', #111234, #22771, #77929 ) ;
#56204 = FACE_OUTER_BOUND ( 'NONE', #60020, .T. ) ;
#56205 = CARTESIAN_POINT ( 'NONE',  ( 6.489213562373093325, -27.52281430457059841, 5.000000000000000000 ) ) ;
#56206 = CARTESIAN_POINT ( 'NONE',  ( -26.99999999999980105, 1.552185695429149304, 5.000000000000000000 ) ) ;
#56207 = ORIENTED_EDGE ( 'NONE', *, *, #41668, .T. ) ;
#56208 = EDGE_CURVE ( 'NONE', #142584, #137698, #10946, .T. ) ;
#56209 = DIRECTION ( 'NONE',  ( -0.7071067811865487940, 0.7071067811865463515, -0.000000000000000000 ) ) ;
#56210 = DIRECTION ( 'NONE',  ( 0.7071067811865486830, -0.7071067811865464625, -0.000000000000000000 ) ) ;
#56211 = LINE ( 'NONE', #112678, #37654 ) ;
#56212 = CARTESIAN_POINT ( 'NONE',  ( 6.489213562373093325, -27.52281430457059841, 5.000000000000000000 ) ) ;
#56213 = CARTESIAN_POINT ( 'NONE',  ( 55.03709685856478018, -3.054999999999999272, -5.291415217122919401 ) ) ;
#56214 = VECTOR ( 'NONE', #60599, 1000.000000000000227 ) ;
#56215 = DIRECTION ( 'NONE',  ( 0.6830127018922181881, 0.6830127018922202975, -0.2588190451025214056 ) ) ;
#56216 = DIRECTION ( 'NONE',  ( 0.7071067811865487940, 0.7071067811865463515, 0.000000000000000000 ) ) ;
#56217 = CARTESIAN_POINT ( 'NONE',  ( 84.27083333333332860, -7.949999999999998401, -2.130196079827426203 ) ) ;
#56218 = ADVANCED_FACE ( 'NONE', ( #9521 ), #97998, .F. ) ;
#56219 = VECTOR ( 'NONE', #104807, 1000.000000000000000 ) ;
#56220 = EDGE_LOOP ( 'NONE', ( #25182, #28241, #117112, #45539 ) ) ;
#56221 = DIRECTION ( 'NONE',  ( -0.000000000000000000, 0.000000000000000000, 1.000000000000000000 ) ) ;
#56222 = ORIENTED_EDGE ( 'NONE', *, *, #15930, .T. ) ;
#56223 = AXIS2_PLACEMENT_3D ( 'NONE', #133614, #55338, #74967 ) ;
#56224 = DIRECTION ( 'NONE',  ( 1.000000000000000000, 1.224606353822377258E-16, 0.000000000000000000 ) ) ;
#56225 = VECTOR ( 'NONE', #73021, 1000.000000000000227 ) ;
#56226 = PLANE ( 'NONE',  #113187 ) ;
#56227 = CARTESIAN_POINT ( 'NONE',  ( 5.488313940715645600, 6.759292476615645917, 16.35960578974468049 ) ) ;
#56228 = DIRECTION ( 'NONE',  ( -0.7071067811865486830, -0.7071067811865464625, 0.000000000000000000 ) ) ;
#56229 = EDGE_CURVE ( 'NONE', #44279, #19888, #42921, .T. ) ;
#56230 = DIRECTION ( 'NONE',  ( -0.000000000000000000, -0.3543493200069152693, 0.9351131265310292928 ) ) ;
#56231 = FACE_OUTER_BOUND ( 'NONE', #106539, .T. ) ;
#56232 = ORIENTED_EDGE ( 'NONE', *, *, #93656, .T. ) ;
#56233 = EDGE_CURVE ( 'NONE', #106369, #46696, #102020, .T. ) ;
#56234 = ORIENTED_EDGE ( 'NONE', *, *, #62243, .T. ) ;
#56235 = CARTESIAN_POINT ( 'NONE',  ( 4.499999999999974243, -7.912538124160676922, 4.000000000000000000 ) ) ;
#56236 = DIRECTION ( 'NONE',  ( -0.7071067811865486830, -0.7071067811865464625, 0.000000000000000000 ) ) ;
#56237 = UNCERTAINTY_MEASURE_WITH_UNIT (LENGTH_MEASURE( 1.000000000000000082E-05 ), #14893, 'distance_accuracy_value', 'NONE');
#56238 = CARTESIAN_POINT ( 'NONE',  ( 7.408407645496676963, 9.139736423841732040E-16, 0.000000000000000000 ) ) ;
#56239 = CARTESIAN_POINT ( 'NONE',  ( 16.37913961620377279, -5.278424836066145431, -3.047499999999993658 ) ) ;
#56240 = CARTESIAN_POINT ( 'NONE',  ( 75.32919371712957002, -3.975000000000001865, 6.884901960086284411 ) ) ;
#56241 = CYLINDRICAL_SURFACE ( 'NONE', #122685, 4.999999999999998224 ) ;
#56242 = ADVANCED_FACE ( 'NONE', ( #13102 ), #89950, .F. ) ;
#56243 = CARTESIAN_POINT ( 'NONE',  ( -32.99999999999976552, -8.731860332648864187, -2.120594902707616747 ) ) ;
#56244 = ORIENTED_EDGE ( 'NONE', *, *, #23147, .T. ) ;
#56245 = CARTESIAN_POINT ( 'NONE',  ( 75.95833333333332860, 3.974999999999997424, 6.884901960086288852 ) ) ;
#56246 = CARTESIAN_POINT ( 'NONE',  ( -31.17183060077626067, 6.759292476615656575, 4.000000000000000000 ) ) ;
#56247 = DIRECTION ( 'NONE',  ( 0.7071067811865486830, -0.7071067811865464625, -0.000000000000000000 ) ) ;
#56249 = VECTOR ( 'NONE', #50200, 1000.000000000000000 ) ;
#56248 = LINE ( 'NONE', #35188, #12696 ) ;
#56250 = VECTOR ( 'NONE', #46063, 1000.000000000000000 ) ;
#56251 = ORIENTED_EDGE ( 'NONE', *, *, #1920, .F. ) ;
#56252 = EDGE_CURVE ( 'NONE', #143240, #108517, #60345, .T. ) ;
#56253 = PLANE ( 'NONE',  #65277 ) ;
#56254 = ORIENTED_EDGE ( 'NONE', *, *, #18418, .F. ) ;
#56255 = EDGE_CURVE ( 'NONE', #139810, #5145, #36314, .T. ) ;
#56256 = CARTESIAN_POINT ( 'NONE',  ( -31.49999999999977973, 22.22500000000000142, 4.362957392718792349 ) ) ;
#56257 = CARTESIAN_POINT ( 'NONE',  ( 67.37543019189810423, -5.291415217122920289, -3.055000000000001492 ) ) ;
#56258 = VERTEX_POINT ( 'NONE', #56683 ) ;
#56259 = ORIENTED_EDGE ( 'NONE', *, *, #37425, .F. ) ;
#56260 = AXIS2_PLACEMENT_3D ( 'NONE', #133972, #70198, #113637 ) ;
#56261 = CARTESIAN_POINT ( 'NONE',  ( 18.01107201284014536, 3.821174125832445049E-16, 0.000000000000000000 ) ) ;
#56262 = DIRECTION ( 'NONE',  ( -0.000000000000000000, 0.3543493200069153248, 0.9351131265310292928 ) ) ;
#56263 = PLANE ( 'NONE',  #79069 ) ;
#56264 = LINE ( 'NONE', #133779, #60229 ) ;
#56265 = EDGE_CURVE ( 'NONE', #103031, #36832, #123341, .T. ) ;
#56266 = CARTESIAN_POINT ( 'NONE',  ( 26.14818355038129027, 17.25929247661554200, 8.802941693769263054 ) ) ;
#56268 = ORIENTED_EDGE ( 'NONE', *, *, #11820, .T. ) ;
#56267 = FACE_OUTER_BOUND ( 'NONE', #87798, .T. ) ;
#56269 = CARTESIAN_POINT ( 'NONE',  ( 8.585466709768445170, 3.821174125832445049E-16, 0.000000000000000000 ) ) ;
#56270 = CARTESIAN_POINT ( 'NONE',  ( -7.940000000000007496, -60.26999999999998892, -7.752100000000002211 ) ) ;
#56271 = VECTOR ( 'NONE', #12160, 1000.000000000000000 ) ;
#56272 = PLANE ( 'NONE',  #116543 ) ;
#56273 = ORIENTED_EDGE ( 'NONE', *, *, #120959, .T. ) ;
#56274 = VERTEX_POINT ( 'NONE', #91414 ) ;
#56275 = CARTESIAN_POINT ( 'NONE',  ( 66.93793019189809002, -6.110000000000001208, 1.637169565754158951 ) ) ;
#56276 = ORIENTED_EDGE ( 'NONE', *, *, #10941, .T. ) ;
#56277 = CARTESIAN_POINT ( 'NONE',  ( 19.73159235450332005, -2.500000000000000000, 3.061616997868384127E-16 ) ) ;
#56278 = DIRECTION ( 'NONE',  ( 0.7071067811865487940, 0.7071067811865463515, 0.000000000000000000 ) ) ;
#56279 = CARTESIAN_POINT ( 'NONE',  ( -0.4892135623730947680, -27.52281430457055578, 5.000000000000000000 ) ) ;
#56280 = CARTESIAN_POINT ( 'NONE',  ( -15.48921356237309510, -27.52281430457066236, 5.000000000000000000 ) ) ;
#56281 = DIRECTION ( 'NONE',  ( -0.7071067811865486830, -0.7071067811865464625, -0.000000000000000000 ) ) ;
#56282 = ORIENTED_EDGE ( 'NONE', *, *, #17441, .F. ) ;
#56283 = ORIENTED_EDGE ( 'NONE', *, *, #20282, .F. ) ;
#56284 = VECTOR ( 'NONE', #87883, 1000.000000000000000 ) ;
#56285 = DIRECTION ( 'NONE',  ( -0.7071067811865486830, -0.7071067811865464625, 0.000000000000000000 ) ) ;
#56286 = CARTESIAN_POINT ( 'NONE',  ( -19.93618819985229251, -3.270000000000008900, -35.71710890046286124 ) ) ;
#56287 = VECTOR ( 'NONE', #75029, 1000.000000000000000 ) ;
#56288 = ORIENTED_EDGE ( 'NONE', *, *, #30698, .F. ) ;
#56289 = LINE ( 'NONE', #100470, #46813 ) ;
#56291 = CARTESIAN_POINT ( 'NONE',  ( -34.49999999999975842, -5.945670655168998842, 4.994342998332166772 ) ) ;
#56290 = COLOUR_RGB ( '', 0.72549020, 0.75294118, 0.79215686) ;
#56292 = CARTESIAN_POINT ( 'NONE',  ( 15.49238828748955576, 2.500000000000000444, 0.000000000000000000 ) ) ;
#56293 = VECTOR ( 'NONE', #115705, 999.9999999999998863 ) ;
#56294 = MECHANICAL_DESIGN_GEOMETRIC_PRESENTATION_REPRESENTATION (  '', ( #111821 ), #128082 ) ;
#56295 = ORIENTED_EDGE ( 'NONE', *, *, #18226, .T. ) ;
#56296 = FACE_BOUND ( 'NONE', #76089, .T. ) ;
#56297 = DIRECTION ( 'NONE',  ( -0.7071067811865487940, 0.7071067811865463515, 0.000000000000000000 ) ) ;
#56298 = DIRECTION ( 'NONE',  ( 0.7071067811865487940, 0.7071067811865463515, 0.000000000000000000 ) ) ;
#56299 = LINE ( 'NONE', #68578, #25087 ) ;
#56300 = LINE ( 'NONE', #134548, #4041 ) ;
#56301 = FACE_OUTER_BOUND ( 'NONE', #114011, .T. ) ;
#56302 = ORIENTED_EDGE ( 'NONE', *, *, #124514, .T. ) ;
#56303 = ADVANCED_FACE ( 'NONE', ( #133489 ), #110977, .F. ) ;
#56304 = VECTOR ( 'NONE', #6720, 1000.000000000000000 ) ;
#56305 = ORIENTED_EDGE ( 'NONE', *, *, #47966, .F. ) ;
#56306 = CARTESIAN_POINT ( 'NONE',  ( 101.4120968585647802, 5.291415217122921177, -3.054999999999994831 ) ) ;
#56307 = ORIENTED_EDGE ( 'NONE', *, *, #96225, .F. ) ;
#56308 = EDGE_CURVE ( 'NONE', #125435, #132154, #34175, .T. ) ;
#56309 = DIRECTION ( 'NONE',  ( -1.000000000000000000, 2.496005001405478586E-15, 0.000000000000000000 ) ) ;
#56310 = VERTEX_POINT ( 'NONE', #58099 ) ;
#56311 = ADVANCED_FACE ( 'NONE', ( #102993 ), #100145, .F. ) ;
#56312 = PLANE ( 'NONE',  #100183 ) ;
#56313 = ADVANCED_FACE ( 'NONE', ( #47929 ), #92093, .F. ) ;
#56314 = AXIS2_PLACEMENT_3D ( 'NONE', #68107, #79704, #25986 ) ;
#56315 = DIRECTION ( 'NONE',  ( 0.000000000000000000, -1.000000000000000000, 0.000000000000000000 ) ) ;
#56316 = LINE ( 'NONE', #55568, #791 ) ;
#56317 = ORIENTED_EDGE ( 'NONE', *, *, #68076, .T. ) ;
#56318 = LINE ( 'NONE', #135285, #83165 ) ;
#56319 = PLANE ( 'NONE',  #38037 ) ;
#56320 = DIRECTION ( 'NONE',  ( -0.7071067811865486830, -0.7071067811865464625, -0.000000000000000000 ) ) ;
#56321 = VECTOR ( 'NONE', #23505, 999.9999999999998863 ) ;
#56322 = EDGE_CURVE ( 'NONE', #112494, #120574, #22537, .T. ) ;
#56323 = DIRECTION ( 'NONE',  ( -0.7071067811865486830, -0.7071067811865464625, -0.000000000000000000 ) ) ;
#56324 = CARTESIAN_POINT ( 'NONE',  ( -15.41161490594820904, 22.22500000000000142, 4.777194822843812361 ) ) ;
#56325 = CARTESIAN_POINT ( 'NONE',  ( -12.48921356237309155, -27.52281430457064104, 5.000000000000000000 ) ) ;
#56326 = DIRECTION ( 'NONE',  ( -0.3543493200069162685, -0.000000000000000000, -0.9351131265310288487 ) ) ;
#56327 = VERTEX_POINT ( 'NONE', #78391 ) ;
#56328 = CARTESIAN_POINT ( 'NONE',  ( -12.69999999999998153, 0.000000000000000000, 2.500000000000000444 ) ) ;
#56329 = DIRECTION ( 'NONE',  ( -1.000000000000000000, -0.000000000000000000, -0.000000000000000000 ) ) ;
#56330 = ADVANCED_FACE ( 'NONE', ( #68963 ), #122584, .F. ) ;
#56331 = ORIENTED_EDGE ( 'NONE', *, *, #57517, .F. ) ;
#56332 = ORIENTED_EDGE ( 'NONE', *, *, #44687, .T. ) ;
#56333 = ADVANCED_FACE ( 'NONE', ( #111732 ), #27917, .T. ) ;
#56334 = VERTEX_POINT ( 'NONE', #2201 ) ;
#56335 = CARTESIAN_POINT ( 'NONE',  ( 51.62543019189811133, 5.291415217122919401, 3.055000000000002824 ) ) ;
#56336 = ORIENTED_EDGE ( 'NONE', *, *, #110869, .T. ) ;
#56337 = EDGE_CURVE ( 'NONE', #103081, #15156, #85757, .T. ) ;
#56338 = CIRCLE ( 'NONE', #58047, 3.000000000000002665 ) ;
#56339 = DIRECTION ( 'NONE',  ( 0.7071067811865487940, 0.7071067811865463515, -0.000000000000000000 ) ) ;
#56340 = STYLED_ITEM ( 'NONE', ( #68644 ), #46161 ) ;
#56341 = CARTESIAN_POINT ( 'NONE',  ( 4.712472949537106715, 0.000000000000000000, 6.094999999999989981 ) ) ;
#56342 = CARTESIAN_POINT ( 'NONE',  ( 94.79209685856476142, -5.291415217122921177, 3.054999999999999272 ) ) ;
#56343 = SURFACE_STYLE_FILL_AREA ( #133163 ) ;
#56344 = ORIENTED_EDGE ( 'NONE', *, *, #2950, .F. ) ;
#56345 = VECTOR ( 'NONE', #128500, 1000.000000000000000 ) ;
#56346 = ORIENTED_EDGE ( 'NONE', *, *, #45168, .T. ) ;
#56347 = CARTESIAN_POINT ( 'NONE',  ( 11.90156419391756337, 11.25929247661560595, 10.79108189686409780 ) ) ;
#56348 = AXIS2_PLACEMENT_3D ( 'NONE', #72477, #138402, #47862 ) ;
#56349 = DIRECTION ( 'NONE',  ( 0.7071067811865487940, 0.7071067811865463515, -0.000000000000000000 ) ) ;
#56350 = VERTEX_POINT ( 'NONE', #69680 ) ;
#56351 = DIRECTION ( 'NONE',  ( 0.000000000000000000, 0.000000000000000000, 1.000000000000000000 ) ) ;
#56352 = CARTESIAN_POINT ( 'NONE',  ( -3.707106781186522593, 20.25929247661551358, 5.000000000000000000 ) ) ;
#56353 = ORIENTED_EDGE ( 'NONE', *, *, #62865, .T. ) ;
#56354 = CARTESIAN_POINT ( 'NONE',  ( 20.29298673570680123, -21.74070752338406720, 4.999753212805221558 ) ) ;
#56355 = ORIENTED_EDGE ( 'NONE', *, *, #70554, .F. ) ;
#56356 = ORIENTED_EDGE ( 'NONE', *, *, #110847, .T. ) ;
#56357 = ORIENTED_EDGE ( 'NONE', *, *, #57735, .F. ) ;
#56358 = EDGE_CURVE ( 'NONE', #31963, #137771, #135627, .T. ) ;
#56359 = AXIS2_PLACEMENT_3D ( 'NONE', #24779, #24081, #68340 ) ;
#56360 = LINE ( 'NONE', #112133, #123350 ) ;
#56361 = FACE_OUTER_BOUND ( 'NONE', #44756, .T. ) ;
#56362 = CARTESIAN_POINT ( 'NONE',  ( 18.18398860626898994, 28.73617430169800002, 5.000000000000000000 ) ) ;
#56363 = AXIS2_PLACEMENT_3D ( 'NONE', #115550, #93838, #6782 ) ;
#56364 = EDGE_LOOP ( 'NONE', ( #49096, #142799, #139356, #42692 ) ) ;
#56365 = DIRECTION ( 'NONE',  ( 1.000000000000000000, 0.000000000000000000, 0.000000000000000000 ) ) ;
#56366 = EDGE_CURVE ( 'NONE', #112045, #141891, #79135, .T. ) ;
#56367 = CARTESIAN_POINT ( 'NONE',  ( 13.83290314143522082, -3.967499999999994476, 6.871911579029513106 ) ) ;
#56368 = CARTESIAN_POINT ( 'NONE',  ( 0.000000000000000000, -43.14999999999999147, -40.92499999999998295 ) ) ;
#56369 = DIRECTION ( 'NONE',  ( -0.7071067811865486830, -0.7071067811865464625, 0.000000000000000000 ) ) ;
#56370 = PLANE ( 'NONE',  #44361 ) ;
#56371 = ORIENTED_EDGE ( 'NONE', *, *, #76655, .T. ) ;
#56372 = VERTEX_POINT ( 'NONE', #124034 ) ;
#56373 = EDGE_CURVE ( 'NONE', #48791, #94433, #113132, .T. ) ;
#56374 = ORIENTED_EDGE ( 'NONE', *, *, #2999, .T. ) ;
#56375 = PLANE ( 'NONE',  #44152 ) ;
#56376 = UNCERTAINTY_MEASURE_WITH_UNIT (LENGTH_MEASURE( 1.000000000000000082E-05 ), #37717, 'distance_accuracy_value', 'NONE');
#56377 = VECTOR ( 'NONE', #4932, 1000.000000000000000 ) ;
#56378 = CARTESIAN_POINT ( 'NONE',  ( 23.99999999999982592, -2.904428200921294057, -6.989807076075000403 ) ) ;
#56379 = CARTESIAN_POINT ( 'NONE',  ( 27.48921356237309155, -27.52281430457074762, 5.000000000000000000 ) ) ;
#56380 = CARTESIAN_POINT ( 'NONE',  ( -11.70822291016945016, -15.74070752338412404, 19.73771281079094919 ) ) ;
#56381 = CONICAL_SURFACE ( 'NONE', #88747, 2.055000000000001048, 0.9599310885968758145 ) ;
#56382 = CARTESIAN_POINT ( 'NONE',  ( -17.99451991528748351, 28.92564299267950645, 4.000000000000000000 ) ) ;
#56383 = DIRECTION ( 'NONE',  ( -0.000000000000000000, 0.3543493200069153248, 0.9351131265310292928 ) ) ;
#56384 = ADVANCED_FACE ( 'NONE', ( #71812 ), #51475, .F. ) ;
#56385 = CARTESIAN_POINT ( 'NONE',  ( -2.048096618150911485, 22.22500000000000142, -7.458287694568845438 ) ) ;
#56386 = FACE_OUTER_BOUND ( 'NONE', #66127, .T. ) ;
#56387 = ORIENTED_EDGE ( 'NONE', *, *, #83785, .F. ) ;
#56388 = CYLINDRICAL_SURFACE ( 'NONE', #60439, 2.500000000000000444 ) ;
#56389 = PLANE ( 'NONE',  #584 ) ;
#56390 = EDGE_LOOP ( 'NONE', ( #37840, #67559, #49734, #125996 ) ) ;
#56391 = CARTESIAN_POINT ( 'NONE',  ( 19.91020365697643513, -3.046927250066239434, -34.73593278446270460 ) ) ;
#56392 = ORIENTED_EDGE ( 'NONE', *, *, #3165, .T. ) ;
#56393 = CARTESIAN_POINT ( 'NONE',  ( -1.828169399223521507, 18.75929247661552424, 4.000000000000000000 ) ) ;
#56395 = EDGE_LOOP ( 'NONE', ( #98741, #46452, #121906 ) ) ;
#56394 = DIRECTION ( 'NONE',  ( -1.000000000000000000, -1.224606353822377258E-16, -0.000000000000000000 ) ) ;
#56396 = EDGE_CURVE ( 'NONE', #1085, #63434, #39903, .T. ) ;
#56397 = CARTESIAN_POINT ( 'NONE',  ( -36.48921356237310221, -27.52281430457080802, 5.000000000000000000 ) ) ;
#56398 = CARTESIAN_POINT ( 'NONE',  ( -60.18398860626900415, 28.73617430169829490, 5.000000000000000000 ) ) ;
#56399 = ORIENTED_EDGE ( 'NONE', *, *, #131227, .T. ) ;
#56400 = LINE ( 'NONE', #54248, #34660 ) ;
#56401 = VERTEX_POINT ( 'NONE', #93544 ) ;
#56402 = CARTESIAN_POINT ( 'NONE',  ( -34.42500000000001137, -22.22500000000000142, 5.000000000000000000 ) ) ;
#56403 = UNCERTAINTY_MEASURE_WITH_UNIT (LENGTH_MEASURE( 1.000000000000000082E-05 ), #331, 'distance_accuracy_value', 'NONE');
#56404 = ORIENTED_EDGE ( 'NONE', *, *, #56957, .T. ) ;
#56405 = AXIS2_PLACEMENT_3D ( 'NONE', #83569, #74841, #63942 ) ;
#56406 = DIRECTION ( 'NONE',  ( -0.6830127018922181881, 0.6830127018922202975, -0.2588190451025214056 ) ) ;
#56407 = CARTESIAN_POINT ( 'NONE',  ( 111.4958603837962272, -3.974999999999998312, -6.884901960086286188 ) ) ;
#56408 = CARTESIAN_POINT ( 'NONE',  ( 10.49999999999993250, 9.052185695429077583, 5.000000000000000000 ) ) ;
#56409 = VECTOR ( 'NONE', #47314, 1000.000000000000000 ) ;
#56410 = VERTEX_POINT ( 'NONE', #115978 ) ;
#56411 = FACE_OUTER_BOUND ( 'NONE', #6992, .T. ) ;
#56412 = CARTESIAN_POINT ( 'NONE',  ( -12.19999999999999929, -59.76999999999998892, -40.00000000000000000 ) ) ;
#56413 = CARTESIAN_POINT ( 'NONE',  ( -23.67183060077630685, -0.7407075233842735917, 4.000000000000000000 ) ) ;
#56414 = CARTESIAN_POINT ( 'NONE',  ( 18.81250000000000355, -4.461849672132299993, -4.461849672132299105 ) ) ;
#56415 = CARTESIAN_POINT ( 'NONE',  ( -5.510786437626906675, -27.52281430457051314, 5.000000000000000000 ) ) ;
#56416 = DIRECTION ( 'NONE',  ( 0.3543493200069163240, 0.000000000000000000, 0.9351131265310288487 ) ) ;
#56417 = DIRECTION ( 'NONE',  ( 0.6830127018922180770, -0.6830127018922204085, -0.2588190451025213501 ) ) ;
#56418 = VERTEX_POINT ( 'NONE', #26846 ) ;
#56419 = VECTOR ( 'NONE', #75750, 999.9999999999998863 ) ;
#56420 = ORIENTED_EDGE ( 'NONE', *, *, #140373, .F. ) ;
#56421 = FACE_OUTER_BOUND ( 'NONE', #78781, .T. ) ;
#56422 = VERTEX_POINT ( 'NONE', #105809 ) ;
#56423 = EDGE_CURVE ( 'NONE', #105277, #51650, #15927, .T. ) ;
#56424 = VECTOR ( 'NONE', #22745, 1000.000000000000227 ) ;
#56425 = EDGE_CURVE ( 'NONE', #69752, #65577, #18072, .T. ) ;
#56426 = CARTESIAN_POINT ( 'NONE',  ( 93.77126352523141861, 4.472830434245839371, 4.472830434245842035 ) ) ;
#56427 = CARTESIAN_POINT ( 'NONE',  ( -33.48921356237309510, -27.52281430457078670, 5.000000000000000000 ) ) ;
#56428 = DIRECTION ( 'NONE',  ( 0.7071067811865487940, 0.7071067811865463515, 0.000000000000000000 ) ) ;
#56429 = CARTESIAN_POINT ( 'NONE',  ( 17.06332250466817158, 0.000000000000000000, 2.500000000000000444 ) ) ;
#56430 = LINE ( 'NONE', #80999, #20036 ) ;
#56431 = VERTEX_POINT ( 'NONE', #95669 ) ;
#56432 = DIRECTION ( 'NONE',  ( 0.6830127018922180770, -0.6830127018922204085, -0.2588190451025213501 ) ) ;
#56433 = DIRECTION ( 'NONE',  ( 0.3543493200069162685, -0.000000000000000000, -0.9351131265310288487 ) ) ;
#56434 =( BOUNDED_CURVE ( )  B_SPLINE_CURVE ( 2, ( #51071, #84430, #62662, #106852, #53187, #97387, #42349, #143062, #65548, #101693, #88706, #22670, #134346 ),
 .UNSPECIFIED., .F., .T. ) 
 B_SPLINE_CURVE_WITH_KNOTS ( ( 3, 2, 2, 2, 2, 2, 3 ),
 ( 0.3833333333333333592, 0.3861111111111111271, 0.3888888888888888951, 0.3916666666666666630, 0.3944444444444444309, 0.3972222222222221988, 0.4000000000000000222 ),
 .UNSPECIFIED. ) 
 CURVE ( )  GEOMETRIC_REPRESENTATION_ITEM ( )  RATIONAL_B_SPLINE_CURVE ( ( 1.000000000000000000, 0.9659258262890683122, 1.000000000000000000, 0.9659258262890683122, 1.000000000000000000, 0.9659258262890683122, 1.000000000000000000, 0.9659258262890683122, 1.000000000000000000, 0.9659258262890683122, 1.000000000000000000, 0.9659258262890683122, 1.000000000000000000 ) ) 
 REPRESENTATION_ITEM ( '' )  );
#56435 = VECTOR ( 'NONE', #68639, 1000.000000000000000 ) ;
#56436 = CARTESIAN_POINT ( 'NONE',  ( 7.637717201596474048, -2.500000000000000000, 3.061616997868383634E-16 ) ) ;
#56437 = EDGE_CURVE ( 'NONE', #139662, #33976, #114562, .T. ) ;
#56438 = DIRECTION ( 'NONE',  ( 1.000000000000000000, 0.000000000000000000, 0.000000000000000000 ) ) ;
#56439 = ADVANCED_FACE ( 'NONE', ( #104400 ), #103667, .F. ) ;
#56440 = CARTESIAN_POINT ( 'NONE',  ( 9.792893218813395251, -8.240707523384196875, 5.000000000000000000 ) ) ;
#56442 = ORIENTED_EDGE ( 'NONE', *, *, #57461, .T. ) ;
#56441 = DIRECTION ( 'NONE',  ( 1.000000000000000000, 1.369518533665900312E-16, -0.000000000000000000 ) ) ;
#56443 = CARTESIAN_POINT ( 'NONE',  ( -12.79333936457838661, 21.75929247661549581, 4.998822639870701856 ) ) ;
#56444 = PLANE ( 'NONE',  #96193 ) ;
#56445 = DIRECTION ( 'NONE',  ( -1.000000000000000000, -0.000000000000000000, -0.000000000000000000 ) ) ;
#56446 = CARTESIAN_POINT ( 'NONE',  ( -16.50229999999999819, 3.130000000000007887, -22.35000000000000142 ) ) ;
#56447 = CARTESIAN_POINT ( 'NONE',  ( 34.17183060077623225, -14.24070752338414003, 4.000000000000000000 ) ) ;
#56448 = VECTOR ( 'NONE', #119888, 1000.000000000000000 ) ;
#56449 = EDGE_LOOP ( 'NONE', ( #63178, #65971, #8571 ) ) ;
#56450 = VERTEX_POINT ( 'NONE', #84124 ) ;
#56451 = ORIENTED_EDGE ( 'NONE', *, *, #37987, .T. ) ;
#56452 = CARTESIAN_POINT ( 'NONE',  ( 88.08376352523144703, -6.110000000000001208, -3.741295971395164515E-16 ) ) ;
#56453 = VECTOR ( 'NONE', #56531, 1000.000000000000000 ) ;
#56454 = ORIENTED_EDGE ( 'NONE', *, *, #79020, .T. ) ;
#56455 = CARTESIAN_POINT ( 'NONE',  ( 3.183988606268992161, 28.73617430169789699, 5.000000000000000000 ) ) ;
#56456 = CARTESIAN_POINT ( 'NONE',  ( 33.48921356237309510, -27.52281430457078670, 5.000000000000000000 ) ) ;
#56457 = AXIS2_PLACEMENT_3D ( 'NONE', #64403, #10017, #54281 ) ;
#56458 = CARTESIAN_POINT ( 'NONE',  ( -69.48921356237309510, -27.52281430457103895, 5.000000000000000000 ) ) ;
#56459 = DIRECTION ( 'NONE',  ( -0.000000000000000000, -0.3543493200069152693, 0.9351131265310292928 ) ) ;
#56460 = ORIENTED_EDGE ( 'NONE', *, *, #122530, .F. ) ;
#56461 = EDGE_CURVE ( 'NONE', #127371, #131836, #8948, .T. ) ;
#56462 = DIRECTION ( 'NONE',  ( -0.7071067811865486830, -0.7071067811865464625, 0.000000000000000000 ) ) ;
#56463 = DIRECTION ( 'NONE',  ( -0.7071067811865486830, -0.7071067811865464625, 0.000000000000000000 ) ) ;
#56464 = CARTESIAN_POINT ( 'NONE',  ( 99.00000000000000000, 0.000000000000000000, -7.950000000000000178 ) ) ;
#56465 = CARTESIAN_POINT ( 'NONE',  ( 85.51626352523145158, -4.472830434245839371, 4.472830434245839371 ) ) ;
#56466 = ORIENTED_EDGE ( 'NONE', *, *, #131219, .T. ) ;
#56467 = CARTESIAN_POINT ( 'NONE',  ( -48.18398860626899705, 28.73617430169820608, 5.000000000000000000 ) ) ;
#56468 = CARTESIAN_POINT ( 'NONE',  ( -25.39999999999996305, 0.000000000000000000, 0.000000000000000000 ) ) ;
#56469 = ORIENTED_EDGE ( 'NONE', *, *, #75901, .T. ) ;
#56470 = VERTEX_POINT ( 'NONE', #71098 ) ;
#56471 = LINE ( 'NONE', #44126, #118624 ) ;
#56472 = LINE ( 'NONE', #136112, #45519 ) ;
#56473 = AXIS2_PLACEMENT_3D ( 'NONE', #66230, #49310, #11804 ) ;
#56474 = LINE ( 'NONE', #79662, #39605 ) ;
#56475 = CARTESIAN_POINT ( 'NONE',  ( 3.487905803711529806, -49.11927476322659913, -40.22110306067540364 ) ) ;
#56476 = LINE ( 'NONE', #102073, #120490 ) ;
#56477 = EDGE_CURVE ( 'NONE', #25822, #33858, #61653, .T. ) ;
#56478 = LINE ( 'NONE', #34686, #33548 ) ;
#56479 = EDGE_CURVE ( 'NONE', #63415, #102811, #38345, .T. ) ;
#56480 = VECTOR ( 'NONE', #25791, 999.9999999999998863 ) ;
#56481 = ORIENTED_EDGE ( 'NONE', *, *, #86557, .F. ) ;
#56482 = ORIENTED_EDGE ( 'NONE', *, *, #98847, .F. ) ;
#56483 = ADVANCED_FACE ( 'NONE', ( #39166 ), #26148, .F. ) ;
#56484 = LINE ( 'NONE', #41999, #78122 ) ;
#56485 = VERTEX_POINT ( 'NONE', #28292 ) ;
#56486 = ORIENTED_EDGE ( 'NONE', *, *, #51351, .T. ) ;
#56487 = ADVANCED_FACE ( 'NONE', ( #72556 ), #50752, .T. ) ;
#56488 = EDGE_CURVE ( 'NONE', #42800, #46825, #137775, .T. ) ;
#56489 = VECTOR ( 'NONE', #121704, 999.9999999999998863 ) ;
#56490 = CARTESIAN_POINT ( 'NONE',  ( 7.499999999999947597, -20.53675388469229546, 2.352720554255910645 ) ) ;
#56491 = ORIENTED_EDGE ( 'NONE', *, *, #96163, .T. ) ;
#56492 = DIRECTION ( 'NONE',  ( -0.000000000000000000, -0.3543493200069152693, 0.9351131265310292928 ) ) ;
#56493 = LINE ( 'NONE', #122387, #44901 ) ;
#56494 = CARTESIAN_POINT ( 'NONE',  ( 0.000000000000000000, 0.000000000000000000, 5.000000000000000000 ) ) ;
#56495 = CARTESIAN_POINT ( 'NONE',  ( -78.48921356237309510, -27.52281430457109934, 5.000000000000000000 ) ) ;
#56496 = VERTEX_POINT ( 'NONE', #17396 ) ;
#56497 =( NAMED_UNIT ( * ) PLANE_ANGLE_UNIT ( ) SI_UNIT ( $, .RADIAN. ) );
#56498 = EDGE_CURVE ( 'NONE', #139011, #70912, #83387, .T. ) ;
#56499 = EDGE_LOOP ( 'NONE', ( #123523, #25296, #124033, #20251 ) ) ;
#56500 = LINE ( 'NONE', #91248, #34234 ) ;
#56501 = VERTEX_POINT ( 'NONE', #82676 ) ;
#56502 = FILL_AREA_STYLE ('',( #12214 ) ) ;
#56503 = ADVANCED_FACE ( 'NONE', ( #60966 ), #105126, .T. ) ;
#56504 = EDGE_LOOP ( 'NONE', ( #39558, #119380, #21816, #21702, #97813 ) ) ;
#56505 = DIRECTION ( 'NONE',  ( -0.7071067811865486830, -0.7071067811865464625, 0.000000000000000000 ) ) ;
#56506 = ORIENTED_EDGE ( 'NONE', *, *, #94034, .T. ) ;
#56507 = VERTEX_POINT ( 'NONE', #52860 ) ;
#56508 = AXIS2_PLACEMENT_3D ( 'NONE', #60029, #104194, #88204 ) ;
#56509 = ORIENTED_EDGE ( 'NONE', *, *, #10589, .F. ) ;
#56510 = ADVANCED_FACE ( 'NONE', ( #97055 ), #141317, .F. ) ;
#56511 = DIRECTION ( 'NONE',  ( -0.7071067811865486830, -0.7071067811865464625, 0.000000000000000000 ) ) ;
#56512 = VECTOR ( 'NONE', #9412, 1000.000000000000000 ) ;
#56513 = CARTESIAN_POINT ( 'NONE',  ( -16.49999999999988276, -20.94781430457062044, 5.000000000000000000 ) ) ;
#56514 = FACE_OUTER_BOUND ( 'NONE', #51692, .T. ) ;
#56515 = CARTESIAN_POINT ( 'NONE',  ( 116.2295968585647756, -6.110000000000000320, -1.637169565754161393 ) ) ;
#56516 = CARTESIAN_POINT ( 'NONE',  ( 17.99999999999986855, -18.03360074219755660, 5.000000000000000000 ) ) ;
#56517 = PLANE ( 'NONE',  #73703 ) ;
#56518 = EDGE_CURVE ( 'NONE', #133007, #40456, #86246, .T. ) ;
#56520 = CARTESIAN_POINT ( 'NONE',  ( -34.49999999999975842, 12.05432934483081553, 4.994342998332167660 ) ) ;
#56519 = VECTOR ( 'NONE', #109613, 1000.000000000000000 ) ;
#56521 = SURFACE_SIDE_STYLE ('',( #134778 ) ) ;
#56522 = VERTEX_POINT ( 'NONE', #120988 ) ;
#56523 = CARTESIAN_POINT ( 'NONE',  ( -17.02886364525924989, -2.441401769420105339, 4.000000000000000000 ) ) ;
#56525 = CARTESIAN_POINT ( 'NONE',  ( 33.79289321881321939, 9.759292476615623713, 5.000000000000000000 ) ) ;
#56524 = VECTOR ( 'NONE', #30477, 1000.000000000000000 ) ;
#56526 = DIRECTION ( 'NONE',  ( 0.7071067811865487940, -0.7071067811865463515, 0.000000000000000000 ) ) ;
#56527 = ORIENTED_EDGE ( 'NONE', *, *, #98456, .T. ) ;
#56528 = ORIENTED_EDGE ( 'NONE', *, *, #53594, .T. ) ;
#56530 = EDGE_LOOP ( 'NONE', ( #44117, #115723, #19699, #28791 ) ) ;
#56529 = EDGE_CURVE ( 'NONE', #104458, #101026, #65222, .T. ) ;
#56531 = DIRECTION ( 'NONE',  ( 0.7071067811865487940, 0.7071067811865463515, -0.000000000000000000 ) ) ;
#56532 = VERTEX_POINT ( 'NONE', #97817 ) ;
#56533 = CIRCLE ( 'NONE', #75037, 3.000000000000002665 ) ;
#56534 = ORIENTED_EDGE ( 'NONE', *, *, #13430, .T. ) ;
#56535 = DIRECTION ( 'NONE',  ( 0.000000000000000000, 0.000000000000000000, 1.000000000000000000 ) ) ;
#56536 = VECTOR ( 'NONE', #78428, 1000.000000000000227 ) ;
#56537 = FACE_OUTER_BOUND ( 'NONE', #86558, .T. ) ;
#56538 = CARTESIAN_POINT ( 'NONE',  ( 12.18398860626900060, 28.73617430169795739, 5.000000000000000000 ) ) ;
#56539 = EDGE_CURVE ( 'NONE', #69571, #29421, #65945, .T. ) ;
#56540 = VERTEX_POINT ( 'NONE', #84803 ) ;
#56541 = DIRECTION ( 'NONE',  ( 0.7071067811865487940, 0.7071067811865463515, 0.000000000000000000 ) ) ;
#56542 = ORIENTED_EDGE ( 'NONE', *, *, #104428, .T. ) ;
#56544 = AXIS2_PLACEMENT_3D ( 'NONE', #107943, #8616, #141318 ) ;
#56543 = CARTESIAN_POINT ( 'NONE',  ( -9.511686059284260253, 6.759292476615653023, 16.35960578974471957 ) ) ;
#56545 = ADVANCED_FACE ( 'NONE', ( #109406 ), #41285, .F. ) ;
#56546 = VECTOR ( 'NONE', #80758, 1000.000000000000000 ) ;
#56547 = CARTESIAN_POINT ( 'NONE',  ( 20.62956980810188412, -3.967499999999998028, -6.871911579029511330 ) ) ;
#56548 = EDGE_LOOP ( 'NONE', ( #19581, #96185, #124411, #100642, #123519 ) ) ;
#56549 = CARTESIAN_POINT ( 'NONE',  ( 82.89126352523142316, -4.472830434245839371, -4.472830434245839371 ) ) ;
#56550 =( BOUNDED_CURVE ( )  B_SPLINE_CURVE ( 3, ( #123613, #101824, #35890, #13361 ),
 .UNSPECIFIED., .F., .F. ) 
 B_SPLINE_CURVE_WITH_KNOTS ( ( 4, 4 ),
 ( 5.043186909253412509, 5.074607125596358514 ),
 .UNSPECIFIED. ) 
 CURVE ( )  GEOMETRIC_REPRESENTATION_ITEM ( )  RATIONAL_B_SPLINE_CURVE ( ( 1.000000000000000000, 0.9999177325257868620, 0.9999177325257868620, 1.000000000000000000 ) ) 
 REPRESENTATION_ITEM ( '' )  );
#56551 = DIRECTION ( 'NONE',  ( 0.6830127018922181881, 0.6830127018922202975, -0.2588190451025214056 ) ) ;
#56552 = DIRECTION ( 'NONE',  ( 1.000000000000000000, 0.000000000000000000, 0.000000000000000000 ) ) ;
#56553 = ORIENTED_EDGE ( 'NONE', *, *, #26593, .T. ) ;
#56554 = CARTESIAN_POINT ( 'NONE',  ( -4.499999999999968914, -20.56887692260760048, 4.000000000000000000 ) ) ;
#56555 = EDGE_LOOP ( 'NONE', ( #132459, #120635, #120437, #12017 ) ) ;
#56556 = ORIENTED_EDGE ( 'NONE', *, *, #60727, .T. ) ;
#56557 = FACE_OUTER_BOUND ( 'NONE', #131782, .T. ) ;
#56559 = AXIS2_PLACEMENT_3D ( 'NONE', #84548, #72277, #106243 ) ;
#56558 = DIRECTION ( 'NONE',  ( 0.6830127018922180770, -0.6830127018922204085, -0.2588190451025214056 ) ) ;
#56560 = CARTESIAN_POINT ( 'NONE',  ( 27.70710678118635073, -3.740707523384246613, 5.000000000000000000 ) ) ;
#56561 = DIRECTION ( 'NONE',  ( -0.7071067811865487940, 0.7071067811865463515, -0.000000000000000000 ) ) ;
#56562 = CARTESIAN_POINT ( 'NONE',  ( -28.49999999999979750, 15.43112307739202471, 4.000000000000000000 ) ) ;
#56563 = EDGE_LOOP ( 'NONE', ( #48451, #80001, #136142, #107427 ) ) ;
#56564 = CARTESIAN_POINT ( 'NONE',  ( -60.29974487139158867, -27.71228299555248142, 4.000000000000000000 ) ) ;
#56565 = DIRECTION ( 'NONE',  ( -0.000000000000000000, 0.000000000000000000, 1.000000000000000000 ) ) ;
#56566 = LINE ( 'NONE', #88444, #37593 ) ;
#56567 = EDGE_LOOP ( 'NONE', ( #137397, #91410, #118070, #60980 ) ) ;
#56568 = CARTESIAN_POINT ( 'NONE',  ( 18.51665438641032324, 22.22500000000000142, 4.500000000000000888 ) ) ;
#56569 = CIRCLE ( 'NONE', #105139, 2.055000000000000604 ) ;
#56570 = DIRECTION ( 'NONE',  ( -0.7071067811865487940, 0.7071067811865463515, -0.000000000000000000 ) ) ;
#56571 = VERTEX_POINT ( 'NONE', #31158 ) ;
#56573 = ORIENTED_EDGE ( 'NONE', *, *, #73192, .T. ) ;
#56572 = LINE ( 'NONE', #131954, #11612 ) ;
#56574 = ORIENTED_EDGE ( 'NONE', *, *, #14029, .F. ) ;
#56575 = EDGE_CURVE ( 'NONE', #95760, #31203, #119537, .T. ) ;
#56576 = LINE ( 'NONE', #12989, #121055 ) ;
#56577 = VERTEX_POINT ( 'NONE', #18816 ) ;
#56578 = FACE_OUTER_BOUND ( 'NONE', #33746, .T. ) ;
#56579 = UNCERTAINTY_MEASURE_WITH_UNIT (LENGTH_MEASURE( 1.000000000000000082E-05 ), #38703, 'distance_accuracy_value', 'NONE');
#56580 = DIRECTION ( 'NONE',  ( 0.7071067811865486830, -0.7071067811865464625, -0.000000000000000000 ) ) ;
#56581 = DIRECTION ( 'NONE',  ( -0.000000000000000000, 0.3543493200069153248, 0.9351131265310292928 ) ) ;
#56583 = VECTOR ( 'NONE', #140794, 1000.000000000000000 ) ;
#56582 = CARTESIAN_POINT ( 'NONE',  ( 21.32816939922338406, -21.74070752338405654, 4.000000000000000000 ) ) ;
#56584 = LINE ( 'NONE', #100749, #143211 ) ;
#56585 = DIRECTION ( 'NONE',  ( 0.7071067811865487940, 0.7071067811865463515, 0.000000000000000000 ) ) ;
#56587 = EDGE_CURVE ( 'NONE', #123496, #57984, #43445, .T. ) ;
#56586 = CARTESIAN_POINT ( 'NONE',  ( 11.56505274454301357, 4.584330080086930965E-16, 0.000000000000000000 ) ) ;
#56588 = CARTESIAN_POINT ( 'NONE',  ( -8.395137668124739605, 21.75929247661549937, 21.32995629748188193 ) ) ;
#56589 = CARTESIAN_POINT ( 'NONE',  ( 34.92499999999998295, -4.168643983631856287, 15.00153835162126903 ) ) ;
#56590 = CARTESIAN_POINT ( 'NONE',  ( 18.64540314143522437, -2.126176841940958351, -7.934999999999989839 ) ) ;
#56591 = CARTESIAN_POINT ( 'NONE',  ( -25.39999999999996305, 0.000000000000000000, 0.000000000000000000 ) ) ;
#56592 = LINE ( 'NONE', #113769, #140813 ) ;
#56593 = DIRECTION ( 'NONE',  ( 0.6830127018922180770, 0.6830127018922202975, -0.2588190451025213501 ) ) ;
#56594 = LINE ( 'NONE', #110184, #82477 ) ;
#56595 = ORIENTED_EDGE ( 'NONE', *, *, #115749, .T. ) ;
#56596 = VECTOR ( 'NONE', #8100, 1000.000000000000227 ) ;
#56597 = ORIENTED_EDGE ( 'NONE', *, *, #65968, .F. ) ;
#56598 = CARTESIAN_POINT ( 'NONE',  ( 101.3333333333333286, -6.884901960086287964, 3.974999999999998312 ) ) ;
#56599 = ORIENTED_EDGE ( 'NONE', *, *, #14184, .F. ) ;
#56600 = ORIENTED_EDGE ( 'NONE', *, *, #138396, .T. ) ;
#56601 = ORIENTED_EDGE ( 'NONE', *, *, #100448, .F. ) ;
#56602 = CARTESIAN_POINT ( 'NONE',  ( 23.99999999999984013, -8.151047557385048492, -8.977947279169853800 ) ) ;
#56603 = CARTESIAN_POINT ( 'NONE',  ( -33.18398860626899705, 28.73617430169810305, 5.000000000000000000 ) ) ;
#56604 = CARTESIAN_POINT ( 'NONE',  ( -78.18398860626899705, 28.73617430169841924, 5.000000000000000000 ) ) ;
#56605 = ORIENTED_EDGE ( 'NONE', *, *, #143458, .T. ) ;
#56606 = CARTESIAN_POINT ( 'NONE',  ( -54.29974487139159578, -27.71228299555243879, 4.000000000000000000 ) ) ;
#56607 = DIRECTION ( 'NONE',  ( -0.3543493200069162685, -0.000000000000000000, -0.9351131265310288487 ) ) ;
#56608 = CARTESIAN_POINT ( 'NONE',  ( -17.01793588964200410, 8.788317580041923094, 4.329525704382049867 ) ) ;
#56609 = LINE ( 'NONE', #45713, #39691 ) ;
#56610 = EDGE_CURVE ( 'NONE', #125114, #71992, #131062, .T. ) ;
#56611 = ORIENTED_EDGE ( 'NONE', *, *, #80232, .T. ) ;
#56612 = FACE_OUTER_BOUND ( 'NONE', #36280, .T. ) ;
#56613 = EDGE_CURVE ( 'NONE', #8014, #45414, #53618, .T. ) ;
#56614 = CARTESIAN_POINT ( 'NONE',  ( 4.495848767239241539, 4.584330080086930965E-16, 0.000000000000000000 ) ) ;
#56615 = LINE ( 'NONE', #3570, #60639 ) ;
#56616 = VECTOR ( 'NONE', #6842, 999.9999999999998863 ) ;
#56617 = DIRECTION ( 'NONE',  ( -0.7071067811865486830, -0.7071067811865464625, 0.000000000000000000 ) ) ;
#56618 = CARTESIAN_POINT ( 'NONE',  ( -23.99999999999982592, -1.447814304570811617, 5.000000000000000000 ) ) ;
#56619 = CARTESIAN_POINT ( 'NONE',  ( 3.489213562373097322, -27.52281430457057709, 5.000000000000000000 ) ) ;
#56620 = CARTESIAN_POINT ( 'NONE',  ( 86.12086038379622721, -6.884901960086286188, 3.974999999999997424 ) ) ;
#56621 = DIRECTION ( 'NONE',  ( -0.7071067811865487940, 0.7071067811865463515, 0.000000000000000000 ) ) ;
#56622 = AXIS2_PLACEMENT_3D ( 'NONE', #76346, #29254, #86518 ) ;
#56623 = EDGE_LOOP ( 'NONE', ( #114016, #27530, #44940, #142470 ) ) ;
#56624 = EDGE_LOOP ( 'NONE', ( #86155, #62027, #25125, #44693 ) ) ;
#56625 = CARTESIAN_POINT ( 'NONE',  ( 122.0629301918981042, 1.637169565754157174, 6.110000000000002984 ) ) ;
#56626 = EDGE_LOOP ( 'NONE', ( #80649, #29983, #48966, #9373 ) ) ;
#56627 = ADVANCED_FACE ( 'NONE', ( #64480 ), #131885, .F. ) ;
#56628 = VECTOR ( 'NONE', #13534, 999.9999999999998863 ) ;
#56629 = CARTESIAN_POINT ( 'NONE',  ( 34.42499999999998295, -21.72500000000000142, 0.5000000000000000000 ) ) ;
#56630 = FACE_OUTER_BOUND ( 'NONE', #49825, .T. ) ;
#56631 = EDGE_CURVE ( 'NONE', #3592, #136288, #142067, .T. ) ;
#56632 = LINE ( 'NONE', #33438, #46736 ) ;
#56633 = CARTESIAN_POINT ( 'NONE',  ( 30.48921356237309510, -27.52281430457076894, 5.000000000000000000 ) ) ;
#56634 = CARTESIAN_POINT ( 'NONE',  ( 111.1829301918981230, -1.637169565754158951, -6.109999999999998543 ) ) ;
#56635 = VECTOR ( 'NONE', #38325, 1000.000000000000000 ) ;
#56636 = VERTEX_POINT ( 'NONE', #118107 ) ;
#56637 = ORIENTED_EDGE ( 'NONE', *, *, #139767, .T. ) ;
#56638 = EDGE_CURVE ( 'NONE', #112641, #127735, #107256, .T. ) ;
#56639 = CARTESIAN_POINT ( 'NONE',  ( 8.816011393731004731, 28.73617430169781173, 5.000000000000000000 ) ) ;
#56640 = ORIENTED_EDGE ( 'NONE', *, *, #80794, .F. ) ;
#56641 = EDGE_LOOP ( 'NONE', ( #95347, #120362, #22669, #107604 ) ) ;
#56642 = CARTESIAN_POINT ( 'NONE',  ( 37.33376352523143282, 6.110000000000001208, 1.122388791418549305E-15 ) ) ;
#56643 = VERTEX_POINT ( 'NONE', #20958 ) ;
#56644 = DIRECTION ( 'NONE',  ( -0.000000000000000000, 0.3543493200069153248, 0.9351131265310292928 ) ) ;
#56645 = CARTESIAN_POINT ( 'NONE',  ( 3.567069808101886341, 2.126176841940952134, -7.934999999999992504 ) ) ;
#56646 = AXIS2_PLACEMENT_3D ( 'NONE', #142095, #63115, #86973 ) ;
#56647 =( GEOMETRIC_REPRESENTATION_CONTEXT ( 3 ) GLOBAL_UNCERTAINTY_ASSIGNED_CONTEXT ( ( #113024 ) ) GLOBAL_UNIT_ASSIGNED_CONTEXT ( ( #133699, #78600, #101045 ) ) REPRESENTATION_CONTEXT ( 'NONE', 'WORKASPACE' ) );
#56648 = VECTOR ( 'NONE', #56561, 999.9999999999998863 ) ;
#56649 = CARTESIAN_POINT ( 'NONE',  ( 26.74543019189810877, -5.291415217122918513, -3.055000000000000160 ) ) ;
#56650 = ORIENTED_EDGE ( 'NONE', *, *, #47807, .T. ) ;
#56651 = ADVANCED_FACE ( 'NONE', ( #52169 ), #131162, .T. ) ;
#56652 = CARTESIAN_POINT ( 'NONE',  ( -29.20710678118634007, -5.240707523384228850, 5.000000000000000000 ) ) ;
#56653 = ORIENTED_EDGE ( 'NONE', *, *, #64600, .F. ) ;
#56654 = ORIENTED_EDGE ( 'NONE', *, *, #90137, .F. ) ;
#56655 = VERTEX_POINT ( 'NONE', #56513 ) ;
#56656 = EDGE_CURVE ( 'NONE', #128813, #106215, #127072, .T. ) ;
#56657 = EDGE_CURVE ( 'NONE', #78474, #118381, #57207, .T. ) ;
#56658 = FACE_OUTER_BOUND ( 'NONE', #9158, .T. ) ;
#56659 = DIRECTION ( 'NONE',  ( 0.7071067811865487940, 0.7071067811865463515, -0.000000000000000000 ) ) ;
#56660 = ORIENTED_EDGE ( 'NONE', *, *, #115661, .F. ) ;
#56661 = CARTESIAN_POINT ( 'NONE',  ( -11.99999999999991296, -2.904428200921318481, -6.989807076074915138 ) ) ;
#56662 = DIRECTION ( 'NONE',  ( -0.000000000000000000, 1.000000000000000000, -0.000000000000000000 ) ) ;
#56663 = CARTESIAN_POINT ( 'NONE',  ( -5.510786437626906675, -27.52281430457051314, 5.000000000000000000 ) ) ;
#56664 = ADVANCED_FACE ( 'NONE', ( #110803 ), #59944, .T. ) ;
#56665 = CARTESIAN_POINT ( 'NONE',  ( 1.176659101599728752, 5.259292476615672562, 15.86257073897097847 ) ) ;
#56666 = FACE_BOUND ( 'NONE', #41618, .T. ) ;
#56667 = EDGE_CURVE ( 'NONE', #35104, #59514, #102118, .T. ) ;
#56668 = ORIENTED_EDGE ( 'NONE', *, *, #91337, .F. ) ;
#56669 = CARTESIAN_POINT ( 'NONE',  ( 27.48921356237309155, -27.52281430457074762, 5.000000000000000000 ) ) ;
#56670 = CARTESIAN_POINT ( 'NONE',  ( 23.20710678118638626, -2.240707523384260824, 5.000000000000000000 ) ) ;
#56671 = CARTESIAN_POINT ( 'NONE',  ( 0.000000000000000000, 0.000000000000000000, 7.950000000000000178 ) ) ;
#56672 = CARTESIAN_POINT ( 'NONE',  ( 7.799999601179139042, 2.500000000000001776, 3.061616997868385113E-16 ) ) ;
#56673 = ADVANCED_FACE ( 'NONE', ( #88394 ), #89105, .T. ) ;
#56674 = ORIENTED_EDGE ( 'NONE', *, *, #9114, .F. ) ;
#56675 = CARTESIAN_POINT ( 'NONE',  ( 24.25413961620377279, 3.047499999999993214, -5.278424836066146320 ) ) ;
#56676 = ORIENTED_EDGE ( 'NONE', *, *, #137035, .T. ) ;
#56677 = VERTEX_POINT ( 'NONE', #132631 ) ;
#56678 = ORIENTED_EDGE ( 'NONE', *, *, #36890, .T. ) ;
#56679 = CARTESIAN_POINT ( 'NONE',  ( 42.78709685856478728, 3.054999999999997495, 5.291415217122919401 ) ) ;
#56680 = EDGE_CURVE ( 'NONE', #112275, #39158, #69256, .T. ) ;
#56681 = ORIENTED_EDGE ( 'NONE', *, *, #104845, .T. ) ;
#56682 = EDGE_CURVE ( 'NONE', #69422, #46533, #66633, .T. ) ;
#56683 = CARTESIAN_POINT ( 'NONE',  ( 5.207106781186502609, -20.24070752338407431, 5.000000000000000000 ) ) ;
#56684 = CARTESIAN_POINT ( 'NONE',  ( -69.29974487139159578, -27.71228299555254537, 4.000000000000000000 ) ) ;
#56685 = EDGE_LOOP ( 'NONE', ( #61552, #15669, #23567, #72752, #118404 ) ) ;
#56686 = CARTESIAN_POINT ( 'NONE',  ( 0.4116149059483135697, 22.22500000000000142, 4.777194822843816802 ) ) ;
#56687 = CARTESIAN_POINT ( 'NONE',  ( 160.0000000000000000, 7.776507174585690191E-16, -6.349999999999997868 ) ) ;
#56688 = EDGE_CURVE ( 'NONE', #98793, #22459, #99327, .T. ) ;
#56689 = VECTOR ( 'NONE', #84127, 1000.000000000000000 ) ;
#56690 = FILL_AREA_STYLE_COLOUR ( '', #68788 ) ;
#56691 = DIRECTION ( 'NONE',  ( -1.000000000000000000, -1.224606353822377258E-16, -0.000000000000000000 ) ) ;
#56692 = DIRECTION ( 'NONE',  ( -0.7071067811865486830, 0.7071067811865464625, 0.000000000000000000 ) ) ;
#56693 = VERTEX_POINT ( 'NONE', #112282 ) ;
#56694 = ORIENTED_EDGE ( 'NONE', *, *, #65779, .F. ) ;
#56695 = ORIENTED_EDGE ( 'NONE', *, *, #134300, .F. ) ;
#56696 = ORIENTED_EDGE ( 'NONE', *, *, #121246, .F. ) ;
#56697 = DIRECTION ( 'NONE',  ( -0.7071067811865487940, 0.7071067811865463515, -0.000000000000000000 ) ) ;
#56698 = CARTESIAN_POINT ( 'NONE',  ( 35.95419371712956291, 6.884901960086283523, 3.975000000000002753 ) ) ;
#56699 = VERTEX_POINT ( 'NONE', #68099 ) ;
#56700 = ORIENTED_EDGE ( 'NONE', *, *, #31991, .T. ) ;
#56701 = DIRECTION ( 'NONE',  ( -0.3543493200069162685, -0.000000000000000000, -0.9351131265310288487 ) ) ;
#56702 = DIRECTION ( 'NONE',  ( -0.000000000000000000, 0.000000000000000000, 1.000000000000000000 ) ) ;
#56703 = VERTEX_POINT ( 'NONE', #79696 ) ;
#56704 = EDGE_CURVE ( 'NONE', #106514, #61464, #78227, .T. ) ;
#56705 = CARTESIAN_POINT ( 'NONE',  ( -8.999999999999936051, 13.55218569542903495, 5.000000000000000000 ) ) ;
#56706 = EDGE_CURVE ( 'NONE', #37184, #123300, #89789, .T. ) ;
#56707 = LINE ( 'NONE', #100869, #86145 ) ;
#56708 = EDGE_CURVE ( 'NONE', #61158, #15400, #67354, .T. ) ;
#56709 = VECTOR ( 'NONE', #107364, 1000.000000000000000 ) ;
#56710 = CARTESIAN_POINT ( 'NONE',  ( 23.40040314143521982, -7.934999999999989839, 2.126176841940957907 ) ) ;
#56711 = FACE_OUTER_BOUND ( 'NONE', #94703, .T. ) ;
#56712 = ORIENTED_EDGE ( 'NONE', *, *, #40867, .T. ) ;
#56714 = CARTESIAN_POINT ( 'NONE',  ( -10.49999999999992895, 0.4311230773921849169, 4.000000000000000000 ) ) ;
#56713 = CARTESIAN_POINT ( 'NONE',  ( 108.8495968585647660, 6.109999999999997655, 1.637169565754163836 ) ) ;
#56715 = VECTOR ( 'NONE', #72102, 1000.000000000000000 ) ;
#56716 = DIRECTION ( 'NONE',  ( 0.7071067811865487940, 0.7071067811865463515, 0.000000000000000000 ) ) ;
#56717 = LINE ( 'NONE', #79895, #74362 ) ;
#56718 = LINE ( 'NONE', #67576, #75040 ) ;
#56720 = VERTEX_POINT ( 'NONE', #134031 ) ;
#56719 = DIRECTION ( 'NONE',  ( -0.000000000000000000, 0.3543493200069153248, 0.9351131265310292928 ) ) ;
#56721 = PLANE ( 'NONE',  #134183 ) ;
#56722 = ORIENTED_EDGE ( 'NONE', *, *, #30537, .F. ) ;
#56723 = PLANE ( 'NONE',  #12701 ) ;
#56724 = EDGE_CURVE ( 'NONE', #66617, #118405, #35999, .T. ) ;
#56725 = CARTESIAN_POINT ( 'NONE',  ( 21.32816939922338051, 14.25929247661557397, 4.000000000000000000 ) ) ;
#56726 = CARTESIAN_POINT ( 'NONE',  ( 121.3124999999999858, 5.819803920172571310, 5.819803920172576639 ) ) ;
#56727 = ORIENTED_EDGE ( 'NONE', *, *, #121238, .T. ) ;
#56728 = FACE_OUTER_BOUND ( 'NONE', #75390, .T. ) ;
#56729 = VECTOR ( 'NONE', #59917, 1000.000000000000000 ) ;
#56730 = DIRECTION ( 'NONE',  ( 0.6830127018922181881, 0.6830127018922202975, -0.2588190451025214056 ) ) ;
#56731 = CARTESIAN_POINT ( 'NONE',  ( 17.39159235450332019, 9.902892378096218942E-16, 0.000000000000000000 ) ) ;
#56732 = VERTEX_POINT ( 'NONE', #125857 ) ;
#56733 = PLANE ( 'NONE',  #21470 ) ;
#56734 = ORIENTED_EDGE ( 'NONE', *, *, #115787, .F. ) ;
#56735 = DIRECTION ( 'NONE',  ( -1.000000000000000000, -1.224606353822377258E-16, -0.000000000000000000 ) ) ;
#56737 = ORIENTED_EDGE ( 'NONE', *, *, #77218, .F. ) ;
#56736 = CARTESIAN_POINT ( 'NONE',  ( 6.938893903907228378E-15, 11.96639925780214675, 5.000000000000000000 ) ) ;
#56738 = EDGE_LOOP ( 'NONE', ( #73631, #20204, #35440 ) ) ;
#56739 = CARTESIAN_POINT ( 'NONE',  ( -34.92500000000001137, -22.22500000000000142, 4.000000000000000000 ) ) ;
#56740 = DIRECTION ( 'NONE',  ( 0.7071067811865486830, -0.7071067811865464625, -0.000000000000000000 ) ) ;
#56741 = ORIENTED_EDGE ( 'NONE', *, *, #129645, .T. ) ;
#56742 = VECTOR ( 'NONE', #20338, 1000.000000000000000 ) ;
#56743 = LINE ( 'NONE', #126068, #103763 ) ;
#56744 = PRESENTATION_LAYER_ASSIGNMENT (  '', '', ( #47438 ) ) ;
#56745 = VECTOR ( 'NONE', #75914, 999.9999999999998863 ) ;
#56746 = FACE_OUTER_BOUND ( 'NONE', #35549, .T. ) ;
#56747 = DIRECTION ( 'NONE',  ( 0.6830127018922181881, 0.6830127018922202975, -0.2588190451025214056 ) ) ;
#56748 = ORIENTED_EDGE ( 'NONE', *, *, #6116, .T. ) ;
#56749 = AXIS2_PLACEMENT_3D ( 'NONE', #54391, #87696, #142792 ) ;
#56750 = CARTESIAN_POINT ( 'NONE',  ( 9.005480084712511157, 28.92564299267931816, 4.000000000000000000 ) ) ;
#56751 = CARTESIAN_POINT ( 'NONE',  ( -34.92500000000001137, 21.72500000000000142, 5.000000000000000000 ) ) ;
#56752 = CARTESIAN_POINT ( 'NONE',  ( -1.180000000000000160, 9.043340090917734386, 10.00000000000000000 ) ) ;
#56753 = DIRECTION ( 'NONE',  ( -0.000000000000000000, 0.000000000000000000, 1.000000000000000000 ) ) ;
#56754 = DIRECTION ( 'NONE',  ( -0.000000000000000000, -0.3543493200069152693, 0.9351131265310292928 ) ) ;
#56755 = CARTESIAN_POINT ( 'NONE',  ( 128.5583603837962130, -7.949999999999997513, -2.130196079827425759 ) ) ;
#56756 = LINE ( 'NONE', #120489, #69777 ) ;
#56757 = EDGE_LOOP ( 'NONE', ( #105004, #85509, #232, #114597 ) ) ;
#56758 = ORIENTED_EDGE ( 'NONE', *, *, #37322, .F. ) ;
#56759 = ORIENTED_EDGE ( 'NONE', *, *, #22708, .T. ) ;
#56760 = LINE ( 'NONE', #22613, #111331 ) ;
#56761 = VERTEX_POINT ( 'NONE', #67940 ) ;
#56762 = ORIENTED_EDGE ( 'NONE', *, *, #99598, .T. ) ;
#56763 = ORIENTED_EDGE ( 'NONE', *, *, #124211, .F. ) ;
#56764 = CARTESIAN_POINT ( 'NONE',  ( 0.5388684133533581111, -7.552109465304689628, -0.3911787640923247711 ) ) ;
#56765 = DIRECTION ( 'NONE',  ( -0.7071067811865486830, -0.7071067811865464625, -0.000000000000000000 ) ) ;
#56766 = VERTEX_POINT ( 'NONE', #104051 ) ;
#56767 = CARTESIAN_POINT ( 'NONE',  ( 13.49999999999991118, -7.420205493532887608, -2.617629953481223293 ) ) ;
#56768 = DIRECTION ( 'NONE',  ( 0.7071067811865487940, 0.7071067811865463515, 0.000000000000000000 ) ) ;
#56769 = ADVANCED_FACE ( 'NONE', ( #26530 ), #14920, .F. ) ;
#56770 = LINE ( 'NONE', #142323, #23160 ) ;
#56771 = CARTESIAN_POINT ( 'NONE',  ( -6.792893218813407685, 3.759292476615680112, 5.000000000000000000 ) ) ;
#56772 = CARTESIAN_POINT ( 'NONE',  ( 118.8545968585647898, -1.637169565754161615, 6.110000000000000320 ) ) ;
#56773 = EDGE_CURVE ( 'NONE', #82756, #23807, #13470, .T. ) ;
#56774 = ORIENTED_EDGE ( 'NONE', *, *, #114687, .T. ) ;
#56775 = LINE ( 'NONE', #26249, #39537 ) ;
#56776 = LINE ( 'NONE', #98096, #93182 ) ;
#56777 = CARTESIAN_POINT ( 'NONE',  ( 78.43750000000000000, 5.819803920172574863, -5.819803920172573086 ) ) ;
#56778 = DIRECTION ( 'NONE',  ( 0.000000000000000000, -1.000000000000000000, 0.000000000000000000 ) ) ;
#56779 = DIRECTION ( 'NONE',  ( -1.000000000000000000, -1.224606353822377258E-16, -0.000000000000000000 ) ) ;
#56780 = CARTESIAN_POINT ( 'NONE',  ( 9.654944837453772521, 5.259292476615669010, 12.77922209995895919 ) ) ;
#56781 = LINE ( 'NONE', #137159, #50468 ) ;
#56782 = EDGE_CURVE ( 'NONE', #18270, #98423, #80225, .T. ) ;
#56784 = EDGE_CURVE ( 'NONE', #5826, #100179, #124409, .T. ) ;
#56783 = CARTESIAN_POINT ( 'NONE',  ( 51.85002705046287730, -5.819803920172572198, -5.819803920172572198 ) ) ;
#56785 = DIRECTION ( 'NONE',  ( 0.7071067811865486830, -0.7071067811865464625, -0.000000000000000000 ) ) ;
#56786 = DIRECTION ( 'NONE',  ( -0.000000000000000000, 0.000000000000000000, 1.000000000000000000 ) ) ;
#56787 = ORIENTED_EDGE ( 'NONE', *, *, #101420, .F. ) ;
#56788 = VERTEX_POINT ( 'NONE', #112813 ) ;
#56789 = CARTESIAN_POINT ( 'NONE',  ( 47.66666666666666430, 6.884901960086285300, 3.975000000000003642 ) ) ;
#56790 = EDGE_CURVE ( 'NONE', #82218, #108587, #80920, .T. ) ;
#56791 = DIRECTION ( 'NONE',  ( -0.6830127018922181881, 0.6830127018922202975, -0.2588190451025214056 ) ) ;
#56792 = VERTEX_POINT ( 'NONE', #135997 ) ;
#56793 = LINE ( 'NONE', #56067, #133597 ) ;
#56794 = DIRECTION ( 'NONE',  ( -0.7071067811865487940, 0.7071067811865463515, 0.000000000000000000 ) ) ;
#56795 = EDGE_CURVE ( 'NONE', #72734, #106882, #101943, .T. ) ;
#56796 = CARTESIAN_POINT ( 'NONE',  ( 35.43793019189810423, -6.110000000000001208, 1.637169565754158951 ) ) ;
#56797 = VERTEX_POINT ( 'NONE', #3997 ) ;
#56798 =( NAMED_UNIT ( * ) PLANE_ANGLE_UNIT ( ) SI_UNIT ( $, .RADIAN. ) );
#56799 = ORIENTED_EDGE ( 'NONE', *, *, #7544, .F. ) ;
#56800 = DIRECTION ( 'NONE',  ( 0.000000000000000000, 0.000000000000000000, 1.000000000000000000 ) ) ;
#56801 = EDGE_CURVE ( 'NONE', #42167, #89926, #136702, .T. ) ;
#56802 = FACE_OUTER_BOUND ( 'NONE', #102683, .T. ) ;
#56803 = DIRECTION ( 'NONE',  ( -0.7071067811865486830, -0.7071067811865464625, 0.000000000000000000 ) ) ;
#56804 = CARTESIAN_POINT ( 'NONE',  ( 25.39999999999999858, 0.000000000000000000, 0.000000000000000000 ) ) ;
#56805 = VERTEX_POINT ( 'NONE', #69331 ) ;
#56806 = FACE_OUTER_BOUND ( 'NONE', #4897, .T. ) ;
#56807 = VERTEX_POINT ( 'NONE', #125116 ) ;
#56808 = LINE ( 'NONE', #100971, #70260 ) ;
#56809 = LINE ( 'NONE', #67681, #62412 ) ;
#56810 = CARTESIAN_POINT ( 'NONE',  ( -25.49999999999982236, 9.052185695429074030, 5.000000000000000000 ) ) ;
#56811 = EDGE_CURVE ( 'NONE', #131612, #62746, #58501, .T. ) ;
#56812 = DIRECTION ( 'NONE',  ( 0.7071067811865487940, -0.7071067811865463515, 0.000000000000000000 ) ) ;
#56813 = CARTESIAN_POINT ( 'NONE',  ( -14.28242261357422116, -21.73023691814492864, 5.000000000000000888 ) ) ;
#56814 = VECTOR ( 'NONE', #33253, 1000.000000000000000 ) ;
#56815 = ORIENTED_EDGE ( 'NONE', *, *, #132405, .F. ) ;
#56816 = DIRECTION ( 'NONE',  ( -0.000000000000000000, 0.000000000000000000, 1.000000000000000000 ) ) ;
#56817 = CARTESIAN_POINT ( 'NONE',  ( 56.93293019189810877, 1.637169565754156508, 6.110000000000000320 ) ) ;
#56818 = COLOUR_RGB ( '', 0.09019608, 0.27058824, 0.51372549) ;
#56819 = DIRECTION ( 'NONE',  ( -1.000000000000000000, -1.224606353822377258E-16, -0.000000000000000000 ) ) ;
#56820 = EDGE_CURVE ( 'NONE', #34380, #6222, #89636, .T. ) ;
#56821 = CARTESIAN_POINT ( 'NONE',  ( -14.70025512860841133, -27.71228299555195917, 4.000000000000000000 ) ) ;
#56822 = CARTESIAN_POINT ( 'NONE',  ( -45.18398860626900415, 28.73617430169818832, 5.000000000000000000 ) ) ;
#56823 = VERTEX_POINT ( 'NONE', #133861 ) ;
#56824 = DIRECTION ( 'NONE',  ( -1.000000000000000000, -1.369518533665899572E-16, 0.000000000000000000 ) ) ;
#56825 = ORIENTED_EDGE ( 'NONE', *, *, #49894, .F. ) ;
#56826 =( BOUNDED_CURVE ( )  B_SPLINE_CURVE ( 3, ( #74964, #19821, #61258, #64062 ),
 .UNSPECIFIED., .F., .F. ) 
 B_SPLINE_CURVE_WITH_KNOTS ( ( 4, 4 ),
 ( 4.350170835173025274, 4.500739107949270235 ),
 .UNSPECIFIED. ) 
 CURVE ( )  GEOMETRIC_REPRESENTATION_ITEM ( )  RATIONAL_B_SPLINE_CURVE ( ( 1.000000000000000000, 0.9981116584018941973, 0.9981116584018941973, 1.000000000000000000 ) ) 
 REPRESENTATION_ITEM ( '' )  );
#56827 = ADVANCED_FACE ( 'NONE', ( #25075 ), #1860, .F. ) ;
#56828 = AXIS2_PLACEMENT_3D ( 'NONE', #64545, #36215, #135529 ) ;
#56829 = LINE ( 'NONE', #111132, #93115 ) ;
#56831 = ADVANCED_FACE ( 'NONE', ( #78779 ), #102677, .T. ) ;
#56830 = VERTEX_POINT ( 'NONE', #113516 ) ;
#56832 = DIRECTION ( 'NONE',  ( 1.000000000000000000, 0.000000000000000000, 0.000000000000000000 ) ) ;
#56833 = CARTESIAN_POINT ( 'NONE',  ( -27.18398860626900060, 28.73617430169806042, 5.000000000000000000 ) ) ;
#56834 = LINE ( 'NONE', #100994, #69411 ) ;
#56835 = EDGE_CURVE ( 'NONE', #28781, #58036, #57049, .T. ) ;
#56836 = PLANE ( 'NONE',  #115951 ) ;
#56837 = FACE_BOUND ( 'NONE', #142518, .T. ) ;
#56838 = DIRECTION ( 'NONE',  ( 1.000000000000000000, 0.000000000000000000, 0.000000000000000000 ) ) ;
#56839 = PLANE ( 'NONE',  #58368 ) ;
#56840 = CARTESIAN_POINT ( 'NONE',  ( 28.49999999999980105, -8.568876922607731927, 4.000000000000000000 ) ) ;
#56842 = ORIENTED_EDGE ( 'NONE', *, *, #29111, .T. ) ;
#56841 = CARTESIAN_POINT ( 'NONE',  ( 9.183988606268997046, 28.73617430169793607, 5.000000000000000000 ) ) ;
#56843 = DIRECTION ( 'NONE',  ( 0.000000000000000000, -1.000000000000000000, 0.000000000000000000 ) ) ;
#56844 = VECTOR ( 'NONE', #99891, 1000.000000000000000 ) ;
#56845 = VERTEX_POINT ( 'NONE', #14209 ) ;
#56846 = VECTOR ( 'NONE', #67756, 999.9999999999998863 ) ;
#56848 = ORIENTED_EDGE ( 'NONE', *, *, #36437, .F. ) ;
#56847 = VECTOR ( 'NONE', #69615, 1000.000000000000000 ) ;
#56849 = CARTESIAN_POINT ( 'NONE',  ( 78.37043019189812298, -3.055000000000001492, 5.291415217122917625 ) ) ;
#56850 = ORIENTED_EDGE ( 'NONE', *, *, #73955, .T. ) ;
#56851 = CARTESIAN_POINT ( 'NONE',  ( -26.99999999999981171, -21.84840872380826937, 2.849755605029545169 ) ) ;
#56852 = VECTOR ( 'NONE', #66288, 1000.000000000000000 ) ;
#56853 = EDGE_CURVE ( 'NONE', #112333, #122403, #46171, .T. ) ;
#56854 = LINE ( 'NONE', #40084, #34873 ) ;
#56855 = EDGE_LOOP ( 'NONE', ( #31296, #126900, #25428 ) ) ;
#56856 = DIRECTION ( 'NONE',  ( 1.000000000000000000, 0.000000000000000000, 0.000000000000000000 ) ) ;
#56857 = EDGE_CURVE ( 'NONE', #30899, #103815, #123724, .T. ) ;
#56858 = CARTESIAN_POINT ( 'NONE',  ( 122.9166666666666714, -6.884901960086287076, -3.975000000000000977 ) ) ;
#56859 = DIRECTION ( 'NONE',  ( 0.6830127018922181881, 0.6830127018922202975, -0.2588190451025214056 ) ) ;
#56860 =( LENGTH_UNIT ( ) NAMED_UNIT ( * ) SI_UNIT ( .MILLI., .METRE. ) );
#56862 = LINE ( 'NONE', #132981, #72808 ) ;
#56861 = DIRECTION ( 'NONE',  ( -0.6830127018922181881, 0.6830127018922202975, -0.2588190451025214056 ) ) ;
#56863 = CARTESIAN_POINT ( 'NONE',  ( 17.84878961325748037, -2.500000000000000000, 3.061616997868383634E-16 ) ) ;
#56864 = LINE ( 'NONE', #101020, #104131 ) ;
#56865 = VERTEX_POINT ( 'NONE', #3319 ) ;
#56866 = VERTEX_POINT ( 'NONE', #36673 ) ;
#56867 = LINE ( 'NONE', #103172, #58994 ) ;
#56868 = CARTESIAN_POINT ( 'NONE',  ( 10.93003974513585064, -0.7407075233842805861, 13.87443053587608333 ) ) ;
#56869 = ORIENTED_EDGE ( 'NONE', *, *, #120630, .F. ) ;
#56870 = ORIENTED_EDGE ( 'NONE', *, *, #125828, .F. ) ;
#56871 = VERTEX_POINT ( 'NONE', #49738 ) ;
#56872 = CARTESIAN_POINT ( 'NONE',  ( 26.83376352523143993, 6.110000000000001208, 1.122388791418549305E-15 ) ) ;
#56873 = ORIENTED_EDGE ( 'NONE', *, *, #48196, .T. ) ;
#56874 = DIRECTION ( 'NONE',  ( -0.7071067811865486830, -0.7071067811865464625, 0.000000000000000000 ) ) ;
#56875 = EDGE_CURVE ( 'NONE', #18494, #132815, #5455, .T. ) ;
#56876 = CARTESIAN_POINT ( 'NONE',  ( 89.91252705046289861, -7.949999999999998401, -4.867971026610728450E-16 ) ) ;
#56877 = CARTESIAN_POINT ( 'NONE',  ( 32.27497294953710849, 4.461849672132300881, 4.461849672132299105 ) ) ;
#56878 = CARTESIAN_POINT ( 'NONE',  ( 16.63593005512386824, 5.882511235426649776, -28.99105463435266472 ) ) ;
#56879 = VERTEX_POINT ( 'NONE', #94616 ) ;
#56880 = CARTESIAN_POINT ( 'NONE',  ( -34.92500000000001137, -13.27521306008089930, -8.452357796116194422 ) ) ;
#56881 = CARTESIAN_POINT ( 'NONE',  ( -11.20666063542143753, 21.75929247661549937, 4.998822639870708073 ) ) ;
#56882 = DIRECTION ( 'NONE',  ( 0.7071067811865487940, 0.7071067811865463515, 0.000000000000000000 ) ) ;
#56884 = ORIENTED_EDGE ( 'NONE', *, *, #134231, .F. ) ;
#56883 = DIRECTION ( 'NONE',  ( -0.7071067811865487940, 0.7071067811865463515, -0.000000000000000000 ) ) ;
#56885 = ORIENTED_EDGE ( 'NONE', *, *, #19235, .F. ) ;
#56886 = LINE ( 'NONE', #67764, #100118 ) ;
#56887 = DIRECTION ( 'NONE',  ( 0.000000000000000000, -1.000000000000000000, 0.000000000000000000 ) ) ;
#56888 = ORIENTED_EDGE ( 'NONE', *, *, #57926, .F. ) ;
#56889 = PRESENTATION_STYLE_ASSIGNMENT (( #113347 ) ) ;
#56890 = LINE ( 'NONE', #35854, #14707 ) ;
#56891 = FACE_OUTER_BOUND ( 'NONE', #138771, .T. ) ;
#56892 = CARTESIAN_POINT ( 'NONE',  ( 27.18398860626900060, 28.73617430169806042, 5.000000000000000000 ) ) ;
#56893 = CARTESIAN_POINT ( 'NONE',  ( -4.499999999999976019, 16.18958161055402201, -11.56426086740812487 ) ) ;
#56894 = CARTESIAN_POINT ( 'NONE',  ( 18.18398860626898994, 28.73617430169800002, 5.000000000000000000 ) ) ;
#56895 = LINE ( 'NONE', #24238, #23988 ) ;
#56896 = CARTESIAN_POINT ( 'NONE',  ( -29.99451991528749417, 28.92564299267958816, 4.000000000000000000 ) ) ;
#56897 = EDGE_LOOP ( 'NONE', ( #59564, #18304, #117624, #83203 ) ) ;
#56898 = ORIENTED_EDGE ( 'NONE', *, *, #89851, .F. ) ;
#56899 = FACE_OUTER_BOUND ( 'NONE', #116604, .T. ) ;
#56900 = DIRECTION ( 'NONE',  ( -0.7071067811865487940, 0.7071067811865463515, -0.000000000000000000 ) ) ;
#56901 = FILL_AREA_STYLE_COLOUR ( '', #96008 ) ;
#56902 = DIRECTION ( 'NONE',  ( 1.000000000000000000, 0.000000000000000000, 0.000000000000000000 ) ) ;
#56903 = ORIENTED_EDGE ( 'NONE', *, *, #127783, .T. ) ;
#56904 = CARTESIAN_POINT ( 'NONE',  ( 7.171830600776423204, 15.75929247661555976, 4.000000000000000000 ) ) ;
#56905 = DIRECTION ( 'NONE',  ( -0.000000000000000000, 0.3543493200069153248, 0.9351131265310292928 ) ) ;
#56906 = CARTESIAN_POINT ( 'NONE',  ( 13.11345250541376473, 3.796869306786346598, 4.054893674211259125 ) ) ;
#56907 = VECTOR ( 'NONE', #43229, 999.9999999999998863 ) ;
#56908 = ORIENTED_EDGE ( 'NONE', *, *, #12582, .F. ) ;
#56909 = CARTESIAN_POINT ( 'NONE',  ( 111.8333333333333428, -6.884901960086287964, 3.974999999999998312 ) ) ;
#56910 = LINE ( 'NONE', #1732, #95569 ) ;
#56911 = CARTESIAN_POINT ( 'NONE',  ( 17.51078643762690845, -27.52281430457043143, 5.000000000000000000 ) ) ;
#56912 = CARTESIAN_POINT ( 'NONE',  ( 54.45376352523144448, -6.109999999999999432, -3.741295971395163529E-16 ) ) ;
#56913 = DIRECTION ( 'NONE',  ( -0.7071067811865486830, 0.7071067811865464625, 0.000000000000000000 ) ) ;
#56914 = VECTOR ( 'NONE', #128745, 1000.000000000000000 ) ;
#56915 = FACE_OUTER_BOUND ( 'NONE', #7058, .T. ) ;
#56916 = LINE ( 'NONE', #35881, #18635 ) ;
#56917 = ORIENTED_EDGE ( 'NONE', *, *, #93252, .F. ) ;
#56918 = CARTESIAN_POINT ( 'NONE',  ( -3.328169399223496860, -9.740707523384180888, 4.000000000000000000 ) ) ;
#56919 = ORIENTED_EDGE ( 'NONE', *, *, #139290, .F. ) ;
#56920 = DIRECTION ( 'NONE',  ( 0.000000000000000000, -1.000000000000000000, 0.000000000000000000 ) ) ;
#56921 = FILL_AREA_STYLE ('',( #115503 ) ) ;
#56922 = DIRECTION ( 'NONE',  ( -0.6830127018922181881, 0.6830127018922202975, -0.2588190451025214056 ) ) ;
#56923 = DIRECTION ( 'NONE',  ( 0.3543493200069162685, -0.000000000000000000, -0.9351131265310288487 ) ) ;
#56924 = CARTESIAN_POINT ( 'NONE',  ( -0.4892135623730947680, -27.52281430457055578, 5.000000000000000000 ) ) ;
#56925 = DIRECTION ( 'NONE',  ( -0.6830127018922180770, -0.6830127018922204085, -0.2588190451025213501 ) ) ;
#56926 = EDGE_CURVE ( 'NONE', #6521, #78331, #6155, .T. ) ;
#56927 = EDGE_CURVE ( 'NONE', #27120, #1016, #20441, .T. ) ;
#56928 = ORIENTED_EDGE ( 'NONE', *, *, #82275, .F. ) ;
#56929 = ORIENTED_EDGE ( 'NONE', *, *, #28532, .T. ) ;
#56930 = CARTESIAN_POINT ( 'NONE',  ( 5.816011393731002066, 28.73617430169783304, 5.000000000000000000 ) ) ;
#56931 = FACE_OUTER_BOUND ( 'NONE', #9730, .T. ) ;
#56932 = CARTESIAN_POINT ( 'NONE',  ( -8.510786437626906675, -27.52281430457049183, 5.000000000000000000 ) ) ;
#56933 = VECTOR ( 'NONE', #13397, 1000.000000000000227 ) ;
#56934 = DIRECTION ( 'NONE',  ( 0.7071067811865487940, 0.7071067811865463515, 0.000000000000000000 ) ) ;
#56935 = EDGE_CURVE ( 'NONE', #81524, #19482, #94768, .T. ) ;
#56937 = EDGE_CURVE ( 'NONE', #106357, #105369, #115553, .T. ) ;
#56936 = CARTESIAN_POINT ( 'NONE',  ( 77.37086038379622721, 6.884901960086289741, -3.974999999999993427 ) ) ;
#56938 = DIRECTION ( 'NONE',  ( 1.000000000000000000, -0.000000000000000000, 0.000000000000000000 ) ) ;
#56939 = VECTOR ( 'NONE', #43734, 1000.000000000000000 ) ;
#56940 = LINE ( 'NONE', #102573, #106229 ) ;
#56941 = ORIENTED_EDGE ( 'NONE', *, *, #92410, .T. ) ;
#56942 = CARTESIAN_POINT ( 'NONE',  ( 70.56250000000001421, -5.819803920172572198, -5.819803920172573086 ) ) ;
#56943 = CARTESIAN_POINT ( 'NONE',  ( 8.241399257801971245, 21.72500000000000142, 5.000000000000000000 ) ) ;
#56944 = EDGE_CURVE ( 'NONE', #128780, #12755, #131372, .T. ) ;
#56945 = PLANE ( 'NONE',  #6885 ) ;
#56946 = DIRECTION ( 'NONE',  ( 0.7071067811865487940, 0.7071067811865463515, -0.000000000000000000 ) ) ;
#56948 = ADVANCED_FACE ( 'NONE', ( #93913 ), #116390, .F. ) ;
#56947 = VECTOR ( 'NONE', #87386, 1000.000000000000227 ) ;
#56949 = ORIENTED_EDGE ( 'NONE', *, *, #56233, .T. ) ;
#56950 = LINE ( 'NONE', #93822, #88447 ) ;
#56951 = EDGE_CURVE ( 'NONE', #79346, #63984, #50433, .T. ) ;
#56952 = CARTESIAN_POINT ( 'NONE',  ( 0.000000000000000000, 0.000000000000000000, 5.000000000000000000 ) ) ;
#56953 = CARTESIAN_POINT ( 'NONE',  ( 61.68793019189811844, 6.110000000000002984, -1.637169565754156730 ) ) ;
#56954 = ORIENTED_EDGE ( 'NONE', *, *, #128292, .F. ) ;
#56955 = VERTEX_POINT ( 'NONE', #17082 ) ;
#56956 = CARTESIAN_POINT ( 'NONE',  ( 32.99999999999977263, -10.06887692260770528, 4.000000000000000000 ) ) ;
#56957 = EDGE_CURVE ( 'NONE', #13150, #20021, #106191, .T. ) ;
#56958 = LINE ( 'NONE', #43920, #99929 ) ;
#56959 = CARTESIAN_POINT ( 'NONE',  ( -17.81601139373099940, 28.73617430169775133, 5.000000000000000000 ) ) ;
#56960 = PLANE ( 'NONE',  #120610 ) ;
#56962 = ORIENTED_EDGE ( 'NONE', *, *, #93656, .F. ) ;
#56961 = LINE ( 'NONE', #37328, #121629 ) ;
#56963 =( REPRESENTATION_RELATIONSHIP ('NONE','NONE', #69070, #118114 ) REPRESENTATION_RELATIONSHIP_WITH_TRANSFORMATION ( #142396 )SHAPE_REPRESENTATION_RELATIONSHIP( ) );
#56964 = FACE_OUTER_BOUND ( 'NONE', #105667, .T. ) ;
#56965 = FACE_OUTER_BOUND ( 'NONE', #79845, .T. ) ;
#56966 = LINE ( 'NONE', #99713, #130429 ) ;
#56967 = EDGE_CURVE ( 'NONE', #51992, #111906, #39567, .T. ) ;
#56968 = CARTESIAN_POINT ( 'NONE',  ( -5.510786437626906675, -27.52281430457051314, 5.000000000000000000 ) ) ;
#56969 = EDGE_LOOP ( 'NONE', ( #11653, #108932, #33669, #61847 ) ) ;
#56970 = ORIENTED_EDGE ( 'NONE', *, *, #96054, .F. ) ;
#56971 = CARTESIAN_POINT ( 'NONE',  ( 58.91709685856477563, 3.054999999999998828, 5.291415217122922066 ) ) ;
#56972 = ORIENTED_EDGE ( 'NONE', *, *, #23651, .F. ) ;
#56973 = DIRECTION ( 'NONE',  ( -0.7071067811865486830, -0.7071067811865464625, 0.000000000000000000 ) ) ;
#56974 = DIRECTION ( 'NONE',  ( 1.000000000000000000, 0.000000000000000000, -0.000000000000000000 ) ) ;
#56975 = DIRECTION ( 'NONE',  ( -0.7071067811865486830, -0.7071067811865464625, -0.000000000000000000 ) ) ;
#56976 = ADVANCED_FACE ( 'NONE', ( #128006 ), #31353, .T. ) ;
#56977 = FACE_OUTER_BOUND ( 'NONE', #6995, .T. ) ;
#56978 = DIRECTION ( 'NONE',  ( -0.7071067811865487940, 0.7071067811865463515, -0.000000000000000000 ) ) ;
#56979 = ORIENTED_EDGE ( 'NONE', *, *, #124972, .T. ) ;
#56980 = VERTEX_POINT ( 'NONE', #83051 ) ;
#56981 = PLANE ( 'NONE',  #63160 ) ;
#56982 = DIRECTION ( 'NONE',  ( 0.000000000000000000, 0.000000000000000000, 1.000000000000000000 ) ) ;
#56983 = EDGE_CURVE ( 'NONE', #141725, #68424, #127252, .T. ) ;
#56984 = EDGE_LOOP ( 'NONE', ( #119554, #109748, #106992, #78803 ) ) ;
#56985 = CARTESIAN_POINT ( 'NONE',  ( -21.41161490594815575, 22.22500000000000142, 4.777194822843816802 ) ) ;
#56986 = ADVANCED_FACE ( 'NONE', ( #138152 ), #117082, .T. ) ;
#56987 = DIRECTION ( 'NONE',  ( -0.7071067811865487940, 0.7071067811865463515, -0.000000000000000000 ) ) ;
#56988 = CARTESIAN_POINT ( 'NONE',  ( 14.54487008052911534, -0.7407075233842805861, 4.335043535661647240 ) ) ;
#56989 = ADVANCED_FACE ( 'NONE', ( #27954 ), #73897, .T. ) ;
#56990 = VERTEX_POINT ( 'NONE', #64693 ) ;
#56991 = EDGE_CURVE ( 'NONE', #8350, #140410, #104795, .T. ) ;
#56992 = FACE_BOUND ( 'NONE', #115027, .T. ) ;
#56993 = DIRECTION ( 'NONE',  ( 0.3543493200069162685, -0.000000000000000000, -0.9351131265310288487 ) ) ;
#56994 = CARTESIAN_POINT ( 'NONE',  ( 8.999999999999941380, 16.55218569542900298, 5.000000000000000000 ) ) ;
#56995 = CARTESIAN_POINT ( 'NONE',  ( 37.26669371712955581, -7.949999999999998401, 2.130196079827423983 ) ) ;
#56996 = CARTESIAN_POINT ( 'NONE',  ( 24.39999999999999858, -16.48000000000005016, -34.92499999999998295 ) ) ;
#56997 =( BOUNDED_CURVE ( )  B_SPLINE_CURVE ( 3, ( #51382, #6377, #62260, #94143 ),
 .UNSPECIFIED., .F., .T. ) 
 B_SPLINE_CURVE_WITH_KNOTS ( ( 4, 4 ),
 ( 1.208578181583236821, 1.359146454359418277 ),
 .UNSPECIFIED. ) 
 CURVE ( )  GEOMETRIC_REPRESENTATION_ITEM ( )  RATIONAL_B_SPLINE_CURVE ( ( 1.000000000000000000, 0.9981116584018958626, 0.9981116584018958626, 1.000000000000000000 ) ) 
 REPRESENTATION_ITEM ( '' )  );
#56998 = PLANE ( 'NONE',  #92928 ) ;
#56999 = CARTESIAN_POINT ( 'NONE',  ( 109.3125099229812491, 7.919999999999945750, 19.05499999999803507 ) ) ;
#57001 = ORIENTED_EDGE ( 'NONE', *, *, #122970, .T. ) ;
#57000 = VECTOR ( 'NONE', #66451, 999.9999999999998863 ) ;
#57002 = ORIENTED_EDGE ( 'NONE', *, *, #5869, .F. ) ;
#57003 = CARTESIAN_POINT ( 'NONE',  ( 107.6829301918981088, -1.637169565754158951, -6.109999999999998543 ) ) ;
#57004 = ORIENTED_EDGE ( 'NONE', *, *, #45995, .T. ) ;
#57005 =( GEOMETRIC_REPRESENTATION_CONTEXT ( 3 ) GLOBAL_UNCERTAINTY_ASSIGNED_CONTEXT ( ( #131616 ) ) GLOBAL_UNIT_ASSIGNED_CONTEXT ( ( #85109, #130056, #53946 ) ) REPRESENTATION_CONTEXT ( 'NONE', 'WORKASPACE' ) );
#57006 = EDGE_CURVE ( 'NONE', #129739, #8240, #9557, .T. ) ;
#57007 = CARTESIAN_POINT ( 'NONE',  ( 33.48921356237309510, -27.52281430457078670, 5.000000000000000000 ) ) ;
#57008 = EDGE_LOOP ( 'NONE', ( #86960, #106283, #137383, #80834 ) ) ;
#57009 = DIRECTION ( 'NONE',  ( 0.6830127018922181881, 0.6830127018922202975, -0.2588190451025214056 ) ) ;
#57010 = LINE ( 'NONE', #47575, #89472 ) ;
#57011 = DIRECTION ( 'NONE',  ( 0.000000000000000000, 1.000000000000000000, 0.000000000000000000 ) ) ;
#57012 = ORIENTED_EDGE ( 'NONE', *, *, #140237, .T. ) ;
#57013 = DIRECTION ( 'NONE',  ( 0.000000000000000000, 4.440892098500626162E-15, -1.000000000000000000 ) ) ;
#57014 = PLANE ( 'NONE',  #102809 ) ;
#57015 = EDGE_CURVE ( 'NONE', #81561, #28403, #65429, .T. ) ;
#57016 = LINE ( 'NONE', #111345, #64011 ) ;
#57017 = VECTOR ( 'NONE', #95937, 999.9999999999998863 ) ;
#57018 = CARTESIAN_POINT ( 'NONE',  ( 25.39999999999999858, 7.796566843815467607, 1.475727091950665537 ) ) ;
#57020 = DIRECTION ( 'NONE',  ( -0.000000000000000000, -0.3543493200069152693, 0.9351131265310292928 ) ) ;
#57019 = CARTESIAN_POINT ( 'NONE',  ( 69.10416666666665719, 2.130196079827422206, 7.950000000000001954 ) ) ;
#57021 = CARTESIAN_POINT ( 'NONE',  ( -42.48921356237308800, -27.52281430457085065, 5.000000000000000000 ) ) ;
#57022 = LINE ( 'NONE', #135292, #44516 ) ;
#57023 = ORIENTED_EDGE ( 'NONE', *, *, #107276, .F. ) ;
#57024 = CARTESIAN_POINT ( 'NONE',  ( 87.04166666666665719, -3.975000000000002753, 6.884901960086286188 ) ) ;
#57025 = DIRECTION ( 'NONE',  ( 0.7071067811865487940, 0.7071067811865463515, 0.000000000000000000 ) ) ;
#57026 = ORIENTED_EDGE ( 'NONE', *, *, #76877, .T. ) ;
#57027 = ADVANCED_FACE ( 'NONE', ( #49008 ), #111012, .T. ) ;
#57029 = ORIENTED_EDGE ( 'NONE', *, *, #26656, .T. ) ;
#57028 = VECTOR ( 'NONE', #142700, 1000.000000000000000 ) ;
#57030 = EDGE_LOOP ( 'NONE', ( #112194, #71036, #88673, #76332, #25671 ) ) ;
#57031 = CARTESIAN_POINT ( 'NONE',  ( 50.75043019189810423, 3.055000000000002824, -5.291415217122919401 ) ) ;
#57032 = ORIENTED_EDGE ( 'NONE', *, *, #75403, .F. ) ;
#57033 = VECTOR ( 'NONE', #48200, 1000.000000000000227 ) ;
#57034 = PLANE ( 'NONE',  #83740 ) ;
#57035 = VECTOR ( 'NONE', #121118, 1000.000000000000227 ) ;
#57036 = CARTESIAN_POINT ( 'NONE',  ( 3.983306282870438864, 6.094999999999991758, 1.633150327867687102 ) ) ;
#57037 = CARTESIAN_POINT ( 'NONE',  ( 88.81293019189809002, -1.637169565754159617, -6.110000000000001208 ) ) ;
#57038 = LINE ( 'NONE', #124400, #40513 ) ;
#57039 = ORIENTED_EDGE ( 'NONE', *, *, #139622, .F. ) ;
#57040 = VECTOR ( 'NONE', #105740, 1000.000000000000227 ) ;
#57041 = LINE ( 'NONE', #99053, #133624 ) ;
#57042 = VERTEX_POINT ( 'NONE', #10976 ) ;
#57043 = PLANE ( 'NONE',  #141303 ) ;
#57044 = VECTOR ( 'NONE', #102378, 999.9999999999998863 ) ;
#57045 = LINE ( 'NONE', #136697, #21604 ) ;
#57046 = ORIENTED_EDGE ( 'NONE', *, *, #50073, .F. ) ;
#57047 = EDGE_CURVE ( 'NONE', #105802, #134641, #44392, .T. ) ;
#57048 = DIRECTION ( 'NONE',  ( -0.7071067811865487940, 0.7071067811865463515, -0.000000000000000000 ) ) ;
#57049 = LINE ( 'NONE', #47609, #50824 ) ;
#57050 = CARTESIAN_POINT ( 'NONE',  ( 34.92499999999998295, 22.22500000000000142, 4.500000000000000888 ) ) ;
#57051 = ORIENTED_EDGE ( 'NONE', *, *, #123929, .T. ) ;
#57052 = ADVANCED_FACE ( 'NONE', ( #123373 ), #24738, .F. ) ;
#57053 = FACE_OUTER_BOUND ( 'NONE', #107351, .T. ) ;
#57054 = ORIENTED_EDGE ( 'NONE', *, *, #59601, .F. ) ;
#57055 = VERTEX_POINT ( 'NONE', #11691 ) ;
#57056 = ORIENTED_EDGE ( 'NONE', *, *, #97962, .F. ) ;
#57057 =( NAMED_UNIT ( * ) PLANE_ANGLE_UNIT ( ) SI_UNIT ( $, .RADIAN. ) );
#57058 = DIRECTION ( 'NONE',  ( -0.6830127018922180770, -0.6830127018922204085, -0.2588190451025213501 ) ) ;
#57059 = FACE_OUTER_BOUND ( 'NONE', #64330, .T. ) ;
#57060 = CARTESIAN_POINT ( 'NONE',  ( -26.99999999999981526, 14.87792677143806230, -11.06722581663446192 ) ) ;
#57061 = EDGE_CURVE ( 'NONE', #81042, #104580, #55980, .T. ) ;
#57062 = DIRECTION ( 'NONE',  ( -0.6830127018922180770, -0.6830127018922204085, -0.2588190451025213501 ) ) ;
#57063 = ORIENTED_EDGE ( 'NONE', *, *, #91288, .T. ) ;
#57064 = PLANE ( 'NONE',  #130708 ) ;
#57065 = CARTESIAN_POINT ( 'NONE',  ( 22.87456980810188867, 6.871911579029510442, -3.967499999999998916 ) ) ;
#57066 = CARTESIAN_POINT ( 'NONE',  ( 8.111591955682463606, 2.055000000000001048, 2.516649172247811554E-16 ) ) ;
#57067 = CARTESIAN_POINT ( 'NONE',  ( 28.49999999999980815, 6.052185695429108669, 5.000000000000000000 ) ) ;
#57068 = CARTESIAN_POINT ( 'NONE',  ( 18.17159235450331778, -2.500000000000000000, 3.061616997868384127E-16 ) ) ;
#57069 = EDGE_LOOP ( 'NONE', ( #21703, #62585, #45073, #3900 ) ) ;
#57070 = EDGE_LOOP ( 'NONE', ( #121784, #128114, #76219, #21650 ) ) ;
#57071 = VERTEX_POINT ( 'NONE', #57396 ) ;
#57072 = CARTESIAN_POINT ( 'NONE',  ( -13.49999999999990408, -8.947814304570734123, 5.000000000000000000 ) ) ;
#57073 = CARTESIAN_POINT ( 'NONE',  ( 57.87499999999999289, 7.950000000000000178, 1.460391307983218535E-15 ) ) ;
#57074 = VECTOR ( 'NONE', #51594, 1000.000000000000000 ) ;
#57075 = CARTESIAN_POINT ( 'NONE',  ( 63.18398860626900415, 28.73617430169831621, 5.000000000000000000 ) ) ;
#57076 = CARTESIAN_POINT ( 'NONE',  ( -48.18398860626899705, 28.73617430169820608, 5.000000000000000000 ) ) ;
#57077 = CARTESIAN_POINT ( 'NONE',  ( 9.743626569336168330, 8.447988834747505393, 4.345749975250972064 ) ) ;
#57078 = DIRECTION ( 'NONE',  ( 0.7071067811865487940, -0.7071067811865463515, 0.000000000000000000 ) ) ;
#57079 = CARTESIAN_POINT ( 'NONE',  ( -2.700255128608413990, -27.71228299555204089, 4.000000000000000000 ) ) ;
#57080 = CARTESIAN_POINT ( 'NONE',  ( 2.292893218813447209, -15.74070752338412760, 5.000000000000000000 ) ) ;
#57081 = DIRECTION ( 'NONE',  ( 0.000000000000000000, -1.000000000000000000, 0.000000000000000000 ) ) ;
#57082 = DIRECTION ( 'NONE',  ( -0.000000000000000000, -0.3543493200069152693, 0.9351131265310292928 ) ) ;
#57083 = AXIS2_PLACEMENT_3D ( 'NONE', #68509, #67812, #56920 ) ;
#57084 = EDGE_LOOP ( 'NONE', ( #136513, #65912, #143007, #106254 ) ) ;
#57085 =( LENGTH_UNIT ( ) NAMED_UNIT ( * ) SI_UNIT ( .MILLI., .METRE. ) );
#57086 = ORIENTED_EDGE ( 'NONE', *, *, #7511, .T. ) ;
#57087 = CARTESIAN_POINT ( 'NONE',  ( 0.000000000000000000, 0.000000000000000000, 5.000000000000000000 ) ) ;
#57089 = ORIENTED_EDGE ( 'NONE', *, *, #6836, .F. ) ;
#57088 = DIRECTION ( 'NONE',  ( 0.7071067811865486830, -0.7071067811865464625, -0.000000000000000000 ) ) ;
#57090 = CARTESIAN_POINT ( 'NONE',  ( -11.51078643762690490, -27.52281430457047406, 5.000000000000000000 ) ) ;
#57091 = DIRECTION ( 'NONE',  ( -0.000000000000000000, -0.3543493200069152693, 0.9351131265310292928 ) ) ;
#57092 = EDGE_CURVE ( 'NONE', #40545, #67945, #133517, .T. ) ;
#57093 = VERTEX_POINT ( 'NONE', #134234 ) ;
#57094 = FILL_AREA_STYLE_COLOUR ( '', #64661 ) ;
#57095 = VERTEX_POINT ( 'NONE', #98722 ) ;
#57096 = DIRECTION ( 'NONE',  ( -0.7071067811865486830, -0.7071067811865464625, -0.000000000000000000 ) ) ;
#57097 = ORIENTED_EDGE ( 'NONE', *, *, #1736, .F. ) ;
#57098 = CARTESIAN_POINT ( 'NONE',  ( 0.5685132242927012358, 4.584330080086930965E-16, 0.000000000000000000 ) ) ;
#57099 = CIRCLE ( 'NONE', #114877, 2.337593264352433753 ) ;
#57100 = ADVANCED_FACE ( 'NONE', ( #45115 ), #33514, .F. ) ;
#57102 = EDGE_CURVE ( 'NONE', #123374, #73777, #57776, .T. ) ;
#57101 = CARTESIAN_POINT ( 'NONE',  ( 98.95419371712955581, 6.884901960086283523, 3.975000000000002753 ) ) ;
#57103 = DIRECTION ( 'NONE',  ( -1.000000000000000000, -1.224606353822377258E-16, -0.000000000000000000 ) ) ;
#57104 = CARTESIAN_POINT ( 'NONE',  ( 2.999999999999999112, -1.600000000000086020, -31.92499999999998295 ) ) ;
#57106 = ADVANCED_FACE ( 'NONE', ( #22564 ), #112473, .F. ) ;
#57105 = VERTEX_POINT ( 'NONE', #46551 ) ;
#57107 = VECTOR ( 'NONE', #19336, 1000.000000000000000 ) ;
#57108 =( NAMED_UNIT ( * ) PLANE_ANGLE_UNIT ( ) SI_UNIT ( $, .RADIAN. ) );
#57109 = CYLINDRICAL_SURFACE ( 'NONE', #61171, 2.500000000000000444 ) ;
#57110 = ADVANCED_FACE ( 'NONE', ( #77715 ), #43642, .F. ) ;
#57111 = CARTESIAN_POINT ( 'NONE',  ( -31.49999999999977973, -17.91344420646045776, 1.358650452708392242 ) ) ;
#57112 = CARTESIAN_POINT ( 'NONE',  ( 10.06250000000000178, 4.461849672132300881, 4.461849672132299105 ) ) ;
#57113 = PLANE ( 'NONE',  #37513 ) ;
#57115 = EDGE_CURVE ( 'NONE', #115930, #119665, #87862, .T. ) ;
#57114 = CARTESIAN_POINT ( 'NONE',  ( -5.999999999999963585, -11.35517001088073208, -1.126524801160121214 ) ) ;
#57116 = ORIENTED_EDGE ( 'NONE', *, *, #35087, .F. ) ;
#57117 = ORIENTED_EDGE ( 'NONE', *, *, #142202, .F. ) ;
#57118 = CARTESIAN_POINT ( 'NONE',  ( -25.39999999999996305, 0.000000000000000000, 0.000000000000000000 ) ) ;
#57120 = ORIENTED_EDGE ( 'NONE', *, *, #2904, .F. ) ;
#57119 = ADVANCED_FACE ( 'NONE', ( #56711 ), #68296, .F. ) ;
#57122 = EDGE_CURVE ( 'NONE', #35940, #29609, #132101, .T. ) ;
#57121 = AXIS2_PLACEMENT_3D ( 'NONE', #96865, #75193, #76619 ) ;
#57123 = CARTESIAN_POINT ( 'NONE',  ( 92.45876352523144703, 0.000000000000000000, -6.110000000000001208 ) ) ;
#57124 = LINE ( 'NONE', #11396, #140350 ) ;
#57125 = CARTESIAN_POINT ( 'NONE',  ( 7.171830600776419651, -17.24070752338410273, 4.000000000000000000 ) ) ;
#57126 = DIRECTION ( 'NONE',  ( 0.6830127018922181881, 0.6830127018922202975, -0.2588190451025214056 ) ) ;
#57127 = CARTESIAN_POINT ( 'NONE',  ( 126.9785101690948608, -47.44491123045356318, -36.62621018405940276 ) ) ;
#57128 = ORIENTED_EDGE ( 'NONE', *, *, #5294, .F. ) ;
#57129 = CARTESIAN_POINT ( 'NONE',  ( 48.48921356237309510, -27.52281430457089328, 5.000000000000000000 ) ) ;
#57130 = DIRECTION ( 'NONE',  ( -0.7071067811865486830, -0.7071067811865464625, -0.000000000000000000 ) ) ;
#57131 = ADVANCED_FACE ( 'NONE', ( #88599 ), #53069, .T. ) ;
#57132 = DIRECTION ( 'NONE',  ( 0.6830127018922180770, -0.6830127018922204085, -0.2588190451025213501 ) ) ;
#57133 = VECTOR ( 'NONE', #56281, 1000.000000000000000 ) ;
#57134 = ORIENTED_EDGE ( 'NONE', *, *, #33706, .F. ) ;
#57135 = EDGE_CURVE ( 'NONE', #95889, #102448, #13126, .T. ) ;
#57136 = CARTESIAN_POINT ( 'NONE',  ( 42.48921356237308800, -27.52281430457085065, 5.000000000000000000 ) ) ;
#57137 = DIRECTION ( 'NONE',  ( -0.6830127018922181881, 0.6830127018922202975, -0.2588190451025214056 ) ) ;
#57139 = ORIENTED_EDGE ( 'NONE', *, *, #115124, .F. ) ;
#57138 = LINE ( 'NONE', #137528, #79888 ) ;
#57140 = CARTESIAN_POINT ( 'NONE',  ( 20.99451991528748707, 28.92564299267952777, 4.000000000000000000 ) ) ;
#57141 = LINE ( 'NONE', #4084, #21548 ) ;
#57142 = CARTESIAN_POINT ( 'NONE',  ( 0.000000000000000000, 0.000000000000000000, 5.000000000000000000 ) ) ;
#57143 = ADVANCED_FACE ( 'NONE', ( #23290 ), #53141, .T. ) ;
#57144 = VECTOR ( 'NONE', #113636, 1000.000000000000000 ) ;
#57145 = LINE ( 'NONE', #131103, #49157 ) ;
#57146 = AXIS2_PLACEMENT_3D ( 'NONE', #137372, #91705, #38064 ) ;
#57147 = ORIENTED_EDGE ( 'NONE', *, *, #109828, .F. ) ;
#57148 = VERTEX_POINT ( 'NONE', #71486 ) ;
#57149 = EDGE_LOOP ( 'NONE', ( #28232, #101027, #108979, #11178, #55107 ) ) ;
#57150 = AXIS2_PLACEMENT_3D ( 'NONE', #45893, #88679, #43724 ) ;
#57151 = CARTESIAN_POINT ( 'NONE',  ( 84.00043019189810423, -3.055000000000002380, 5.291415217122920289 ) ) ;
#57152 = VECTOR ( 'NONE', #116433, 1000.000000000000000 ) ;
#57153 = VERTEX_POINT ( 'NONE', #6887 ) ;
#57154 = FACE_OUTER_BOUND ( 'NONE', #68119, .T. ) ;
#57155 = DIRECTION ( 'NONE',  ( -0.7071067811865486830, -0.7071067811865464625, -0.000000000000000000 ) ) ;
#57157 = VECTOR ( 'NONE', #46423, 999.9999999999998863 ) ;
#57156 = DIRECTION ( 'NONE',  ( 1.000000000000000000, 0.000000000000000000, 0.000000000000000000 ) ) ;
#57158 = CARTESIAN_POINT ( 'NONE',  ( 152.4000000000000057, -17.48000000000005016, -33.92499999999998295 ) ) ;
#57159 = ORIENTED_EDGE ( 'NONE', *, *, #109795, .F. ) ;
#57160 = PLANE ( 'NONE',  #106997 ) ;
#57161 = LINE ( 'NONE', #4097, #11939 ) ;
#57162 = CARTESIAN_POINT ( 'NONE',  ( -33.18398860626899705, 28.73617430169810305, 5.000000000000000000 ) ) ;
#57163 = CARTESIAN_POINT ( 'NONE',  ( 90.03709685856478018, -3.054999999999998828, -5.291415217122919401 ) ) ;
#57164 = VERTEX_POINT ( 'NONE', #104814 ) ;
#57165 = FACE_OUTER_BOUND ( 'NONE', #92063, .T. ) ;
#57166 = ADVANCED_FACE ( 'NONE', ( #5478 ), #49757, .T. ) ;
#57167 = PLANE ( 'NONE',  #40099 ) ;
#57168 = ORIENTED_EDGE ( 'NONE', *, *, #80802, .F. ) ;
#57169 = VERTEX_POINT ( 'NONE', #106213 ) ;
#57170 = DIRECTION ( 'NONE',  ( -0.7071067811865486830, 0.7071067811865464625, 0.000000000000000000 ) ) ;
#57171 = CARTESIAN_POINT ( 'NONE',  ( 23.83790314143521982, -6.871911579029513106, -3.967499999999993587 ) ) ;
#57172 = CARTESIAN_POINT ( 'NONE',  ( 25.40000000000000568, -6.088644610809077484, -0.2782657062331916342 ) ) ;
#57173 = FACE_OUTER_BOUND ( 'NONE', #64809, .T. ) ;
#57174 = ADVANCED_FACE ( 'NONE', ( #51165 ), #117798, .F. ) ;
#57175 = CARTESIAN_POINT ( 'NONE',  ( -19.08335816409769237, -22.22500000000000142, -1.002990283292573004 ) ) ;
#57176 = CARTESIAN_POINT ( 'NONE',  ( 0.000000000000000000, 0.9892420537897061994, -14.41609864557725729 ) ) ;
#57177 =( LENGTH_UNIT ( ) NAMED_UNIT ( * ) SI_UNIT ( .MILLI., .METRE. ) );
#57178 = VERTEX_POINT ( 'NONE', #99638 ) ;
#57179 = VERTEX_POINT ( 'NONE', #66337 ) ;
#57180 = CARTESIAN_POINT ( 'NONE',  ( -36.18398860626899705, 28.73617430169812437, 5.000000000000000000 ) ) ;
#57182 = EDGE_LOOP ( 'NONE', ( #31554, #89759, #33642, #124316 ) ) ;
#57181 = ADVANCED_FACE ( 'NONE', ( #33713 ), #131578, .T. ) ;
#57183 = ORIENTED_EDGE ( 'NONE', *, *, #20812, .T. ) ;
#57184 = AXIS2_PLACEMENT_3D ( 'NONE', #98640, #32702, #131280 ) ;
#57185 = FACE_OUTER_BOUND ( 'NONE', #140225, .T. ) ;
#57186 = ORIENTED_EDGE ( 'NONE', *, *, #105646, .F. ) ;
#57187 = LINE ( 'NONE', #2003, #89968 ) ;
#57188 = DIRECTION ( 'NONE',  ( 0.000000000000000000, 0.000000000000000000, 1.000000000000000000 ) ) ;
#57189 = EDGE_CURVE ( 'NONE', #5220, #66103, #31551, .T. ) ;
#57190 = AXIS2_PLACEMENT_3D ( 'NONE', #6563, #138567, #81353 ) ;
#57191 = DIRECTION ( 'NONE',  ( -1.000000000000000000, -0.000000000000000000, -0.000000000000000000 ) ) ;
#57192 = CARTESIAN_POINT ( 'NONE',  ( 8.816011393731004731, 28.73617430169781173, 5.000000000000000000 ) ) ;
#57193 = VERTEX_POINT ( 'NONE', #64903 ) ;
#57194 = LINE ( 'NONE', #68085, #85827 ) ;
#57196 = VERTEX_POINT ( 'NONE', #33012 ) ;
#57195 = VECTOR ( 'NONE', #31137, 1000.000000000000000 ) ;
#57198 = EDGE_CURVE ( 'NONE', #4623, #123033, #76500, .T. ) ;
#57197 = DIRECTION ( 'NONE',  ( 0.000000000000000000, 0.000000000000000000, 1.000000000000000000 ) ) ;
#57199 = ORIENTED_EDGE ( 'NONE', *, *, #101886, .T. ) ;
#57200 = VERTEX_POINT ( 'NONE', #75081 ) ;
#57201 = CARTESIAN_POINT ( 'NONE',  ( 9.299744871391588674, -27.71228299555212971, 4.000000000000000000 ) ) ;
#57202 = EDGE_LOOP ( 'NONE', ( #107623, #132863, #75220, #9608 ) ) ;
#57203 = ORIENTED_EDGE ( 'NONE', *, *, #116994, .T. ) ;
#57204 = ORIENTED_EDGE ( 'NONE', *, *, #119757, .T. ) ;
#57205 = VECTOR ( 'NONE', #141513, 999.9999999999998863 ) ;
#57206 = CARTESIAN_POINT ( 'NONE',  ( 30.48921356237309510, -27.52281430457076894, 5.000000000000000000 ) ) ;
#57207 = LINE ( 'NONE', #57924, #122409 ) ;
#57208 = CARTESIAN_POINT ( 'NONE',  ( -42.29974487139158157, -27.71228299555235708, 4.000000000000000000 ) ) ;
#57209 = VECTOR ( 'NONE', #56993, 1000.000000000000227 ) ;
#57210 = CARTESIAN_POINT ( 'NONE',  ( 113.7504301918981042, 3.055000000000002824, -5.291415217122919401 ) ) ;
#57211 = DIRECTION ( 'NONE',  ( 0.7071067811865487940, -0.7071067811865463515, 0.000000000000000000 ) ) ;
#57212 = DIRECTION ( 'NONE',  ( 0.7071067811865487940, -0.7071067811865463515, 0.000000000000000000 ) ) ;
#57213 = CARTESIAN_POINT ( 'NONE',  ( -34.92460739249806068, 21.74787736706806029, 4.224371856075229026 ) ) ;
#57214 = CARTESIAN_POINT ( 'NONE',  ( 0.000000000000000000, 0.000000000000000000, 5.000000000000000000 ) ) ;
#57215 = DIRECTION ( 'NONE',  ( -0.000000000000000000, 0.000000000000000000, 1.000000000000000000 ) ) ;
#57216 = VERTEX_POINT ( 'NONE', #77917 ) ;
#57217 = EDGE_CURVE ( 'NONE', #70779, #137008, #2139, .T. ) ;
#57218 = CARTESIAN_POINT ( 'NONE',  ( 16.49999999999988276, -6.839392718269117211, -8.480912228396125130 ) ) ;
#57219 = FACE_OUTER_BOUND ( 'NONE', #92236, .T. ) ;
#57220 = ORIENTED_EDGE ( 'NONE', *, *, #119927, .F. ) ;
#57221 = EDGE_LOOP ( 'NONE', ( #95398, #130154, #1094, #17392 ) ) ;
#57222 = LINE ( 'NONE', #46356, #10121 ) ;
#57223 = ORIENTED_EDGE ( 'NONE', *, *, #30376, .T. ) ;
#57224 = CYLINDRICAL_SURFACE ( 'NONE', #104698, 0.5000000000000004441 ) ;
#57225 = DIRECTION ( 'NONE',  ( -0.7071067811865486830, -0.7071067811865464625, 0.000000000000000000 ) ) ;
#57226 = CIRCLE ( 'NONE', #126611, 5.968999999999998529 ) ;
#57227 = DIRECTION ( 'NONE',  ( -0.000000000000000000, 0.000000000000000000, 1.000000000000000000 ) ) ;
#57228 = EDGE_CURVE ( 'NONE', #52039, #18836, #21390, .T. ) ;
#57229 = DIRECTION ( 'NONE',  ( -0.7071067811865486830, -0.7071067811865464625, -0.000000000000000000 ) ) ;
#57230 = ORIENTED_EDGE ( 'NONE', *, *, #141716, .F. ) ;
#57231 = LINE ( 'NONE', #54379, #134363 ) ;
#57232 = ORIENTED_EDGE ( 'NONE', *, *, #58807, .T. ) ;
#57233 = VECTOR ( 'NONE', #57523, 1000.000000000000000 ) ;
#57236 = PLANE ( 'NONE',  #9748 ) ;
#57235 = VECTOR ( 'NONE', #35776, 1000.000000000000000 ) ;
#57234 = PRODUCT_RELATED_PRODUCT_CATEGORY ( 'part', '', ( #54028 ) ) ;
#57237 = AXIS2_PLACEMENT_3D ( 'NONE', #84242, #107379, #41407 ) ;
#57238 = CARTESIAN_POINT ( 'NONE',  ( 18.44206980810188767, 7.934999999999993392, 2.126176841940951689 ) ) ;
#57239 = EDGE_LOOP ( 'NONE', ( #69702, #93205, #56674, #6163 ) ) ;
#57240 = CARTESIAN_POINT ( 'NONE',  ( 80.26626352523145158, 4.472830434245839371, -4.472830434245839371 ) ) ;
#57241 = DIRECTION ( 'NONE',  ( -0.6830127018922180770, 0.6830127018922202975, -0.2588190451025213501 ) ) ;
#57242 = FACE_OUTER_BOUND ( 'NONE', #139939, .T. ) ;
#57243 = ORIENTED_EDGE ( 'NONE', *, *, #52351, .F. ) ;
#57244 = VECTOR ( 'NONE', #25175, 999.9999999999998863 ) ;
#57245 = ORIENTED_EDGE ( 'NONE', *, *, #104797, .T. ) ;
#57246 = VERTEX_POINT ( 'NONE', #98923 ) ;
#57247 = LINE ( 'NONE', #69544, #12521 ) ;
#57248 = CARTESIAN_POINT ( 'NONE',  ( 8.585466709768445170, 3.821174125832445049E-16, 0.000000000000000000 ) ) ;
#57249 = VECTOR ( 'NONE', #129861, 1000.000000000000000 ) ;
#57250 = CARTESIAN_POINT ( 'NONE',  ( 6.299744871391586898, -27.71228299555210484, 4.000000000000000000 ) ) ;
#57251 = LINE ( 'NONE', #677, #88982 ) ;
#57252 = EDGE_CURVE ( 'NONE', #31140, #25493, #39236, .T. ) ;
#57253 = EDGE_LOOP ( 'NONE', ( #27076, #20738, #106578, #55900 ) ) ;
#57254 = CARTESIAN_POINT ( 'NONE',  ( 48.18398860626899705, 28.73617430169820608, 5.000000000000000000 ) ) ;
#57255 = SURFACE_STYLE_FILL_AREA ( #12978 ) ;
#57256 = CARTESIAN_POINT ( 'NONE',  ( 3.710381658649933634, 4.584330080086930965E-16, 0.000000000000000000 ) ) ;
#57257 = ORIENTED_EDGE ( 'NONE', *, *, #27205, .T. ) ;
#57258 = LINE ( 'NONE', #67417, #135011 ) ;
#57259 = ORIENTED_EDGE ( 'NONE', *, *, #36955, .T. ) ;
#57260 =( BOUNDED_CURVE ( )  B_SPLINE_CURVE ( 3, ( #17149, #15666, #136773, #97344 ),
 .UNSPECIFIED., .F., .F. ) 
 B_SPLINE_CURVE_WITH_KNOTS ( ( 4, 4 ),
 ( 6.095931195673057523, 6.243513561394028244 ),
 .UNSPECIFIED. ) 
 CURVE ( )  GEOMETRIC_REPRESENTATION_ITEM ( )  RATIONAL_B_SPLINE_CURVE ( ( 1.000000000000000000, 0.9981857772260753769, 0.9981857772260753769, 1.000000000000000000 ) ) 
 REPRESENTATION_ITEM ( '' )  );
#57262 = ORIENTED_EDGE ( 'NONE', *, *, #28072, .T. ) ;
#57261 = CARTESIAN_POINT ( 'NONE',  ( 57.90314192168424512, -45.52550609311789032, -35.40428284070723208 ) ) ;
#57263 = VERTEX_POINT ( 'NONE', #122106 ) ;
#57264 = LINE ( 'NONE', #88456, #23907 ) ;
#57266 = VECTOR ( 'NONE', #46162, 1000.000000000000000 ) ;
#57265 = CARTESIAN_POINT ( 'NONE',  ( 0.000000000000000000, 0.000000000000000000, 5.000000000000000000 ) ) ;
#57267 = ORIENTED_EDGE ( 'NONE', *, *, #38259, .F. ) ;
#57268 = SURFACE_STYLE_USAGE ( .BOTH. , #2092 ) ;
#57269 = ORIENTED_EDGE ( 'NONE', *, *, #98575, .F. ) ;
#57270 = DIRECTION ( 'NONE',  ( -0.000000000000000000, -0.3543493200069152693, 0.9351131265310292928 ) ) ;
#57271 = LINE ( 'NONE', #35530, #131862 ) ;
#57272 = EDGE_CURVE ( 'NONE', #108649, #124601, #310, .T. ) ;
#57273 = VECTOR ( 'NONE', #16862, 1000.000000000000000 ) ;
#57274 = DIRECTION ( 'NONE',  ( -0.6830127018922180770, -0.6830127018922204085, -0.2588190451025213501 ) ) ;
#57275 = CARTESIAN_POINT ( 'NONE',  ( 152.4000000000000057, -17.48000000000005016, 12.69999999999954632 ) ) ;
#57276 = EDGE_CURVE ( 'NONE', #135430, #15191, #13741, .T. ) ;
#57277 = DIRECTION ( 'NONE',  ( 0.3543493200069162685, -0.000000000000000000, -0.9351131265310288487 ) ) ;
#57278 = CARTESIAN_POINT ( 'NONE',  ( -18.18398860626898994, 28.73617430169800002, 5.000000000000000000 ) ) ;
#57279 = CARTESIAN_POINT ( 'NONE',  ( 9.183988606268997046, 28.73617430169793607, 5.000000000000000000 ) ) ;
#57280 = EDGE_CURVE ( 'NONE', #99958, #96272, #108343, .T. ) ;
#57281 = DIRECTION ( 'NONE',  ( -2.496005001405472275E-15, -1.000000000000000000, 0.000000000000000000 ) ) ;
#57282 = CARTESIAN_POINT ( 'NONE',  ( 18.49956980810188867, -3.967499999999998028, -6.871911579029511330 ) ) ;
#57284 = VECTOR ( 'NONE', #130239, 1000.000000000000000 ) ;
#57283 = LINE ( 'NONE', #36225, #44458 ) ;
#57285 = CARTESIAN_POINT ( 'NONE',  ( 19.49999999999986144, -14.56887692260766443, 4.000000000000000000 ) ) ;
#57286 = PLANE ( 'NONE',  #32816 ) ;
#57288 = EDGE_CURVE ( 'NONE', #88886, #84730, #119246, .T. ) ;
#57287 = LINE ( 'NONE', #79044, #57157 ) ;
#57289 = ORIENTED_EDGE ( 'NONE', *, *, #37249, .F. ) ;
#57290 = ORIENTED_EDGE ( 'NONE', *, *, #24659, .T. ) ;
#57291 = CARTESIAN_POINT ( 'NONE',  ( 91.41666666666667140, -6.884901960086287076, -3.975000000000000977 ) ) ;
#57292 = ORIENTED_EDGE ( 'NONE', *, *, #14729, .T. ) ;
#57293 = ORIENTED_EDGE ( 'NONE', *, *, #131975, .F. ) ;
#57294 = ORIENTED_EDGE ( 'NONE', *, *, #94737, .T. ) ;
#57295 = VECTOR ( 'NONE', #115886, 1000.000000000000000 ) ;
#57296 = DIRECTION ( 'NONE',  ( 0.7071067811865487940, 0.7071067811865463515, -0.000000000000000000 ) ) ;
#57297 = CARTESIAN_POINT ( 'NONE',  ( 88.64583333333334281, 2.130196079827394229, -7.950000000000021494 ) ) ;
#57298 = CARTESIAN_POINT ( 'NONE',  ( 10.90756199573120000, 8.448038036319919897, -4.345660073319586481 ) ) ;
#57299 = ORIENTED_EDGE ( 'NONE', *, *, #102468, .T. ) ;
#57300 = DIRECTION ( 'NONE',  ( -0.000000000000000000, 0.3543493200069153248, 0.9351131265310292928 ) ) ;
#57301 = CARTESIAN_POINT ( 'NONE',  ( 3.250000000000000000, -4.999999999999999112, -7.627214432543508948 ) ) ;
#57302 = EDGE_CURVE ( 'NONE', #110142, #126713, #11173, .T. ) ;
#57303 = PLANE ( 'NONE',  #139053 ) ;
#57304 = DIRECTION ( 'NONE',  ( 0.6830127018922181881, 0.6830127018922202975, -0.2588190451025214056 ) ) ;
#57305 = ADVANCED_FACE ( 'NONE', ( #100383 ), #65651, .F. ) ;
#57306 = CARTESIAN_POINT ( 'NONE',  ( 128.3912635252314374, -4.472830434245838482, -4.472830434245838482 ) ) ;
#57307 = LINE ( 'NONE', #86529, #2990 ) ;
#57308 = LINE ( 'NONE', #99321, #61276 ) ;
#57309 = DIRECTION ( 'NONE',  ( -0.7071067811865486830, -0.7071067811865464625, -0.000000000000000000 ) ) ;
#57310 = CARTESIAN_POINT ( 'NONE',  ( 34.42499999999998295, 22.22500000000000142, 5.000000000000000000 ) ) ;
#57311 = FACE_OUTER_BOUND ( 'NONE', #113621, .T. ) ;
#57312 = CYLINDRICAL_SURFACE ( 'NONE', #128621, 2.500000000000000444 ) ;
#57313 = EDGE_CURVE ( 'NONE', #16774, #55512, #111221, .T. ) ;
#57314 = CARTESIAN_POINT ( 'NONE',  ( -14.99999999999989164, -13.06887692260767686, 4.000000000000000000 ) ) ;
#57315 = VERTEX_POINT ( 'NONE', #9780 ) ;
#57316 = VERTEX_POINT ( 'NONE', #109817 ) ;
#57317 = CARTESIAN_POINT ( 'NONE',  ( 121.9170968585647756, 3.054999999999998828, 5.291415217122922066 ) ) ;
#57318 = VERTEX_POINT ( 'NONE', #22762 ) ;
#57319 = LINE ( 'NONE', #66745, #110307 ) ;
#57320 = ADVANCED_FACE ( 'NONE', ( #88803 ), #11915, .F. ) ;
#57321 = FACE_OUTER_BOUND ( 'NONE', #86801, .T. ) ;
#57322 = LINE ( 'NONE', #2896, #25764 ) ;
#57323 = DIRECTION ( 'NONE',  ( -1.000000000000000000, -0.000000000000000000, -0.000000000000000000 ) ) ;
#57324 = CARTESIAN_POINT ( 'NONE',  ( 111.7662635252314516, 4.472830434245839371, -4.472830434245838482 ) ) ;
#57325 = ORIENTED_EDGE ( 'NONE', *, *, #59479, .T. ) ;
#57326 = ORIENTED_EDGE ( 'NONE', *, *, #75299, .F. ) ;
#57327 = ADVANCED_FACE ( 'NONE', ( #56201 ), #89489, .T. ) ;
#57328 = CARTESIAN_POINT ( 'NONE',  ( 51.18398860626899705, 28.73617430169823095, 5.000000000000000000 ) ) ;
#57329 = VECTOR ( 'NONE', #3484, 1000.000000000000000 ) ;
#57330 = ORIENTED_EDGE ( 'NONE', *, *, #34211, .T. ) ;
#57331 = ORIENTED_EDGE ( 'NONE', *, *, #33113, .F. ) ;
#57332 = VECTOR ( 'NONE', #24332, 1000.000000000000000 ) ;
#57333 = ORIENTED_EDGE ( 'NONE', *, *, #55455, .T. ) ;
#57334 = DIRECTION ( 'NONE',  ( -0.000000000000000000, 0.000000000000000000, 1.000000000000000000 ) ) ;
#57335 = CARTESIAN_POINT ( 'NONE',  ( 1.671236474768553082, 0.000000000000000000, 7.934999999999990727 ) ) ;
#57336 = CIRCLE ( 'NONE', #138333, 2.500000000000000888 ) ;
#57337 = AXIS2_PLACEMENT_3D ( 'NONE', #90490, #35433, #24509 ) ;
#57338 = EDGE_CURVE ( 'NONE', #57318, #127365, #134443, .T. ) ;
#57339 = VECTOR ( 'NONE', #72492, 1000.000000000000227 ) ;
#57340 = LINE ( 'NONE', #2166, #19921 ) ;
#57341 = VERTEX_POINT ( 'NONE', #25656 ) ;
#57342 = ORIENTED_EDGE ( 'NONE', *, *, #86334, .F. ) ;
#57343 = DIRECTION ( 'NONE',  ( -0.7071067811865487940, 0.7071067811865463515, 0.000000000000000000 ) ) ;
#57344 = ORIENTED_EDGE ( 'NONE', *, *, #51805, .T. ) ;
#57345 = VERTEX_POINT ( 'NONE', #69931 ) ;
#57346 = VECTOR ( 'NONE', #33095, 1000.000000000000000 ) ;
#57347 = ORIENTED_EDGE ( 'NONE', *, *, #51805, .F. ) ;
#57348 = FACE_OUTER_BOUND ( 'NONE', #107644, .T. ) ;
#57349 = CARTESIAN_POINT ( 'NONE',  ( -19.05499999999999261, 3.130000000000007887, -22.35000000000000142 ) ) ;
#57350 = CARTESIAN_POINT ( 'NONE',  ( -11.99999999999990052, -19.44781430457063465, 5.000000000000000000 ) ) ;
#57351 = ORIENTED_EDGE ( 'NONE', *, *, #135630, .T. ) ;
#57352 = FACE_OUTER_BOUND ( 'NONE', #20250, .T. ) ;
#57353 = EDGE_CURVE ( 'NONE', #44653, #79735, #136551, .T. ) ;
#57354 = DIRECTION ( 'NONE',  ( 0.7071067811865487940, 0.7071067811865463515, 0.000000000000000000 ) ) ;
#57355 = DIRECTION ( 'NONE',  ( 0.7071067811865487940, 0.7071067811865463515, 0.000000000000000000 ) ) ;
#57356 = FACE_BOUND ( 'NONE', #113143, .T. ) ;
#57357 = ORIENTED_EDGE ( 'NONE', *, *, #108238, .F. ) ;
#57358 = CARTESIAN_POINT ( 'NONE',  ( -27.85181644961838288, 17.25929247661554200, 8.802941693769138709 ) ) ;
#57360 = EDGE_CURVE ( 'NONE', #48401, #14592, #90200, .T. ) ;
#57359 = LINE ( 'NONE', #46510, #69306 ) ;
#57361 = CARTESIAN_POINT ( 'NONE',  ( 6.628407645496676714, 9.139736423841732040E-16, 0.000000000000000000 ) ) ;
#57362 = DIRECTION ( 'NONE',  ( -0.7071067811865486830, -0.7071067811865464625, 0.000000000000000000 ) ) ;
#57363 = EDGE_LOOP ( 'NONE', ( #143355, #24529, #140760, #77107 ) ) ;
#57364 = CARTESIAN_POINT ( 'NONE',  ( -17.11087965568911073, 8.820243421702873121, 4.000000000000000000 ) ) ;
#57365 = EDGE_LOOP ( 'NONE', ( #89779, #109886, #32070, #44470, #101772 ) ) ;
#57366 = VECTOR ( 'NONE', #59033, 1000.000000000000114 ) ;
#57367 = ORIENTED_EDGE ( 'NONE', *, *, #137972, .F. ) ;
#57368 = ORIENTED_EDGE ( 'NONE', *, *, #28249, .T. ) ;
#57369 = CARTESIAN_POINT ( 'NONE',  ( 45.99543019189810877, 5.291415217122916737, 3.055000000000001936 ) ) ;
#57370 = EDGE_LOOP ( 'NONE', ( #63568, #79404, #122813 ) ) ;
#57371 = DIRECTION ( 'NONE',  ( 0.000000000000000000, -1.000000000000000000, 0.000000000000000000 ) ) ;
#57372 = DIRECTION ( 'NONE',  ( -0.3543493200069162685, -0.000000000000000000, -0.9351131265310288487 ) ) ;
#57373 = EDGE_CURVE ( 'NONE', #30354, #24532, #12633, .T. ) ;
#57374 = ORIENTED_EDGE ( 'NONE', *, *, #46889, .T. ) ;
#57375 = DIRECTION ( 'NONE',  ( -0.3543493200069162685, -0.000000000000000000, -0.9351131265310288487 ) ) ;
#57376 = CARTESIAN_POINT ( 'NONE',  ( -33.32816939922329880, 11.25929247661560062, 4.000000000000000000 ) ) ;
#57377 = CARTESIAN_POINT ( 'NONE',  ( 3.489213562373097322, -27.52281430457057709, 5.000000000000000000 ) ) ;
#57378 = EDGE_CURVE ( 'NONE', #942, #90062, #52304, .T. ) ;
#57379 = PRESENTATION_STYLE_ASSIGNMENT (( #125477 ) ) ;
#57380 = DIRECTION ( 'NONE',  ( 0.000000000000000000, -1.000000000000000000, 0.000000000000000000 ) ) ;
#57381 = ORIENTED_EDGE ( 'NONE', *, *, #108237, .T. ) ;
#57382 = ORIENTED_EDGE ( 'NONE', *, *, #18248, .F. ) ;
#57383 = VERTEX_POINT ( 'NONE', #103212 ) ;
#57384 = EDGE_LOOP ( 'NONE', ( #114896, #33522, #114009, #1484 ) ) ;
#57385 = CARTESIAN_POINT ( 'NONE',  ( 2.994519915287485734, 28.92564299267940342, 4.000000000000000000 ) ) ;
#57386 = ORIENTED_EDGE ( 'NONE', *, *, #86125, .T. ) ;
#57387 = VERTEX_POINT ( 'NONE', #101071 ) ;
#57388 = CARTESIAN_POINT ( 'NONE',  ( -34.92500000000001137, -22.22500000000000142, 4.500000000000000888 ) ) ;
#57389 = EDGE_CURVE ( 'NONE', #54369, #128989, #3864, .T. ) ;
#57390 = ADVANCED_FACE ( 'NONE', ( #125712 ), #26393, .F. ) ;
#57391 = PLANE ( 'NONE',  #55542 ) ;
#57392 = ORIENTED_EDGE ( 'NONE', *, *, #95935, .T. ) ;
#57393 = CARTESIAN_POINT ( 'NONE',  ( 51.18398860626899705, 28.73617430169823095, 5.000000000000000000 ) ) ;
#57394 = CARTESIAN_POINT ( 'NONE',  ( 0.000000000000000000, 0.3999999999999995781, 2.015694669338588429 ) ) ;
#57395 = CARTESIAN_POINT ( 'NONE',  ( 29.67123647476855552, 0.000000000000000000, 7.934999999999990727 ) ) ;
#57396 = CARTESIAN_POINT ( 'NONE',  ( -22.49999999999984013, -4.912538124160710673, 4.000000000000000000 ) ) ;
#57397 = EDGE_LOOP ( 'NONE', ( #51384, #38876, #110628, #127791 ) ) ;
#57399 = DIRECTION ( 'NONE',  ( 0.7071067811865487940, 0.7071067811865463515, 0.000000000000000000 ) ) ;
#57398 = CARTESIAN_POINT ( 'NONE',  ( 114.6829301918980946, -1.637169565754159173, -6.109999999999999432 ) ) ;
#57400 = AXIS2_PLACEMENT_3D ( 'NONE', #106895, #130834, #74297 ) ;
#57401 = CARTESIAN_POINT ( 'NONE',  ( 22.49999999999983658, -14.94781430457066840, 5.000000000000000000 ) ) ;
#57402 = DIRECTION ( 'NONE',  ( 0.7071067811865487940, 0.7071067811865463515, -0.000000000000000000 ) ) ;
#57403 = ORIENTED_EDGE ( 'NONE', *, *, #143285, .F. ) ;
#57404 = DIRECTION ( 'NONE',  ( 0.7071067811865487940, -0.7071067811865463515, 0.000000000000000000 ) ) ;
#57406 = ORIENTED_EDGE ( 'NONE', *, *, #54129, .T. ) ;
#57405 = DIRECTION ( 'NONE',  ( -1.000000000000000000, 0.000000000000000000, -0.000000000000000000 ) ) ;
#57407 = CARTESIAN_POINT ( 'NONE',  ( 2.999999999999978240, -10.06887692260771416, 4.000000000000000000 ) ) ;
#57408 = EDGE_LOOP ( 'NONE', ( #135337, #136496, #81121 ) ) ;
#57409 = CARTESIAN_POINT ( 'NONE',  ( 63.18398860626900415, 28.73617430169831621, 5.000000000000000000 ) ) ;
#57410 = CARTESIAN_POINT ( 'NONE',  ( 17.01299345043647193, -0.9444868035624204294, -36.39086428169088094 ) ) ;
#57411 = DIRECTION ( 'NONE',  ( -0.7071067811865487940, 0.7071067811865463515, -0.000000000000000000 ) ) ;
#57412 = FACE_OUTER_BOUND ( 'NONE', #106712, .T. ) ;
#57413 = EDGE_CURVE ( 'NONE', #7339, #136825, #13338, .T. ) ;
#57414 = VERTEX_POINT ( 'NONE', #112671 ) ;
#57415 = DIRECTION ( 'NONE',  ( 0.3543493200069163240, -0.000000000000000000, 0.9351131265310288487 ) ) ;
#57416 = VECTOR ( 'NONE', #111081, 1000.000000000000000 ) ;
#57417 = LINE ( 'NONE', #87879, #78935 ) ;
#57418 = CARTESIAN_POINT ( 'NONE',  ( 69.48921356237309510, -27.52281430457103895, 5.000000000000000000 ) ) ;
#57419 = ORIENTED_EDGE ( 'NONE', *, *, #80195, .T. ) ;
#57420 = VECTOR ( 'NONE', #133705, 1000.000000000000000 ) ;
#57421 = DIRECTION ( 'NONE',  ( 0.7071067811865486830, -0.7071067811865464625, -0.000000000000000000 ) ) ;
#57422 = ORIENTED_EDGE ( 'NONE', *, *, #137776, .T. ) ;
#57423 = VECTOR ( 'NONE', #138822, 1000.000000000000227 ) ;
#57424 = LINE ( 'NONE', #66156, #141053 ) ;
#57426 = ORIENTED_EDGE ( 'NONE', *, *, #36689, .T. ) ;
#57425 = LINE ( 'NONE', #13863, #34852 ) ;
#57427 = ORIENTED_EDGE ( 'NONE', *, *, #47299, .F. ) ;
#57428 = CARTESIAN_POINT ( 'NONE',  ( 16.83830262477991369, 5.618291726703525057, -29.10193646598569472 ) ) ;
#57429 = CARTESIAN_POINT ( 'NONE',  ( -0.2997448713915885632, -27.71228299555206220, 4.000000000000000000 ) ) ;
#57430 = VECTOR ( 'NONE', #5959, 1000.000000000000000 ) ;
#57431 = EDGE_LOOP ( 'NONE', ( #6411, #56355, #73397, #125142 ) ) ;
#57432 = AXIS2_PLACEMENT_3D ( 'NONE', #32011, #79127, #66789 ) ;
#57433 =( BOUNDED_CURVE ( )  B_SPLINE_CURVE ( 3, ( #103247, #15495, #14090, #93101 ),
 .UNSPECIFIED., .F., .T. ) 
 B_SPLINE_CURVE_WITH_KNOTS ( ( 4, 4 ),
 ( 4.350170835173026163, 4.500739107949204509 ),
 .UNSPECIFIED. ) 
 CURVE ( )  GEOMETRIC_REPRESENTATION_ITEM ( )  RATIONAL_B_SPLINE_CURVE ( ( 1.000000000000000000, 0.9981116584018959736, 0.9981116584018959736, 1.000000000000000000 ) ) 
 REPRESENTATION_ITEM ( '' )  );
#57434 = LINE ( 'NONE', #857, #62205 ) ;
#57435 = EDGE_CURVE ( 'NONE', #91556, #111517, #15459, .T. ) ;
#57436 =( LENGTH_UNIT ( ) NAMED_UNIT ( * ) SI_UNIT ( .MILLI., .METRE. ) );
#57437 = ORIENTED_EDGE ( 'NONE', *, *, #74104, .F. ) ;
#57438 = EDGE_CURVE ( 'NONE', #25811, #45676, #59747, .T. ) ;
#57439 = PLANE ( 'NONE',  #53608 ) ;
#57440 = CARTESIAN_POINT ( 'NONE',  ( -5.004924772211909456, -5.240707523384228850, 12.38332538355497192 ) ) ;
#57441 = LINE ( 'NONE', #55290, #104892 ) ;
#57442 = CARTESIAN_POINT ( 'NONE',  ( -8.999999999999934275, -11.35517001088073208, -1.126524801160128986 ) ) ;
#57443 = CARTESIAN_POINT ( 'NONE',  ( 19.93618820137057668, -0.2699999999999959099, -36.39086428169088094 ) ) ;
#57444 = PLANE ( 'NONE',  #58198 ) ;
#57445 = ADVANCED_FACE ( 'NONE', ( #122839 ), #23515, .T. ) ;
#57447 = EDGE_CURVE ( 'NONE', #15104, #34146, #117068, .T. ) ;
#57446 = ORIENTED_EDGE ( 'NONE', *, *, #62982, .F. ) ;
#57448 = ORIENTED_EDGE ( 'NONE', *, *, #13248, .F. ) ;
#57449 = EDGE_LOOP ( 'NONE', ( #55733, #80428, #83381, #10467 ) ) ;
#57450 = CARTESIAN_POINT ( 'NONE',  ( 23.99999999999983302, 12.25461709320622639, -10.07315571508691754 ) ) ;
#57451 = VERTEX_POINT ( 'NONE', #69186 ) ;
#57452 = ORIENTED_EDGE ( 'NONE', *, *, #136770, .F. ) ;
#57453 = ORIENTED_EDGE ( 'NONE', *, *, #93635, .F. ) ;
#57454 = CARTESIAN_POINT ( 'NONE',  ( -17.99999999999986855, 7.007997736742429318, -8.085015511992153847 ) ) ;
#57455 = FACE_OUTER_BOUND ( 'NONE', #44532, .T. ) ;
#57456 = ORIENTED_EDGE ( 'NONE', *, *, #18148, .T. ) ;
#57457 = DIRECTION ( 'NONE',  ( 0.3543493200069162685, -0.000000000000000000, -0.9351131265310288487 ) ) ;
#57459 = VECTOR ( 'NONE', #137441, 1000.000000000000000 ) ;
#57458 = PLANE ( 'NONE',  #90619 ) ;
#57460 = CARTESIAN_POINT ( 'NONE',  ( 39.18398860626899705, 28.73617430169814568, 5.000000000000000000 ) ) ;
#57461 = EDGE_CURVE ( 'NONE', #142771, #138853, #3186, .T. ) ;
#57462 = CARTESIAN_POINT ( 'NONE',  ( -7.828169399223472880, -2.240707523384257716, 4.000000000000000000 ) ) ;
#57463 = CARTESIAN_POINT ( 'NONE',  ( 123.3754301918981184, -5.291415217122920289, -3.055000000000001492 ) ) ;
#57464 = ORIENTED_EDGE ( 'NONE', *, *, #12357, .F. ) ;
#57465 = EDGE_CURVE ( 'NONE', #6381, #29382, #36541, .T. ) ;
#57466 = CARTESIAN_POINT ( 'NONE',  ( 20.84387692260743918, -22.22500000000000142, 4.000000000000000000 ) ) ;
#57467 = CARTESIAN_POINT ( 'NONE',  ( 105.0791937171295700, 3.975000000000002753, -6.884901960086283523 ) ) ;
#57468 = VECTOR ( 'NONE', #10951, 1000.000000000000000 ) ;
#57469 = CARTESIAN_POINT ( 'NONE',  ( -5.671830600776431197, -3.740707523384244837, 4.000000000000000000 ) ) ;
#57470 = CARTESIAN_POINT ( 'NONE',  ( 1.101062715680663384, 3.976440521211707768, 5.768354895643406977 ) ) ;
#57471 = LINE ( 'NONE', #37114, #70677 ) ;
#57472 = DIRECTION ( 'NONE',  ( -0.7071067811865486830, -0.7071067811865464625, 0.000000000000000000 ) ) ;
#57473 = FACE_OUTER_BOUND ( 'NONE', #20608, .T. ) ;
#57474 = CARTESIAN_POINT ( 'NONE',  ( 43.97502705046288440, -5.819803920172572198, 5.819803920172572198 ) ) ;
#57475 = CARTESIAN_POINT ( 'NONE',  ( -26.20710678118635428, 6.759292476615649470, 5.000000000000000000 ) ) ;
#57476 = FACE_OUTER_BOUND ( 'NONE', #28828, .T. ) ;
#57477 = ORIENTED_EDGE ( 'NONE', *, *, #56773, .F. ) ;
#57478 = ORIENTED_EDGE ( 'NONE', *, *, #26490, .F. ) ;
#57479 = CARTESIAN_POINT ( 'NONE',  ( 48.39583333333332860, -2.130196079827427091, 7.949999999999999289 ) ) ;
#57480 = EDGE_CURVE ( 'NONE', #111351, #126851, #95912, .T. ) ;
#57481 = VERTEX_POINT ( 'NONE', #49596 ) ;
#57482 = DIRECTION ( 'NONE',  ( 0.000000000000000000, 0.000000000000000000, -1.000000000000000000 ) ) ;
#57483 = ORIENTED_EDGE ( 'NONE', *, *, #89955, .T. ) ;
#57484 = ADVANCED_FACE ( 'NONE', ( #117631 ), #116950, .F. ) ;
#57485 = VECTOR ( 'NONE', #31512, 1000.000000000000000 ) ;
#57486 = LINE ( 'NONE', #3069, #50192 ) ;
#57488 = VECTOR ( 'NONE', #143169, 1000.000000000000000 ) ;
#57487 = CARTESIAN_POINT ( 'NONE',  ( -42.18398860626899705, 28.73617430169816700, 5.000000000000000000 ) ) ;
#57489 = CARTESIAN_POINT ( 'NONE',  ( 37.04209685856476852, 5.291415217122923842, -3.054999999999996163 ) ) ;
#57490 = ORIENTED_EDGE ( 'NONE', *, *, #133702, .T. ) ;
#57491 = CARTESIAN_POINT ( 'NONE',  ( -11.99999999999991296, -10.44781430457072346, 5.000000000000000000 ) ) ;
#57492 = ORIENTED_EDGE ( 'NONE', *, *, #130568, .T. ) ;
#57493 = EDGE_CURVE ( 'NONE', #47109, #120574, #40150, .T. ) ;
#57494 = CARTESIAN_POINT ( 'NONE',  ( 32.99451991528749062, 28.92564299267960948, 4.000000000000000000 ) ) ;
#57495 = FACE_OUTER_BOUND ( 'NONE', #48042, .T. ) ;
#57496 = ORIENTED_EDGE ( 'NONE', *, *, #96037, .F. ) ;
#57497 = CARTESIAN_POINT ( 'NONE',  ( -14.95341186370446884, 14.25929247661557753, 18.84478104361331674 ) ) ;
#57498 = ORIENTED_EDGE ( 'NONE', *, *, #113931, .F. ) ;
#57499 = PLANE ( 'NONE',  #81837 ) ;
#57500 = CARTESIAN_POINT ( 'NONE',  ( -27.48921356237309155, -27.52281430457074762, 5.000000000000000000 ) ) ;
#57501 = CARTESIAN_POINT ( 'NONE',  ( -34.17183060077623225, 15.75929247661555443, 4.000000000000000000 ) ) ;
#57502 = EDGE_CURVE ( 'NONE', #91612, #106637, #28537, .T. ) ;
#57503 = EDGE_CURVE ( 'NONE', #46830, #96047, #85036, .T. ) ;
#57504 = CARTESIAN_POINT ( 'NONE',  ( -11.99999999999990941, -9.412538124160661823, 4.000000000000000000 ) ) ;
#57505 = CARTESIAN_POINT ( 'NONE',  ( 15.67180000000000639, 3.174999999999997602, 0.000000000000000000 ) ) ;
#57506 = EDGE_CURVE ( 'NONE', #91733, #9906, #138006, .T. ) ;
#57507 = VERTEX_POINT ( 'NONE', #93779 ) ;
#57508 = STYLED_ITEM ( 'NONE', ( #87131 ), #93708 ) ;
#57509 = DIRECTION ( 'NONE',  ( -1.000000000000000000, -1.224606353822377258E-16, -0.000000000000000000 ) ) ;
#57510 = CARTESIAN_POINT ( 'NONE',  ( 56.34959685856478018, 6.109999999999996767, 1.637169565754163836 ) ) ;
#57511 = LINE ( 'NONE', #34308, #34847 ) ;
#57512 = CARTESIAN_POINT ( 'NONE',  ( 33.32816939922329880, -12.74070752338415247, 4.000000000000000000 ) ) ;
#57514 = ORIENTED_EDGE ( 'NONE', *, *, #122647, .F. ) ;
#57513 = DIRECTION ( 'NONE',  ( 0.7071067811865487940, 0.7071067811865463515, -0.000000000000000000 ) ) ;
#57515 = ORIENTED_EDGE ( 'NONE', *, *, #17599, .T. ) ;
#57516 = CARTESIAN_POINT ( 'NONE',  ( 17.85999999999999943, 9.521314400968980422E-16, 0.000000000000000000 ) ) ;
#57517 = EDGE_CURVE ( 'NONE', #61882, #50410, #17617, .T. ) ;
#57518 = ORIENTED_EDGE ( 'NONE', *, *, #2802, .F. ) ;
#57519 = VECTOR ( 'NONE', #11708, 1000.000000000000000 ) ;
#57520 = FACE_OUTER_BOUND ( 'NONE', #110993, .T. ) ;
#57521 = ORIENTED_EDGE ( 'NONE', *, *, #55004, .T. ) ;
#57522 = DIRECTION ( 'NONE',  ( -0.000000000000000000, 0.000000000000000000, 1.000000000000000000 ) ) ;
#57523 = DIRECTION ( 'NONE',  ( -0.000000000000000000, -0.3543493200069152693, 0.9351131265310292928 ) ) ;
#57524 = CARTESIAN_POINT ( 'NONE',  ( 3.328169399223511515, 20.25929247661551713, 4.000000000000000000 ) ) ;
#57525 = VECTOR ( 'NONE', #6279, 1000.000000000000000 ) ;
#57526 = AXIS2_PLACEMENT_3D ( 'NONE', #57589, #135156, #33692 ) ;
#57527 = DIRECTION ( 'NONE',  ( -1.000000000000000000, 0.000000000000000000, 0.000000000000000000 ) ) ;
#57528 = AXIS2_PLACEMENT_3D ( 'NONE', #71983, #115410, #27013 ) ;
#57529 = FACE_BOUND ( 'NONE', #124413, .T. ) ;
#57530 = LINE ( 'NONE', #101718, #94207 ) ;
#57531 = LINE ( 'NONE', #91566, #14214 ) ;
#57532 = LINE ( 'NONE', #124190, #34143 ) ;
#57534 = VERTEX_POINT ( 'NONE', #105353 ) ;
#57533 = DIRECTION ( 'NONE',  ( 0.7071067811865487940, -0.7071067811865463515, 0.000000000000000000 ) ) ;
#57535 = AXIS2_PLACEMENT_3D ( 'NONE', #37764, #92826, #113139 ) ;
#57536 = ORIENTED_EDGE ( 'NONE', *, *, #38250, .F. ) ;
#57537 = VECTOR ( 'NONE', #70408, 999.9999999999998863 ) ;
#57538 = CARTESIAN_POINT ( 'NONE',  ( -32.20710678118631165, -8.240707523384193323, 5.000000000000000000 ) ) ;
#57539 = EDGE_LOOP ( 'NONE', ( #41435, #105428, #96550, #94614, #66362 ) ) ;
#57540 = VERTEX_POINT ( 'NONE', #6010 ) ;
#57541 = CARTESIAN_POINT ( 'NONE',  ( 79.68293019189812298, -1.637169565754158951, -6.109999999999998543 ) ) ;
#57542 = ORIENTED_EDGE ( 'NONE', *, *, #9549, .F. ) ;
#57543 = DIRECTION ( 'NONE',  ( 0.000000000000000000, 0.000000000000000000, 1.000000000000000000 ) ) ;
#57544 = ADVANCED_FACE ( 'NONE', ( #38690 ), #19066, .T. ) ;
#57545 = EDGE_LOOP ( 'NONE', ( #66116, #27560, #32441 ) ) ;
#57546 = PLANE ( 'NONE',  #88390 ) ;
#57547 = AXIS2_PLACEMENT_3D ( 'NONE', #38686, #70640, #29219 ) ;
#57548 = LINE ( 'NONE', #11849, #130616 ) ;
#57549 = CIRCLE ( 'NONE', #97117, 2.999999999999999112 ) ;
#57550 = CARTESIAN_POINT ( 'NONE',  ( 1.827855086967997922, -2.055000000000000160, 2.789133085058097101E-16 ) ) ;
#57551 = CARTESIAN_POINT ( 'NONE',  ( 34.42499999999998295, 8.977185695429312773, 5.000000000000000000 ) ) ;
#57553 = FILL_AREA_STYLE ('',( #13996 ) ) ;
#57552 = FACE_OUTER_BOUND ( 'NONE', #40522, .T. ) ;
#57554 = DIRECTION ( 'NONE',  ( 0.000000000000000000, -1.000000000000000000, 0.000000000000000000 ) ) ;
#57555 = DIRECTION ( 'NONE',  ( 0.000000000000000000, 0.000000000000000000, 1.000000000000000000 ) ) ;
#57556 = ORIENTED_EDGE ( 'NONE', *, *, #73686, .T. ) ;
#57557 = EDGE_LOOP ( 'NONE', ( #78742, #37459, #16869, #74513 ) ) ;
#57558 = CARTESIAN_POINT ( 'NONE',  ( -18.28838880452753202, -2.745211937670052560, 5.000000000000000000 ) ) ;
#57559 = DIRECTION ( 'NONE',  ( 1.000000000000000000, 0.000000000000000000, 0.000000000000000000 ) ) ;
#57560 = ORIENTED_EDGE ( 'NONE', *, *, #128913, .F. ) ;
#57561 = AXIS2_PLACEMENT_3D ( 'NONE', #143154, #86658, #54049 ) ;
#57562 = ORIENTED_EDGE ( 'NONE', *, *, #11337, .T. ) ;
#57563 = AXIS2_PLACEMENT_3D ( 'NONE', #18083, #52178, #120248 ) ;
#57564 = VERTEX_POINT ( 'NONE', #106774 ) ;
#57565 = ADVANCED_FACE ( 'NONE', ( #84363 ), #7453, .T. ) ;
#57566 = EDGE_CURVE ( 'NONE', #100222, #84831, #51719, .T. ) ;
#57567 = CARTESIAN_POINT ( 'NONE',  ( 30.18793019189809357, 6.110000000000002984, -1.637169565754156730 ) ) ;
#57568 = EDGE_LOOP ( 'NONE', ( #60693, #126163, #78540, #55238 ) ) ;
#57569 = CARTESIAN_POINT ( 'NONE',  ( 45.04166666666665719, -3.975000000000002753, 6.884901960086286188 ) ) ;
#57570 = ADVANCED_FACE ( 'NONE', ( #61888 ), #106047, .F. ) ;
#57571 = CARTESIAN_POINT ( 'NONE',  ( -21.48921356237309155, -27.52281430457070499, 5.000000000000000000 ) ) ;
#57572 = CARTESIAN_POINT ( 'NONE',  ( 31.69163961620377634, 6.094999999999988205, -1.633150327867694651 ) ) ;
#57573 = CARTESIAN_POINT ( 'NONE',  ( 18.70701326429291456, -21.74070752338405654, 4.999753212805210012 ) ) ;
#57574 = ORIENTED_EDGE ( 'NONE', *, *, #124872, .F. ) ;
#57575 = ADVANCED_FACE ( 'NONE', ( #95190 ), #72068, .F. ) ;
#57576 = PLANE ( 'NONE',  #17874 ) ;
#57577 = CARTESIAN_POINT ( 'NONE',  ( 120.1000270504628986, 5.819803920172570422, 5.819803920172575751 ) ) ;
#57578 = LINE ( 'NONE', #23488, #93842 ) ;
#57579 = AXIS2_PLACEMENT_3D ( 'NONE', #127848, #82910, #106037 ) ;
#57581 = ORIENTED_EDGE ( 'NONE', *, *, #3332, .F. ) ;
#57580 = CARTESIAN_POINT ( 'NONE',  ( 7.171830600776432973, 21.75929247661550647, 4.000000000000000000 ) ) ;
#57582 = VERTEX_POINT ( 'NONE', #74174 ) ;
#57583 = FILL_AREA_STYLE ('',( #33687 ) ) ;
#57584 = LINE ( 'NONE', #66311, #53881 ) ;
#57585 = MECHANICAL_DESIGN_GEOMETRIC_PRESENTATION_REPRESENTATION (  '', ( #115366 ), #83020 ) ;
#57586 = CARTESIAN_POINT ( 'NONE',  ( 27.53159235450332076, 9.902892378096218942E-16, 0.000000000000000000 ) ) ;
#57587 = EDGE_CURVE ( 'NONE', #40891, #128588, #118365, .T. ) ;
#57588 = ORIENTED_EDGE ( 'NONE', *, *, #93089, .T. ) ;
#57589 = CARTESIAN_POINT ( 'NONE',  ( 16.30000000000000071, 9.521314400968980422E-16, 0.000000000000000000 ) ) ;
#57590 = CARTESIAN_POINT ( 'NONE',  ( -45.48921356237309510, -27.52281430457087197, 5.000000000000000000 ) ) ;
#57591 = SURFACE_SIDE_STYLE ('',( #13317 ) ) ;
#57592 =( NAMED_UNIT ( * ) SI_UNIT ( $, .STERADIAN. ) SOLID_ANGLE_UNIT ( ) );
#57593 = CARTESIAN_POINT ( 'NONE',  ( 1.499999999999997780, -11.94781430457070925, 5.000000000000000000 ) ) ;
#57594 = EDGE_CURVE ( 'NONE', #19920, #105277, #137296, .T. ) ;
#57595 = DIRECTION ( 'NONE',  ( 0.000000000000000000, 1.000000000000000000, 0.000000000000000000 ) ) ;
#57596 = LINE ( 'NONE', #47461, #12278 ) ;
#57597 = CARTESIAN_POINT ( 'NONE',  ( -34.92500000000001137, 20.18441419595454889, 5.773254242255872803 ) ) ;
#57598 = DIRECTION ( 'NONE',  ( -0.000000000000000000, -0.3543493200069152693, 0.9351131265310292928 ) ) ;
#57599 = CARTESIAN_POINT ( 'NONE',  ( -31.82816939922330235, 18.75929247661553134, 4.000000000000000000 ) ) ;
#57600 = ORIENTED_EDGE ( 'NONE', *, *, #30070, .T. ) ;
#57601 = ORIENTED_EDGE ( 'NONE', *, *, #9618, .F. ) ;
#57602 = EDGE_CURVE ( 'NONE', #123479, #19313, #116242, .T. ) ;
#57603 = EDGE_CURVE ( 'NONE', #98296, #80652, #115483, .T. ) ;
#57604 = DIRECTION ( 'NONE',  ( -0.7071067811865486830, 0.7071067811865464625, 0.000000000000000000 ) ) ;
#57605 = FACE_OUTER_BOUND ( 'NONE', #44021, .T. ) ;
#57606 = SURFACE_STYLE_FILL_AREA ( #99637 ) ;
#57607 = CARTESIAN_POINT ( 'NONE',  ( 4.553349423367797577, 2.259292476615694323, 14.86850063742353356 ) ) ;
#57608 = ORIENTED_EDGE ( 'NONE', *, *, #96621, .F. ) ;
#57609 = CARTESIAN_POINT ( 'NONE',  ( 24.79289321881328689, -8.240707523384202204, 5.000000000000000000 ) ) ;
#57610 = CARTESIAN_POINT ( 'NONE',  ( -6.707106781186496391, 11.25929247661560595, 5.000000000000000000 ) ) ;
#57611 = DIRECTION ( 'NONE',  ( 1.000000000000000000, 3.115803279706882722E-16, -0.000000000000000000 ) ) ;
#57612 = ORIENTED_EDGE ( 'NONE', *, *, #47132, .T. ) ;
#57613 = ADVANCED_FACE ( 'NONE', ( #87181 ), #64719, .T. ) ;
#57614 = CARTESIAN_POINT ( 'NONE',  ( -28.49999999999980460, -14.56887692260766443, 4.000000000000000000 ) ) ;
#57615 = CARTESIAN_POINT ( 'NONE',  ( 48.48921356237309510, -27.52281430457089328, 5.000000000000000000 ) ) ;
#57616 = CARTESIAN_POINT ( 'NONE',  ( 59.26626352523145869, 4.472830434245839371, -4.472830434245839371 ) ) ;
#57617 = CARTESIAN_POINT ( 'NONE',  ( -18.29974487139159223, -27.71228299555219010, 4.000000000000000000 ) ) ;
#57618 = EDGE_CURVE ( 'NONE', #138855, #94977, #66164, .T. ) ;
#57619 = EDGE_CURVE ( 'NONE', #6418, #77362, #65463, .T. ) ;
#57620 = VECTOR ( 'NONE', #120290, 1000.000000000000227 ) ;
#57621 = DIRECTION ( 'NONE',  ( 0.7071067811865487940, 0.7071067811865463515, 0.000000000000000000 ) ) ;
#57622 = ORIENTED_EDGE ( 'NONE', *, *, #4901, .T. ) ;
#57623 = DIRECTION ( 'NONE',  ( 0.7071067811865487940, -0.7071067811865463515, 0.000000000000000000 ) ) ;
#57624 = ORIENTED_EDGE ( 'NONE', *, *, #20804, .T. ) ;
#57625 = CARTESIAN_POINT ( 'NONE',  ( -14.16347128873441896, 15.75929247661555443, 9.299976744542886919 ) ) ;
#57626 = AXIS2_PLACEMENT_3D ( 'NONE', #46882, #1828, #133142 ) ;
#57627 = VECTOR ( 'NONE', #3340, 1000.000000000000114 ) ;
#57628 = VECTOR ( 'NONE', #87636, 1000.000000000000000 ) ;
#57629 = EDGE_CURVE ( 'NONE', #2459, #90362, #64462, .T. ) ;
#57630 = DIRECTION ( 'NONE',  ( -0.6830127018922180770, -0.6830127018922204085, -0.2588190451025213501 ) ) ;
#57631 = PLANE ( 'NONE',  #111384 ) ;
#57632 =( GEOMETRIC_REPRESENTATION_CONTEXT ( 3 ) GLOBAL_UNCERTAINTY_ASSIGNED_CONTEXT ( ( #105383 ) ) GLOBAL_UNIT_ASSIGNED_CONTEXT ( ( #89244, #38434, #60949 ) ) REPRESENTATION_CONTEXT ( 'NONE', 'WORKASPACE' ) );
#57633 = FACE_OUTER_BOUND ( 'NONE', #53802, .T. ) ;
#57634 = EDGE_CURVE ( 'NONE', #91413, #15309, #131411, .T. ) ;
#57635 = CYLINDRICAL_SURFACE ( 'NONE', #129791, 7.950000000000000178 ) ;
#57636 = CARTESIAN_POINT ( 'NONE',  ( 9.208651418775088970, 3.061616997868383634E-16, -2.500000000000000444 ) ) ;
#57637 = VERTEX_POINT ( 'NONE', #129979 ) ;
#57638 = ORIENTED_EDGE ( 'NONE', *, *, #65026, .F. ) ;
#57639 = CARTESIAN_POINT ( 'NONE',  ( 32.99999999999977973, -10.44781430457071458, 5.000000000000000000 ) ) ;
#57640 = CARTESIAN_POINT ( 'NONE',  ( 0.000000000000000000, 0.000000000000000000, 0.000000000000000000 ) ) ;
#57641 = UNCERTAINTY_MEASURE_WITH_UNIT (LENGTH_MEASURE( 1.000000000000000082E-05 ), #49956, 'distance_accuracy_value', 'NONE');
#57642 = CIRCLE ( 'NONE', #43748, 3.378199999999994319 ) ;
#57643 = VECTOR ( 'NONE', #93781, 1000.000000000000227 ) ;
#57644 = DIRECTION ( 'NONE',  ( 0.7071067811865486830, -0.7071067811865464625, -0.000000000000000000 ) ) ;
#57645 = LINE ( 'NONE', #136587, #55024 ) ;
#57646 = CARTESIAN_POINT ( 'NONE',  ( 70.80836038379624142, 7.949999999999997513, 2.130196079827431088 ) ) ;
#57647 = CARTESIAN_POINT ( 'NONE',  ( 3.792893218813431222, 12.75929247661559351, 5.000000000000000000 ) ) ;
#57648 = DIRECTION ( 'NONE',  ( -0.000000000000000000, -0.000000000000000000, 1.000000000000000000 ) ) ;
#57649 = ORIENTED_EDGE ( 'NONE', *, *, #14161, .T. ) ;
#57650 = CARTESIAN_POINT ( 'NONE',  ( 74.20833333333331439, -3.974999999999999201, -6.884901960086287964 ) ) ;
#57651 = EDGE_CURVE ( 'NONE', #127842, #142744, #106035, .T. ) ;
#57652 = PLANE ( 'NONE',  #47053 ) ;
#57653 = PLANE ( 'NONE',  #122614 ) ;
#57654 = CARTESIAN_POINT ( 'NONE',  ( -31.49999999999977973, 10.08746187583914811, 4.000000000000000000 ) ) ;
#57655 = PRESENTATION_LAYER_ASSIGNMENT (  '', '', ( #141012 ) ) ;
#57656 = PRESENTATION_LAYER_ASSIGNMENT (  '', '', ( #59916 ) ) ;
#57657 = ORIENTED_EDGE ( 'NONE', *, *, #66929, .F. ) ;
#57658 = EDGE_CURVE ( 'NONE', #16129, #107875, #32090, .T. ) ;
#57659 =( BOUNDED_CURVE ( )  B_SPLINE_CURVE ( 3, ( #9090, #52635, #31619, #119313 ),
 .UNSPECIFIED., .F., .F. ) 
 B_SPLINE_CURVE_WITH_KNOTS ( ( 4, 4 ),
 ( 5.143245962375971203, 6.645403452391246191 ),
 .UNSPECIFIED. ) 
 CURVE ( )  GEOMETRIC_REPRESENTATION_ITEM ( )  RATIONAL_B_SPLINE_CURVE ( ( 1.000000000000000000, 0.8206354192515254997, 0.8206354192515254997, 1.000000000000000000 ) ) 
 REPRESENTATION_ITEM ( '' )  );
#57660 = CARTESIAN_POINT ( 'NONE',  ( -22.59167451900985668, -0.7407075233842665973, 14.76736230305375130 ) ) ;
#57661 = VECTOR ( 'NONE', #65694, 1000.000000000000227 ) ;
#57662 = DIRECTION ( 'NONE',  ( 0.000000000000000000, 1.000000000000000000, 0.000000000000000000 ) ) ;
#57663 = CARTESIAN_POINT ( 'NONE',  ( 69.27126352523144703, 4.472830434245839371, 4.472830434245842035 ) ) ;
#57664 = DIRECTION ( 'NONE',  ( -0.7071067811865486830, -0.7071067811865464625, 0.000000000000000000 ) ) ;
#57665 = ORIENTED_EDGE ( 'NONE', *, *, #142328, .F. ) ;
#57666 = VERTEX_POINT ( 'NONE', #86485 ) ;
#57667 = AXIS2_PLACEMENT_3D ( 'NONE', #93996, #72312, #7696 ) ;
#57668 =( BOUNDED_CURVE ( )  B_SPLINE_CURVE ( 3, ( #142437, #143131, #30829, #64876 ),
 .UNSPECIFIED., .F., .T. ) 
 B_SPLINE_CURVE_WITH_KNOTS ( ( 4, 4 ),
 ( 1.208578181583236821, 1.359146454359482670 ),
 .UNSPECIFIED. ) 
 CURVE ( )  GEOMETRIC_REPRESENTATION_ITEM ( )  RATIONAL_B_SPLINE_CURVE ( ( 1.000000000000000000, 0.9981116584018941973, 0.9981116584018941973, 1.000000000000000000 ) ) 
 REPRESENTATION_ITEM ( '' )  );
#57669 = PLANE ( 'NONE',  #33753 ) ;
#57670 = CARTESIAN_POINT ( 'NONE',  ( -15.48921356237309510, -27.52281430457066236, 5.000000000000000000 ) ) ;
#57671 = VECTOR ( 'NONE', #138911, 1000.000000000000000 ) ;
#57672 = CARTESIAN_POINT ( 'NONE',  ( -13.08316395874281568, 3.014287036135060660, 4.000000000000000000 ) ) ;
#57673 = DIRECTION ( 'NONE',  ( 0.3543493200069162685, -0.000000000000000000, -0.9351131265310288487 ) ) ;
#57675 = ORIENTED_EDGE ( 'NONE', *, *, #19396, .F. ) ;
#57674 = CARTESIAN_POINT ( 'NONE',  ( -20.99999999999984368, -16.02097659208072855, -11.96015758381203575 ) ) ;
#57676 = DIRECTION ( 'NONE',  ( -0.6830127018922180770, -0.6830127018922204085, -0.2588190451025213501 ) ) ;
#57677 = CARTESIAN_POINT ( 'NONE',  ( 2.229957205422063993, 21.73644205237997440, 5.000000000000000888 ) ) ;
#57678 = DIRECTION ( 'NONE',  ( -0.6830127018922180770, -0.6830127018922204085, -0.2588190451025213501 ) ) ;
#57679 = CIRCLE ( 'NONE', #96923, 2.055000000000000604 ) ;
#57680 = CARTESIAN_POINT ( 'NONE',  ( 24.98155265364315625, 18.75929247661553134, 20.33588619593437485 ) ) ;
#57681 = MECHANICAL_DESIGN_GEOMETRIC_PRESENTATION_REPRESENTATION (  '', ( #103870 ), #41395 ) ;
#57682 = EDGE_LOOP ( 'NONE', ( #57612, #125480, #102992, #11630 ) ) ;
#57683 = EDGE_CURVE ( 'NONE', #33609, #115095, #43566, .T. ) ;
#57684 = EDGE_LOOP ( 'NONE', ( #37575, #100377, #101307, #28354 ) ) ;
#57685 = CARTESIAN_POINT ( 'NONE',  ( 59.06293019189809712, 1.637169565754157174, 6.110000000000002984 ) ) ;
#57686 = EDGE_CURVE ( 'NONE', #25494, #135001, #132136, .T. ) ;
#57687 = ORIENTED_EDGE ( 'NONE', *, *, #89116, .T. ) ;
#57688 = LINE ( 'NONE', #101866, #47600 ) ;
#57689 = DIRECTION ( 'NONE',  ( 0.7071067811865486830, -0.7071067811865464625, -0.000000000000000000 ) ) ;
#57690 = LINE ( 'NONE', #121476, #94273 ) ;
#57691 = CARTESIAN_POINT ( 'NONE',  ( -39.29974487139159578, -27.71228299555233576, 4.000000000000000000 ) ) ;
#57692 = CARTESIAN_POINT ( 'NONE',  ( -34.47516574401892342, 4.490517612115571211, 4.998110765256835286 ) ) ;
#57693 = VERTEX_POINT ( 'NONE', #53867 ) ;
#57694 = ORIENTED_EDGE ( 'NONE', *, *, #95833, .T. ) ;
#57695 = VECTOR ( 'NONE', #105347, 1000.000000000000000 ) ;
#57696 = CARTESIAN_POINT ( 'NONE',  ( -19.65190707646159751, -1.080577986147907454, -31.74483932211373372 ) ) ;
#57697 = VERTEX_POINT ( 'NONE', #19774 ) ;
#57698 = DIRECTION ( 'NONE',  ( -0.3543493200069162685, -0.000000000000000000, -0.9351131265310288487 ) ) ;
#57699 = CARTESIAN_POINT ( 'NONE',  ( 113.3916937171295700, 2.130196079827421762, 7.950000000000000178 ) ) ;
#57700 = CARTESIAN_POINT ( 'NONE',  ( 14.58437909282842426, -0.7858193515946185759, 4.111732654926449015 ) ) ;
#57701 = EDGE_LOOP ( 'NONE', ( #8316, #6697, #113915, #95209 ) ) ;
#57702 = FACE_BOUND ( 'NONE', #95246, .T. ) ;
#57703 = CARTESIAN_POINT ( 'NONE',  ( 69.48921356237309510, -27.52281430457103895, 5.000000000000000000 ) ) ;
#57704 = DIRECTION ( 'NONE',  ( -0.7071067811865486830, -0.7071067811865464625, 0.000000000000000000 ) ) ;
#57705 = FACE_OUTER_BOUND ( 'NONE', #140407, .T. ) ;
#57706 = CARTESIAN_POINT ( 'NONE',  ( 1.499999999999997780, 16.46639925780209168, 5.000000000000000000 ) ) ;
#57707 = CYLINDRICAL_SURFACE ( 'NONE', #13950, 2.552699999999959779 ) ;
#57708 = DIRECTION ( 'NONE',  ( -0.7477445707973108258, -0.5381879072143367360, -0.3888853730489201799 ) ) ;
#57709 = EDGE_LOOP ( 'NONE', ( #53841, #86131, #36945 ) ) ;
#57710 = ORIENTED_EDGE ( 'NONE', *, *, #60946, .T. ) ;
#57711 = CARTESIAN_POINT ( 'NONE',  ( 99.95376352523145158, -6.109999999999998543, -3.741295971395162543E-16 ) ) ;
#57712 = ORIENTED_EDGE ( 'NONE', *, *, #121698, .F. ) ;
#57713 = CARTESIAN_POINT ( 'NONE',  ( -34.92500000000001137, 22.22500000000000142, 4.000000000000000000 ) ) ;
#57714 = EDGE_LOOP ( 'NONE', ( #10000, #100511, #87320, #82639 ) ) ;
#57715 = CARTESIAN_POINT ( 'NONE',  ( -12.48921356237309155, -27.52281430457064104, 5.000000000000000000 ) ) ;
#57716 = CARTESIAN_POINT ( 'NONE',  ( 20.36747333860806819, 3.821174125832445049E-16, 0.000000000000000000 ) ) ;
#57717 = SPHERICAL_SURFACE ( 'NONE', #139726, 0.5000000000000000000 ) ;
#57718 = EDGE_LOOP ( 'NONE', ( #6158, #36528, #53607, #127436 ) ) ;
#57719 = CARTESIAN_POINT ( 'NONE',  ( -0.4892135623730947680, -27.52281430457055578, 5.000000000000000000 ) ) ;
#57720 = FILL_AREA_STYLE ('',( #68595 ) ) ;
#57721 = DIRECTION ( 'NONE',  ( 0.6830127018922180770, -0.6830127018922204085, -0.2588190451025213501 ) ) ;
#57722 = CARTESIAN_POINT ( 'NONE',  ( 67.64583333333331439, 2.130196079827431976, -7.949999999999998401 ) ) ;
#57723 = CARTESIAN_POINT ( 'NONE',  ( 27.10359120979227399, -7.619655331802865028, -2.702369829154340319 ) ) ;
#57724 = AXIS2_PLACEMENT_3D ( 'NONE', #72070, #70643, #82920 ) ;
#57725 = CARTESIAN_POINT ( 'NONE',  ( 26.40000000000000568, -16.48000000000005016, -12.70000000000045404 ) ) ;
#57726 = AXIS2_PLACEMENT_3D ( 'NONE', #76573, #120752, #66400 ) ;
#57727 = VERTEX_POINT ( 'NONE', #11012 ) ;
#57728 = DIRECTION ( 'NONE',  ( -0.000000000000000000, -0.000000000000000000, 1.000000000000000000 ) ) ;
#57729 = DIRECTION ( 'NONE',  ( -0.000000000000000000, 0.000000000000000000, 1.000000000000000000 ) ) ;
#57731 = EDGE_CURVE ( 'NONE', #40407, #58595, #55280, .T. ) ;
#57730 = VECTOR ( 'NONE', #93351, 1000.000000000000000 ) ;
#57732 = EDGE_LOOP ( 'NONE', ( #78220, #6063, #130297, #14502 ) ) ;
#57733 = ORIENTED_EDGE ( 'NONE', *, *, #140335, .T. ) ;
#57734 = EDGE_CURVE ( 'NONE', #29906, #32532, #76317, .T. ) ;
#57735 = EDGE_CURVE ( 'NONE', #113850, #5145, #108180, .T. ) ;
#57736 = VERTEX_POINT ( 'NONE', #126 ) ;
#57737 = CARTESIAN_POINT ( 'NONE',  ( 52.64626352523143282, -4.472830434245840259, 4.472830434245838482 ) ) ;
#57738 = ORIENTED_EDGE ( 'NONE', *, *, #80871, .T. ) ;
#57739 = PRESENTATION_LAYER_ASSIGNMENT (  '', '', ( #99284 ) ) ;
#57740 = EDGE_CURVE ( 'NONE', #80483, #123482, #123412, .T. ) ;
#57741 = EDGE_CURVE ( 'NONE', #61260, #82836, #60845, .T. ) ;
#57742 = CARTESIAN_POINT ( 'NONE',  ( 2.524972949537106270, -4.461849672132299993, -4.461849672132299105 ) ) ;
#57743 = CARTESIAN_POINT ( 'NONE',  ( 89.10459685856478984, 1.637169565754164946, -6.109999999999999432 ) ) ;
#57744 = LINE ( 'NONE', #35286, #59070 ) ;
#57745 = ORIENTED_EDGE ( 'NONE', *, *, #98847, .T. ) ;
#57746 = EDGE_CURVE ( 'NONE', #28445, #63490, #56743, .T. ) ;
#57747 = CARTESIAN_POINT ( 'NONE',  ( -48.18398860626899705, 28.73617430169820608, 5.000000000000000000 ) ) ;
#57748 = ORIENTED_EDGE ( 'NONE', *, *, #5526, .F. ) ;
#57749 = DIRECTION ( 'NONE',  ( 0.7071067811865486830, -0.7071067811865464625, -0.000000000000000000 ) ) ;
#57750 = VECTOR ( 'NONE', #31401, 1000.000000000000227 ) ;
#57751 = VECTOR ( 'NONE', #11899, 1000.000000000000000 ) ;
#57752 = DIRECTION ( 'NONE',  ( 0.7071067811865486830, -0.7071067811865464625, -0.000000000000000000 ) ) ;
#57753 = ORIENTED_EDGE ( 'NONE', *, *, #97046, .T. ) ;
#57754 = PRESENTATION_STYLE_ASSIGNMENT (( #12771 ) ) ;
#57755 = CARTESIAN_POINT ( 'NONE',  ( 16.40832548098991239, -0.7407075233842701500, 14.76736230305384190 ) ) ;
#57756 = LINE ( 'NONE', #70081, #72991 ) ;
#57757 = EDGE_CURVE ( 'NONE', #72725, #76924, #93426, .T. ) ;
#57758 = ORIENTED_EDGE ( 'NONE', *, *, #51924, .T. ) ;
#57759 = VECTOR ( 'NONE', #89363, 999.9999999999998863 ) ;
#57760 = DIRECTION ( 'NONE',  ( 0.3543493200069162685, -0.000000000000000000, -0.9351131265310288487 ) ) ;
#57761 = VERTEX_POINT ( 'NONE', #72434 ) ;
#57762 = EDGE_LOOP ( 'NONE', ( #103894, #56451, #113322, #35903 ) ) ;
#57763 = ORIENTED_EDGE ( 'NONE', *, *, #12528, .T. ) ;
#57764 = LINE ( 'NONE', #114253, #70227 ) ;
#57765 = VECTOR ( 'NONE', #106666, 1000.000000000000000 ) ;
#57766 = VECTOR ( 'NONE', #135877, 1000.000000000000000 ) ;
#57767 = PRESENTATION_STYLE_ASSIGNMENT (( #4005 ) ) ;
#57768 = VECTOR ( 'NONE', #87378, 1000.000000000000000 ) ;
#57769 = DIRECTION ( 'NONE',  ( -0.7071067811865486830, -0.7071067811865464625, 0.000000000000000000 ) ) ;
#57770 = CARTESIAN_POINT ( 'NONE',  ( -8.999999999999932498, 19.93112307739198386, 4.000000000000000000 ) ) ;
#57771 = VECTOR ( 'NONE', #95801, 1000.000000000000227 ) ;
#57772 = CARTESIAN_POINT ( 'NONE',  ( 16.76840764549667639, 9.139736423841732040E-16, 0.000000000000000000 ) ) ;
#57773 = EDGE_LOOP ( 'NONE', ( #17223, #14109, #95807, #65618 ) ) ;
#57774 = AXIS2_PLACEMENT_3D ( 'NONE', #68005, #1239, #122303 ) ;
#57775 = EDGE_CURVE ( 'NONE', #11393, #7217, #89323, .T. ) ;
#57776 = CIRCLE ( 'NONE', #20362, 2.500000000000000888 ) ;
#57777 = CARTESIAN_POINT ( 'NONE',  ( 14.90156419391754916, 11.25929247661560595, 10.79108189686410491 ) ) ;
#57778 = CARTESIAN_POINT ( 'NONE',  ( 22.29123647476855652, -9.717572351234235426E-16, -7.934999999999990727 ) ) ;
#57779 = FACE_OUTER_BOUND ( 'NONE', #26909, .T. ) ;
#57780 = LINE ( 'NONE', #91117, #122463 ) ;
#57781 = FACE_OUTER_BOUND ( 'NONE', #4400, .T. ) ;
#57782 = ORIENTED_EDGE ( 'NONE', *, *, #81474, .F. ) ;
#57783 = ORIENTED_EDGE ( 'NONE', *, *, #121757, .F. ) ;
#57785 = ORIENTED_EDGE ( 'NONE', *, *, #125210, .T. ) ;
#57784 = EDGE_CURVE ( 'NONE', #51247, #115197, #137662, .T. ) ;
#57786 = DIRECTION ( 'NONE',  ( 0.7071067811865487940, -0.7071067811865463515, 0.000000000000000000 ) ) ;
#57787 = UNCERTAINTY_MEASURE_WITH_UNIT (LENGTH_MEASURE( 1.000000000000000082E-05 ), #133637, 'distance_accuracy_value', 'NONE');
#57788 = AXIS2_PLACEMENT_3D ( 'NONE', #99195, #129698, #132610 ) ;
#57789 = CARTESIAN_POINT ( 'NONE',  ( 60.29974487139158867, -27.71228299555248142, 4.000000000000000000 ) ) ;
#57790 = CARTESIAN_POINT ( 'NONE',  ( 6.178324517025699514, 9.396498330079532835, -1.424408727490640070 ) ) ;
#57791 = EDGE_CURVE ( 'NONE', #102386, #142915, #45148, .T. ) ;
#57792 = DIRECTION ( 'NONE',  ( -0.7071067811865487940, 0.7071067811865463515, 0.000000000000000000 ) ) ;
#57793 = CARTESIAN_POINT ( 'NONE',  ( -11.99451991528749417, 28.92564299267946382, 4.000000000000000000 ) ) ;
#57794 = DIRECTION ( 'NONE',  ( -0.000000000000000000, 0.000000000000000000, 1.000000000000000000 ) ) ;
#57795 = DIRECTION ( 'NONE',  ( 0.000000000000000000, -1.000000000000000000, 0.000000000000000000 ) ) ;
#57796 = EDGE_CURVE ( 'NONE', #91593, #14375, #39041, .T. ) ;
#57797 = FACE_OUTER_BOUND ( 'NONE', #58527, .T. ) ;
#57798 = ORIENTED_EDGE ( 'NONE', *, *, #18551, .T. ) ;
#57799 = CARTESIAN_POINT ( 'NONE',  ( 19.65184941750880299, -1.080186769994980533, -31.74454988527380905 ) ) ;
#57800 = VERTEX_POINT ( 'NONE', #134266 ) ;
#57801 = EDGE_CURVE ( 'NONE', #137194, #122494, #57434, .T. ) ;
#57802 = CARTESIAN_POINT ( 'NONE',  ( 34.92499999999998295, -0.8020632299005416854, 13.72581505463526064 ) ) ;
#57804 = ORIENTED_EDGE ( 'NONE', *, *, #93938, .T. ) ;
#57803 = CARTESIAN_POINT ( 'NONE',  ( -3.005480084712505828, 28.92564299267936079, 4.000000000000000000 ) ) ;
#57805 = DIRECTION ( 'NONE',  ( 0.3543493200069162685, -0.000000000000000000, -0.9351131265310288487 ) ) ;
#57806 = DIRECTION ( 'NONE',  ( -1.000000000000000000, -0.000000000000000000, -0.000000000000000000 ) ) ;
#57807 = APPLICATION_CONTEXT ( 'automotive_design' ) ;
#57808 = VERTEX_POINT ( 'NONE', #68329 ) ;
#57809 = FACE_OUTER_BOUND ( 'NONE', #62, .T. ) ;
#57810 = EDGE_LOOP ( 'NONE', ( #12474, #113001, #73723, #106122 ) ) ;
#57811 = DIRECTION ( 'NONE',  ( -0.7071067811865487940, 0.7071067811865463515, -0.000000000000000000 ) ) ;
#57812 = EDGE_LOOP ( 'NONE', ( #103292, #95682, #130212, #20277 ) ) ;
#57813 = ADVANCED_FACE ( 'NONE', ( #15806 ), #112502, .F. ) ;
#57814 = DIRECTION ( 'NONE',  ( 0.7071067811865486830, -0.7071067811865464625, -0.000000000000000000 ) ) ;
#57815 = CARTESIAN_POINT ( 'NONE',  ( 103.7666937171295416, -7.949999999999999289, 2.130196079827424427 ) ) ;
#57816 = DIRECTION ( 'NONE',  ( -1.000000000000000000, -0.000000000000000000, -0.000000000000000000 ) ) ;
#57817 = VERTEX_POINT ( 'NONE', #49940 ) ;
#57818 = EDGE_CURVE ( 'NONE', #40570, #117341, #101619, .T. ) ;
#57819 = DIRECTION ( 'NONE',  ( 0.000000000000000000, -1.000000000000000000, 0.000000000000000000 ) ) ;
#57820 = CARTESIAN_POINT ( 'NONE',  ( 14.81601139373099585, 28.73617430169776910, 5.000000000000000000 ) ) ;
#57821 = CARTESIAN_POINT ( 'NONE',  ( 13.41666666666666785, 5.278424836066147208, 3.047499999999990550 ) ) ;
#57822 = CARTESIAN_POINT ( 'NONE',  ( 22.87456980810188867, 6.871911579029510442, -3.967499999999998916 ) ) ;
#57823 = DIRECTION ( 'NONE',  ( -0.6830127018922181881, 0.6830127018922202975, -0.2588190451025214056 ) ) ;
#57824 = DIRECTION ( 'NONE',  ( 0.000000000000000000, 0.000000000000000000, 1.000000000000000000 ) ) ;
#57825 = ORIENTED_EDGE ( 'NONE', *, *, #76492, .T. ) ;
#57826 = DIRECTION ( 'NONE',  ( -0.6830127018922180770, -0.6830127018922204085, -0.2588190451025213501 ) ) ;
#57827 = ORIENTED_EDGE ( 'NONE', *, *, #115787, .T. ) ;
#57828 = ADVANCED_FACE ( 'NONE', ( #83267 ), #16554, .F. ) ;
#57829 = CARTESIAN_POINT ( 'NONE',  ( 94.64626352523143282, -4.472830434245840259, 4.472830434245839371 ) ) ;
#57830 = FACE_OUTER_BOUND ( 'NONE', #73273, .T. ) ;
#57831 = CARTESIAN_POINT ( 'NONE',  ( 34.92499999999998295, -3.425372908132426453, 14.71988515618268423 ) ) ;
#57832 = FACE_OUTER_BOUND ( 'NONE', #65737, .T. ) ;
#57833 = CARTESIAN_POINT ( 'NONE',  ( 128.8595569075059473, -47.26730531257628343, -36.54674188582578154 ) ) ;
#57834 = EDGE_LOOP ( 'NONE', ( #471, #68902, #13091, #120973 ) ) ;
#57835 = AXIS2_PLACEMENT_3D ( 'NONE', #14745, #92287, #26346 ) ;
#57836 = VECTOR ( 'NONE', #125877, 1000.000000000000000 ) ;
#57837 = VECTOR ( 'NONE', #77724, 1000.000000000000000 ) ;
#57838 = LINE ( 'NONE', #23758, #100750 ) ;
#57839 = CARTESIAN_POINT ( 'NONE',  ( -16.17183060077636014, 15.75929247661555443, 4.000000000000000000 ) ) ;
#57840 = AXIS2_PLACEMENT_3D ( 'NONE', #38636, #61157, #40096 ) ;
#57841 = CARTESIAN_POINT ( 'NONE',  ( -17.28769006033960309, -21.73547319004781642, 4.999917730833662866 ) ) ;
#57842 = VERTEX_POINT ( 'NONE', #92691 ) ;
#57843 = CARTESIAN_POINT ( 'NONE',  ( 24.64327148205084939, 5.259292476615662792, 4.831541298974423526 ) ) ;
#57844 = DIRECTION ( 'NONE',  ( -0.7071067811865486830, -0.7071067811865464625, -0.000000000000000000 ) ) ;
#57846 = ORIENTED_EDGE ( 'NONE', *, *, #12121, .F. ) ;
#57845 = DIRECTION ( 'NONE',  ( 0.7071067811865486830, -0.7071067811865464625, -0.000000000000000000 ) ) ;
#57847 = CARTESIAN_POINT ( 'NONE',  ( -1.001930566820972812, -22.22500000000000142, 4.500000000000000888 ) ) ;
#57848 = LINE ( 'NONE', #45549, #56844 ) ;
#57849 = FACE_OUTER_BOUND ( 'NONE', #118562, .T. ) ;
#57850 = DIRECTION ( 'NONE',  ( -0.3543493200069162685, -0.000000000000000000, -0.9351131265310288487 ) ) ;
#57851 = STYLED_ITEM ( 'NONE', ( #121597 ), #139780 ) ;
#57852 =( BOUNDED_CURVE ( )  B_SPLINE_CURVE ( 3, ( #64023, #118377, #53880, #107511 ),
 .UNSPECIFIED., .F., .F. ) 
 B_SPLINE_CURVE_WITH_KNOTS ( ( 4, 4 ),
 ( 5.106027341939276099, 6.645403452391245303 ),
 .UNSPECIFIED. ) 
 CURVE ( )  GEOMETRIC_REPRESENTATION_ITEM ( )  RATIONAL_B_SPLINE_CURVE ( ( 1.000000000000000000, 0.8120851936182269526, 0.8120851936182269526, 1.000000000000000000 ) ) 
 REPRESENTATION_ITEM ( '' )  );
#57853 = DIRECTION ( 'NONE',  ( -0.000000000000000000, 0.3543493200069153248, 0.9351131265310292928 ) ) ;
#57854 = ORIENTED_EDGE ( 'NONE', *, *, #84921, .T. ) ;
#57855 = EDGE_CURVE ( 'NONE', #98898, #138457, #136927, .T. ) ;
#57856 = ORIENTED_EDGE ( 'NONE', *, *, #34253, .F. ) ;
#57857 = VERTEX_POINT ( 'NONE', #94118 ) ;
#57858 = CARTESIAN_POINT ( 'NONE',  ( 79.18793019189810423, 6.110000000000002984, -1.637169565754156730 ) ) ;
#57859 = AXIS2_PLACEMENT_3D ( 'NONE', #2822, #136916, #36875 ) ;
#57860 = ORIENTED_EDGE ( 'NONE', *, *, #53949, .T. ) ;
#57861 = DIRECTION ( 'NONE',  ( 0.7071067811865486830, -0.7071067811865464625, -0.000000000000000000 ) ) ;
#57862 = DIRECTION ( 'NONE',  ( 0.7071067811865487940, 0.7071067811865463515, 0.000000000000000000 ) ) ;
#57863 = VECTOR ( 'NONE', #133575, 999.9999999999998863 ) ;
#57864 = DIRECTION ( 'NONE',  ( 1.192622389734054877E-16, -1.000000000000000000, 0.000000000000000000 ) ) ;
#57865 = LINE ( 'NONE', #68049, #80204 ) ;
#57866 = ORIENTED_EDGE ( 'NONE', *, *, #111919, .T. ) ;
#57867 = CARTESIAN_POINT ( 'NONE',  ( 103.3750000000000000, 7.950000000000000178, 1.460391307983218535E-15 ) ) ;
#57868 = DIRECTION ( 'NONE',  ( -0.6830127018922180770, -0.6830127018922204085, -0.2588190451025213501 ) ) ;
#57869 = LINE ( 'NONE', #69446, #18653 ) ;
#57870 = VECTOR ( 'NONE', #121458, 1000.000000000000000 ) ;
#57871 = CARTESIAN_POINT ( 'NONE',  ( 76.18293019189810877, -1.637169565754158951, -6.109999999999998543 ) ) ;
#57872 = EDGE_CURVE ( 'NONE', #16056, #78330, #34968, .T. ) ;
#57873 = ORIENTED_EDGE ( 'NONE', *, *, #46059, .F. ) ;
#57874 = DIRECTION ( 'NONE',  ( -0.7071067811865486830, -0.7071067811865464625, -0.000000000000000000 ) ) ;
#57875 = DIRECTION ( 'NONE',  ( -0.7071067811865487940, 0.7071067811865463515, 0.000000000000000000 ) ) ;
#57876 = VECTOR ( 'NONE', #135232, 1000.000000000000000 ) ;
#57877 = VECTOR ( 'NONE', #115690, 1000.000000000000000 ) ;
#57878 = ORIENTED_EDGE ( 'NONE', *, *, #26850, .T. ) ;
#57879 = VERTEX_POINT ( 'NONE', #138359 ) ;
#57880 = FACE_OUTER_BOUND ( 'NONE', #117268, .T. ) ;
#57881 = EDGE_CURVE ( 'NONE', #97802, #73980, #2271, .T. ) ;
#57882 = VECTOR ( 'NONE', #82002, 1000.000000000000000 ) ;
#57883 = CARTESIAN_POINT ( 'NONE',  ( -42.29974487139158157, -27.71228299555235708, 4.000000000000000000 ) ) ;
#57884 = CARTESIAN_POINT ( 'NONE',  ( 23.69206980810188412, -7.934999999999990727, -2.126176841940955242 ) ) ;
#57885 = DIRECTION ( 'NONE',  ( -1.000000000000000000, 0.000000000000000000, -0.000000000000000000 ) ) ;
#57886 = VECTOR ( 'NONE', #25698, 1000.000000000000000 ) ;
#57887 = CARTESIAN_POINT ( 'NONE',  ( -63.48921356237309510, -27.52281430457099631, 5.000000000000000000 ) ) ;
#57888 = DIRECTION ( 'NONE',  ( 1.000000000000000000, 0.000000000000000000, 0.000000000000000000 ) ) ;
#57889 = CARTESIAN_POINT ( 'NONE',  ( 3.250000000000000000, -4.999999999999999112, -7.627214432543508948 ) ) ;
#57890 = SURFACE_STYLE_FILL_AREA ( #47733 ) ;
#57891 = ORIENTED_EDGE ( 'NONE', *, *, #134438, .T. ) ;
#57892 = ORIENTED_EDGE ( 'NONE', *, *, #36686, .T. ) ;
#57893 = DIRECTION ( 'NONE',  ( 0.7071067811865487940, -0.7071067811865463515, 0.000000000000000000 ) ) ;
#57894 = ORIENTED_EDGE ( 'NONE', *, *, #81051, .F. ) ;
#57895 = ORIENTED_EDGE ( 'NONE', *, *, #59300, .T. ) ;
#57896 = VECTOR ( 'NONE', #43889, 999.9999999999998863 ) ;
#57897 = PLANE ( 'NONE',  #105240 ) ;
#57898 = ORIENTED_EDGE ( 'NONE', *, *, #59981, .T. ) ;
#57899 = CARTESIAN_POINT ( 'NONE',  ( 56.51669371712956291, 7.950000000000000178, -2.130196079827421318 ) ) ;
#57900 = LINE ( 'NONE', #45598, #125890 ) ;
#57901 = EDGE_CURVE ( 'NONE', #71697, #106502, #11731, .T. ) ;
#57902 = DIRECTION ( 'NONE',  ( -0.7071067811865487940, 0.7071067811865463515, 0.000000000000000000 ) ) ;
#57903 = CARTESIAN_POINT ( 'NONE',  ( -35.01844734635648138, 18.75929247661553134, 20.33588619593451341 ) ) ;
#57904 = EDGE_CURVE ( 'NONE', #81604, #105391, #34238, .T. ) ;
#57905 = VECTOR ( 'NONE', #15422, 1000.000000000000227 ) ;
#57906 = PLANE ( 'NONE',  #111641 ) ;
#57907 = ORIENTED_EDGE ( 'NONE', *, *, #135394, .F. ) ;
#57908 = CARTESIAN_POINT ( 'NONE',  ( -13.49999999999990408, -19.53360074219754594, 5.000000000000000000 ) ) ;
#57909 = SURFACE_STYLE_FILL_AREA ( #112957 ) ;
#57910 = ORIENTED_EDGE ( 'NONE', *, *, #45438, .F. ) ;
#57911 = DIRECTION ( 'NONE',  ( -1.000000000000000000, -1.224606353822377258E-16, -0.000000000000000000 ) ) ;
#57912 = ORIENTED_EDGE ( 'NONE', *, *, #74290, .F. ) ;
#57913 = CARTESIAN_POINT ( 'NONE',  ( -24.29974487139158867, -27.71228299555223273, 4.000000000000000000 ) ) ;
#57916 = EDGE_CURVE ( 'NONE', #29477, #90522, #82824, .T. ) ;
#57915 = EDGE_LOOP ( 'NONE', ( #21536, #84690, #138665, #82397 ) ) ;
#57914 = EDGE_CURVE ( 'NONE', #45084, #137138, #111795, .T. ) ;
#57917 = LINE ( 'NONE', #92624, #96792 ) ;
#57918 = EDGE_LOOP ( 'NONE', ( #50201, #38300, #120216, #7663 ) ) ;
#57919 = ORIENTED_EDGE ( 'NONE', *, *, #128156, .T. ) ;
#57920 = VERTEX_POINT ( 'NONE', #50633 ) ;
#57921 = ADVANCED_FACE ( 'NONE', ( #97703 ), #128210, .T. ) ;
#57922 = ADVANCED_FACE ( 'NONE', ( #84013 ), #107143, .F. ) ;
#57923 = DIRECTION ( 'NONE',  ( 0.5735764363510448272, -0.8191520442889927978, 1.003171929053526103E-16 ) ) ;
#57924 = CARTESIAN_POINT ( 'NONE',  ( -63.18398860626900415, 28.73617430169831621, 5.000000000000000000 ) ) ;
#57926 = EDGE_CURVE ( 'NONE', #133007, #84626, #130352, .T. ) ;
#57925 = LINE ( 'NONE', #138306, #10315 ) ;
#57927 = CARTESIAN_POINT ( 'NONE',  ( 120.7504301918981184, 3.055000000000002824, -5.291415217122919401 ) ) ;
#57928 = PLANE ( 'NONE',  #51794 ) ;
#57929 = EDGE_CURVE ( 'NONE', #29579, #48649, #81983, .T. ) ;
#57930 = DIRECTION ( 'NONE',  ( -0.000000000000000000, 0.3543493200069153248, 0.9351131265310292928 ) ) ;
#57931 = CARTESIAN_POINT ( 'NONE',  ( -17.56319896779159606, -12.74070752338415069, 9.898150129686415610 ) ) ;
#57932 = EDGE_CURVE ( 'NONE', #108166, #83276, #9216, .T. ) ;
#57933 = CYLINDRICAL_SURFACE ( 'NONE', #77101, 0.5000000000000004441 ) ;
#57934 = CARTESIAN_POINT ( 'NONE',  ( -12.29974487139158512, -27.71228299555214747, 4.000000000000000000 ) ) ;
#57935 = EDGE_CURVE ( 'NONE', #59881, #5654, #117987, .T. ) ;
#57937 = ORIENTED_EDGE ( 'NONE', *, *, #14852, .F. ) ;
#57936 = VECTOR ( 'NONE', #105665, 1000.000000000000000 ) ;
#57938 = CARTESIAN_POINT ( 'NONE',  ( 0.000000000000000000, -0.6000000000000000888, 3.054668707061620747 ) ) ;
#57939 = ORIENTED_EDGE ( 'NONE', *, *, #15957, .F. ) ;
#57940 = ORIENTED_EDGE ( 'NONE', *, *, #35845, .F. ) ;
#57941 = VECTOR ( 'NONE', #95263, 1000.000000000000000 ) ;
#57942 = LINE ( 'NONE', #92650, #19442 ) ;
#57943 = AXIS2_PLACEMENT_3D ( 'NONE', #40107, #140115, #6675 ) ;
#57944 = AXIS2_PLACEMENT_3D ( 'NONE', #30494, #129069, #128379 ) ;
#57945 = VERTEX_POINT ( 'NONE', #107838 ) ;
#57946 = VECTOR ( 'NONE', #23117, 1000.000000000000000 ) ;
#57947 = AXIS2_PLACEMENT_3D ( 'NONE', #108847, #131349, #97247 ) ;
#57948 = CARTESIAN_POINT ( 'NONE',  ( -18.18398860626898994, 28.73617430169800002, 5.000000000000000000 ) ) ;
#57949 = CARTESIAN_POINT ( 'NONE',  ( 14.48330628287044064, 6.094999999999991758, 1.633150327867686880 ) ) ;
#57950 = EDGE_CURVE ( 'NONE', #94597, #74021, #62240, .T. ) ;
#57951 = CARTESIAN_POINT ( 'NONE',  ( -24.70710678118637205, 20.25929247661551713, 5.000000000000000000 ) ) ;
#57952 = CARTESIAN_POINT ( 'NONE',  ( -19.49999999999987210, -2.777013188829482893, 4.549262955118030582 ) ) ;
#57953 = EDGE_LOOP ( 'NONE', ( #96040, #141659, #126357, #32804, #121568 ) ) ;
#57954 = LINE ( 'NONE', #59373, #88201 ) ;
#57955 = VERTEX_POINT ( 'NONE', #106396 ) ;
#57956 = EDGE_CURVE ( 'NONE', #18457, #97230, #141955, .T. ) ;
#57957 = DIRECTION ( 'NONE',  ( -0.6830127018922181881, 0.6830127018922202975, -0.2588190451025214056 ) ) ;
#57958 = CARTESIAN_POINT ( 'NONE',  ( 28.06706980810189123, 2.126176841940952134, -7.934999999999993392 ) ) ;
#57959 = ORIENTED_EDGE ( 'NONE', *, *, #19772, .F. ) ;
#57960 = CARTESIAN_POINT ( 'NONE',  ( 42.48921356237308800, -27.52281430457085065, 5.000000000000000000 ) ) ;
#57961 = CARTESIAN_POINT ( 'NONE',  ( -2.510786437626908008, -27.52281430457053446, 5.000000000000000000 ) ) ;
#57962 = ORIENTED_EDGE ( 'NONE', *, *, #51502, .F. ) ;
#57963 = VERTEX_POINT ( 'NONE', #131054 ) ;
#57964 = VERTEX_POINT ( 'NONE', #52066 ) ;
#57966 = CIRCLE ( 'NONE', #28, 2.999999999999998224 ) ;
#57965 = DIRECTION ( 'NONE',  ( 1.000000000000000000, 0.000000000000000000, 0.000000000000000000 ) ) ;
#57967 = DIRECTION ( 'NONE',  ( 0.7071067811865487940, -0.7071067811865463515, 0.000000000000000000 ) ) ;
#57968 = DIRECTION ( 'NONE',  ( -0.000000000000000000, -0.3543493200069152693, 0.9351131265310292928 ) ) ;
#57969 = LINE ( 'NONE', #102166, #17246 ) ;
#57970 = EDGE_LOOP ( 'NONE', ( #79672, #91231, #5868, #59714 ) ) ;
#57971 = FACE_OUTER_BOUND ( 'NONE', #42832, .T. ) ;
#57972 = CARTESIAN_POINT ( 'NONE',  ( -13.10966639810773771, 3.759292476615678336, 4.164048746910666843 ) ) ;
#57973 = AXIS2_PLACEMENT_3D ( 'NONE', #102592, #135914, #3239 ) ;
#57974 = CARTESIAN_POINT ( 'NONE',  ( -0.2997448713915885632, -27.71228299555206220, 4.000000000000000000 ) ) ;
#57975 = LINE ( 'NONE', #15800, #95422 ) ;
#57976 = EDGE_CURVE ( 'NONE', #66483, #30242, #39787, .T. ) ;
#57977 = VECTOR ( 'NONE', #69964, 999.9999999999998863 ) ;
#57978 = ORIENTED_EDGE ( 'NONE', *, *, #136480, .T. ) ;
#57980 = CIRCLE ( 'NONE', #127370, 7.950000000000000178 ) ;
#57979 = CARTESIAN_POINT ( 'NONE',  ( -19.49999999999986144, -16.91253812416058366, 4.000000000000000000 ) ) ;
#57981 = VERTEX_POINT ( 'NONE', #117287 ) ;
#57982 = EDGE_CURVE ( 'NONE', #43201, #93841, #96945, .T. ) ;
#57984 = VERTEX_POINT ( 'NONE', #19427 ) ;
#57983 = CARTESIAN_POINT ( 'NONE',  ( -16.49999999999988276, -15.29013452822855967, 0.3645803511609976288 ) ) ;
#57985 = ORIENTED_EDGE ( 'NONE', *, *, #114098, .T. ) ;
#57986 = VECTOR ( 'NONE', #6183, 1000.000000000000000 ) ;
#57987 = LINE ( 'NONE', #102181, #5348 ) ;
#57988 = DIRECTION ( 'NONE',  ( 1.000000000000000000, 0.000000000000000000, 0.000000000000000000 ) ) ;
#57989 = VERTEX_POINT ( 'NONE', #96241 ) ;
#57990 =( LENGTH_UNIT ( ) NAMED_UNIT ( * ) SI_UNIT ( .MILLI., .METRE. ) );
#57991 = VERTEX_POINT ( 'NONE', #29577 ) ;
#57992 = ADVANCED_FACE ( 'NONE', ( #30306 ), #116601, .F. ) ;
#57993 = CARTESIAN_POINT ( 'NONE',  ( 34.92499999999998295, -8.028593703617110222, -6.464217593021339248 ) ) ;
#57994 = CARTESIAN_POINT ( 'NONE',  ( -57.29974487139158157, -27.71228299555246011, 4.000000000000000000 ) ) ;
#57995 = CARTESIAN_POINT ( 'NONE',  ( 2.999999999999978240, 4.965500833774331824, -4.007596771432663907 ) ) ;
#57996 = DIRECTION ( 'NONE',  ( -0.000000000000000000, -0.3543493200069152693, 0.9351131265310292928 ) ) ;
#57997 = FACE_OUTER_BOUND ( 'NONE', #8952, .T. ) ;
#57998 = EDGE_CURVE ( 'NONE', #98679, #31597, #92283, .T. ) ;
#57999 = PLANE ( 'NONE',  #102374 ) ;
#58000 = LINE ( 'NONE', #3542, #86486 ) ;
#58001 = CARTESIAN_POINT ( 'NONE',  ( 12.18398860626900060, 28.73617430169795739, 5.000000000000000000 ) ) ;
#58003 = VECTOR ( 'NONE', #84382, 999.9999999999998863 ) ;
#58002 = CARTESIAN_POINT ( 'NONE',  ( 19.66623647476855297, 7.934999999999990727, -1.457635852685135314E-15 ) ) ;
#58004 = CARTESIAN_POINT ( 'NONE',  ( 1.874569808101886226, 6.871911579029510442, -3.967499999999998916 ) ) ;
#58005 = LINE ( 'NONE', #34799, #92178 ) ;
#58006 = CARTESIAN_POINT ( 'NONE',  ( 26.51078643762690845, -27.52281430457036748, 5.000000000000000000 ) ) ;
#58007 = DIRECTION ( 'NONE',  ( -0.000000000000000000, -0.3543493200069152693, 0.9351131265310292928 ) ) ;
#58008 = VERTEX_POINT ( 'NONE', #41174 ) ;
#58009 = ORIENTED_EDGE ( 'NONE', *, *, #25324, .T. ) ;
#58010 = CARTESIAN_POINT ( 'NONE',  ( 96.52083333333332860, 7.949999999999999289, 2.130196079827431532 ) ) ;
#58011 = ORIENTED_EDGE ( 'NONE', *, *, #59723, .F. ) ;
#58012 = VERTEX_POINT ( 'NONE', #139083 ) ;
#58013 = ORIENTED_EDGE ( 'NONE', *, *, #142669, .T. ) ;
#58014 = CARTESIAN_POINT ( 'NONE',  ( 51.48921356237309510, -27.52281430457091460, 5.000000000000000000 ) ) ;
#58015 = DIRECTION ( 'NONE',  ( 0.7071067811865486830, -0.7071067811865464625, -0.000000000000000000 ) ) ;
#58016 = VECTOR ( 'NONE', #77551, 1000.000000000000000 ) ;
#58017 = CARTESIAN_POINT ( 'NONE',  ( 14.25109569580971147, 9.301276702823301434, -1.951341953592312883 ) ) ;
#58018 = ORIENTED_EDGE ( 'NONE', *, *, #116212, .T. ) ;
#58019 = CARTESIAN_POINT ( 'NONE',  ( 25.39999999999999858, -7.600000000000061817, 33.92499999999998295 ) ) ;
#58020 = CARTESIAN_POINT ( 'NONE',  ( -69.18398860626899705, 28.73617430169835529, 5.000000000000000000 ) ) ;
#58021 = FACE_OUTER_BOUND ( 'NONE', #624, .T. ) ;
#58022 = CARTESIAN_POINT ( 'NONE',  ( 0.000000000000000000, 0.000000000000000000, 0.000000000000000000 ) ) ;
#58023 = EDGE_CURVE ( 'NONE', #86178, #138040, #85384, .T. ) ;
#58024 = EDGE_CURVE ( 'NONE', #120984, #106637, #1218, .T. ) ;
#58025 = CARTESIAN_POINT ( 'NONE',  ( 127.3704301918981088, -3.055000000000001492, 5.291415217122917625 ) ) ;
#58026 = CARTESIAN_POINT ( 'NONE',  ( 5.206660635421493488, 21.75929247661549937, 4.998822639870701856 ) ) ;
#58027 = LINE ( 'NONE', #71027, #116778 ) ;
#58028 = CARTESIAN_POINT ( 'NONE',  ( -4.499999999999967137, 6.052185695429111334, 5.000000000000000000 ) ) ;
#58029 = DIRECTION ( 'NONE',  ( -1.000000000000000000, -0.000000000000000000, -0.000000000000000000 ) ) ;
#58030 = AXIS2_PLACEMENT_3D ( 'NONE', #106979, #19967, #7661 ) ;
#58031 = CARTESIAN_POINT ( 'NONE',  ( 15.48921356237309510, -27.52281430457066236, 5.000000000000000000 ) ) ;
#58032 = DIRECTION ( 'NONE',  ( -0.7071067811865487940, 0.7071067811865463515, 0.000000000000000000 ) ) ;
#58033 = DIRECTION ( 'NONE',  ( 0.7071067811865487940, 0.7071067811865463515, 0.000000000000000000 ) ) ;
#58034 = CARTESIAN_POINT ( 'NONE',  ( 56.10188787153392553, -51.19676978474260665, 38.21513923099968935 ) ) ;
#58035 = VERTEX_POINT ( 'NONE', #75957 ) ;
#58036 = VERTEX_POINT ( 'NONE', #22959 ) ;
#58037 = CARTESIAN_POINT ( 'NONE',  ( 107.7712635252314186, 4.472830434245839371, 4.472830434245842035 ) ) ;
#58038 = EDGE_LOOP ( 'NONE', ( #26679, #84699, #115724, #91926 ) ) ;
#58039 = EDGE_CURVE ( 'NONE', #42167, #39995, #43335, .T. ) ;
#58040 = DIRECTION ( 'NONE',  ( -0.6830127018922180770, -0.6830127018922202975, -0.2588190451025213501 ) ) ;
#58041 = DIRECTION ( 'NONE',  ( 0.7071067811865487940, 0.7071067811865463515, 0.000000000000000000 ) ) ;
#58042 = VECTOR ( 'NONE', #45333, 999.9999999999998863 ) ;
#58043 = CARTESIAN_POINT ( 'NONE',  ( 8.510786437626906675, -27.52281430457049183, 5.000000000000000000 ) ) ;
#58045 = EDGE_CURVE ( 'NONE', #83916, #40909, #101604, .T. ) ;
#58044 = CARTESIAN_POINT ( 'NONE',  ( 30.48921356237309510, -27.52281430457076894, 5.000000000000000000 ) ) ;
#58046 = VECTOR ( 'NONE', #112265, 1000.000000000000227 ) ;
#58047 = AXIS2_PLACEMENT_3D ( 'NONE', #113445, #135926, #45388 ) ;
#58048 = CARTESIAN_POINT ( 'NONE',  ( 100.8287635252314516, 0.000000000000000000, -6.109999999999998543 ) ) ;
#58049 = EDGE_CURVE ( 'NONE', #121495, #65849, #131919, .T. ) ;
#58050 = EDGE_LOOP ( 'NONE', ( #100888, #127988, #51324, #77807 ) ) ;
#58051 = ORIENTED_EDGE ( 'NONE', *, *, #2449, .T. ) ;
#58052 = CARTESIAN_POINT ( 'NONE',  ( 8.358306282870438864, -1.633150327867700202, 6.094999999999985540 ) ) ;
#58053 = AXIS2_PLACEMENT_3D ( 'NONE', #60811, #27397, #14406 ) ;
#58054 = CONICAL_SURFACE ( 'NONE', #113559, 2.055000000000001048, 0.9599310885968758145 ) ;
#58055 = AXIS2_PLACEMENT_3D ( 'NONE', #61377, #125146, #124434 ) ;
#58056 = AXIS2_PLACEMENT_3D ( 'NONE', #3080, #103798, #60354 ) ;
#58057 = CARTESIAN_POINT ( 'NONE',  ( 99.00000000000000000, 0.000000000000000000, -7.950000000000000178 ) ) ;
#58058 = VECTOR ( 'NONE', #57749, 1000.000000000000000 ) ;
#58059 = ORIENTED_EDGE ( 'NONE', *, *, #134001, .T. ) ;
#58060 = ORIENTED_EDGE ( 'NONE', *, *, #119046, .T. ) ;
#58061 = VERTEX_POINT ( 'NONE', #133908 ) ;
#58062 = CARTESIAN_POINT ( 'NONE',  ( 33.66846741159835688, -18.74070752338409562, 20.73178291233849535 ) ) ;
#58063 = ADVANCED_FACE ( 'NONE', ( #32462 ), #76699, .F. ) ;
#58064 = DIRECTION ( 'NONE',  ( -0.7071067811865487940, 0.7071067811865463515, 0.000000000000000000 ) ) ;
#58065 = VECTOR ( 'NONE', #34816, 1000.000000000000227 ) ;
#58066 = CARTESIAN_POINT ( 'NONE',  ( 34.47459685856478018, 1.637169565754164058, -6.109999999999996767 ) ) ;
#58067 = ORIENTED_EDGE ( 'NONE', *, *, #133808, .T. ) ;
#58068 = VERTEX_POINT ( 'NONE', #90397 ) ;
#58069 = DIRECTION ( 'NONE',  ( -1.000000000000000000, -1.224606353822377258E-16, -0.000000000000000000 ) ) ;
#58070 = VERTEX_POINT ( 'NONE', #67984 ) ;
#58071 = VERTEX_POINT ( 'NONE', #56393 ) ;
#58072 = VECTOR ( 'NONE', #40330, 999.9999999999998863 ) ;
#58073 = ORIENTED_EDGE ( 'NONE', *, *, #31040, .T. ) ;
#58074 = DIRECTION ( 'NONE',  ( -1.000000000000000000, -1.424048422229243832E-14, 0.000000000000000000 ) ) ;
#58075 = VECTOR ( 'NONE', #112938, 1000.000000000000227 ) ;
#58076 = DIRECTION ( 'NONE',  ( 0.7071067811865486830, -0.7071067811865464625, -0.000000000000000000 ) ) ;
#58077 = DIRECTION ( 'NONE',  ( 0.000000000000000000, -1.000000000000000000, 0.000000000000000000 ) ) ;
#58078 = ORIENTED_EDGE ( 'NONE', *, *, #91449, .F. ) ;
#58079 = LINE ( 'NONE', #35614, #113149 ) ;
#58080 = AXIS2_PLACEMENT_3D ( 'NONE', #104675, #138031, #17646 ) ;
#58081 = LINE ( 'NONE', #137028, #43736 ) ;
#58082 = AXIS2_PLACEMENT_3D ( 'NONE', #122852, #22092, #66349 ) ;
#58083 = FILL_AREA_STYLE_COLOUR ( '', #21187 ) ;
#58084 = FACE_BOUND ( 'NONE', #46881, .T. ) ;
#58085 = ORIENTED_EDGE ( 'NONE', *, *, #10098, .F. ) ;
#58086 = CARTESIAN_POINT ( 'NONE',  ( 63.66252705046289151, 7.949999999999998401, 1.460391307983218338E-15 ) ) ;
#58087 = DIRECTION ( 'NONE',  ( -0.7071067811865487940, 0.7071067811865463515, 0.000000000000000000 ) ) ;
#58088 =( GEOMETRIC_REPRESENTATION_CONTEXT ( 3 ) GLOBAL_UNCERTAINTY_ASSIGNED_CONTEXT ( ( #127136 ) ) GLOBAL_UNIT_ASSIGNED_CONTEXT ( ( #59065, #101079, #133732 ) ) REPRESENTATION_CONTEXT ( 'NONE', 'WORKASPACE' ) );
#58089 = LINE ( 'NONE', #56671, #111703 ) ;
#58090 = ORIENTED_EDGE ( 'NONE', *, *, #41484, .T. ) ;
#58091 = DIRECTION ( 'NONE',  ( -0.3543493200069162685, -0.000000000000000000, -0.9351131265310288487 ) ) ;
#58092 = ORIENTED_EDGE ( 'NONE', *, *, #11433, .F. ) ;
#58093 = ORIENTED_EDGE ( 'NONE', *, *, #46361, .T. ) ;
#58094 = ORIENTED_EDGE ( 'NONE', *, *, #63248, .T. ) ;
#58095 = EDGE_CURVE ( 'NONE', #8673, #37784, #10663, .T. ) ;
#58096 = CARTESIAN_POINT ( 'NONE',  ( 39.57876352523144448, -7.482591942790325086E-16, 6.109999999999998543 ) ) ;
#58097 = ORIENTED_EDGE ( 'NONE', *, *, #71820, .T. ) ;
#58098 =( GEOMETRIC_REPRESENTATION_CONTEXT ( 3 ) GLOBAL_UNCERTAINTY_ASSIGNED_CONTEXT ( ( #70990 ) ) GLOBAL_UNIT_ASSIGNED_CONTEXT ( ( #98940, #133740, #1043 ) ) REPRESENTATION_CONTEXT ( 'NONE', 'WORKASPACE' ) );
#58099 = CARTESIAN_POINT ( 'NONE',  ( -11.29289321881337571, -6.740707523384214639, 5.000000000000000000 ) ) ;
#58100 = EDGE_CURVE ( 'NONE', #113825, #11807, #111425, .T. ) ;
#58101 = ADVANCED_FACE ( 'NONE', ( #134642 ), #124696, .T. ) ;
#58102 = DIRECTION ( 'NONE',  ( -0.3543493200069162685, -0.000000000000000000, -0.9351131265310288487 ) ) ;
#58103 = ORIENTED_EDGE ( 'NONE', *, *, #105231, .F. ) ;
#58104 = ADVANCED_FACE ( 'NONE', ( #44053 ), #55644, .T. ) ;
#58105 =( LENGTH_UNIT ( ) NAMED_UNIT ( * ) SI_UNIT ( .MILLI., .METRE. ) );
#58107 = CARTESIAN_POINT ( 'NONE',  ( -3.489213562373097322, -27.52281430457057709, 5.000000000000000000 ) ) ;
#58106 = VECTOR ( 'NONE', #69603, 1000.000000000000227 ) ;
#58108 = EDGE_CURVE ( 'NONE', #51759, #133266, #110684, .T. ) ;
#58109 = LINE ( 'NONE', #102306, #125622 ) ;
#58110 = CARTESIAN_POINT ( 'NONE',  ( 19.41972383043609440, 4.584330080086930965E-16, 0.000000000000000000 ) ) ;
#58111 = DIRECTION ( 'NONE',  ( -0.7071067811865486830, -0.7071067811865464625, -0.000000000000000000 ) ) ;
#58112 = DIRECTION ( 'NONE',  ( 1.000000000000000000, 0.000000000000000000, 0.000000000000000000 ) ) ;
#58113 = ADVANCED_FACE ( 'NONE', ( #9975 ), #142642, .F. ) ;
#58114 = VERTEX_POINT ( 'NONE', #122288 ) ;
#58115 = ORIENTED_EDGE ( 'NONE', *, *, #100127, .F. ) ;
#58116 = ORIENTED_EDGE ( 'NONE', *, *, #84383, .F. ) ;
#58117 = VECTOR ( 'NONE', #4170, 1000.000000000000000 ) ;
#58118 = ORIENTED_EDGE ( 'NONE', *, *, #44662, .F. ) ;
#58119 = DIRECTION ( 'NONE',  ( -0.000000000000000000, 1.000000000000000000, 0.000000000000000000 ) ) ;
#58120 = ORIENTED_EDGE ( 'NONE', *, *, #74114, .T. ) ;
#58121 = ORIENTED_EDGE ( 'NONE', *, *, #79029, .T. ) ;
#58122 = DIRECTION ( 'NONE',  ( -0.7071067811865486830, 0.7071067811865464625, 0.000000000000000000 ) ) ;
#58123 = ADVANCED_FACE ( 'NONE', ( #99846 ), #66518, .F. ) ;
#58124 = EDGE_CURVE ( 'NONE', #67219, #19842, #78109, .T. ) ;
#58125 = FACE_OUTER_BOUND ( 'NONE', #32340, .T. ) ;
#58126 = EDGE_LOOP ( 'NONE', ( #139207, #7779, #129173, #142091, #103305 ) ) ;
#58127 = CARTESIAN_POINT ( 'NONE',  ( 34.92500000000001847, -6.269999999999991580, -40.00000000000000000 ) ) ;
#58128 = AXIS2_PLACEMENT_3D ( 'NONE', #85060, #74935, #31409 ) ;
#58129 = CIRCLE ( 'NONE', #51066, 2.055000000000000604 ) ;
#58130 = VERTEX_POINT ( 'NONE', #15642 ) ;
#58131 = EDGE_CURVE ( 'NONE', #123040, #46717, #114961, .T. ) ;
#58132 = DIRECTION ( 'NONE',  ( -0.7071067811865486830, -0.7071067811865464625, 0.000000000000000000 ) ) ;
#58133 = CARTESIAN_POINT ( 'NONE',  ( 23.69206980810188057, -7.934999999999991616, -2.126176841940955242 ) ) ;
#58134 = CARTESIAN_POINT ( 'NONE',  ( -0.5162635252314473622, -5.808823158059035485, -5.808823158059033709 ) ) ;
#58135 = ORIENTED_EDGE ( 'NONE', *, *, #32609, .T. ) ;
#58137 = CARTESIAN_POINT ( 'NONE',  ( -22.49999999999984368, -13.91253812416060853, 4.000000000000000000 ) ) ;
#58136 = CARTESIAN_POINT ( 'NONE',  ( 108.9954301918981088, 5.291415217122917625, 3.055000000000002380 ) ) ;
#58138 = CARTESIAN_POINT ( 'NONE',  ( -21.29974487139158512, -27.71228299555221142, 4.000000000000000000 ) ) ;
#58139 = FILL_AREA_STYLE_COLOUR ( '', #7139 ) ;
#58140 = VERTEX_POINT ( 'NONE', #16376 ) ;
#58142 = ORIENTED_EDGE ( 'NONE', *, *, #10429, .F. ) ;
#58141 = DIRECTION ( 'NONE',  ( -0.6830127018922180770, -0.6830127018922204085, -0.2588190451025213501 ) ) ;
#58143 = DIRECTION ( 'NONE',  ( -0.000000000000000000, 0.000000000000000000, 1.000000000000000000 ) ) ;
#58144 = CARTESIAN_POINT ( 'NONE',  ( 3.469446951953614189E-15, 10.55218569542906870, 5.000000000000000000 ) ) ;
#58145 = CARTESIAN_POINT ( 'NONE',  ( 28.00000000000002487, -49.14999999999999147, -34.92499999999976978 ) ) ;
#58146 = AXIS2_PLACEMENT_3D ( 'NONE', #63820, #107984, #8655 ) ;
#58147 = CARTESIAN_POINT ( 'NONE',  ( 23.99999999999983302, 18.08204922493375122, 0.9627537363044317287 ) ) ;
#58148 = CARTESIAN_POINT ( 'NONE',  ( 42.18398860626899705, 28.73617430169816700, 5.000000000000000000 ) ) ;
#58149 = ORIENTED_EDGE ( 'NONE', *, *, #69714, .T. ) ;
#58150 = VECTOR ( 'NONE', #136681, 1000.000000000000000 ) ;
#58151 = CARTESIAN_POINT ( 'NONE',  ( 55.56056557994608625, -52.00875322212550600, 39.86617647058822200 ) ) ;
#58152 = VECTOR ( 'NONE', #139366, 1000.000000000000000 ) ;
#58153 = CARTESIAN_POINT ( 'NONE',  ( 29.99999999999979039, 2.342191155542475034, -5.001666872980155887 ) ) ;
#58154 = PLANE ( 'NONE',  #127739 ) ;
#58155 = EDGE_CURVE ( 'NONE', #10046, #118345, #104840, .T. ) ;
#58156 = VERTEX_POINT ( 'NONE', #93961 ) ;
#58157 = CARTESIAN_POINT ( 'NONE',  ( 96.47502705046288440, -5.819803920172573086, 5.819803920172573086 ) ) ;
#58158 = VECTOR ( 'NONE', #102352, 1000.000000000000000 ) ;
#58159 = VECTOR ( 'NONE', #71347, 1000.000000000000000 ) ;
#58160 = CIRCLE ( 'NONE', #129926, 2.500000000000000444 ) ;
#58161 = VECTOR ( 'NONE', #28415, 1000.000000000000000 ) ;
#58162 = LINE ( 'NONE', #136376, #70148 ) ;
#58164 = ORIENTED_EDGE ( 'NONE', *, *, #99694, .T. ) ;
#58163 = VECTOR ( 'NONE', #14021, 1000.000000000000000 ) ;
#58166 = ORIENTED_EDGE ( 'NONE', *, *, #82792, .T. ) ;
#58165 = DIRECTION ( 'NONE',  ( -0.3543493200069163240, -0.000000000000000000, -0.9351131265310288487 ) ) ;
#58167 = ORIENTED_EDGE ( 'NONE', *, *, #101746, .F. ) ;
#58168 = CARTESIAN_POINT ( 'NONE',  ( -28.49999999999980105, -17.94781430457063820, 5.000000000000000000 ) ) ;
#58169 = AXIS2_PLACEMENT_3D ( 'NONE', #112205, #91852, #45543 ) ;
#58170 =( NAMED_UNIT ( * ) SI_UNIT ( $, .STERADIAN. ) SOLID_ANGLE_UNIT ( ) );
#58171 = VERTEX_POINT ( 'NONE', #25123 ) ;
#58172 = CARTESIAN_POINT ( 'NONE',  ( 34.42499999999998295, 19.54139925780185294, 5.000000000000000000 ) ) ;
#58173 = DIRECTION ( 'NONE',  ( 3.115803279706882722E-16, -1.000000000000000000, -1.016133275908817741E-16 ) ) ;
#58174 = VERTEX_POINT ( 'NONE', #101992 ) ;
#58175 = CIRCLE ( 'NONE', #30393, 2.500000000000000444 ) ;
#58176 = CARTESIAN_POINT ( 'NONE',  ( 16.88982677111777875, -22.22500000000000497, 4.785647885939349422 ) ) ;
#58177 = EDGE_CURVE ( 'NONE', #113634, #687, #37464, .T. ) ;
#58178 = LINE ( 'NONE', #35706, #60584 ) ;
#58179 =( NAMED_UNIT ( * ) SI_UNIT ( $, .STERADIAN. ) SOLID_ANGLE_UNIT ( ) );
#58180 = STYLED_ITEM ( 'NONE', ( #13354 ), #49611 ) ;
#58181 = LINE ( 'NONE', #102373, #51663 ) ;
#58182 = DIRECTION ( 'NONE',  ( -0.000000000000000000, 0.000000000000000000, 1.000000000000000000 ) ) ;
#58183 = CARTESIAN_POINT ( 'NONE',  ( -12.69999999999998153, 0.000000000000000000, 0.000000000000000000 ) ) ;
#58184 = CARTESIAN_POINT ( 'NONE',  ( -21.48921356237309155, -27.52281430457070499, 5.000000000000000000 ) ) ;
#58185 = EDGE_LOOP ( 'NONE', ( #131735, #81056, #140542, #20912 ) ) ;
#58186 = VECTOR ( 'NONE', #40755, 1000.000000000000000 ) ;
#58187 = VERTEX_POINT ( 'NONE', #126574 ) ;
#58188 = ORIENTED_EDGE ( 'NONE', *, *, #112245, .T. ) ;
#58189 = CARTESIAN_POINT ( 'NONE',  ( 119.7083333333333286, -3.974999999999999201, -6.884901960086287964 ) ) ;
#58190 = VECTOR ( 'NONE', #46823, 1000.000000000000000 ) ;
#58191 = EDGE_LOOP ( 'NONE', ( #89156, #110377, #107252 ) ) ;
#58192 = EDGE_LOOP ( 'NONE', ( #84719, #105484, #102943, #20265 ) ) ;
#58193 = EDGE_CURVE ( 'NONE', #107560, #26065, #104097, .T. ) ;
#58194 = VECTOR ( 'NONE', #128841, 1000.000000000000000 ) ;
#58195 = ORIENTED_EDGE ( 'NONE', *, *, #98134, .T. ) ;
#58196 = DIRECTION ( 'NONE',  ( 0.7071067811865486830, -0.7071067811865464625, -0.000000000000000000 ) ) ;
#58197 = CARTESIAN_POINT ( 'NONE',  ( 23.99999999999984013, 20.58746187583902909, 4.000000000000000000 ) ) ;
#58198 = AXIS2_PLACEMENT_3D ( 'NONE', #33560, #2280, #77061 ) ;
#58199 = EDGE_LOOP ( 'NONE', ( #74397, #110668, #65511, #8879 ) ) ;
#58200 = CARTESIAN_POINT ( 'NONE',  ( 34.92499999999998295, 22.22500000000000142, 4.500000000000000888 ) ) ;
#58201 = DIRECTION ( 'NONE',  ( -0.7071067811865486830, 0.7071067811865464625, 0.000000000000000000 ) ) ;
#58202 = CARTESIAN_POINT ( 'NONE',  ( -5.700255128608413102, -27.71228299555201957, 4.000000000000000000 ) ) ;
#58203 = CARTESIAN_POINT ( 'NONE',  ( 4.898587196589412829E-16, -60.00000000000000000, 4.000000000000000000 ) ) ;
#58204 = CARTESIAN_POINT ( 'NONE',  ( 109.9587635252314470, 0.000000000000000000, -6.110000000000001208 ) ) ;
#58205 = EDGE_CURVE ( 'NONE', #118058, #86236, #102714, .T. ) ;
#58206 = AXIS2_PLACEMENT_3D ( 'NONE', #17466, #49429, #104472 ) ;
#58207 = ORIENTED_EDGE ( 'NONE', *, *, #22225, .F. ) ;
#58208 = CARTESIAN_POINT ( 'NONE',  ( 9.291777089830421943, -15.74070752338411694, 19.73771281079099893 ) ) ;
#58209 = CARTESIAN_POINT ( 'NONE',  ( 105.8083603837962414, 7.949999999999996625, 2.130196079827431088 ) ) ;
#58210 = CARTESIAN_POINT ( 'NONE',  ( 34.92499999999998295, -2.781974347153350902, -4.476077389926498284 ) ) ;
#58211 = CARTESIAN_POINT ( 'NONE',  ( 10.52840764549667618, 9.139736423841732040E-16, 0.000000000000000000 ) ) ;
#58212 = PLANE ( 'NONE',  #121533 ) ;
#58213 = LINE ( 'NONE', #80642, #120985 ) ;
#58214 = CARTESIAN_POINT ( 'NONE',  ( -34.42500000000001137, 4.541399257801965739, 5.000000000000000000 ) ) ;
#58215 = CARTESIAN_POINT ( 'NONE',  ( 43.39169371712955581, 2.130196079827421762, 7.950000000000001066 ) ) ;
#58216 = LINE ( 'NONE', #114663, #2763 ) ;
#58217 = DIRECTION ( 'NONE',  ( -0.000000000000000000, 0.000000000000000000, 1.000000000000000000 ) ) ;
#58218 = VECTOR ( 'NONE', #71594, 1000.000000000000000 ) ;
#58219 = VERTEX_POINT ( 'NONE', #70127 ) ;
#58220 = ORIENTED_EDGE ( 'NONE', *, *, #74311, .F. ) ;
#58221 = CARTESIAN_POINT ( 'NONE',  ( 31.77083333333333215, -7.949999999999999289, -2.130196079827426203 ) ) ;
#58222 = VERTEX_POINT ( 'NONE', #4759 ) ;
#58223 = CARTESIAN_POINT ( 'NONE',  ( 152.4000000000000057, 7.919999999999947526, -18.97500000000001918 ) ) ;
#58224 = VECTOR ( 'NONE', #107010, 1000.000000000000000 ) ;
#58225 = DIRECTION ( 'NONE',  ( -0.7071067811865487940, 0.7071067811865463515, 0.000000000000000000 ) ) ;
#58226 = DIRECTION ( 'NONE',  ( 1.000000000000000000, 1.224606353822377258E-16, 0.000000000000000000 ) ) ;
#58227 = ORIENTED_EDGE ( 'NONE', *, *, #61710, .F. ) ;
#58228 = VECTOR ( 'NONE', #8498, 1000.000000000000000 ) ;
#58229 = CARTESIAN_POINT ( 'NONE',  ( 54.18398860626899705, 28.73617430169825226, 5.000000000000000000 ) ) ;
#58230 = DIRECTION ( 'NONE',  ( 1.000000000000000000, 0.000000000000000000, 0.000000000000000000 ) ) ;
#58231 = CARTESIAN_POINT ( 'NONE',  ( 41.41709685856477563, 3.054999999999998828, 5.291415217122922066 ) ) ;
#58232 = EDGE_CURVE ( 'NONE', #139414, #99498, #59241, .T. ) ;
#58233 = ORIENTED_EDGE ( 'NONE', *, *, #60905, .T. ) ;
#58234 = AXIS2_PLACEMENT_3D ( 'NONE', #48190, #125767, #93124 ) ;
#58235 = CARTESIAN_POINT ( 'NONE',  ( 7.630678725896657077, 22.22500000000000142, -11.12593748405039662 ) ) ;
#58236 = ORIENTED_EDGE ( 'NONE', *, *, #29833, .T. ) ;
#58237 = AXIS2_PLACEMENT_3D ( 'NONE', #138532, #114613, #81313 ) ;
#58238 = DIRECTION ( 'NONE',  ( -0.6830127018922180770, -0.6830127018922204085, -0.2588190451025213501 ) ) ;
#58239 = LINE ( 'NONE', #90839, #36122 ) ;
#58240 = FACE_OUTER_BOUND ( 'NONE', #93557, .T. ) ;
#58241 = PLANE ( 'NONE',  #118116 ) ;
#58243 = EDGE_CURVE ( 'NONE', #109156, #129380, #13626, .T. ) ;
#58242 = ORIENTED_EDGE ( 'NONE', *, *, #104423, .F. ) ;
#58244 = VERTEX_POINT ( 'NONE', #114287 ) ;
#58245 = LINE ( 'NONE', #1624, #88754 ) ;
#58246 = EDGE_CURVE ( 'NONE', #39048, #75609, #125171, .T. ) ;
#58247 = LINE ( 'NONE', #3088, #85550 ) ;
#58248 = DIRECTION ( 'NONE',  ( -0.7071067811865486830, -0.7071067811865464625, 0.000000000000000000 ) ) ;
#58249 = CARTESIAN_POINT ( 'NONE',  ( 3.489213562373097322, -27.52281430457057709, 5.000000000000000000 ) ) ;
#58250 = VECTOR ( 'NONE', #63009, 1000.000000000000000 ) ;
#58251 = DIRECTION ( 'NONE',  ( 8.673617379884034239E-17, -1.000000000000000000, 0.000000000000000000 ) ) ;
#58252 =( BOUNDED_CURVE ( )  B_SPLINE_CURVE ( 3, ( #41851, #96896, #74499, #66472 ),
 .UNSPECIFIED., .F., .T. ) 
 B_SPLINE_CURVE_WITH_KNOTS ( ( 4, 4 ),
 ( 2.431655599645419663, 2.488862747797044861 ),
 .UNSPECIFIED. ) 
 CURVE ( )  GEOMETRIC_REPRESENTATION_ITEM ( )  RATIONAL_B_SPLINE_CURVE ( ( 1.000000000000000000, 0.9997272971104411710, 0.9997272971104411710, 1.000000000000000000 ) ) 
 REPRESENTATION_ITEM ( '' )  );
#58253 = CARTESIAN_POINT ( 'NONE',  ( 59.26626352523145869, 4.472830434245839371, -4.472830434245838482 ) ) ;
#58254 = CARTESIAN_POINT ( 'NONE',  ( 21.66240673564756491, 0.000000000000000000, 0.000000000000000000 ) ) ;
#58255 = CARTESIAN_POINT ( 'NONE',  ( 7.499999999999954703, 10.46639925780215563, 5.000000000000000000 ) ) ;
#58256 = ORIENTED_EDGE ( 'NONE', *, *, #127392, .T. ) ;
#58257 = EDGE_LOOP ( 'NONE', ( #102322, #140003, #18471, #130513 ) ) ;
#58258 = DIRECTION ( 'NONE',  ( 0.7071067811865487940, 0.7071067811865463515, 0.000000000000000000 ) ) ;
#58259 = VECTOR ( 'NONE', #16349, 999.9999999999998863 ) ;
#58260 = ORIENTED_EDGE ( 'NONE', *, *, #107276, .T. ) ;
#58261 = EDGE_CURVE ( 'NONE', #4040, #6529, #14960, .T. ) ;
#58262 = VECTOR ( 'NONE', #17734, 999.9999999999998863 ) ;
#58263 = AXIS2_PLACEMENT_3D ( 'NONE', #94567, #93863, #38783 ) ;
#58264 = CARTESIAN_POINT ( 'NONE',  ( 34.25389700712507590, 22.27000000000000668, -12.46204991634331094 ) ) ;
#58265 = ORIENTED_EDGE ( 'NONE', *, *, #115932, .F. ) ;
#58266 = DIRECTION ( 'NONE',  ( 0.7071067811865486830, -0.7071067811865464625, -0.000000000000000000 ) ) ;
#58267 = VECTOR ( 'NONE', #42086, 1000.000000000000000 ) ;
#58269 = DIRECTION ( 'NONE',  ( 0.7071067811865487940, 0.7071067811865463515, -0.000000000000000000 ) ) ;
#58268 = VECTOR ( 'NONE', #87574, 1000.000000000000114 ) ;
#58270 = VECTOR ( 'NONE', #109475, 1000.000000000000000 ) ;
#58271 = VECTOR ( 'NONE', #99908, 1000.000000000000000 ) ;
#58272 = AXIS2_PLACEMENT_3D ( 'NONE', #103876, #61858, #18288 ) ;
#58273 = CARTESIAN_POINT ( 'NONE',  ( 4.045157733366646191, -21.74070752338405299, 21.72585301388584966 ) ) ;
#58274 = FACE_BOUND ( 'NONE', #53371, .T. ) ;
#58275 = LINE ( 'NONE', #56114, #101146 ) ;
#58276 = DIRECTION ( 'NONE',  ( 1.000000000000000000, 0.000000000000000000, 0.000000000000000000 ) ) ;
#58277 = FACE_OUTER_BOUND ( 'NONE', #142843, .T. ) ;
#58279 = EDGE_LOOP ( 'NONE', ( #35800, #142777, #102581, #88949 ) ) ;
#58278 = CARTESIAN_POINT ( 'NONE',  ( -9.183988606268997046, 28.73617430169793607, 5.000000000000000000 ) ) ;
#58280 = ORIENTED_EDGE ( 'NONE', *, *, #105148, .F. ) ;
#58281 = FACE_OUTER_BOUND ( 'NONE', #42894, .T. ) ;
#58282 = EDGE_LOOP ( 'NONE', ( #49306, #13625, #16512, #142394 ) ) ;
#58284 = ORIENTED_EDGE ( 'NONE', *, *, #68063, .F. ) ;
#58283 = ADVANCED_FACE ( 'NONE', ( #24424 ), #137487, .F. ) ;
#58285 = CARTESIAN_POINT ( 'NONE',  ( 65.09959685856478018, -6.109999999999997655, -1.637169565754160283 ) ) ;
#58286 = ORIENTED_EDGE ( 'NONE', *, *, #38752, .T. ) ;
#58287 = AXIS2_PLACEMENT_3D ( 'NONE', #54681, #32202, #111154 ) ;
#58288 = DIRECTION ( 'NONE',  ( -0.7071067811865487940, 0.7071067811865463515, 0.000000000000000000 ) ) ;
#58289 = EDGE_CURVE ( 'NONE', #133168, #11390, #115676, .T. ) ;
#58290 = ORIENTED_EDGE ( 'NONE', *, *, #56657, .F. ) ;
#58291 = LINE ( 'NONE', #93005, #30541 ) ;
#58292 = ADVANCED_FACE ( 'NONE', ( #91141 ), #5506, .F. ) ;
#58293 = ADVANCED_FACE ( 'NONE', ( #14262 ), #112853, .F. ) ;
#58294 = VECTOR ( 'NONE', #138462, 1000.000000000000000 ) ;
#58295 = CARTESIAN_POINT ( 'NONE',  ( 18.29974487139159223, -27.71228299555219010, 4.000000000000000000 ) ) ;
#58296 = CIRCLE ( 'NONE', #88258, 9.000000000000001776 ) ;
#58297 = CARTESIAN_POINT ( 'NONE',  ( 33.48921356237309510, -27.52281430457078670, 5.000000000000000000 ) ) ;
#58298 = CARTESIAN_POINT ( 'NONE',  ( 0.000000000000000000, 0.000000000000000000, 5.000000000000000000 ) ) ;
#58300 = CARTESIAN_POINT ( 'NONE',  ( 24.18398860626899705, 28.73617430169804265, 5.000000000000000000 ) ) ;
#58299 = CYLINDRICAL_SURFACE ( 'NONE', #129205, 2.500000000000000000 ) ;
#58301 = VECTOR ( 'NONE', #133849, 1000.000000000000000 ) ;
#58302 = CARTESIAN_POINT ( 'NONE',  ( -28.03340032343005461, 6.759292476615653023, 12.28218704918515591 ) ) ;
#58303 = LINE ( 'NONE', #59014, #120261 ) ;
#58304 = VERTEX_POINT ( 'NONE', #13524 ) ;
#58305 = ORIENTED_EDGE ( 'NONE', *, *, #78247, .T. ) ;
#58306 = AXIS2_PLACEMENT_3D ( 'NONE', #7844, #5694, #84035 ) ;
#58307 = DIRECTION ( 'NONE',  ( -0.7071067811865487940, 0.7071067811865463515, 0.000000000000000000 ) ) ;
#58308 = LINE ( 'NONE', #46722, #102204 ) ;
#58309 = ORIENTED_EDGE ( 'NONE', *, *, #19468, .F. ) ;
#58310 = ORIENTED_EDGE ( 'NONE', *, *, #99262, .F. ) ;
#58311 = VERTEX_POINT ( 'NONE', #135359 ) ;
#58312 = EDGE_CURVE ( 'NONE', #80179, #28705, #4038, .T. ) ;
#58313 = EDGE_CURVE ( 'NONE', #122891, #76404, #136747, .T. ) ;
#58314 = DIRECTION ( 'NONE',  ( 0.7071067811865487940, 0.7071067811865463515, -0.000000000000000000 ) ) ;
#58315 = EDGE_LOOP ( 'NONE', ( #30835, #84652, #125698, #138659 ) ) ;
#58316 = DIRECTION ( 'NONE',  ( 0.6830127018922181881, 0.6830127018922202975, -0.2588190451025214056 ) ) ;
#58317 = ADVANCED_FACE ( 'NONE', ( #18516 ), #41736, .F. ) ;
#58318 = DIRECTION ( 'NONE',  ( -1.000000000000000000, 0.000000000000000000, 0.000000000000000000 ) ) ;
#58319 = CARTESIAN_POINT ( 'NONE',  ( -0.5162635252314473622, -5.808823158059035485, -5.808823158059033709 ) ) ;
#58320 = LINE ( 'NONE', #122070, #21762 ) ;
#58321 = ORIENTED_EDGE ( 'NONE', *, *, #109447, .T. ) ;
#58322 = PLANE ( 'NONE',  #27208 ) ;
#58323 = CARTESIAN_POINT ( 'NONE',  ( 12.71159235450332048, 9.902892378096218942E-16, 0.000000000000000000 ) ) ;
#58324 = FACE_OUTER_BOUND ( 'NONE', #73251, .T. ) ;
#58325 = ADVANCED_FACE ( 'NONE', ( #74383 ), #30877, .F. ) ;
#58327 = ORIENTED_EDGE ( 'NONE', *, *, #142251, .T. ) ;
#58326 = CARTESIAN_POINT ( 'NONE',  ( -3.328169399223505742, 5.259292476615667233, 4.000000000000000000 ) ) ;
#58328 = VECTOR ( 'NONE', #43684, 1000.000000000000000 ) ;
#58329 = ORIENTED_EDGE ( 'NONE', *, *, #57373, .F. ) ;
#58330 = CARTESIAN_POINT ( 'NONE',  ( 5.848407645496676466, -2.499999999999999556, 0.000000000000000000 ) ) ;
#58331 = DIRECTION ( 'NONE',  ( 1.000000000000000000, 1.224606353822377258E-16, 0.000000000000000000 ) ) ;
#58332 = VERTEX_POINT ( 'NONE', #30129 ) ;
#58333 = LINE ( 'NONE', #122085, #57420 ) ;
#58334 = LINE ( 'NONE', #25635, #124301 ) ;
#58335 = VECTOR ( 'NONE', #89111, 1000.000000000000000 ) ;
#58336 = DIRECTION ( 'NONE',  ( 0.000000000000000000, -1.000000000000000000, 0.000000000000000000 ) ) ;
#58337 = LINE ( 'NONE', #102520, #48704 ) ;
#58338 = FACE_OUTER_BOUND ( 'NONE', #37123, .T. ) ;
#58339 = EDGE_CURVE ( 'NONE', #24531, #89253, #51195, .T. ) ;
#58340 = VECTOR ( 'NONE', #109625, 1000.000000000000000 ) ;
#58341 = ORIENTED_EDGE ( 'NONE', *, *, #51672, .F. ) ;
#58342 = DIRECTION ( 'NONE',  ( -0.7071067811865487940, 0.7071067811865463515, -0.000000000000000000 ) ) ;
#58343 = DIRECTION ( 'NONE',  ( -0.000000000000000000, 0.3543493200069153248, 0.9351131265310292928 ) ) ;
#58344 = CARTESIAN_POINT ( 'NONE',  ( 0.000000000000000000, 0.000000000000000000, 5.000000000000000000 ) ) ;
#58345 = CARTESIAN_POINT ( 'NONE',  ( 20.35681257248249310, -20.24070752338407431, 21.22881796311217428 ) ) ;
#58346 = ORIENTED_EDGE ( 'NONE', *, *, #2709, .T. ) ;
#58347 = EDGE_CURVE ( 'NONE', #75683, #116329, #127301, .T. ) ;
#58348 = ORIENTED_EDGE ( 'NONE', *, *, #82583, .T. ) ;
#58349 = ADVANCED_FACE ( 'NONE', ( #128051 ), #40334, .T. ) ;
#58350 = VECTOR ( 'NONE', #128398, 1000.000000000000000 ) ;
#58351 = FILL_AREA_STYLE ('',( #134441 ) ) ;
#58352 = CARTESIAN_POINT ( 'NONE',  ( -56.99451991528749062, 28.92564299267978001, 4.000000000000000000 ) ) ;
#58353 = EDGE_CURVE ( 'NONE', #25609, #49451, #73653, .T. ) ;
#58354 =( LENGTH_UNIT ( ) NAMED_UNIT ( * ) SI_UNIT ( .MILLI., .METRE. ) );
#58355 = CARTESIAN_POINT ( 'NONE',  ( -34.49999999999976552, -2.945670655169033481, 4.994342998332163219 ) ) ;
#58356 = LINE ( 'NONE', #1031, #136445 ) ;
#58357 = CARTESIAN_POINT ( 'NONE',  ( 34.92499999999998295, -7.285322628117683053, -6.182564397582753557 ) ) ;
#58358 = CARTESIAN_POINT ( 'NONE',  ( 39.48921356237310221, -27.52281430457082934, 5.000000000000000000 ) ) ;
#58359 = ORIENTED_EDGE ( 'NONE', *, *, #14852, .T. ) ;
#58360 = DIRECTION ( 'NONE',  ( 0.6830127018922180770, 0.6830127018922202975, -0.2588190451025213501 ) ) ;
#58361 = LINE ( 'NONE', #127864, #116377 ) ;
#58362 = VECTOR ( 'NONE', #74915, 1000.000000000000000 ) ;
#58363 = AXIS2_PLACEMENT_3D ( 'NONE', #75567, #76286, #824 ) ;
#58364 = CARTESIAN_POINT ( 'NONE',  ( 8.968407645496675684, 9.139736423841732040E-16, 0.000000000000000000 ) ) ;
#58365 = CARTESIAN_POINT ( 'NONE',  ( 60.87043019189810877, -3.055000000000001936, 5.291415217122918513 ) ) ;
#58366 = DIRECTION ( 'NONE',  ( 0.7071067811865487940, 0.7071067811865463515, 0.000000000000000000 ) ) ;
#58367 = VECTOR ( 'NONE', #111374, 1000.000000000000000 ) ;
#58368 = AXIS2_PLACEMENT_3D ( 'NONE', #24870, #124901, #58276 ) ;
#58369 = DIRECTION ( 'NONE',  ( -0.7071067811865487940, 0.7071067811865463515, -0.000000000000000000 ) ) ;
#58370 = EDGE_LOOP ( 'NONE', ( #97754, #22727, #137595, #124350 ) ) ;
#58371 = LINE ( 'NONE', #132340, #7063 ) ;
#58372 = ORIENTED_EDGE ( 'NONE', *, *, #94851, .T. ) ;
#58373 = VECTOR ( 'NONE', #61252, 1000.000000000000000 ) ;
#58374 = VECTOR ( 'NONE', #130195, 1000.000000000000000 ) ;
#58375 = DIRECTION ( 'NONE',  ( 1.734723475976806848E-16, -1.000000000000000000, 0.000000000000000000 ) ) ;
#58376 = PRESENTATION_LAYER_ASSIGNMENT (  '', '', ( #55964 ) ) ;
#58377 = DIRECTION ( 'NONE',  ( 1.000000000000000000, 0.000000000000000000, 0.000000000000000000 ) ) ;
#58378 = DIRECTION ( 'NONE',  ( 0.3543493200069162685, -0.000000000000000000, -0.9351131265310288487 ) ) ;
#58379 = LINE ( 'NONE', #92349, #64912 ) ;
#58380 = CARTESIAN_POINT ( 'NONE',  ( -14.67183060077637080, 11.25929247661560595, 4.000000000000000000 ) ) ;
#58381 = FACE_OUTER_BOUND ( 'NONE', #96527, .T. ) ;
#58382 = ORIENTED_EDGE ( 'NONE', *, *, #46026, .T. ) ;
#58383 = EDGE_LOOP ( 'NONE', ( #71470, #31278, #94081, #97365 ) ) ;
#58384 = DIRECTION ( 'NONE',  ( -0.000000000000000000, 0.3543493200069153248, 0.9351131265310292928 ) ) ;
#58385 = CARTESIAN_POINT ( 'NONE',  ( 28.49999999999980460, -5.568876922607759461, 4.000000000000000000 ) ) ;
#58386 = DIRECTION ( 'NONE',  ( -0.000000000000000000, -0.3543493200069152693, 0.9351131265310292928 ) ) ;
#58387 = DIRECTION ( 'NONE',  ( -0.7071067811865486830, -0.7071067811865464625, 0.000000000000000000 ) ) ;
#58388 = CARTESIAN_POINT ( 'NONE',  ( 78.53752705046289861, -9.735942053221456900E-16, 7.949999999999998401 ) ) ;
#58389 = CARTESIAN_POINT ( 'NONE',  ( -19.82816939922339472, -8.240707523384191546, 4.000000000000000000 ) ) ;
#58390 = DIRECTION ( 'NONE',  ( -0.7071067811865486830, -0.7071067811865464625, 0.000000000000000000 ) ) ;
#58391 = ORIENTED_EDGE ( 'NONE', *, *, #47607, .T. ) ;
#58392 = CARTESIAN_POINT ( 'NONE',  ( 73.33333333333332860, -6.884901960086287964, 3.974999999999998312 ) ) ;
#58393 = CARTESIAN_POINT ( 'NONE',  ( -27.48921356237309155, -27.52281430457074762, 5.000000000000000000 ) ) ;
#58394 = CARTESIAN_POINT ( 'NONE',  ( -25.49999999999981526, -7.533600742197664069, 5.000000000000000000 ) ) ;
#58395 = CARTESIAN_POINT ( 'NONE',  ( -12.69999999999998153, 0.000000000000000000, 0.000000000000000000 ) ) ;
#58396 = VERTEX_POINT ( 'NONE', #8348 ) ;
#58397 = VECTOR ( 'NONE', #119358, 999.9999999999998863 ) ;
#58398 = CARTESIAN_POINT ( 'NONE',  ( -16.82816939922340893, 21.75929247661550647, 4.000000000000000000 ) ) ;
#58399 =( GEOMETRIC_REPRESENTATION_CONTEXT ( 3 ) GLOBAL_UNCERTAINTY_ASSIGNED_CONTEXT ( ( #96953 ) ) GLOBAL_UNIT_ASSIGNED_CONTEXT ( ( #67876, #36616, #91037 ) ) REPRESENTATION_CONTEXT ( 'NONE', 'WORKASPACE' ) );
#58400 = DIRECTION ( 'NONE',  ( -0.6830127018922181881, 0.6830127018922202975, -0.2588190451025214056 ) ) ;
#58401 = CARTESIAN_POINT ( 'NONE',  ( 65.04209685856477563, 5.291415217122923842, -3.054999999999996163 ) ) ;
#58402 = VECTOR ( 'NONE', #55788, 999.9999999999998863 ) ;
#58403 = LINE ( 'NONE', #111984, #117699 ) ;
#58404 = ORIENTED_EDGE ( 'NONE', *, *, #38478, .F. ) ;
#58405 = ORIENTED_EDGE ( 'NONE', *, *, #28442, .T. ) ;
#58406 = VECTOR ( 'NONE', #36416, 1000.000000000000227 ) ;
#58407 = LINE ( 'NONE', #62646, #12900 ) ;
#58408 = CARTESIAN_POINT ( 'NONE',  ( 43.87500000000000000, 7.950000000000000178, 1.460391307983218535E-15 ) ) ;
#58409 = EDGE_CURVE ( 'NONE', #87440, #56693, #128736, .T. ) ;
#58410 = DIRECTION ( 'NONE',  ( 0.7071067811865487940, 0.7071067811865463515, 0.000000000000000000 ) ) ;
#58412 = ORIENTED_EDGE ( 'NONE', *, *, #130295, .T. ) ;
#58411 = CARTESIAN_POINT ( 'NONE',  ( 86.75000000000000000, -9.735942053221458872E-16, 7.950000000000000178 ) ) ;
#58413 = EDGE_CURVE ( 'NONE', #108755, #15722, #139655, .T. ) ;
#58414 = DIRECTION ( 'NONE',  ( 0.7071067811865487940, 0.7071067811865463515, 0.000000000000000000 ) ) ;
#58415 = DIRECTION ( 'NONE',  ( -1.000000000000000000, -1.224606353822377258E-16, -0.000000000000000000 ) ) ;
#58416 = DIRECTION ( 'NONE',  ( 0.7071067811865486830, -0.7071067811865464625, -0.000000000000000000 ) ) ;
#58417 = VECTOR ( 'NONE', #129912, 1000.000000000000000 ) ;
#58418 = CARTESIAN_POINT ( 'NONE',  ( 25.39999999999999858, 0.000000000000000000, 0.000000000000000000 ) ) ;
#58419 = ORIENTED_EDGE ( 'NONE', *, *, #3710, .T. ) ;
#58420 = ORIENTED_EDGE ( 'NONE', *, *, #113496, .T. ) ;
#58421 = CARTESIAN_POINT ( 'NONE',  ( 57.60459685856477563, 1.637169565754164946, -6.109999999999999432 ) ) ;
#58422 = ORIENTED_EDGE ( 'NONE', *, *, #116656, .F. ) ;
#58423 = ADVANCED_FACE ( 'NONE', ( #72272 ), #52599, .F. ) ;
#58424 = PLANE ( 'NONE',  #96167 ) ;
#58425 = LINE ( 'NONE', #101149, #78811 ) ;
#58426 = CARTESIAN_POINT ( 'NONE',  ( 17.20710678118642889, -11.24070752338416668, 5.000000000000000000 ) ) ;
#58427 = VECTOR ( 'NONE', #126635, 1000.000000000000000 ) ;
#58428 = LINE ( 'NONE', #102607, #36214 ) ;
#58429 = CARTESIAN_POINT ( 'NONE',  ( 54.08333333333332860, 6.884901960086290629, -3.974999999999994316 ) ) ;
#58430 = EDGE_LOOP ( 'NONE', ( #47775, #20356, #90, #66760, #3793, #125945 ) ) ;
#58431 = ORIENTED_EDGE ( 'NONE', *, *, #113792, .T. ) ;
#58432 = AXIS2_PLACEMENT_3D ( 'NONE', #76890, #66701, #44995 ) ;
#58433 = FACE_OUTER_BOUND ( 'NONE', #18295, .T. ) ;
#58434 = CARTESIAN_POINT ( 'NONE',  ( -16.84500517045543333, -0.1638869648888886532, -31.04645391278758026 ) ) ;
#58435 = EDGE_CURVE ( 'NONE', #95865, #105802, #38878, .T. ) ;
#58436 = ORIENTED_EDGE ( 'NONE', *, *, #42419, .T. ) ;
#58437 = CARTESIAN_POINT ( 'NONE',  ( -19.17183060077633172, 9.759292476615618384, 4.000000000000000000 ) ) ;
#58438 = EDGE_LOOP ( 'NONE', ( #7474, #89482, #113677, #102523 ) ) ;
#58439 = FACE_OUTER_BOUND ( 'NONE', #38031, .T. ) ;
#58440 = DIRECTION ( 'NONE',  ( 0.6830127018922180770, -0.6830127018922204085, -0.2588190451025213501 ) ) ;
#58441 = AXIS2_PLACEMENT_3D ( 'NONE', #127467, #37629, #82546 ) ;
#58442 = EDGE_CURVE ( 'NONE', #111882, #82210, #85951, .T. ) ;
#58443 = EDGE_CURVE ( 'NONE', #46733, #37203, #90118, .T. ) ;
#58444 = ORIENTED_EDGE ( 'NONE', *, *, #128641, .T. ) ;
#58445 = FACE_BOUND ( 'NONE', #35712, .T. ) ;
#58446 = LINE ( 'NONE', #11275, #15427 ) ;
#58447 = PLANE ( 'NONE',  #74470 ) ;
#58448 = CARTESIAN_POINT ( 'NONE',  ( 184.1500000000000057, 26.96999999999993847, 34.92499999999998295 ) ) ;
#58449 = VECTOR ( 'NONE', #79604, 1000.000000000000000 ) ;
#58450 = CARTESIAN_POINT ( 'NONE',  ( -5.999999999999956479, 12.25461709320620507, -10.07315571508698682 ) ) ;
#58451 = CARTESIAN_POINT ( 'NONE',  ( 34.92499999999998295, 22.22500000000000142, 4.000000000000000000 ) ) ;
#58452 = DIRECTION ( 'NONE',  ( 0.7477445707973130462, 0.5381879072143345155, 0.3888853730489190141 ) ) ;
#58453 = VERTEX_POINT ( 'NONE', #106977 ) ;
#58454 = ORIENTED_EDGE ( 'NONE', *, *, #114859, .T. ) ;
#58455 = CARTESIAN_POINT ( 'NONE',  ( 104.0370968585647802, -3.054999999999998828, -5.291415217122919401 ) ) ;
#58456 = ORIENTED_EDGE ( 'NONE', *, *, #125138, .T. ) ;
#58457 = LINE ( 'NONE', #136663, #113691 ) ;
#58458 = ORIENTED_EDGE ( 'NONE', *, *, #37309, .T. ) ;
#58459 = EDGE_CURVE ( 'NONE', #98731, #81677, #64208, .T. ) ;
#58460 = CARTESIAN_POINT ( 'NONE',  ( 0.000000000000000000, 0.000000000000000000, 5.000000000000000000 ) ) ;
#58461 = CIRCLE ( 'NONE', #86251, 2.500000000000000888 ) ;
#58462 = AXIS2_PLACEMENT_3D ( 'NONE', #100717, #1361, #58692 ) ;
#58463 = VECTOR ( 'NONE', #81222, 1000.000000000000000 ) ;
#58464 = LINE ( 'NONE', #12028, #142765 ) ;
#58465 = EDGE_CURVE ( 'NONE', #141981, #8088, #7656, .T. ) ;
#58467 = EDGE_CURVE ( 'NONE', #129514, #91137, #6198, .T. ) ;
#58466 = CIRCLE ( 'NONE', #51485, 2.055000000000001048 ) ;
#58468 = MECHANICAL_DESIGN_GEOMETRIC_PRESENTATION_REPRESENTATION (  '', ( #35368 ), #130249 ) ;
#58469 = CARTESIAN_POINT ( 'NONE',  ( 25.93003974513575827, -0.7407075233842770334, 13.87443053587604780 ) ) ;
#58470 = ORIENTED_EDGE ( 'NONE', *, *, #137121, .T. ) ;
#58471 = DIRECTION ( 'NONE',  ( -0.7071067811865486830, -0.7071067811865464625, -0.000000000000000000 ) ) ;
#58472 = SURFACE_STYLE_FILL_AREA ( #57720 ) ;
#58473 = FACE_OUTER_BOUND ( 'NONE', #43587, .T. ) ;
#58474 = FACE_OUTER_BOUND ( 'NONE', #139038, .T. ) ;
#58475 = CARTESIAN_POINT ( 'NONE',  ( 12.48921356237309155, -27.52281430457064104, 5.000000000000000000 ) ) ;
#58476 = VECTOR ( 'NONE', #9464, 1000.000000000000114 ) ;
#58477 = AXIS2_PLACEMENT_3D ( 'NONE', #135207, #38021, #71355 ) ;
#58478 = FACE_OUTER_BOUND ( 'NONE', #118574, .T. ) ;
#58479 = ORIENTED_EDGE ( 'NONE', *, *, #117888, .F. ) ;
#58480 = EDGE_CURVE ( 'NONE', #67347, #87818, #116440, .T. ) ;
#58481 = LINE ( 'NONE', #2583, #139889 ) ;
#58482 = CARTESIAN_POINT ( 'NONE',  ( -17.51078643762690845, -27.52281430457043143, 5.000000000000000000 ) ) ;
#58483 = EDGE_LOOP ( 'NONE', ( #78947, #53615, #70083 ) ) ;
#58484 = EDGE_LOOP ( 'NONE', ( #138496, #126193, #76192, #46017 ) ) ;
#58485 = EDGE_CURVE ( 'NONE', #25524, #30424, #50475, .T. ) ;
#58487 = VERTEX_POINT ( 'NONE', #32296 ) ;
#58486 = EDGE_CURVE ( 'NONE', #17176, #115135, #17810, .T. ) ;
#58488 = CARTESIAN_POINT ( 'NONE',  ( 55.27126352523142572, 4.472830434245838482, 4.472830434245842035 ) ) ;
#58489 = ORIENTED_EDGE ( 'NONE', *, *, #54279, .T. ) ;
#58490 = CARTESIAN_POINT ( 'NONE',  ( 4.566639616203772789, 1.633150327867695095, 6.094999999999988205 ) ) ;
#58491 = LINE ( 'NONE', #1852, #137461 ) ;
#58492 = EDGE_CURVE ( 'NONE', #13019, #141546, #100407, .T. ) ;
#58493 = ORIENTED_EDGE ( 'NONE', *, *, #103164, .T. ) ;
#58494 = DIRECTION ( 'NONE',  ( -0.000000000000000000, 0.3543493200069153248, 0.9351131265310292928 ) ) ;
#58495 = ORIENTED_EDGE ( 'NONE', *, *, #91118, .T. ) ;
#58496 = LINE ( 'NONE', #136695, #104348 ) ;
#58497 = EDGE_CURVE ( 'NONE', #102967, #90134, #132349, .T. ) ;
#58498 = CARTESIAN_POINT ( 'NONE',  ( 63.48921356237309510, -27.52281430457099631, 5.000000000000000000 ) ) ;
#58499 = ORIENTED_EDGE ( 'NONE', *, *, #37100, .F. ) ;
#58500 = VECTOR ( 'NONE', #105131, 1000.000000000000227 ) ;
#58501 = LINE ( 'NONE', #70773, #138693 ) ;
#58502 = CARTESIAN_POINT ( 'NONE',  ( -48.18398860626899705, 28.73617430169820608, 5.000000000000000000 ) ) ;
#58503 = ORIENTED_EDGE ( 'NONE', *, *, #16856, .T. ) ;
#58504 = CARTESIAN_POINT ( 'NONE',  ( 13.49999999999990763, -16.53360074219757081, 5.000000000000000000 ) ) ;
#58505 = ORIENTED_EDGE ( 'NONE', *, *, #143117, .T. ) ;
#58506 = VECTOR ( 'NONE', #134609, 1000.000000000000000 ) ;
#58507 = ORIENTED_EDGE ( 'NONE', *, *, #18787, .F. ) ;
#58508 = ORIENTED_EDGE ( 'NONE', *, *, #114779, .T. ) ;
#58509 = CARTESIAN_POINT ( 'NONE',  ( -54.29974487139159578, -27.71228299555243879, 4.000000000000000000 ) ) ;
#58510 = VECTOR ( 'NONE', #63721, 1000.000000000000227 ) ;
#58511 = PLANE ( 'NONE',  #19118 ) ;
#58512 = CARTESIAN_POINT ( 'NONE',  ( 53.99451991528749062, 28.92564299267975869, 4.000000000000000000 ) ) ;
#58513 = FACE_OUTER_BOUND ( 'NONE', #62842, .T. ) ;
#58514 = CARTESIAN_POINT ( 'NONE',  ( 14.81601139373099585, 28.73617430169776910, 5.000000000000000000 ) ) ;
#58515 = ORIENTED_EDGE ( 'NONE', *, *, #97353, .F. ) ;
#58516 = EDGE_CURVE ( 'NONE', #18784, #11268, #88098, .T. ) ;
#58517 = FACE_OUTER_BOUND ( 'NONE', #88990, .T. ) ;
#58518 = EDGE_CURVE ( 'NONE', #17485, #130029, #45339, .T. ) ;
#58519 = EDGE_CURVE ( 'NONE', #78029, #5674, #99664, .T. ) ;
#58520 = CARTESIAN_POINT ( 'NONE',  ( 26.52040314143521726, 7.934999999999989839, -2.126176841940961904 ) ) ;
#58521 = DIRECTION ( 'NONE',  ( 1.000000000000000000, 0.000000000000000000, 0.000000000000000000 ) ) ;
#58522 = CARTESIAN_POINT ( 'NONE',  ( 4.658131166821905644, -2.500000000000000444, 0.000000000000000000 ) ) ;
#58523 = DIRECTION ( 'NONE',  ( 0.5735764363510453823, -0.8191520442889923537, 1.003171929053525486E-16 ) ) ;
#58524 = ORIENTED_EDGE ( 'NONE', *, *, #112617, .T. ) ;
#58525 = ORIENTED_EDGE ( 'NONE', *, *, #63146, .F. ) ;
#58526 = AXIS2_PLACEMENT_3D ( 'NONE', #104727, #61286, #128633 ) ;
#58527 = EDGE_LOOP ( 'NONE', ( #60234, #64620, #32326, #136508 ) ) ;
#58528 = CARTESIAN_POINT ( 'NONE',  ( 14.29298673570684919, -21.74070752338406365, 4.999753212805221558 ) ) ;
#58529 = LINE ( 'NONE', #113543, #99701 ) ;
#58530 = VECTOR ( 'NONE', #47672, 1000.000000000000114 ) ;
#58531 = LINE ( 'NONE', #2640, #49776 ) ;
#58532 = EDGE_CURVE ( 'NONE', #82772, #101759, #85449, .T. ) ;
#58533 = DIRECTION ( 'NONE',  ( 0.000000000000000000, 1.000000000000000000, 0.000000000000000000 ) ) ;
#58534 = CARTESIAN_POINT ( 'NONE',  ( 5.978975958053759143, 9.486554164729072980, 0.5799792595215604862 ) ) ;
#58535 = FACE_OUTER_BOUND ( 'NONE', #28145, .T. ) ;
#58536 =( BOUNDED_CURVE ( )  B_SPLINE_CURVE ( 2, ( #65162, #88332, #122346, #78171, #54295, #23023, #107891, #52804, #99904, #87603, #110049, #131115, #33271 ),
 .UNSPECIFIED., .F., .F. ) 
 B_SPLINE_CURVE_WITH_KNOTS ( ( 3, 2, 2, 2, 2, 2, 3 ),
 ( 0.4166666666666666852, 0.4194444444444444531, 0.4222222222222222210, 0.4249999999999999889, 0.4277777777777777568, 0.4305555555555555802, 0.4333333333333333481 ),
 .UNSPECIFIED. ) 
 CURVE ( )  GEOMETRIC_REPRESENTATION_ITEM ( )  RATIONAL_B_SPLINE_CURVE ( ( 1.000000000000000000, 0.9659258262890683122, 1.000000000000000000, 0.9659258262890683122, 1.000000000000000000, 0.9659258262890683122, 1.000000000000000000, 0.9659258262890683122, 1.000000000000000000, 0.9659258262890683122, 1.000000000000000000, 0.9659258262890683122, 1.000000000000000000 ) ) 
 REPRESENTATION_ITEM ( '' )  );
#58537 = CARTESIAN_POINT ( 'NONE',  ( -10.82816939922344979, -8.240707523384198652, 4.000000000000000000 ) ) ;
#58538 = LINE ( 'NONE', #93955, #20037 ) ;
#58539 = CARTESIAN_POINT ( 'NONE',  ( 0.000000000000000000, 0.000000000000000000, 5.000000000000000000 ) ) ;
#58540 = LINE ( 'NONE', #116957, #81388 ) ;
#58541 = DIRECTION ( 'NONE',  ( 0.000000000000000000, -1.000000000000000000, 0.000000000000000000 ) ) ;
#58542 = ORIENTED_EDGE ( 'NONE', *, *, #30221, .T. ) ;
#58543 = VECTOR ( 'NONE', #91041, 1000.000000000000000 ) ;
#58544 = LINE ( 'NONE', #102712, #61502 ) ;
#58545 = ORIENTED_EDGE ( 'NONE', *, *, #17898, .F. ) ;
#58546 =( BOUNDED_CURVE ( )  B_SPLINE_CURVE ( 2, ( #58411, #125772, #35207, #80142, #79449, #68545, #26445, #35922, #13394, #2514, #114844, #102594, #101856 ),
 .UNSPECIFIED., .F., .T. ) 
 B_SPLINE_CURVE_WITH_KNOTS ( ( 3, 2, 2, 2, 2, 2, 3 ),
 ( 0.3833333333333334147, 0.3861111111111111827, 0.3888888888888889506, 0.3916666666666667185, 0.3944444444444444864, 0.3972222222222222543, 0.4000000000000000777 ),
 .UNSPECIFIED. ) 
 CURVE ( )  GEOMETRIC_REPRESENTATION_ITEM ( )  RATIONAL_B_SPLINE_CURVE ( ( 0.9999999999999993339, 0.9659258262890689783, 1.000000000000000000, 0.9659258262890683122, 1.000000000000000000, 0.9659258262890683122, 1.000000000000000000, 0.9659258262890683122, 1.000000000000000000, 0.9659258262890683122, 1.000000000000000000, 0.9659258262890676461, 1.000000000000000666 ) ) 
 REPRESENTATION_ITEM ( '' )  );
#58547 = DIRECTION ( 'NONE',  ( 1.000000000000000000, 0.000000000000000000, 0.000000000000000000 ) ) ;
#58549 = ORIENTED_EDGE ( 'NONE', *, *, #37249, .T. ) ;
#58548 = CARTESIAN_POINT ( 'NONE',  ( 18.72281430457046270, -21.72500000000000142, 5.000000000000000000 ) ) ;
#58550 = DIRECTION ( 'NONE',  ( 0.000000000000000000, 1.000000000000000000, 0.000000000000000000 ) ) ;
#58551 = FACE_OUTER_BOUND ( 'NONE', #12355, .T. ) ;
#58552 = ORIENTED_EDGE ( 'NONE', *, *, #120443, .F. ) ;
#58553 = LINE ( 'NONE', #91147, #41569 ) ;
#58555 = ORIENTED_EDGE ( 'NONE', *, *, #28457, .T. ) ;
#58554 = CIRCLE ( 'NONE', #63080, 2.055000000000000604 ) ;
#58556 = LINE ( 'NONE', #6207, #442 ) ;
#58557 = ORIENTED_EDGE ( 'NONE', *, *, #54175, .F. ) ;
#58558 = CARTESIAN_POINT ( 'NONE',  ( -24.48921356237309510, -27.52281430457072631, 5.000000000000000000 ) ) ;
#58559 = CARTESIAN_POINT ( 'NONE',  ( 99.24586038379624142, 3.974999999999996980, 6.884901960086287964 ) ) ;
#58560 = CARTESIAN_POINT ( 'NONE',  ( 8.816011393731004731, 28.73617430169781173, 5.000000000000000000 ) ) ;
#58561 = LINE ( 'NONE', #44823, #126946 ) ;
#58562 = EDGE_LOOP ( 'NONE', ( #133826, #131705, #35025, #133061 ) ) ;
#58563 = CARTESIAN_POINT ( 'NONE',  ( 22.49999999999984368, -10.04351517176476172, -1.623559851933770171 ) ) ;
#58564 = PLANE ( 'NONE',  #119052 ) ;
#58565 = ADVANCED_FACE ( 'NONE', ( #340 ), #78649, .T. ) ;
#58566 = CARTESIAN_POINT ( 'NONE',  ( 13.92145407031093818, 4.584330080086930965E-16, 0.000000000000000000 ) ) ;
#58567 = CARTESIAN_POINT ( 'NONE',  ( 24.93750000000000000, -4.461849672132299105, 4.461849672132299993 ) ) ;
#58568 = CARTESIAN_POINT ( 'NONE',  ( -8.999999999999934275, -9.033600742197648970, 5.000000000000000000 ) ) ;
#58569 = AXIS2_PLACEMENT_3D ( 'NONE', #118355, #73456, #127845 ) ;
#58570 = COLOUR_RGB ( '', 0.66274510, 0.83137255, 0.94901961) ;
#58571 = DIRECTION ( 'NONE',  ( 0.7071067811865487940, 0.7071067811865463515, 0.000000000000000000 ) ) ;
#58572 = EDGE_LOOP ( 'NONE', ( #134959, #123301, #70873, #3434, #21677, #139604 ) ) ;
#58573 = AXIS2_PLACEMENT_3D ( 'NONE', #138523, #119586, #18862 ) ;
#58574 = VECTOR ( 'NONE', #16300, 1000.000000000000000 ) ;
#58575 = FACE_OUTER_BOUND ( 'NONE', #43717, .T. ) ;
#58576 = VERTEX_POINT ( 'NONE', #21415 ) ;
#58577 = CARTESIAN_POINT ( 'NONE',  ( 94.20876352523144703, -7.482591942790329030E-16, 6.110000000000001208 ) ) ;
#58578 = PLANE ( 'NONE',  #50124 ) ;
#58579 = MECHANICAL_DESIGN_GEOMETRIC_PRESENTATION_REPRESENTATION (  '', ( #40037 ), #23628 ) ;
#58581 = AXIS2_PLACEMENT_3D ( 'NONE', #79616, #33243, #91176 ) ;
#58580 = CARTESIAN_POINT ( 'NONE',  ( 28.49999999999980105, -12.66682484999663671, -0.6294897503863281507 ) ) ;
#58582 = FACE_OUTER_BOUND ( 'NONE', #83971, .T. ) ;
#58583 = ORIENTED_EDGE ( 'NONE', *, *, #99089, .T. ) ;
#58584 = EDGE_CURVE ( 'NONE', #36068, #110646, #44637, .T. ) ;
#58585 = DIRECTION ( 'NONE',  ( -0.000000000000000000, -0.3543493200069152693, 0.9351131265310292928 ) ) ;
#58586 = VERTEX_POINT ( 'NONE', #10508 ) ;
#58587 = CARTESIAN_POINT ( 'NONE',  ( 6.471592354503322042, -3.851859888774471706E-31, 2.500000000000001332 ) ) ;
#58588 = ADVANCED_FACE ( 'NONE', ( #34425 ), #43887, .F. ) ;
#58590 = ORIENTED_EDGE ( 'NONE', *, *, #118641, .T. ) ;
#58589 = LINE ( 'NONE', #91188, #126201 ) ;
#58591 = FACE_OUTER_BOUND ( 'NONE', #45548, .T. ) ;
#58592 = CARTESIAN_POINT ( 'NONE',  ( 4.499999999999968914, -12.66682484999666158, -0.6294897503863827737 ) ) ;
#58593 = LINE ( 'NONE', #125220, #16895 ) ;
#58594 = EDGE_CURVE ( 'NONE', #52857, #60630, #64926, .T. ) ;
#58596 = EDGE_CURVE ( 'NONE', #62444, #10426, #75803, .T. ) ;
#58595 = VERTEX_POINT ( 'NONE', #31578 ) ;
#58597 = ORIENTED_EDGE ( 'NONE', *, *, #9473, .F. ) ;
#58598 = VERTEX_POINT ( 'NONE', #33039 ) ;
#58599 = CARTESIAN_POINT ( 'NONE',  ( 85.60459685856478984, 1.637169565754164946, -6.109999999999999432 ) ) ;
#58600 = AXIS2_PLACEMENT_3D ( 'NONE', #139640, #30863, #141011 ) ;
#58601 = ORIENTED_EDGE ( 'NONE', *, *, #54833, .T. ) ;
#58602 = ADVANCED_FACE ( 'NONE', ( #9808 ), #98264, .T. ) ;
#58603 = DIRECTION ( 'NONE',  ( -1.000000000000000000, -0.000000000000000000, -0.000000000000000000 ) ) ;
#58604 = CARTESIAN_POINT ( 'NONE',  ( -66.29974487139159578, -27.71228299555252406, 4.000000000000000000 ) ) ;
#58605 = DIRECTION ( 'NONE',  ( -0.7071067811865486830, 0.7071067811865464625, 0.000000000000000000 ) ) ;
#58606 = CARTESIAN_POINT ( 'NONE',  ( 29.99451991528749417, 28.92564299267958816, 4.000000000000000000 ) ) ;
#58607 = VERTEX_POINT ( 'NONE', #88827 ) ;
#58608 = DIRECTION ( 'NONE',  ( -0.6830127018922181881, 0.6830127018922202975, -0.2588190451025214056 ) ) ;
#58609 = CARTESIAN_POINT ( 'NONE',  ( 39.85005128541000374, -8.240707523384182664, 17.25253755692248347 ) ) ;
#58610 = AXIS2_PLACEMENT_3D ( 'NONE', #4887, #35467, #15758 ) ;
#58611 = EDGE_CURVE ( 'NONE', #65308, #73841, #55375, .T. ) ;
#58612 = CARTESIAN_POINT ( 'NONE',  ( 28.11017322888191217, -22.22500000000000142, 4.785647885939353863 ) ) ;
#58613 = CARTESIAN_POINT ( 'NONE',  ( 77.64126352523146579, 4.472830434245836706, 4.472830434245840259 ) ) ;
#58614 = VERTEX_POINT ( 'NONE', #121422 ) ;
#58615 = STYLED_ITEM ( 'NONE', ( #42441 ), #86209 ) ;
#58616 = DIRECTION ( 'NONE',  ( 0.7071067811865487940, -0.7071067811865463515, 0.000000000000000000 ) ) ;
#58617 = EDGE_CURVE ( 'NONE', #73381, #38444, #122503, .T. ) ;
#58618 = DIRECTION ( 'NONE',  ( 0.6830127018922181881, 0.6830127018922202975, -0.2588190451025214056 ) ) ;
#58619 = CARTESIAN_POINT ( 'NONE',  ( 60.48921356237309510, -27.52281430457097500, 5.000000000000000000 ) ) ;
#58620 = AXIS2_PLACEMENT_3D ( 'NONE', #45554, #112216, #78160 ) ;
#58621 = EDGE_CURVE ( 'NONE', #116708, #7217, #110528, .T. ) ;
#58622 = ORIENTED_EDGE ( 'NONE', *, *, #126643, .F. ) ;
#58623 = ORIENTED_EDGE ( 'NONE', *, *, #15017, .F. ) ;
#58624 = CARTESIAN_POINT ( 'NONE',  ( 65.31250000000000000, 5.819803920172571310, 5.819803920172576639 ) ) ;
#58625 = DIRECTION ( 'NONE',  ( -0.3543493200069162685, -0.000000000000000000, -0.9351131265310288487 ) ) ;
#58626 = CARTESIAN_POINT ( 'NONE',  ( 22.37956980810188767, 3.967499999999998916, 6.871911579029510442 ) ) ;
#58627 = CARTESIAN_POINT ( 'NONE',  ( -7.171830600776425868, -20.24070752338407786, 4.000000000000000000 ) ) ;
#58628 = EDGE_CURVE ( 'NONE', #69257, #130179, #55480, .T. ) ;
#58629 = FILL_AREA_STYLE ('',( #123129 ) ) ;
#58630 = CARTESIAN_POINT ( 'NONE',  ( -21.29974487139158512, -27.71228299555221142, 4.000000000000000000 ) ) ;
#58631 = VECTOR ( 'NONE', #73293, 999.9999999999998863 ) ;
#58632 = DIRECTION ( 'NONE',  ( -0.7071067811865486830, 0.7071067811865464625, 0.000000000000000000 ) ) ;
#58633 =( NAMED_UNIT ( * ) SI_UNIT ( $, .STERADIAN. ) SOLID_ANGLE_UNIT ( ) );
#58634 = EDGE_LOOP ( 'NONE', ( #103445, #132115, #91752, #142446 ) ) ;
#58635 = ORIENTED_EDGE ( 'NONE', *, *, #13230, .F. ) ;
#58636 = DIRECTION ( 'NONE',  ( -0.7071067811865486830, -0.7071067811865464625, -0.000000000000000000 ) ) ;
#58637 = ORIENTED_EDGE ( 'NONE', *, *, #46870, .F. ) ;
#58638 = VECTOR ( 'NONE', #23626, 1000.000000000000000 ) ;
#58639 = ADVANCED_FACE ( 'NONE', ( #122129 ), #56226, .T. ) ;
#58640 = AXIS2_PLACEMENT_3D ( 'NONE', #19812, #8882, #61931 ) ;
#58641 = EDGE_CURVE ( 'NONE', #80628, #13922, #59077, .T. ) ;
#58642 = FACE_OUTER_BOUND ( 'NONE', #64561, .T. ) ;
#58643 = ORIENTED_EDGE ( 'NONE', *, *, #23556, .T. ) ;
#58644 = CARTESIAN_POINT ( 'NONE',  ( 56.95419371712956291, 6.884901960086283523, 3.975000000000002753 ) ) ;
#58645 = CARTESIAN_POINT ( 'NONE',  ( -34.49999999999975842, -11.56887692260769640, 4.000000000000000000 ) ) ;
#58646 = EDGE_CURVE ( 'NONE', #83534, #23652, #126412, .T. ) ;
#58647 = DIRECTION ( 'NONE',  ( -0.5735764363510503783, -0.8191520442889886899, 0.000000000000000000 ) ) ;
#58648 = VECTOR ( 'NONE', #1568, 1000.000000000000000 ) ;
#58649 = DIRECTION ( 'NONE',  ( -0.7071067811865486830, -0.7071067811865464625, 0.000000000000000000 ) ) ;
#58650 = ORIENTED_EDGE ( 'NONE', *, *, #58611, .T. ) ;
#58651 = ADVANCED_FACE ( 'NONE', ( #91656 ), #46787, .F. ) ;
#58652 = CARTESIAN_POINT ( 'NONE',  ( 7.720000000000001528, 9.521314400968980422E-16, 0.000000000000000000 ) ) ;
#58653 = DIRECTION ( 'NONE',  ( 1.000000000000000000, 1.224606353822377258E-16, 0.000000000000000000 ) ) ;
#58654 = ORIENTED_EDGE ( 'NONE', *, *, #107183, .F. ) ;
#58655 = DIRECTION ( 'NONE',  ( -0.7071067811865486830, 0.7071067811865464625, 0.000000000000000000 ) ) ;
#58656 = ORIENTED_EDGE ( 'NONE', *, *, #26350, .F. ) ;
#58657 = ORIENTED_EDGE ( 'NONE', *, *, #56967, .T. ) ;
#58658 = CARTESIAN_POINT ( 'NONE',  ( 17.29289321881334018, 17.25929247661554911, 5.000000000000000000 ) ) ;
#58659 = ORIENTED_EDGE ( 'NONE', *, *, #138161, .T. ) ;
#58660 = ORIENTED_EDGE ( 'NONE', *, *, #43030, .T. ) ;
#58661 = DIRECTION ( 'NONE',  ( -0.7071067811865486830, -0.7071067811865464625, 0.000000000000000000 ) ) ;
#58662 = ORIENTED_EDGE ( 'NONE', *, *, #39800, .T. ) ;
#58663 = LINE ( 'NONE', #14380, #120614 ) ;
#58664 = LINE ( 'NONE', #57208, #125943 ) ;
#58665 = CARTESIAN_POINT ( 'NONE',  ( 116.5212635252314612, -4.472830434245838482, -4.472830434245840259 ) ) ;
#58666 = DIRECTION ( 'NONE',  ( -0.7071067811865486830, -0.7071067811865464625, 0.000000000000000000 ) ) ;
#58667 = EDGE_CURVE ( 'NONE', #98685, #128930, #47493, .T. ) ;
#58668 = DIRECTION ( 'NONE',  ( -0.000000000000000000, 0.3543493200069153248, 0.9351131265310292928 ) ) ;
#58669 = CARTESIAN_POINT ( 'NONE',  ( -22.49999999999984368, -2.947814304570797184, 5.000000000000000000 ) ) ;
#58670 = VECTOR ( 'NONE', #21013, 1000.000000000000227 ) ;
#58671 = EDGE_CURVE ( 'NONE', #27773, #51825, #125734, .T. ) ;
#58672 = DIRECTION ( 'NONE',  ( 1.000000000000000000, 0.000000000000000000, 0.000000000000000000 ) ) ;
#58673 = VECTOR ( 'NONE', #102311, 1000.000000000000000 ) ;
#58674 = ORIENTED_EDGE ( 'NONE', *, *, #52687, .T. ) ;
#58675 = LINE ( 'NONE', #123893, #13286 ) ;
#58676 = PLANE ( 'NONE',  #26793 ) ;
#58677 = ORIENTED_EDGE ( 'NONE', *, *, #89015, .T. ) ;
#58678 = ORIENTED_EDGE ( 'NONE', *, *, #90641, .T. ) ;
#58679 = VECTOR ( 'NONE', #13229, 1000.000000000000000 ) ;
#58680 = AXIS2_PLACEMENT_3D ( 'NONE', #134549, #114194, #100486 ) ;
#58681 = CARTESIAN_POINT ( 'NONE',  ( -14.99999999999989342, -13.97847968911261596, -0.1324546996127147214 ) ) ;
#58682 = ORIENTED_EDGE ( 'NONE', *, *, #7843, .F. ) ;
#58683 = VECTOR ( 'NONE', #22721, 1000.000000000000000 ) ;
#58684 = CARTESIAN_POINT ( 'NONE',  ( -3.299744871391591339, -27.71228299555208352, 4.000000000000000000 ) ) ;
#58685 = CARTESIAN_POINT ( 'NONE',  ( 9.831811731255163167, 22.22500000000000142, 21.96002906245333008 ) ) ;
#58686 = PLANE ( 'NONE',  #9202 ) ;
#58687 = CARTESIAN_POINT ( 'NONE',  ( 3.707106781186521705, -6.740707523384207533, 5.000000000000000000 ) ) ;
#58688 = ADVANCED_FACE ( 'NONE', ( #103927 ), #35168, .T. ) ;
#58689 = ORIENTED_EDGE ( 'NONE', *, *, #4006, .F. ) ;
#58690 = LINE ( 'NONE', #123906, #13966 ) ;
#58691 = EDGE_LOOP ( 'NONE', ( #125326, #41688, #112226, #118090 ) ) ;
#58692 = DIRECTION ( 'NONE',  ( 0.000000000000000000, -1.000000000000000000, 0.000000000000000000 ) ) ;
#58693 = EDGE_CURVE ( 'NONE', #87786, #108114, #4576, .T. ) ;
#58694 = VECTOR ( 'NONE', #103744, 1000.000000000000000 ) ;
#58695 = CARTESIAN_POINT ( 'NONE',  ( 25.58790314143521982, 6.871911579029515771, 3.967499999999989146 ) ) ;
#58696 = VERTEX_POINT ( 'NONE', #103234 ) ;
#58697 = CARTESIAN_POINT ( 'NONE',  ( 1.042387978378689350, 2.055000000000001048, 0.000000000000000000 ) ) ;
#58698 = FACE_OUTER_BOUND ( 'NONE', #66158, .T. ) ;
#58699 = VERTEX_POINT ( 'NONE', #137318 ) ;
#58700 = ORIENTED_EDGE ( 'NONE', *, *, #133673, .T. ) ;
#58701 = EDGE_LOOP ( 'NONE', ( #122353, #111790, #117083, #31124 ) ) ;
#58702 = LINE ( 'NONE', #25282, #130633 ) ;
#58703 = FACE_OUTER_BOUND ( 'NONE', #123008, .T. ) ;
#58704 = LINE ( 'NONE', #125332, #102964 ) ;
#58705 = CARTESIAN_POINT ( 'NONE',  ( -27.48921356237309155, -27.52281430457074762, 5.000000000000000000 ) ) ;
#58706 = VERTEX_POINT ( 'NONE', #2473 ) ;
#58707 = VECTOR ( 'NONE', #112120, 1000.000000000000000 ) ;
#58708 = DIRECTION ( 'NONE',  ( -0.6830127018922180770, -0.6830127018922204085, -0.2588190451025213501 ) ) ;
#58709 = CARTESIAN_POINT ( 'NONE',  ( 28.00000000000002487, -49.14999999999999147, -62.92499999999978400 ) ) ;
#58710 = EDGE_CURVE ( 'NONE', #4252, #108455, #70658, .T. ) ;
#58711 = VECTOR ( 'NONE', #93761, 1000.000000000000227 ) ;
#58712 = LINE ( 'NONE', #26728, #7151 ) ;
#58713 = DIRECTION ( 'NONE',  ( 0.7071067811865487940, 0.7071067811865463515, 0.000000000000000000 ) ) ;
#58714 = ORIENTED_EDGE ( 'NONE', *, *, #126843, .T. ) ;
#58715 = CARTESIAN_POINT ( 'NONE',  ( -25.39999999999996305, 0.000000000000000000, 2.500000000000000000 ) ) ;
#58716 = VERTEX_POINT ( 'NONE', #37284 ) ;
#58717 = VECTOR ( 'NONE', #140297, 1000.000000000000000 ) ;
#58719 = VERTEX_POINT ( 'NONE', #114803 ) ;
#58718 = DIRECTION ( 'NONE',  ( -0.6830127018922180770, -0.6830127018922204085, -0.2588190451025213501 ) ) ;
#58720 = EDGE_LOOP ( 'NONE', ( #140974, #13582, #37891, #106139 ) ) ;
#58721 = EDGE_CURVE ( 'NONE', #40729, #128263, #80799, .T. ) ;
#58722 = FACE_OUTER_BOUND ( 'NONE', #127592, .T. ) ;
#58723 = FACE_OUTER_BOUND ( 'NONE', #78685, .T. ) ;
#58724 = ORIENTED_EDGE ( 'NONE', *, *, #112424, .T. ) ;
#58725 = PLANE ( 'NONE',  #104567 ) ;
#58726 = ORIENTED_EDGE ( 'NONE', *, *, #90691, .T. ) ;
#58727 =( BOUNDED_CURVE ( )  B_SPLINE_CURVE ( 3, ( #8343, #98259, #7649, #19261 ),
 .UNSPECIFIED., .F., .T. ) 
 B_SPLINE_CURVE_WITH_KNOTS ( ( 4, 4 ),
 ( 5.255487504216517003, 5.308805501018120765 ),
 .UNSPECIFIED. ) 
 CURVE ( )  GEOMETRIC_REPRESENTATION_ITEM ( )  RATIONAL_B_SPLINE_CURVE ( ( 1.000000000000000000, 0.9997631132982454094, 0.9997631132982454094, 1.000000000000000000 ) ) 
 REPRESENTATION_ITEM ( '' )  );
#58728 = VECTOR ( 'NONE', #117053, 1000.000000000000000 ) ;
#58729 = LINE ( 'NONE', #84023, #54521 ) ;
#58730 = LINE ( 'NONE', #111626, #48555 ) ;
#58731 = PLANE ( 'NONE',  #36899 ) ;
#58732 = LINE ( 'NONE', #23153, #127165 ) ;
#58733 =( LENGTH_UNIT ( ) NAMED_UNIT ( * ) SI_UNIT ( .MILLI., .METRE. ) );
#58734 = DIRECTION ( 'NONE',  ( 0.7071067811865486830, -0.7071067811865464625, -0.000000000000000000 ) ) ;
#58735 = CARTESIAN_POINT ( 'NONE',  ( -56.99451991528749062, 28.92564299267978001, 4.000000000000000000 ) ) ;
#58736 = CARTESIAN_POINT ( 'NONE',  ( 24.04123647476855652, 0.000000000000000000, 7.934999999999990727 ) ) ;
#58737 = CARTESIAN_POINT ( 'NONE',  ( 0.7071067811865406894, 14.25929247661556865, 5.000000000000000000 ) ) ;
#58738 = CIRCLE ( 'NONE', #49513, 2.500000000000000888 ) ;
#58739 = CARTESIAN_POINT ( 'NONE',  ( -51.48921356237309510, -27.52281430457091460, 5.000000000000000000 ) ) ;
#58740 = CARTESIAN_POINT ( 'NONE',  ( -42.48921356237308800, -27.52281430457085065, 5.000000000000000000 ) ) ;
#58741 = DIRECTION ( 'NONE',  ( 0.7071067811865487940, -0.7071067811865463515, 0.000000000000000000 ) ) ;
#58742 = ORIENTED_EDGE ( 'NONE', *, *, #15182, .F. ) ;
#58743 = ORIENTED_EDGE ( 'NONE', *, *, #73760, .T. ) ;
#58744 = CARTESIAN_POINT ( 'NONE',  ( 94.91666666666665719, -6.884901960086287076, -3.975000000000000977 ) ) ;
#58745 = VERTEX_POINT ( 'NONE', #15483 ) ;
#58746 = ORIENTED_EDGE ( 'NONE', *, *, #17418, .F. ) ;
#58747 = EDGE_CURVE ( 'NONE', #32976, #12574, #134464, .T. ) ;
#58748 = EDGE_CURVE ( 'NONE', #97422, #139654, #26412, .T. ) ;
#58749 = DIRECTION ( 'NONE',  ( 0.000000000000000000, 0.3543493200069153248, 0.9351131265310291818 ) ) ;
#58750 = VECTOR ( 'NONE', #79479, 1000.000000000000000 ) ;
#58751 = CYLINDRICAL_SURFACE ( 'NONE', #138038, 7.950000000000000178 ) ;
#58752 = ORIENTED_EDGE ( 'NONE', *, *, #85443, .F. ) ;
#58753 = CARTESIAN_POINT ( 'NONE',  ( -25.49999999999981881, 16.08746187583908238, 4.000000000000000000 ) ) ;
#58754 = LINE ( 'NONE', #79062, #11663 ) ;
#58755 = DIRECTION ( 'NONE',  ( 0.6830127018922181881, 0.6830127018922202975, -0.2588190451025214056 ) ) ;
#58756 = CARTESIAN_POINT ( 'NONE',  ( 125.8772101740147917, 2.453750636162616239, -7.181886997138566819 ) ) ;
#58757 = EDGE_CURVE ( 'NONE', #95983, #16, #79411, .T. ) ;
#58758 = EDGE_CURVE ( 'NONE', #38910, #142123, #124998, .T. ) ;
#58759 = DIRECTION ( 'NONE',  ( -0.000000000000000000, 0.000000000000000000, 1.000000000000000000 ) ) ;
#58761 = AXIS2_PLACEMENT_3D ( 'NONE', #13398, #135237, #12693 ) ;
#58760 = DIRECTION ( 'NONE',  ( -0.3543493200069163795, -9.265275131829747941E-33, -0.9351131265310288487 ) ) ;
#58762 = CARTESIAN_POINT ( 'NONE',  ( -0.2997448713915885632, -27.71228299555206220, 4.000000000000000000 ) ) ;
#58763 = CARTESIAN_POINT ( 'NONE',  ( 10.15640092694706453, 3.821174125832445049E-16, 0.000000000000000000 ) ) ;
#58764 = DIRECTION ( 'NONE',  ( 0.000000000000000000, -1.000000000000000000, 0.000000000000000000 ) ) ;
#58765 = PLANE ( 'NONE',  #103153 ) ;
#58766 = CARTESIAN_POINT ( 'NONE',  ( 55.56056557994607914, -52.00875322212550600, 39.86617647058822200 ) ) ;
#58767 = EDGE_CURVE ( 'NONE', #132252, #85524, #25677, .T. ) ;
#58768 = ADVANCED_FACE ( 'NONE', ( #114121 ), #123609, .F. ) ;
#58769 = ORIENTED_EDGE ( 'NONE', *, *, #22321, .F. ) ;
#58770 = ORIENTED_EDGE ( 'NONE', *, *, #131545, .F. ) ;
#58771 = CARTESIAN_POINT ( 'NONE',  ( 113.0212635252314186, -4.472830434245839371, -4.472830434245840259 ) ) ;
#58772 = VECTOR ( 'NONE', #119377, 999.9999999999998863 ) ;
#58773 = EDGE_CURVE ( 'NONE', #5681, #94085, #40847, .T. ) ;
#58774 = ORIENTED_EDGE ( 'NONE', *, *, #93606, .T. ) ;
#58775 = ADVANCED_FACE ( 'NONE', ( #95932 ), #85057, .F. ) ;
#58776 = CARTESIAN_POINT ( 'NONE',  ( 99.58333333333332860, 6.884901960086290629, -3.974999999999994316 ) ) ;
#58777 = ADVANCED_FACE ( 'NONE', ( #49620 ), #28557, .F. ) ;
#58778 = DIRECTION ( 'NONE',  ( -1.000000000000000000, 1.248002500702738701E-15, 0.000000000000000000 ) ) ;
#58779 = VERTEX_POINT ( 'NONE', #29244 ) ;
#58780 = CARTESIAN_POINT ( 'NONE',  ( 13.13598696172163116, 0.000000000000000000, 2.500000000000000444 ) ) ;
#58782 = AXIS2_PLACEMENT_3D ( 'NONE', #123145, #67333, #89766 ) ;
#58781 = CARTESIAN_POINT ( 'NONE',  ( -31.49999999999977973, -8.568876922607721269, 4.000000000000000000 ) ) ;
#58783 = ADVANCED_FACE ( 'NONE', ( #61230 ), #95214, .T. ) ;
#58784 = CARTESIAN_POINT ( 'NONE',  ( 108.5579301918980946, 6.110000000000000320, -1.637169565754156064 ) ) ;
#58785 = ORIENTED_EDGE ( 'NONE', *, *, #133178, .F. ) ;
#58786 = EDGE_LOOP ( 'NONE', ( #56482, #40758, #140997, #137888 ) ) ;
#58787 = CARTESIAN_POINT ( 'NONE',  ( 23.20710678118638270, -5.240707523384235955, 5.000000000000000000 ) ) ;
#58788 = DIRECTION ( 'NONE',  ( 0.7071067811865487940, 0.7071067811865463515, 0.000000000000000000 ) ) ;
#58789 = CARTESIAN_POINT ( 'NONE',  ( 98.70833333333332860, -3.974999999999999201, -6.884901960086287964 ) ) ;
#58790 = EDGE_CURVE ( 'NONE', #33966, #87892, #61909, .T. ) ;
#58791 = VERTEX_POINT ( 'NONE', #85766 ) ;
#58792 = ORIENTED_EDGE ( 'NONE', *, *, #143166, .F. ) ;
#58793 = ORIENTED_EDGE ( 'NONE', *, *, #88181, .T. ) ;
#58794 = DIRECTION ( 'NONE',  ( -1.000000000000000000, 0.000000000000000000, -0.000000000000000000 ) ) ;
#58795 =( NAMED_UNIT ( * ) PLANE_ANGLE_UNIT ( ) SI_UNIT ( $, .RADIAN. ) );
#58797 = EDGE_CURVE ( 'NONE', #11322, #132762, #6030, .T. ) ;
#58796 = VECTOR ( 'NONE', #40423, 1000.000000000000000 ) ;
#58798 = VECTOR ( 'NONE', #76718, 1000.000000000000000 ) ;
#58799 = DIRECTION ( 'NONE',  ( -1.000000000000000000, 0.000000000000000000, 0.000000000000000000 ) ) ;
#58800 = EDGE_LOOP ( 'NONE', ( #118493, #18831, #27401, #18518 ) ) ;
#58801 = EDGE_LOOP ( 'NONE', ( #143549, #127194, #102267, #68386 ) ) ;
#58802 = DIRECTION ( 'NONE',  ( 0.000000000000000000, -1.000000000000000000, 0.000000000000000000 ) ) ;
#58803 = EDGE_LOOP ( 'NONE', ( #73315, #94126, #61483, #6327 ) ) ;
#58804 = ORIENTED_EDGE ( 'NONE', *, *, #84800, .T. ) ;
#58805 = AXIS2_PLACEMENT_3D ( 'NONE', #39386, #106742, #95882 ) ;
#58806 = FACE_OUTER_BOUND ( 'NONE', #70636, .T. ) ;
#58807 = EDGE_CURVE ( 'NONE', #22013, #38542, #116969, .T. ) ;
#58808 = PLANE ( 'NONE',  #123984 ) ;
#58809 = LINE ( 'NONE', #126836, #95160 ) ;
#58810 = VERTEX_POINT ( 'NONE', #6734 ) ;
#58811 = VECTOR ( 'NONE', #87875, 1000.000000000000000 ) ;
#58812 = DIRECTION ( 'NONE',  ( 1.000000000000000000, 0.000000000000000000, 0.000000000000000000 ) ) ;
#58813 = B_SPLINE_CURVE_WITH_KNOTS ( 'NONE', 3,
 ( #35568, #111663, #25348, #91359, #135566, #36249, #66731, #23945, #13032, #89200 ),
 .UNSPECIFIED., .F., .F.,
 ( 4, 2, 2, 2, 4 ),
 ( 0.0007022386915571705726, 0.002041165551483828822, 0.003380092411410488048, 0.004719019271337147707, 0.006057946131263806933 ),
 .UNSPECIFIED. ) ;
#58814 = EDGE_CURVE ( 'NONE', #38978, #94114, #38708, .T. ) ;
#58815 = ADVANCED_FACE ( 'NONE', ( #129998 ), #30707, .F. ) ;
#58816 = VECTOR ( 'NONE', #126384, 1000.000000000000000 ) ;
#58817 = FACE_BOUND ( 'NONE', #22034, .T. ) ;
#58818 = ORIENTED_EDGE ( 'NONE', *, *, #44082, .F. ) ;
#58819 = DIRECTION ( 'NONE',  ( 0.7071067811865487940, 0.7071067811865463515, -0.000000000000000000 ) ) ;
#58820 = LINE ( 'NONE', #114553, #127123 ) ;
#58821 = DIRECTION ( 'NONE',  ( -0.7071067811865486830, -0.7071067811865464625, 0.000000000000000000 ) ) ;
#58822 = VERTEX_POINT ( 'NONE', #116265 ) ;
#58823 = CARTESIAN_POINT ( 'NONE',  ( -34.42500000000001137, -16.45860074219782021, 5.000000000000000000 ) ) ;
#58824 = ORIENTED_EDGE ( 'NONE', *, *, #54667, .T. ) ;
#58825 = ORIENTED_EDGE ( 'NONE', *, *, #37225, .T. ) ;
#58826 = VECTOR ( 'NONE', #113552, 1000.000000000000000 ) ;
#58827 = VERTEX_POINT ( 'NONE', #94493 ) ;
#58828 = VECTOR ( 'NONE', #77854, 1000.000000000000000 ) ;
#58829 = CARTESIAN_POINT ( 'NONE',  ( 38.70376352523144448, 6.109999999999998543, 1.122388791418548911E-15 ) ) ;
#58831 = VERTEX_POINT ( 'NONE', #117651 ) ;
#58830 = AXIS2_PLACEMENT_3D ( 'NONE', #13821, #16705, #58850 ) ;
#58832 = CARTESIAN_POINT ( 'NONE',  ( -66.48921356237309510, -27.52281430457101763, 5.000000000000000000 ) ) ;
#58833 = FILL_AREA_STYLE ('',( #14554 ) ) ;
#58834 = LINE ( 'NONE', #26152, #84304 ) ;
#58835 = EDGE_CURVE ( 'NONE', #120201, #24682, #139488, .T. ) ;
#58836 = EDGE_LOOP ( 'NONE', ( #112237, #142416, #84007, #81960 ) ) ;
#58837 = CYLINDRICAL_SURFACE ( 'NONE', #75979, 2.500000000000000000 ) ;
#58838 = PRESENTATION_STYLE_ASSIGNMENT (( #126180 ) ) ;
#58839 = VECTOR ( 'NONE', #57806, 1000.000000000000000 ) ;
#58840 = DIRECTION ( 'NONE',  ( -0.000000000000000000, -0.3543493200069152693, 0.9351131265310292928 ) ) ;
#58841 = LINE ( 'NONE', #137785, #111109 ) ;
#58843 = EDGE_CURVE ( 'NONE', #114851, #16457, #18336, .T. ) ;
#58842 = CARTESIAN_POINT ( 'NONE',  ( 6.299744871391586898, -27.71228299555210484, 4.000000000000000000 ) ) ;
#58844 = DIRECTION ( 'NONE',  ( -0.000000000000000000, 0.3543493200069152138, -0.9351131265310292928 ) ) ;
#58845 = EDGE_LOOP ( 'NONE', ( #106424, #49351, #69064, #128782 ) ) ;
#58846 = EDGE_LOOP ( 'NONE', ( #91644, #33827, #138320, #3522 ) ) ;
#58848 = ORIENTED_EDGE ( 'NONE', *, *, #46982, .F. ) ;
#58847 = VECTOR ( 'NONE', #74338, 999.9999999999998863 ) ;
#58849 = ORIENTED_EDGE ( 'NONE', *, *, #1606, .F. ) ;
#58850 = DIRECTION ( 'NONE',  ( -0.7071067811865486830, -0.7071067811865464625, 0.000000000000000000 ) ) ;
#58851 = EDGE_LOOP ( 'NONE', ( #44557, #63969, #85262, #96131, #8928 ) ) ;
#58852 = ORIENTED_EDGE ( 'NONE', *, *, #135866, .F. ) ;
#58853 = CARTESIAN_POINT ( 'NONE',  ( 34.92499999999998295, 22.22500000000000142, 4.500000000000000888 ) ) ;
#58854 = EDGE_CURVE ( 'NONE', #57981, #118892, #4472, .T. ) ;
#58855 = CARTESIAN_POINT ( 'NONE',  ( 36.48921356237310221, -27.52281430457080802, 5.000000000000000000 ) ) ;
#58856 = VERTEX_POINT ( 'NONE', #32851 ) ;
#58857 = DIRECTION ( 'NONE',  ( -1.000000000000000000, -0.000000000000000000, -0.000000000000000000 ) ) ;
#58858 = ORIENTED_EDGE ( 'NONE', *, *, #55094, .F. ) ;
#58859 = LINE ( 'NONE', #13834, #88437 ) ;
#58860 = EDGE_CURVE ( 'NONE', #56792, #20176, #879, .T. ) ;
#58861 = LINE ( 'NONE', #71126, #126044 ) ;
#58862 = VECTOR ( 'NONE', #35108, 1000.000000000000114 ) ;
#58863 = CARTESIAN_POINT ( 'NONE',  ( 0.2129031414352194063, 3.967499999999992699, -6.871911579029513994 ) ) ;
#58864 = ORIENTED_EDGE ( 'NONE', *, *, #97745, .F. ) ;
#58866 = DIRECTION ( 'NONE',  ( 1.000000000000000000, 0.000000000000000000, 0.000000000000000000 ) ) ;
#58865 = CARTESIAN_POINT ( 'NONE',  ( 100.0995968585647944, -6.109999999999998543, -1.637169565754160727 ) ) ;
#58867 = B_SPLINE_CURVE_WITH_KNOTS ( 'NONE', 3,
 ( #47333, #90045, #134294, #135033, #34994, #79235, #71720, #35726, #79946, #36400, #115883, #77771, #121949, #61573 ),
 .UNSPECIFIED., .F., .F.,
 ( 4, 2, 2, 2, 2, 2, 4 ),
 ( 4.978884922136755915E-17, 0.001506230150421708188, 0.002259345225632537237, 0.003012460300843366502, 0.004518690451265024166, 0.005271805526475853432, 0.006024920601686684432 ),
 .UNSPECIFIED. ) ;
#58868 = CARTESIAN_POINT ( 'NONE',  ( -2.671830600776444964, -18.74070752338408852, 4.000000000000000000 ) ) ;
#58869 = CYLINDRICAL_SURFACE ( 'NONE', #210, 3.999999999999989786 ) ;
#58870 = ORIENTED_EDGE ( 'NONE', *, *, #55806, .T. ) ;
#58871 = ORIENTED_EDGE ( 'NONE', *, *, #70379, .T. ) ;
#58872 = ORIENTED_EDGE ( 'NONE', *, *, #77054, .T. ) ;
#58873 = CARTESIAN_POINT ( 'NONE',  ( 0.000000000000000000, 0.000000000000000000, 5.000000000000000000 ) ) ;
#58874 = LINE ( 'NONE', #47971, #41845 ) ;
#58875 = FACE_OUTER_BOUND ( 'NONE', #114373, .T. ) ;
#58876 = LINE ( 'NONE', #101591, #3582 ) ;
#58877 = CARTESIAN_POINT ( 'NONE',  ( 13.96000000000000085, 2.055000000000001492, 2.516649172247811554E-16 ) ) ;
#58878 = SURFACE_STYLE_USAGE ( .BOTH. , #4360 ) ;
#58881 = ADVANCED_FACE ( 'NONE', ( #132884 ), #32111, .F. ) ;
#58880 = VERTEX_POINT ( 'NONE', #64032 ) ;
#58879 =( GEOMETRIC_REPRESENTATION_CONTEXT ( 3 ) GLOBAL_UNCERTAINTY_ASSIGNED_CONTEXT ( ( #137671 ) ) GLOBAL_UNIT_ASSIGNED_CONTEXT ( ( #108838, #34177, #133490 ) ) REPRESENTATION_CONTEXT ( 'NONE', 'WORKASPACE' ) );
#58882 = CARTESIAN_POINT ( 'NONE',  ( -2.700255128608413990, -27.71228299555204089, 4.000000000000000000 ) ) ;
#58883 = EDGE_CURVE ( 'NONE', #31464, #19753, #131433, .T. ) ;
#58884 = SURFACE_SIDE_STYLE ('',( #94291 ) ) ;
#58885 = DIRECTION ( 'NONE',  ( -0.7071067811865486830, 0.7071067811865464625, 0.000000000000000000 ) ) ;
#58886 = ORIENTED_EDGE ( 'NONE', *, *, #115866, .F. ) ;
#58887 = DIRECTION ( 'NONE',  ( 0.6830127018922181881, 0.6830127018922202975, -0.2588190451025214056 ) ) ;
#58888 = FACE_OUTER_BOUND ( 'NONE', #90034, .T. ) ;
#58889 = ORIENTED_EDGE ( 'NONE', *, *, #11458, .T. ) ;
#58891 = ORIENTED_EDGE ( 'NONE', *, *, #135884, .F. ) ;
#58890 = CARTESIAN_POINT ( 'NONE',  ( 81.18398860626899705, 28.73617430169844056, 5.000000000000000000 ) ) ;
#58892 = ADVANCED_FACE ( 'NONE', ( #99479 ), #87206, .T. ) ;
#58893 = ORIENTED_EDGE ( 'NONE', *, *, #52022, .T. ) ;
#58894 = CARTESIAN_POINT ( 'NONE',  ( 13.49999999999991296, 6.052185695429103340, 5.000000000000000000 ) ) ;
#58895 = PLANE ( 'NONE',  #8923 ) ;
#58896 = VECTOR ( 'NONE', #106168, 1000.000000000000000 ) ;
#58897 = EDGE_LOOP ( 'NONE', ( #26864, #55213, #54002, #2014, #46672, #13773 ) ) ;
#58898 =( NAMED_UNIT ( * ) PLANE_ANGLE_UNIT ( ) SI_UNIT ( $, .RADIAN. ) );
#58899 = VECTOR ( 'NONE', #111075, 1000.000000000000000 ) ;
#58900 = LINE ( 'NONE', #100211, #143290 ) ;
#58901 = ORIENTED_EDGE ( 'NONE', *, *, #13972, .T. ) ;
#58902 = CARTESIAN_POINT ( 'NONE',  ( 12.69999999999999574, -35.05528132343076209, 17.90627459364451113 ) ) ;
#58903 = DIRECTION ( 'NONE',  ( 1.000000000000000000, 0.000000000000000000, 0.000000000000000000 ) ) ;
#58904 = CARTESIAN_POINT ( 'NONE',  ( 63.18398860626900415, 28.73617430169831621, 5.000000000000000000 ) ) ;
#58905 = DIRECTION ( 'NONE',  ( 0.7071067811865487940, 0.7071067811865463515, 0.000000000000000000 ) ) ;
#58906 = CARTESIAN_POINT ( 'NONE',  ( 11.99999999999990585, -10.77435723561694836, -9.972017380717259627 ) ) ;
#58907 = CARTESIAN_POINT ( 'NONE',  ( -3.511686059284292671, 6.759292476615660128, 16.35960578974470536 ) ) ;
#58908 = LINE ( 'NONE', #124105, #97446 ) ;
#58909 = VERTEX_POINT ( 'NONE', #53894 ) ;
#58910 = ORIENTED_EDGE ( 'NONE', *, *, #93325, .F. ) ;
#58911 = VERTEX_POINT ( 'NONE', #88652 ) ;
#58912 = CARTESIAN_POINT ( 'NONE',  ( 122.6250000000000000, -7.950000000000000178, -4.867971026610729436E-16 ) ) ;
#58913 = ORIENTED_EDGE ( 'NONE', *, *, #775, .F. ) ;
#58914 = AXIS2_PLACEMENT_3D ( 'NONE', #78271, #100728, #123923 ) ;
#58915 = EDGE_LOOP ( 'NONE', ( #122721, #63286, #83641 ) ) ;
#58916 = AXIS2_PLACEMENT_3D ( 'NONE', #12522, #58962, #56800 ) ;
#58917 = EDGE_LOOP ( 'NONE', ( #110006, #104417, #39666, #43362 ) ) ;
#58918 = EDGE_CURVE ( 'NONE', #134578, #54699, #66957, .T. ) ;
#58919 = CARTESIAN_POINT ( 'NONE',  ( 0.9064515957856063011, -6.147188561885386981, -3.738859411846097824 ) ) ;
#58920 = CARTESIAN_POINT ( 'NONE',  ( -8.994519915287490619, 28.92564299267944250, 4.000000000000000000 ) ) ;
#58921 = ORIENTED_EDGE ( 'NONE', *, *, #117886, .T. ) ;
#58922 = FACE_OUTER_BOUND ( 'NONE', #74863, .T. ) ;
#58923 = DIRECTION ( 'NONE',  ( -0.7071067811865487940, 0.7071067811865463515, -0.000000000000000000 ) ) ;
#58924 = VECTOR ( 'NONE', #110304, 1000.000000000000000 ) ;
#58925 = DIRECTION ( 'NONE',  ( -0.7071067811865486830, -0.7071067811865464625, 0.000000000000000000 ) ) ;
#58926 = CARTESIAN_POINT ( 'NONE',  ( 109.3754301918981042, -5.291415217122920289, -3.055000000000001492 ) ) ;
#58927 = ORIENTED_EDGE ( 'NONE', *, *, #30269, .T. ) ;
#58928 = ADVANCED_FACE ( 'NONE', ( #43701 ), #77770, .T. ) ;
#58929 = DIRECTION ( 'NONE',  ( 0.6830127018922181881, 0.6830127018922202975, -0.2588190451025214056 ) ) ;
#58930 = CARTESIAN_POINT ( 'NONE',  ( -30.77004279457771574, 21.73644205237998150, 5.000000000000000888 ) ) ;
#58931 = FACE_OUTER_BOUND ( 'NONE', #77704, .T. ) ;
#58932 = CARTESIAN_POINT ( 'NONE',  ( 0.5411153073439879391, 7.255925504780224244, -2.140831595022724798 ) ) ;
#58933 = DIRECTION ( 'NONE',  ( 0.6830127018922180770, -0.6830127018922202975, -0.2588190451025213501 ) ) ;
#58934 = CARTESIAN_POINT ( 'NONE',  ( 19.49999999999986144, 9.431123077392085108, 4.000000000000000000 ) ) ;
#58935 = CARTESIAN_POINT ( 'NONE',  ( 18.79289321881332242, 9.759292476615618384, 5.000000000000000000 ) ) ;
#58936 = VECTOR ( 'NONE', #107974, 1000.000000000000000 ) ;
#58937 = CARTESIAN_POINT ( 'NONE',  ( 48.64169371712955581, -2.130196079827424871, -7.949999999999999289 ) ) ;
#58938 = LINE ( 'NONE', #49469, #65318 ) ;
#58939 = EDGE_CURVE ( 'NONE', #122403, #115805, #56040, .T. ) ;
#58940 = AXIS2_PLACEMENT_3D ( 'NONE', #83973, #21363, #132298 ) ;
#58941 = LINE ( 'NONE', #94352, #90112 ) ;
#58942 = EDGE_LOOP ( 'NONE', ( #27941, #121100, #112608, #30058 ) ) ;
#58943 = ORIENTED_EDGE ( 'NONE', *, *, #66058, .F. ) ;
#58944 = CARTESIAN_POINT ( 'NONE',  ( 39.06249999999999289, -5.819803920172572198, -5.819803920172573086 ) ) ;
#58945 = ADVANCED_FACE ( 'NONE', ( #97330 ), #110355, .F. ) ;
#58946 = ORIENTED_EDGE ( 'NONE', *, *, #58767, .T. ) ;
#58947 = ORIENTED_EDGE ( 'NONE', *, *, #70265, .T. ) ;
#58948 = DIRECTION ( 'NONE',  ( -1.000000000000000000, -0.000000000000000000, -0.000000000000000000 ) ) ;
#58949 = EDGE_CURVE ( 'NONE', #138021, #66046, #21938, .T. ) ;
#58950 = LINE ( 'NONE', #72672, #38525 ) ;
#58951 = ORIENTED_EDGE ( 'NONE', *, *, #100950, .T. ) ;
#58952 = EDGE_CURVE ( 'NONE', #142812, #44722, #141595, .T. ) ;
#58953 = DIRECTION ( 'NONE',  ( 0.000000000000000000, 0.000000000000000000, 1.000000000000000000 ) ) ;
#58954 = SHAPE_REPRESENTATION ( '1.2 Vise Screw', ( #127880 ), #12041 ) ;
#58955 = LINE ( 'NONE', #57487, #113992 ) ;
#58956 = CYLINDRICAL_SURFACE ( 'NONE', #69899, 7.950000000000000178 ) ;
#58957 = CARTESIAN_POINT ( 'NONE',  ( 27.41709685856476142, 3.054999999999998828, 5.291415217122922066 ) ) ;
#58959 = EDGE_CURVE ( 'NONE', #39099, #60685, #66184, .T. ) ;
#58958 = VERTEX_POINT ( 'NONE', #119799 ) ;
#58960 = CARTESIAN_POINT ( 'NONE',  ( -14.92733143757284786, -1.141545485034857643, 4.000000000000000000 ) ) ;
#58961 = ORIENTED_EDGE ( 'NONE', *, *, #88658, .T. ) ;
#58962 = DIRECTION ( 'NONE',  ( 0.000000000000000000, 1.000000000000000000, 0.000000000000000000 ) ) ;
#58963 = LINE ( 'NONE', #3756, #126333 ) ;
#58964 =( NAMED_UNIT ( * ) SI_UNIT ( $, .STERADIAN. ) SOLID_ANGLE_UNIT ( ) );
#58965 = EDGE_CURVE ( 'NONE', #36583, #25072, #124117, .T. ) ;
#58966 = CARTESIAN_POINT ( 'NONE',  ( 63.70833333333332860, -3.974999999999999201, -6.884901960086287964 ) ) ;
#58967 = VERTEX_POINT ( 'NONE', #79234 ) ;
#58968 = ADVANCED_FACE ( 'NONE', ( #102391 ), #3720, .T. ) ;
#58969 = VERTEX_POINT ( 'NONE', #92181 ) ;
#58970 = CARTESIAN_POINT ( 'NONE',  ( -33.48921356237309510, -27.52281430457078670, 5.000000000000000000 ) ) ;
#58971 = LINE ( 'NONE', #26985, #23035 ) ;
#58972 = LINE ( 'NONE', #137197, #82467 ) ;
#58973 = EDGE_CURVE ( 'NONE', #31906, #60720, #113953, .T. ) ;
#58974 = CARTESIAN_POINT ( 'NONE',  ( 53.57876352523144448, -7.482591942790325086E-16, 6.109999999999998543 ) ) ;
#58975 = DIRECTION ( 'NONE',  ( 0.7071067811865487940, 0.7071067811865463515, 0.000000000000000000 ) ) ;
#58976 = ORIENTED_EDGE ( 'NONE', *, *, #51948, .T. ) ;
#58977 = ORIENTED_EDGE ( 'NONE', *, *, #45029, .F. ) ;
#58978 = DIRECTION ( 'NONE',  ( -0.7071067811865487940, 0.7071067811865463515, -0.000000000000000000 ) ) ;
#58979 = ORIENTED_EDGE ( 'NONE', *, *, #114923, .T. ) ;
#58980 = AXIS2_PLACEMENT_3D ( 'NONE', #55052, #88396, #42758 ) ;
#58981 = CARTESIAN_POINT ( 'NONE',  ( 33.81525066741142638, 22.26999999999999957, -13.39192763381150719 ) ) ;
#58982 = PRODUCT_DEFINITION_CONTEXT ( 'detailed design', #139319, 'design' ) ;
#58983 = ORIENTED_EDGE ( 'NONE', *, *, #67622, .F. ) ;
#58984 = CARTESIAN_POINT ( 'NONE',  ( 34.92499999999997584, 7.800094516027095359, 4.759050581649322709 ) ) ;
#58985 = ADVANCED_FACE ( 'NONE', ( #78480 ), #67632, .F. ) ;
#58986 = SURFACE_STYLE_FILL_AREA ( #14708 ) ;
#58987 = FACE_BOUND ( 'NONE', #71406, .T. ) ;
#58988 = FACE_OUTER_BOUND ( 'NONE', #15948, .T. ) ;
#58989 = SURFACE_STYLE_USAGE ( .BOTH. , #69849 ) ;
#58990 = DIRECTION ( 'NONE',  ( -0.7071067811865486830, -0.7071067811865464625, 0.000000000000000000 ) ) ;
#58991 = CARTESIAN_POINT ( 'NONE',  ( 34.92499999999998295, -20.33753812416077267, 4.000000000000000000 ) ) ;
#58993 = VERTEX_POINT ( 'NONE', #26243 ) ;
#58992 = CARTESIAN_POINT ( 'NONE',  ( 20.20710678118641468, 18.75929247661552068, 5.000000000000000000 ) ) ;
#58994 = VECTOR ( 'NONE', #135812, 1000.000000000000114 ) ;
#58995 = DIRECTION ( 'NONE',  ( 1.000000000000000000, 0.000000000000000000, 0.000000000000000000 ) ) ;
#58996 = EDGE_CURVE ( 'NONE', #51865, #31605, #122675, .T. ) ;
#58997 = EDGE_LOOP ( 'NONE', ( #15987, #131625, #128700, #45845 ) ) ;
#58998 = VECTOR ( 'NONE', #26082, 1000.000000000000000 ) ;
#58999 = EDGE_LOOP ( 'NONE', ( #97518, #51043, #24547, #76313, #77180 ) ) ;
#59000 = CARTESIAN_POINT ( 'NONE',  ( 62.76626352523144448, 4.472830434245838482, -4.472830434245837594 ) ) ;
#59001 = ORIENTED_EDGE ( 'NONE', *, *, #4833, .F. ) ;
#59002 = CARTESIAN_POINT ( 'NONE',  ( 66.18398860626901126, 28.73617430169833753, 5.000000000000000000 ) ) ;
#59003 = VECTOR ( 'NONE', #57644, 1000.000000000000000 ) ;
#59004 = EDGE_CURVE ( 'NONE', #3762, #118999, #25502, .T. ) ;
#59005 = ORIENTED_EDGE ( 'NONE', *, *, #3601, .F. ) ;
#59006 = DIRECTION ( 'NONE',  ( -1.000000000000000000, 0.000000000000000000, -0.000000000000000000 ) ) ;
#59007 = LINE ( 'NONE', #95670, #61204 ) ;
#59008 = CARTESIAN_POINT ( 'NONE',  ( 11.51078643762690490, -27.52281430457047406, 5.000000000000000000 ) ) ;
#59009 = VECTOR ( 'NONE', #128387, 999.9999999999998863 ) ;
#59010 = EDGE_CURVE ( 'NONE', #75896, #54552, #69779, .T. ) ;
#59011 = FACE_OUTER_BOUND ( 'NONE', #126267, .T. ) ;
#59012 = CARTESIAN_POINT ( 'NONE',  ( 29.71998032010578328, 0.7592924766157173044, 14.27032725228015764 ) ) ;
#59013 = PLANE ( 'NONE',  #35469 ) ;
#59014 = CARTESIAN_POINT ( 'NONE',  ( -78.18398860626899705, 28.73617430169841924, 5.000000000000000000 ) ) ;
#59015 = VERTEX_POINT ( 'NONE', #111824 ) ;
#59016 = ORIENTED_EDGE ( 'NONE', *, *, #81909, .F. ) ;
#59017 = FACE_OUTER_BOUND ( 'NONE', #48941, .T. ) ;
#59018 = CARTESIAN_POINT ( 'NONE',  ( 29.99451991528749417, 28.92564299267958816, 4.000000000000000000 ) ) ;
#59019 = ORIENTED_EDGE ( 'NONE', *, *, #44182, .T. ) ;
#59020 = ORIENTED_EDGE ( 'NONE', *, *, #27330, .F. ) ;
#59021 = EDGE_LOOP ( 'NONE', ( #120814, #143235, #136137, #139543 ) ) ;
#59022 = EDGE_CURVE ( 'NONE', #12165, #59626, #79945, .T. ) ;
#59023 = LINE ( 'NONE', #3818, #85507 ) ;
#59024 = ORIENTED_EDGE ( 'NONE', *, *, #111050, .T. ) ;
#59025 = DIRECTION ( 'NONE',  ( 1.000000000000000000, 0.000000000000000000, 0.000000000000000000 ) ) ;
#59026 = LINE ( 'NONE', #4515, #33108 ) ;
#59027 = VECTOR ( 'NONE', #89073, 1000.000000000000000 ) ;
#59028 = CARTESIAN_POINT ( 'NONE',  ( -0.8079301918981138808, -7.934999999999991616, -2.126176841940955242 ) ) ;
#59029 = AXIS2_PLACEMENT_3D ( 'NONE', #31898, #88438, #143503 ) ;
#59030 = CARTESIAN_POINT ( 'NONE',  ( 0.000000000000000000, 0.000000000000000000, 5.000000000000000000 ) ) ;
#59031 = ORIENTED_EDGE ( 'NONE', *, *, #53776, .T. ) ;
#59032 = AXIS2_PLACEMENT_3D ( 'NONE', #11290, #76620, #10591 ) ;
#59033 = DIRECTION ( 'NONE',  ( -0.000000000000000000, 0.3543493200069152138, -0.9351131265310292928 ) ) ;
#59034 = CARTESIAN_POINT ( 'NONE',  ( 119.5166937171295558, 7.950000000000000178, -2.130196079827421318 ) ) ;
#59035 = LINE ( 'NONE', #48117, #5750 ) ;
#59037 = VERTEX_POINT ( 'NONE', #113223 ) ;
#59036 = FACE_OUTER_BOUND ( 'NONE', #138299, .T. ) ;
#59038 = VERTEX_POINT ( 'NONE', #137145 ) ;
#59039 = CARTESIAN_POINT ( 'NONE',  ( -34.92500000000001137, 22.22500000000000142, 4.500000000000000888 ) ) ;
#59040 = DIRECTION ( 'NONE',  ( -0.000000000000000000, 0.3543493200069153248, 0.9351131265310292928 ) ) ;
#59041 = CARTESIAN_POINT ( 'NONE',  ( 26.99451991528749417, 28.92564299267956685, 4.000000000000000000 ) ) ;
#59042 = ORIENTED_EDGE ( 'NONE', *, *, #41839, .F. ) ;
#59043 = SURFACE_STYLE_FILL_AREA ( #125692 ) ;
#59044 = PLANE ( 'NONE',  #36345 ) ;
#59045 = EDGE_CURVE ( 'NONE', #87113, #86807, #124830, .T. ) ;
#59046 = DIRECTION ( 'NONE',  ( 1.000000000000000000, 0.000000000000000000, 0.000000000000000000 ) ) ;
#59047 = CARTESIAN_POINT ( 'NONE',  ( -28.00193056682078918, -22.22500000000000142, 4.500000000000000888 ) ) ;
#59048 = LINE ( 'NONE', #103893, #130107 ) ;
#59049 = VERTEX_POINT ( 'NONE', #59602 ) ;
#59050 = CARTESIAN_POINT ( 'NONE',  ( -13.49999999999991118, 14.14708470758590053, -0.5283514160166246088 ) ) ;
#59051 = DIRECTION ( 'NONE',  ( 0.3543493200069162685, -0.000000000000000000, -0.9351131265310288487 ) ) ;
#59052 = CARTESIAN_POINT ( 'NONE',  ( 7.191639616203771901, 6.094999999999988205, -1.633150327867694651 ) ) ;
#59053 = DIRECTION ( 'NONE',  ( 1.000000000000000000, 0.000000000000000000, 0.000000000000000000 ) ) ;
#59054 = ORIENTED_EDGE ( 'NONE', *, *, #105216, .T. ) ;
#59055 = ADVANCED_FACE ( 'NONE', ( #58922 ), #35725, .T. ) ;
#59056 = VERTEX_POINT ( 'NONE', #2297 ) ;
#59057 = CARTESIAN_POINT ( 'NONE',  ( 26.67183060077629264, -3.740707523384234623, 4.000000000000000000 ) ) ;
#59058 = FACE_OUTER_BOUND ( 'NONE', #89531, .T. ) ;
#59059 = CARTESIAN_POINT ( 'NONE',  ( 2.457903141435219485, 6.871911579029515771, 3.967499999999989146 ) ) ;
#59060 = CARTESIAN_POINT ( 'NONE',  ( 64.68336038379622721, -2.130196079827426203, 7.949999999999996625 ) ) ;
#59061 = DIRECTION ( 'NONE',  ( 0.7071067811865486830, -0.7071067811865464625, -0.000000000000000000 ) ) ;
#59062 = LINE ( 'NONE', #69188, #127033 ) ;
#59063 = DIRECTION ( 'NONE',  ( -0.7071067811865487940, 0.7071067811865463515, -0.000000000000000000 ) ) ;
#59064 = ORIENTED_EDGE ( 'NONE', *, *, #126323, .F. ) ;
#59065 =( LENGTH_UNIT ( ) NAMED_UNIT ( * ) SI_UNIT ( .MILLI., .METRE. ) );
#59066 = CARTESIAN_POINT ( 'NONE',  ( 34.92499999999998295, 9.856123077392316745, 4.000000000000000000 ) ) ;
#59067 = FACE_OUTER_BOUND ( 'NONE', #117899, .T. ) ;
#59068 = CARTESIAN_POINT ( 'NONE',  ( 51.53709685856478018, -3.054999999999999272, -5.291415217122919401 ) ) ;
#59069 = EDGE_CURVE ( 'NONE', #42800, #140795, #123441, .T. ) ;
#59070 = VECTOR ( 'NONE', #135306, 1000.000000000000227 ) ;
#59071 = CARTESIAN_POINT ( 'NONE',  ( -30.29974487139158867, -27.71228299555227537, 4.000000000000000000 ) ) ;
#59072 = DIRECTION ( 'NONE',  ( 1.000000000000000000, 0.000000000000000000, 0.000000000000000000 ) ) ;
#59073 = VERTEX_POINT ( 'NONE', #45869 ) ;
#59074 = CARTESIAN_POINT ( 'NONE',  ( -11.81601139373100651, 28.73617430169779041, 5.000000000000000000 ) ) ;
#59075 = ORIENTED_EDGE ( 'NONE', *, *, #63784, .T. ) ;
#59076 = DIRECTION ( 'NONE',  ( -0.7071067811865486830, -0.7071067811865464625, 0.000000000000000000 ) ) ;
#59077 = LINE ( 'NONE', #81531, #15991 ) ;
#59078 = PLANE ( 'NONE',  #106714 ) ;
#59079 = DIRECTION ( 'NONE',  ( -0.000000000000000000, 0.000000000000000000, 1.000000000000000000 ) ) ;
#59080 = DIRECTION ( 'NONE',  ( -0.000000000000000000, -0.000000000000000000, -1.000000000000000000 ) ) ;
#59081 = CARTESIAN_POINT ( 'NONE',  ( 11.66666666666666785, -5.278424836066145431, -3.047499999999993658 ) ) ;
#59082 = ORIENTED_EDGE ( 'NONE', *, *, #100926, .F. ) ;
#59083 = CARTESIAN_POINT ( 'NONE',  ( -9.758600742197899081, 21.72500000000000853, 5.000000000000000000 ) ) ;
#59084 = LINE ( 'NONE', #69965, #51492 ) ;
#59085 = UNCERTAINTY_MEASURE_WITH_UNIT (LENGTH_MEASURE( 1.000000000000000082E-05 ), #8518, 'distance_accuracy_value', 'NONE');
#59086 = CARTESIAN_POINT ( 'NONE',  ( -15.18398860626900237, 28.73617430169797871, 5.000000000000000000 ) ) ;
#59087 = CARTESIAN_POINT ( 'NONE',  ( 34.42499999999998295, -18.02281430457042433, 5.000000000000000000 ) ) ;
#59088 = CARTESIAN_POINT ( 'NONE',  ( 74.60002705046289861, 5.819803920172570422, 5.819803920172574863 ) ) ;
#59089 = VECTOR ( 'NONE', #57845, 1000.000000000000000 ) ;
#59090 = EDGE_CURVE ( 'NONE', #96272, #57196, #34993, .T. ) ;
#59091 = DIRECTION ( 'NONE',  ( -0.000000000000000000, 0.3543493200069153248, 0.9351131265310292928 ) ) ;
#59092 = VERTEX_POINT ( 'NONE', #4404 ) ;
#59093 =( BOUNDED_CURVE ( )  B_SPLINE_CURVE ( 3, ( #37217, #82184, #82881, #140117 ),
 .UNSPECIFIED., .F., .T. ) 
 B_SPLINE_CURVE_WITH_KNOTS ( ( 4, 4 ),
 ( 1.864375635226923844, 1.933014472006567175 ),
 .UNSPECIFIED. ) 
 CURVE ( )  GEOMETRIC_REPRESENTATION_ITEM ( )  RATIONAL_B_SPLINE_CURVE ( ( 1.000000000000000000, 0.9996074310407760954, 0.9996074310407760954, 1.000000000000000000 ) ) 
 REPRESENTATION_ITEM ( '' )  );
#59094 = CARTESIAN_POINT ( 'NONE',  ( 62.83333333333332149, -6.884901960086287964, 3.974999999999998312 ) ) ;
#59095 = CARTESIAN_POINT ( 'NONE',  ( 15.60486233187511473, 21.75929247661549226, 21.32995629748182864 ) ) ;
#59096 = ADVANCED_FACE ( 'NONE', ( #68353 ), #39335, .T. ) ;
#59097 = VECTOR ( 'NONE', #71198, 1000.000000000000227 ) ;
#59098 = LINE ( 'NONE', #50326, #141136 ) ;
#59099 = CARTESIAN_POINT ( 'NONE',  ( 16.49999999999988987, 22.08746187583901843, 4.000000000000000000 ) ) ;
#59100 = ORIENTED_EDGE ( 'NONE', *, *, #38117, .T. ) ;
#59101 = EDGE_CURVE ( 'NONE', #64882, #32697, #36930, .T. ) ;
#59102 = ADVANCED_FACE ( 'NONE', ( #135715 ), #36399, .F. ) ;
#59103 = FACE_OUTER_BOUND ( 'NONE', #74575, .T. ) ;
#59104 = AXIS2_PLACEMENT_3D ( 'NONE', #64377, #129617, #86855 ) ;
#59105 = DIRECTION ( 'NONE',  ( 0.000000000000000000, 0.000000000000000000, 1.000000000000000000 ) ) ;
#59106 = CARTESIAN_POINT ( 'NONE',  ( 53.52126352523144703, -4.472830434245839371, -4.472830434245840259 ) ) ;
#59107 = CARTESIAN_POINT ( 'NONE',  ( -18.63311396761903538, -2.779424156541560276, 4.000000000000000000 ) ) ;
#59108 = EDGE_LOOP ( 'NONE', ( #20517, #47570, #8677, #139747, #30527, #26248 ) ) ;
#59109 = EDGE_LOOP ( 'NONE', ( #69275, #136183 ) ) ;
#59110 = DIRECTION ( 'NONE',  ( -1.000000000000000000, -0.000000000000000000, -0.000000000000000000 ) ) ;
#59111 = CARTESIAN_POINT ( 'NONE',  ( -29.99999999999979039, -16.60178936734451582, 0.8616154019346804471 ) ) ;
#59112 = DIRECTION ( 'NONE',  ( -0.6830127018922181881, 0.6830127018922202975, -0.2588190451025214056 ) ) ;
#59113 = EDGE_CURVE ( 'NONE', #37315, #119727, #39266, .T. ) ;
#59114 = PLANE ( 'NONE',  #69553 ) ;
#59115 = ADVANCED_FACE ( 'NONE', ( #29782 ), #51574, .T. ) ;
#59116 = CARTESIAN_POINT ( 'NONE',  ( 32.99451991528749062, 28.92564299267960948, 4.000000000000000000 ) ) ;
#59118 = VERTEX_POINT ( 'NONE', #50139 ) ;
#59117 = CARTESIAN_POINT ( 'NONE',  ( 3.183988606268992161, 28.73617430169789699, 5.000000000000000000 ) ) ;
#59119 = CARTESIAN_POINT ( 'NONE',  ( -24.00548008471250938, 28.92564299267921513, 4.000000000000000000 ) ) ;
#59120 = CARTESIAN_POINT ( 'NONE',  ( 23.99999999999983302, 15.45873954670187622, -0.03131636524299555302 ) ) ;
#59121 = DIRECTION ( 'NONE',  ( -0.7071067811865486830, -0.7071067811865464625, -0.000000000000000000 ) ) ;
#59122 = PRESENTATION_STYLE_ASSIGNMENT (( #101861 ) ) ;
#59123 = EDGE_CURVE ( 'NONE', #137944, #39127, #74027, .T. ) ;
#59124 = VECTOR ( 'NONE', #92030, 999.9999999999998863 ) ;
#59125 = ORIENTED_EDGE ( 'NONE', *, *, #66035, .F. ) ;
#59126 = VECTOR ( 'NONE', #80753, 1000.000000000000000 ) ;
#59127 = AXIS2_PLACEMENT_3D ( 'NONE', #125117, #69332, #17587 ) ;
#59128 = EDGE_LOOP ( 'NONE', ( #30748, #120079, #122598, #55232 ) ) ;
#59129 = AXIS2_PLACEMENT_3D ( 'NONE', #107453, #137966, #8120 ) ;
#59130 = LINE ( 'NONE', #103279, #114698 ) ;
#59131 = DIRECTION ( 'NONE',  ( -0.6830127018922181881, 0.6830127018922202975, -0.2588190451025214056 ) ) ;
#59132 = DIRECTION ( 'NONE',  ( -0.6830127018922180770, -0.6830127018922204085, -0.2588190451025213501 ) ) ;
#59133 = CARTESIAN_POINT ( 'NONE',  ( 12.82439460721831104, 4.202752102959690472E-16, 0.000000000000000000 ) ) ;
#59134 = ORIENTED_EDGE ( 'NONE', *, *, #22668, .F. ) ;
#59136 = EDGE_CURVE ( 'NONE', #25035, #56060, #49452, .T. ) ;
#59135 = ORIENTED_EDGE ( 'NONE', *, *, #14444, .T. ) ;
#59137 = CARTESIAN_POINT ( 'NONE',  ( -20.46326412755669111, -2.625232532701756494, 4.661243073242806290 ) ) ;
#59138 = DIRECTION ( 'NONE',  ( 0.7071067811865486830, -0.7071067811865464625, -0.000000000000000000 ) ) ;
#59139 = ORIENTED_EDGE ( 'NONE', *, *, #28249, .F. ) ;
#59140 = SURFACE_STYLE_USAGE ( .BOTH. , #3941 ) ;
#59141 = ORIENTED_EDGE ( 'NONE', *, *, #86999, .F. ) ;
#59142 = CARTESIAN_POINT ( 'NONE',  ( -23.99451991528749062, 28.92564299267954908, 4.000000000000000000 ) ) ;
#59143 = EDGE_CURVE ( 'NONE', #36339, #76243, #40689, .T. ) ;
#59144 = CARTESIAN_POINT ( 'NONE',  ( 0.000000000000000000, 0.000000000000000000, 5.000000000000000000 ) ) ;
#59145 = ORIENTED_EDGE ( 'NONE', *, *, #107461, .F. ) ;
#59146 = FACE_BOUND ( 'NONE', #98317, .T. ) ;
#59147 = PLANE ( 'NONE',  #73348 ) ;
#59148 = PLANE ( 'NONE',  #118415 ) ;
#59149 = PLANE ( 'NONE',  #82968 ) ;
#59150 = DIRECTION ( 'NONE',  ( 1.000000000000000000, 0.000000000000000000, 0.000000000000000000 ) ) ;
#59151 =( NAMED_UNIT ( * ) SI_UNIT ( $, .STERADIAN. ) SOLID_ANGLE_UNIT ( ) );
#59154 = ADVANCED_FACE ( 'NONE', ( #128413 ), #116083, .F. ) ;
#59153 =( BOUNDED_CURVE ( )  B_SPLINE_CURVE ( 3, ( #62954, #42632, #107129, #140474 ),
 .UNSPECIFIED., .F., .T. ) 
 B_SPLINE_CURVE_WITH_KNOTS ( ( 4, 4 ),
 ( 2.779374508378133601, 4.199602562396794525 ),
 .UNSPECIFIED. ) 
 CURVE ( )  GEOMETRIC_REPRESENTATION_ITEM ( )  RATIONAL_B_SPLINE_CURVE ( ( 1.000000000000000000, 0.8388583629366721528, 0.8388583629366721528, 1.000000000000000000 ) ) 
 REPRESENTATION_ITEM ( '' )  );
#59152 = DIRECTION ( 'NONE',  ( -2.220446049250313081E-16, -5.551115123125782702E-17, 1.000000000000000222 ) ) ;
#59155 = ORIENTED_EDGE ( 'NONE', *, *, #84024, .F. ) ;
#59156 = EDGE_LOOP ( 'NONE', ( #125461, #114095, #56064, #52908, #73566 ) ) ;
#59157 = CARTESIAN_POINT ( 'NONE',  ( 94.12043019189810877, 3.055000000000001936, -5.291415217122916737 ) ) ;
#59158 = ORIENTED_EDGE ( 'NONE', *, *, #13502, .F. ) ;
#59159 = DIRECTION ( 'NONE',  ( 0.7071067811865486830, -0.7071067811865464625, -0.000000000000000000 ) ) ;
#59160 = DIRECTION ( 'NONE',  ( 0.7071067811865487940, 0.7071067811865463515, 0.000000000000000000 ) ) ;
#59161 = DIRECTION ( 'NONE',  ( -1.000000000000000000, -0.000000000000000000, -0.000000000000000000 ) ) ;
#59162 = LINE ( 'NONE', #127970, #47139 ) ;
#59163 = VERTEX_POINT ( 'NONE', #5157 ) ;
#59164 = DIRECTION ( 'NONE',  ( -0.000000000000000000, 0.3543493200069153248, 0.9351131265310292928 ) ) ;
#59165 = CARTESIAN_POINT ( 'NONE',  ( 0.000000000000000000, 0.000000000000000000, 5.000000000000000000 ) ) ;
#59166 = EDGE_CURVE ( 'NONE', #131471, #17257, #82766, .T. ) ;
#59167 = FILL_AREA_STYLE ('',( #24352 ) ) ;
#59169 = CARTESIAN_POINT ( 'NONE',  ( -17.99999999999986855, -7.447814304570745669, 5.000000000000000000 ) ) ;
#59168 = LINE ( 'NONE', #113485, #103569 ) ;
#59170 = DIRECTION ( 'NONE',  ( -0.3543493200069162685, -0.000000000000000000, -0.9351131265310288487 ) ) ;
#59171 = DIRECTION ( 'NONE',  ( -1.000000000000000000, -1.224606353822377258E-16, -0.000000000000000000 ) ) ;
#59172 = ORIENTED_EDGE ( 'NONE', *, *, #36600, .T. ) ;
#59173 = LINE ( 'NONE', #25777, #119050 ) ;
#59174 = DIRECTION ( 'NONE',  ( 0.7071067811865486830, -0.7071067811865464625, -0.000000000000000000 ) ) ;
#59175 = ORIENTED_EDGE ( 'NONE', *, *, #131812, .T. ) ;
#59176 = VERTEX_POINT ( 'NONE', #107355 ) ;
#59177 = ADVANCED_FACE ( 'NONE', ( #61061 ), #62449, .F. ) ;
#59178 = ORIENTED_EDGE ( 'NONE', *, *, #118593, .T. ) ;
#59179 = CARTESIAN_POINT ( 'NONE',  ( 43.02126352523142572, -4.472830434245838482, -4.472830434245840259 ) ) ;
#59180 = VERTEX_POINT ( 'NONE', #138572 ) ;
#59181 = VECTOR ( 'NONE', #34466, 1000.000000000000000 ) ;
#59182 = CARTESIAN_POINT ( 'NONE',  ( 10.10830628287043709, 1.633150327867687324, -6.094999999999991758 ) ) ;
#59183 = CARTESIAN_POINT ( 'NONE',  ( -8.378674182341532273, 12.11998467473676833, -25.56646076112756916 ) ) ;
#59184 = ORIENTED_EDGE ( 'NONE', *, *, #57634, .F. ) ;
#59185 = CONICAL_SURFACE ( 'NONE', #61466, 2.055000000000000604, 0.9599310885968764806 ) ;
#59186 = ADVANCED_FACE ( 'NONE', ( #18918 ), #63184, .T. ) ;
#59187 = CARTESIAN_POINT ( 'NONE',  ( -5.999999999999956479, -13.97847968911261063, -0.1324546996126930165 ) ) ;
#59188 = ORIENTED_EDGE ( 'NONE', *, *, #68513, .F. ) ;
#59189 = FILL_AREA_STYLE_COLOUR ( '', #74270 ) ;
#59191 = ORIENTED_EDGE ( 'NONE', *, *, #138942, .T. ) ;
#59190 = CARTESIAN_POINT ( 'NONE',  ( 0.000000000000000000, 0.000000000000000000, 5.000000000000000000 ) ) ;
#59192 = ORIENTED_EDGE ( 'NONE', *, *, #95469, .F. ) ;
#59193 = DIRECTION ( 'NONE',  ( 1.000000000000000000, 0.000000000000000000, 0.000000000000000000 ) ) ;
#59194 = DIRECTION ( 'NONE',  ( 0.000000000000000000, 0.3543493200069153248, 0.9351131265310291818 ) ) ;
#59195 = CARTESIAN_POINT ( 'NONE',  ( 27.78752705046289151, 0.000000000000000000, -7.949999999999998401 ) ) ;
#59196 = ORIENTED_EDGE ( 'NONE', *, *, #55094, .T. ) ;
#59197 = CARTESIAN_POINT ( 'NONE',  ( -7.940000000000001279, -33.26999999999999602, -10.00000000000000178 ) ) ;
#59198 = EDGE_LOOP ( 'NONE', ( #119901, #83470, #32754 ) ) ;
#59199 = AXIS2_PLACEMENT_3D ( 'NONE', #67239, #56406, #112867 ) ;
#59201 = ORIENTED_EDGE ( 'NONE', *, *, #90169, .F. ) ;
#59200 = ADVANCED_FACE ( 'NONE', ( #96444 ), #101818, .T. ) ;
#59202 = EDGE_LOOP ( 'NONE', ( #7629, #22552, #98370, #84788 ) ) ;
#59203 = ORIENTED_EDGE ( 'NONE', *, *, #66495, .T. ) ;
#59204 = PRESENTATION_STYLE_ASSIGNMENT (( #14928 ) ) ;
#59205 = CARTESIAN_POINT ( 'NONE',  ( -16.49999999999988276, 15.05218569542901186, 5.000000000000000000 ) ) ;
#59207 = ADVANCED_FACE ( 'NONE', ( #106613 ), #131840, .T. ) ;
#59206 = CARTESIAN_POINT ( 'NONE',  ( 9.994118527364397764, 4.584330080086930965E-16, 0.000000000000000000 ) ) ;
#59208 = DIRECTION ( 'NONE',  ( -0.7071067811865486830, -0.7071067811865464625, 0.000000000000000000 ) ) ;
#59209 = EDGE_CURVE ( 'NONE', #79521, #42427, #82082, .T. ) ;
#59210 = CARTESIAN_POINT ( 'NONE',  ( -32.29289321881323360, -9.740707523384186217, 5.000000000000000000 ) ) ;
#59211 = ORIENTED_EDGE ( 'NONE', *, *, #30816, .T. ) ;
#59212 = LINE ( 'NONE', #100544, #88995 ) ;
#59213 = VECTOR ( 'NONE', #92737, 1000.000000000000000 ) ;
#59214 = CARTESIAN_POINT ( 'NONE',  ( 21.41623647476855652, -7.934999999999990727, 4.858786175617117713E-16 ) ) ;
#59215 = CARTESIAN_POINT ( 'NONE',  ( -3.722814304570581712, -21.72499999999999432, 5.000000000000000000 ) ) ;
#59216 = VECTOR ( 'NONE', #59796, 999.9999999999998863 ) ;
#59217 = DIRECTION ( 'NONE',  ( -0.000000000000000000, 0.000000000000000000, 1.000000000000000000 ) ) ;
#59219 = EDGE_CURVE ( 'NONE', #47367, #83534, #52262, .T. ) ;
#59218 = VECTOR ( 'NONE', #21323, 1000.000000000000000 ) ;
#59220 = CARTESIAN_POINT ( 'NONE',  ( -34.92499999999997584, 22.27000000000000668, -7.752744394707050901 ) ) ;
#59221 = EDGE_LOOP ( 'NONE', ( #789, #36834, #68825, #47706 ) ) ;
#59222 = VERTEX_POINT ( 'NONE', #26939 ) ;
#59223 = ORIENTED_EDGE ( 'NONE', *, *, #68956, .T. ) ;
#59224 = CARTESIAN_POINT ( 'NONE',  ( 10.17183060077639922, -14.24070752338414003, 4.000000000000000000 ) ) ;
#59225 = CARTESIAN_POINT ( 'NONE',  ( 39.18398860626899705, 28.73617430169814568, 5.000000000000000000 ) ) ;
#59226 = UNCERTAINTY_MEASURE_WITH_UNIT (LENGTH_MEASURE( 1.000000000000000082E-05 ), #90075, 'distance_accuracy_value', 'NONE');
#59227 = CARTESIAN_POINT ( 'NONE',  ( 27.48921356237309155, -27.52281430457074762, 5.000000000000000000 ) ) ;
#59228 = VECTOR ( 'NONE', #60675, 999.9999999999998863 ) ;
#59229 = CARTESIAN_POINT ( 'NONE',  ( 0.000000000000000000, 0.000000000000000000, 5.000000000000000000 ) ) ;
#59230 = LINE ( 'NONE', #136732, #6481 ) ;
#59231 = LINE ( 'NONE', #80254, #84836 ) ;
#59232 = ADVANCED_FACE ( 'NONE', ( #71187 ), #115335, .F. ) ;
#59233 = CARTESIAN_POINT ( 'NONE',  ( 80.47916666666664298, -7.950000000000000178, 2.130196079827424427 ) ) ;
#59234 = FACE_OUTER_BOUND ( 'NONE', #120880, .T. ) ;
#59235 = DIRECTION ( 'NONE',  ( 0.000000000000000000, 0.000000000000000000, 1.000000000000000000 ) ) ;
#59236 = CARTESIAN_POINT ( 'NONE',  ( -25.82816939922335209, 18.75929247661552068, 4.000000000000000000 ) ) ;
#59237 = LINE ( 'NONE', #38873, #97430 ) ;
#59238 = ORIENTED_EDGE ( 'NONE', *, *, #56790, .T. ) ;
#59239 = CARTESIAN_POINT ( 'NONE',  ( 17.29169637474938526, -1.887777690644416140, -32.52073842440807283 ) ) ;
#59240 = ORIENTED_EDGE ( 'NONE', *, *, #21907, .F. ) ;
#59241 = LINE ( 'NONE', #27266, #22826 ) ;
#59243 = ORIENTED_EDGE ( 'NONE', *, *, #94829, .F. ) ;
#59242 = DIRECTION ( 'NONE',  ( 0.000000000000000000, -1.000000000000000000, 0.000000000000000000 ) ) ;
#59244 = DIRECTION ( 'NONE',  ( -0.000000000000000000, 0.000000000000000000, 1.000000000000000000 ) ) ;
#59245 = CARTESIAN_POINT ( 'NONE',  ( 30.48921356237309510, -27.52281430457076894, 5.000000000000000000 ) ) ;
#59246 = ORIENTED_EDGE ( 'NONE', *, *, #59022, .T. ) ;
#59247 = DIRECTION ( 'NONE',  ( 1.000000000000000000, 0.000000000000000000, 0.000000000000000000 ) ) ;
#59248 = ORIENTED_EDGE ( 'NONE', *, *, #53095, .T. ) ;
#59249 = SURFACE_SIDE_STYLE ('',( #3369 ) ) ;
#59250 = ORIENTED_EDGE ( 'NONE', *, *, #13389, .F. ) ;
#59251 = CARTESIAN_POINT ( 'NONE',  ( 18.81349135397627492, -15.74070752338412760, 8.904080028138896097 ) ) ;
#59252 = CARTESIAN_POINT ( 'NONE',  ( 101.4333603837962414, 2.130196079827431532, -7.949999999999997513 ) ) ;
#59253 = CARTESIAN_POINT ( 'NONE',  ( 10.32500000000000107, 8.432637487761466488, 4.375000000000001776 ) ) ;
#59254 = EDGE_CURVE ( 'NONE', #15997, #33874, #95039, .T. ) ;
#59255 = CARTESIAN_POINT ( 'NONE',  ( -0.2997448713915885632, -27.71228299555206220, 4.000000000000000000 ) ) ;
#59256 = VERTEX_POINT ( 'NONE', #10178 ) ;
#59257 = CARTESIAN_POINT ( 'NONE',  ( 9.682526172861077640, 4.202752102959690472E-16, 0.000000000000000000 ) ) ;
#59259 = EDGE_CURVE ( 'NONE', #69474, #25047, #87042, .T. ) ;
#59258 = DIRECTION ( 'NONE',  ( -0.3543493200069162685, -0.000000000000000000, -0.9351131265310288487 ) ) ;
#59260 = DIRECTION ( 'NONE',  ( 0.7071067811865487940, 0.7071067811865463515, -0.000000000000000000 ) ) ;
#59261 = CARTESIAN_POINT ( 'NONE',  ( 22.89583333333333215, 1.633150327867687324, -6.094999999999991758 ) ) ;
#59262 = LINE ( 'NONE', #101295, #114913 ) ;
#59263 = ORIENTED_EDGE ( 'NONE', *, *, #44687, .F. ) ;
#59264 = EDGE_CURVE ( 'NONE', #89344, #25946, #42132, .T. ) ;
#59265 = EDGE_CURVE ( 'NONE', #26035, #79450, #129827, .T. ) ;
#59266 = FACE_OUTER_BOUND ( 'NONE', #129146, .T. ) ;
#59267 = ORIENTED_EDGE ( 'NONE', *, *, #33506, .F. ) ;
#59268 = CARTESIAN_POINT ( 'NONE',  ( 98.43793019189811844, -6.110000000000001208, 1.637169565754158951 ) ) ;
#59269 = FACE_OUTER_BOUND ( 'NONE', #48672, .T. ) ;
#59270 = DIRECTION ( 'NONE',  ( -1.000000000000000000, -0.000000000000000000, -0.000000000000000000 ) ) ;
#59271 = LINE ( 'NONE', #93286, #79372 ) ;
#59272 = CARTESIAN_POINT ( 'NONE',  ( 126.2468580783230578, -45.52550609312092433, -35.40428284070834053 ) ) ;
#59273 = ORIENTED_EDGE ( 'NONE', *, *, #96828, .F. ) ;
#59274 = CARTESIAN_POINT ( 'NONE',  ( 27.99999999999999645, -49.14999999999999147, -49.92499999999968452 ) ) ;
#59275 = CARTESIAN_POINT ( 'NONE',  ( -15.18398860626900237, 28.73617430169797871, 5.000000000000000000 ) ) ;
#59276 = EDGE_CURVE ( 'NONE', #84184, #64792, #131258, .T. ) ;
#59277 = ORIENTED_EDGE ( 'NONE', *, *, #96277, .T. ) ;
#59278 = DIRECTION ( 'NONE',  ( -0.6830127018922181881, 0.6830127018922202975, -0.2588190451025214056 ) ) ;
#59279 = EDGE_CURVE ( 'NONE', #24662, #109601, #132726, .T. ) ;
#59280 = DIRECTION ( 'NONE',  ( -0.6830127018922180770, -0.6830127018922204085, -0.2588190451025213501 ) ) ;
#59282 = ORIENTED_EDGE ( 'NONE', *, *, #2326, .F. ) ;
#59281 = CARTESIAN_POINT ( 'NONE',  ( 16.49999999999988987, 16.77039438581780573, 0.4657186855307349771 ) ) ;
#59283 = LINE ( 'NONE', #92558, #46076 ) ;
#59284 = CARTESIAN_POINT ( 'NONE',  ( -34.92500000000001137, 13.80009451602706783, 4.759050581649336920 ) ) ;
#59285 = CARTESIAN_POINT ( 'NONE',  ( 0.000000000000000000, 0.000000000000000000, 5.000000000000000000 ) ) ;
#59286 = FACE_OUTER_BOUND ( 'NONE', #70555, .T. ) ;
#59287 = ORIENTED_EDGE ( 'NONE', *, *, #8982, .T. ) ;
#59288 = VECTOR ( 'NONE', #39116, 1000.000000000000000 ) ;
#59289 = VERTEX_POINT ( 'NONE', #31946 ) ;
#59290 = EDGE_LOOP ( 'NONE', ( #5243, #74879, #104523, #15777 ) ) ;
#59291 = CARTESIAN_POINT ( 'NONE',  ( 86.77126352523141861, 4.472830434245839371, 4.472830434245842035 ) ) ;
#59292 = ORIENTED_EDGE ( 'NONE', *, *, #138047, .T. ) ;
#59293 = EDGE_CURVE ( 'NONE', #89747, #107875, #30532, .T. ) ;
#59294 = VECTOR ( 'NONE', #73199, 999.9999999999998863 ) ;
#59295 = CARTESIAN_POINT ( 'NONE',  ( 24.39999999999999858, 1.399999999999987699, -20.40202195861970580 ) ) ;
#59296 = DIRECTION ( 'NONE',  ( 0.6830127018922180770, -0.6830127018922204085, -0.2588190451025213501 ) ) ;
#59297 = DIRECTION ( 'NONE',  ( -0.7071067811865486830, -0.7071067811865464625, 0.000000000000000000 ) ) ;
#59298 = DIRECTION ( 'NONE',  ( -0.6830127018922181881, 0.6830127018922202975, -0.2588190451025214056 ) ) ;
#59299 = VERTEX_POINT ( 'NONE', #21053 ) ;
#59300 = EDGE_CURVE ( 'NONE', #140903, #67994, #6975, .T. ) ;
#59301 = DIRECTION ( 'NONE',  ( 0.3543493200069162685, -0.000000000000000000, -0.9351131265310288487 ) ) ;
#59302 = CARTESIAN_POINT ( 'NONE',  ( 73.55793019189812298, 6.110000000000000320, -1.637169565754156064 ) ) ;
#59303 = ORIENTED_EDGE ( 'NONE', *, *, #6532, .F. ) ;
#59304 = AXIS2_PLACEMENT_3D ( 'NONE', #101100, #77945, #22792 ) ;
#59305 = LINE ( 'NONE', #112927, #136884 ) ;
#59306 = CARTESIAN_POINT ( 'NONE',  ( -9.328169399223463998, -18.74070752338408852, 4.000000000000000000 ) ) ;
#59307 = EDGE_CURVE ( 'NONE', #26888, #12905, #43983, .T. ) ;
#59308 = DIRECTION ( 'NONE',  ( 0.6830127018922181881, 0.6830127018922202975, -0.2588190451025214056 ) ) ;
#59309 = ORIENTED_EDGE ( 'NONE', *, *, #19568, .F. ) ;
#59310 = ORIENTED_EDGE ( 'NONE', *, *, #103845, .F. ) ;
#59311 = DIRECTION ( 'NONE',  ( -0.6830127018922180770, -0.6830127018922204085, -0.2588190451025213501 ) ) ;
#59312 = FILL_AREA_STYLE ('',( #102797 ) ) ;
#59313 = CARTESIAN_POINT ( 'NONE',  ( 21.94206980810188057, 7.934999999999992504, 2.126176841940951689 ) ) ;
#59314 = FACE_OUTER_BOUND ( 'NONE', #6338, .T. ) ;
#59315 = ADVANCED_FACE ( 'NONE', ( #66719 ), #119632, .F. ) ;
#59316 = CARTESIAN_POINT ( 'NONE',  ( 3.062159117892274018, -48.47815212813052455, -38.14157743968407033 ) ) ;
#59317 = CIRCLE ( 'NONE', #15174, 2.500000000000000444 ) ;
#59318 = DIRECTION ( 'NONE',  ( -0.7071067811865487940, 0.7071067811865463515, 0.000000000000000000 ) ) ;
#59319 = DIRECTION ( 'NONE',  ( -0.7071067811865486830, -0.7071067811865464625, 0.000000000000000000 ) ) ;
#59320 = EDGE_CURVE ( 'NONE', #103659, #114199, #33415, .T. ) ;
#59321 = VECTOR ( 'NONE', #72851, 1000.000000000000000 ) ;
#59322 = VERTEX_POINT ( 'NONE', #131988 ) ;
#59323 = EDGE_LOOP ( 'NONE', ( #77161, #132965 ) ) ;
#59324 = AXIS2_PLACEMENT_3D ( 'NONE', #3573, #4247, #47866 ) ;
#59325 = CARTESIAN_POINT ( 'NONE',  ( 9.333333333333333925, 5.278424836066143655, -3.047499999999997655 ) ) ;
#59326 = ORIENTED_EDGE ( 'NONE', *, *, #23702, .F. ) ;
#59327 = AXIS2_PLACEMENT_3D ( 'NONE', #29767, #72632, #95754 ) ;
#59328 = EDGE_CURVE ( 'NONE', #89130, #81231, #128176, .T. ) ;
#59329 = CARTESIAN_POINT ( 'NONE',  ( -10.17183060077640100, -5.240707523384232402, 4.000000000000000000 ) ) ;
#59330 = ORIENTED_EDGE ( 'NONE', *, *, #38086, .F. ) ;
#59331 = CARTESIAN_POINT ( 'NONE',  ( 69.78752705046289861, 0.000000000000000000, -7.949999999999998401 ) ) ;
#59332 = DIRECTION ( 'NONE',  ( 0.6830127018922181881, 0.6830127018922202975, -0.2588190451025214056 ) ) ;
#59333 = CARTESIAN_POINT ( 'NONE',  ( 69.18398860626899705, 28.73617430169835529, 5.000000000000000000 ) ) ;
#59334 = PLANE ( 'NONE',  #56103 ) ;
#59335 = ORIENTED_EDGE ( 'NONE', *, *, #18785, .F. ) ;
#59336 = LINE ( 'NONE', #4128, #44920 ) ;
#59337 = DIRECTION ( 'NONE',  ( 0.3543493200069162685, -0.000000000000000000, -0.9351131265310288487 ) ) ;
#59338 = VERTEX_POINT ( 'NONE', #141420 ) ;
#59339 = CARTESIAN_POINT ( 'NONE',  ( -32.27718569542918203, -21.72500000000000142, 5.000000000000000000 ) ) ;
#59340 = EDGE_LOOP ( 'NONE', ( #140894, #64270, #44767, #64816 ) ) ;
#59341 = ORIENTED_EDGE ( 'NONE', *, *, #97701, .T. ) ;
#59342 = CARTESIAN_POINT ( 'NONE',  ( 26.12840764549667583, 9.139736423841732040E-16, 0.000000000000000000 ) ) ;
#59343 = ORIENTED_EDGE ( 'NONE', *, *, #16515, .F. ) ;
#59344 = VERTEX_POINT ( 'NONE', #11582 ) ;
#59345 = CARTESIAN_POINT ( 'NONE',  ( 71.75043019189811844, 3.055000000000002824, -5.291415217122919401 ) ) ;
#59346 = EDGE_LOOP ( 'NONE', ( #44309, #134765, #23864, #25002 ) ) ;
#59347 = DIRECTION ( 'NONE',  ( -0.7071067811865486830, -0.7071067811865464625, 0.000000000000000000 ) ) ;
#59348 = DIRECTION ( 'NONE',  ( -0.7071067811865486830, -0.7071067811865464625, 0.000000000000000000 ) ) ;
#59349 = CARTESIAN_POINT ( 'NONE',  ( 118.5629301918981042, 1.637169565754157174, 6.110000000000002984 ) ) ;
#59350 = CARTESIAN_POINT ( 'NONE',  ( 24.18398860626899705, 28.73617430169804265, 5.000000000000000000 ) ) ;
#59351 = EDGE_CURVE ( 'NONE', #20496, #38971, #69561, .T. ) ;
#59352 = DIRECTION ( 'NONE',  ( -0.000000000000000000, 0.3543493200069153248, 0.9351131265310292928 ) ) ;
#59353 = FACE_BOUND ( 'NONE', #10647, .T. ) ;
#59354 = VECTOR ( 'NONE', #73679, 1000.000000000000000 ) ;
#59355 = CARTESIAN_POINT ( 'NONE',  ( -36.18398860626899705, 28.73617430169812437, 5.000000000000000000 ) ) ;
#59356 = DIRECTION ( 'NONE',  ( -1.000000000000000000, -0.000000000000000000, -0.000000000000000000 ) ) ;
#59357 = ORIENTED_EDGE ( 'NONE', *, *, #118976, .F. ) ;
#59358 = FACE_OUTER_BOUND ( 'NONE', #123031, .T. ) ;
#59359 = DIRECTION ( 'NONE',  ( -1.000000000000000000, 0.000000000000000000, -0.000000000000000000 ) ) ;
#59360 = EDGE_LOOP ( 'NONE', ( #135284, #38628, #31430, #89774 ) ) ;
#59361 = ORIENTED_EDGE ( 'NONE', *, *, #58790, .F. ) ;
#59362 = VECTOR ( 'NONE', #95929, 1000.000000000000227 ) ;
#59363 = CARTESIAN_POINT ( 'NONE',  ( -7.140000000000001457, -35.14999999999999147, -40.00000000000000000 ) ) ;
#59364 = EDGE_LOOP ( 'NONE', ( #90746, #19587, #139231, #49238 ) ) ;
#59365 =( BOUNDED_CURVE ( )  B_SPLINE_CURVE ( 2, ( #107334, #74008, #41357, #73305, #108020, #83461, #128396, #117475, #85571, #51553, #129802, #84875, #42111 ),
 .UNSPECIFIED., .F., .T. ) 
 B_SPLINE_CURVE_WITH_KNOTS ( ( 3, 2, 2, 2, 2, 2, 3 ),
 ( 0.7500000000000000000, 0.7527777777777777679, 0.7555555555555555358, 0.7583333333333333037, 0.7611111111111109606, 0.7638888888888887285, 0.7666666666666666075 ),
 .UNSPECIFIED. ) 
 CURVE ( )  GEOMETRIC_REPRESENTATION_ITEM ( )  RATIONAL_B_SPLINE_CURVE ( ( 1.000000000000000000, 0.9659258262890683122, 1.000000000000000000, 0.9659258262890683122, 1.000000000000000000, 0.9659258262890683122, 1.000000000000000000, 0.9659258262890683122, 1.000000000000000000, 0.9659258262890683122, 1.000000000000000000, 0.9659258262890696445, 0.9999999999999986677 ) ) 
 REPRESENTATION_ITEM ( '' )  );
#59366 = PLANE ( 'NONE',  #7402 ) ;
#59367 = LINE ( 'NONE', #70267, #121890 ) ;
#59368 = EDGE_CURVE ( 'NONE', #18045, #9940, #118943, .T. ) ;
#59369 = CARTESIAN_POINT ( 'NONE',  ( -5.540161610502567058, 18.75929247661553489, 8.305906642995470435 ) ) ;
#59370 = CARTESIAN_POINT ( 'NONE',  ( 11.62000000000000099, -2.055000000000000160, 0.000000000000000000 ) ) ;
#59371 = ORIENTED_EDGE ( 'NONE', *, *, #29296, .F. ) ;
#59372 = EDGE_CURVE ( 'NONE', #138330, #64517, #86342, .T. ) ;
#59373 = CARTESIAN_POINT ( 'NONE',  ( -20.99451991528748707, 28.92564299267952777, 4.000000000000000000 ) ) ;
#59374 = VERTEX_POINT ( 'NONE', #97921 ) ;
#59376 = EDGE_CURVE ( 'NONE', #88631, #100364, #110897, .T. ) ;
#59375 = CARTESIAN_POINT ( 'NONE',  ( -29.99999999999978684, -10.06887692260770883, 4.000000000000000000 ) ) ;
#59377 = VECTOR ( 'NONE', #50399, 1000.000000000000227 ) ;
#59378 = CARTESIAN_POINT ( 'NONE',  ( 32.58790314143522693, 6.871911579029515771, 3.967499999999989146 ) ) ;
#59379 = DIRECTION ( 'NONE',  ( 1.000000000000000000, 0.000000000000000000, 0.000000000000000000 ) ) ;
#59380 = VECTOR ( 'NONE', #53388, 999.9999999999998863 ) ;
#59381 = EDGE_CURVE ( 'NONE', #86236, #113805, #83406, .T. ) ;
#59382 = LINE ( 'NONE', #103537, #69833 ) ;
#59383 = ORIENTED_EDGE ( 'NONE', *, *, #23332, .F. ) ;
#59384 = ORIENTED_EDGE ( 'NONE', *, *, #139127, .F. ) ;
#59385 = ORIENTED_EDGE ( 'NONE', *, *, #94440, .T. ) ;
#59386 = CARTESIAN_POINT ( 'NONE',  ( -1.179999999999998384, -9.043340090917736163, 10.00000000000000000 ) ) ;
#59387 = DIRECTION ( 'NONE',  ( 0.3543493200069162685, -0.000000000000000000, -0.9351131265310288487 ) ) ;
#59388 = DIRECTION ( 'NONE',  ( -0.3543493200069162685, -0.000000000000000000, -0.9351131265310288487 ) ) ;
#59389 = SURFACE_STYLE_FILL_AREA ( #16540 ) ;
#59390 = VERTEX_POINT ( 'NONE', #65320 ) ;
#59391 = PLANE ( 'NONE',  #76355 ) ;
#59392 = DIRECTION ( 'NONE',  ( 0.7071067811865486830, -0.7071067811865464625, -0.000000000000000000 ) ) ;
#59393 = EDGE_CURVE ( 'NONE', #98666, #125641, #109504, .T. ) ;
#59394 = DIRECTION ( 'NONE',  ( 0.5735764363510453823, -0.8191520442889923537, 1.003171929053525486E-16 ) ) ;
#59395 = AXIS2_PLACEMENT_3D ( 'NONE', #71602, #29494, #115055 ) ;
#59396 = LINE ( 'NONE', #138353, #16472 ) ;
#59397 = DIRECTION ( 'NONE',  ( -0.7071067811865486830, 0.7071067811865464625, 0.000000000000000000 ) ) ;
#59398 = ORIENTED_EDGE ( 'NONE', *, *, #42689, .T. ) ;
#59399 = DIRECTION ( 'NONE',  ( -0.3543493200069162685, -0.000000000000000000, -0.9351131265310288487 ) ) ;
#59400 = EDGE_CURVE ( 'NONE', #103174, #127004, #55866, .T. ) ;
#59401 = DIRECTION ( 'NONE',  ( 0.7071067811865487940, 0.7071067811865463515, 0.000000000000000000 ) ) ;
#59402 = ORIENTED_EDGE ( 'NONE', *, *, #92753, .T. ) ;
#59404 = ORIENTED_EDGE ( 'NONE', *, *, #133646, .T. ) ;
#59403 = CARTESIAN_POINT ( 'NONE',  ( 59.70964273381705567, -44.90675832754596541, -35.11767176073973218 ) ) ;
#59405 = AXIS2_PLACEMENT_3D ( 'NONE', #75317, #53553, #110744 ) ;
#59406 = ORIENTED_EDGE ( 'NONE', *, *, #142880, .F. ) ;
#59407 = DIRECTION ( 'NONE',  ( 0.7071067811865486830, -0.7071067811865464625, -0.000000000000000000 ) ) ;
#59408 = DIRECTION ( 'NONE',  ( 0.000000000000000000, -1.000000000000000000, 0.000000000000000000 ) ) ;
#59409 = DIRECTION ( 'NONE',  ( -0.7071067811865486830, -0.7071067811865464625, -0.000000000000000000 ) ) ;
#59410 = EDGE_CURVE ( 'NONE', #133459, #124676, #15162, .T. ) ;
#59411 = EDGE_LOOP ( 'NONE', ( #47162, #91012, #22418, #5755, #84418, #17958 ) ) ;
#59412 = CARTESIAN_POINT ( 'NONE',  ( -8.510786437626906675, -27.52281430457049183, 5.000000000000000000 ) ) ;
#59413 = UNCERTAINTY_MEASURE_WITH_UNIT (LENGTH_MEASURE( 1.000000000000000082E-05 ), #120046, 'distance_accuracy_value', 'NONE');
#59414 = ORIENTED_EDGE ( 'NONE', *, *, #116171, .T. ) ;
#59415 = CARTESIAN_POINT ( 'NONE',  ( 39.29974487139159578, -27.71228299555233576, 4.000000000000000000 ) ) ;
#59416 = CARTESIAN_POINT ( 'NONE',  ( -7.499999999999951150, 9.431123077392088661, 4.000000000000000000 ) ) ;
#59418 = CARTESIAN_POINT ( 'NONE',  ( 128.9958603837962414, -3.974999999999998312, -6.884901960086286188 ) ) ;
#59417 = VECTOR ( 'NONE', #29820, 999.9999999999998863 ) ;
#59419 = DIRECTION ( 'NONE',  ( -0.7071067811865486830, -0.7071067811865464625, -0.000000000000000000 ) ) ;
#59420 = DIRECTION ( 'NONE',  ( 0.7071067811865487940, 0.7071067811865463515, -0.000000000000000000 ) ) ;
#59421 = PLANE ( 'NONE',  #19043 ) ;
#59423 = EDGE_CURVE ( 'NONE', #123892, #4072, #67461, .T. ) ;
#59422 = DIRECTION ( 'NONE',  ( -0.7071067811865487940, 0.7071067811865463515, 0.000000000000000000 ) ) ;
#59424 = CARTESIAN_POINT ( 'NONE',  ( -0.7071067811865363595, -9.740707523384179112, 5.000000000000000000 ) ) ;
#59425 = CARTESIAN_POINT ( 'NONE',  ( 30.89540314143522437, 2.126176841940962348, 7.934999999999989839 ) ) ;
#59426 = DIRECTION ( 'NONE',  ( -0.000000000000000000, 0.000000000000000000, 1.000000000000000000 ) ) ;
#59427 = CARTESIAN_POINT ( 'NONE',  ( 13.17183060077638324, 18.75929247661553134, 4.000000000000000000 ) ) ;
#59428 = VECTOR ( 'NONE', #134848, 1000.000000000000000 ) ;
#59429 = DIRECTION ( 'NONE',  ( 0.000000000000000000, 0.000000000000000000, -1.000000000000000000 ) ) ;
#59430 = FACE_OUTER_BOUND ( 'NONE', #37364, .T. ) ;
#59431 = ORIENTED_EDGE ( 'NONE', *, *, #67320, .T. ) ;
#59433 = EDGE_LOOP ( 'NONE', ( #25201, #71750, #842, #35208 ) ) ;
#59432 = EDGE_CURVE ( 'NONE', #46912, #25963, #2871, .T. ) ;
#59434 = EDGE_CURVE ( 'NONE', #57383, #34999, #34105, .T. ) ;
#59435 = CARTESIAN_POINT ( 'NONE',  ( 94.62500000000000000, -7.950000000000000178, -4.867971026610729436E-16 ) ) ;
#59436 = ORIENTED_EDGE ( 'NONE', *, *, #77385, .F. ) ;
#59437 = VERTEX_POINT ( 'NONE', #78314 ) ;
#59438 = CARTESIAN_POINT ( 'NONE',  ( 23.96247294953710849, -7.464222240803106570E-16, -6.094999999999989981 ) ) ;
#59439 = FACE_OUTER_BOUND ( 'NONE', #4421, .T. ) ;
#59440 = ORIENTED_EDGE ( 'NONE', *, *, #66847, .T. ) ;
#59441 = DIRECTION ( 'NONE',  ( 1.000000000000000000, 0.000000000000000000, 0.000000000000000000 ) ) ;
#59442 = EDGE_CURVE ( 'NONE', #25054, #129819, #129641, .T. ) ;
#59443 = CARTESIAN_POINT ( 'NONE',  ( 62.99451991528749772, 28.92564299267982264, 4.000000000000000000 ) ) ;
#59444 = LINE ( 'NONE', #36933, #58065 ) ;
#59445 = CARTESIAN_POINT ( 'NONE',  ( 25.39999999999999858, 0.000000000000000000, 6.094999999999989093 ) ) ;
#59446 = EDGE_CURVE ( 'NONE', #84209, #89560, #70335, .T. ) ;
#59447 = CARTESIAN_POINT ( 'NONE',  ( -23.99999999999983302, 17.96639925780207747, 5.000000000000000000 ) ) ;
#59448 = FACE_OUTER_BOUND ( 'NONE', #19170, .T. ) ;
#59449 = DIRECTION ( 'NONE',  ( -0.6830127018922180770, -0.6830127018922204085, -0.2588190451025213501 ) ) ;
#59450 = DIRECTION ( 'NONE',  ( -0.7071067811865486830, 0.7071067811865464625, 0.000000000000000000 ) ) ;
#59451 = CARTESIAN_POINT ( 'NONE',  ( 24.97566027651206610, 3.896288752498338948, 4.156157854036514721 ) ) ;
#59452 = DIRECTION ( 'NONE',  ( -0.7071067811865487940, 0.7071067811865463515, 0.000000000000000000 ) ) ;
#59453 = PLANE ( 'NONE',  #61494 ) ;
#59454 = ORIENTED_EDGE ( 'NONE', *, *, #142426, .F. ) ;
#59455 = ORIENTED_EDGE ( 'NONE', *, *, #9422, .F. ) ;
#59456 = CARTESIAN_POINT ( 'NONE',  ( 107.4795968585647614, 6.109999999999999432, 1.637169565754164280 ) ) ;
#59457 = ORIENTED_EDGE ( 'NONE', *, *, #12983, .F. ) ;
#59458 = EDGE_CURVE ( 'NONE', #126942, #106637, #123967, .T. ) ;
#59459 = CARTESIAN_POINT ( 'NONE',  ( 26.67183060077628909, 20.25929247661551358, 4.000000000000000000 ) ) ;
#59460 = AXIS2_PLACEMENT_3D ( 'NONE', #123285, #113807, #23956 ) ;
#59461 = CARTESIAN_POINT ( 'NONE',  ( 0.000000000000000000, -30.18000000000009564, 12.69999999999954454 ) ) ;
#59462 = ORIENTED_EDGE ( 'NONE', *, *, #20911, .T. ) ;
#59463 = ADVANCED_FACE ( 'NONE', ( #122502 ), #124661, .T. ) ;
#59464 = DIRECTION ( 'NONE',  ( -0.7071067811865486830, -0.7071067811865463515, 0.000000000000000000 ) ) ;
#59465 = DIRECTION ( 'NONE',  ( -1.000000000000000000, -1.224606353822377258E-16, -0.000000000000000000 ) ) ;
#59466 = CARTESIAN_POINT ( 'NONE',  ( 101.2662635252314374, 4.472830434245839371, -4.472830434245838482 ) ) ;
#59467 = ORIENTED_EDGE ( 'NONE', *, *, #31553, .T. ) ;
#59468 = VERTEX_POINT ( 'NONE', #24629 ) ;
#59469 = CARTESIAN_POINT ( 'NONE',  ( -11.81601139373100651, 28.73617430169779041, 5.000000000000000000 ) ) ;
#59470 = AXIS2_PLACEMENT_3D ( 'NONE', #118204, #63875, #8019 ) ;
#59471 = FILL_AREA_STYLE_COLOUR ( '', #35335 ) ;
#59472 = DIRECTION ( 'NONE',  ( -0.7071067811865486830, -0.7071067811865464625, 0.000000000000000000 ) ) ;
#59473 = EDGE_LOOP ( 'NONE', ( #59860, #83475, #1552, #4121 ) ) ;
#59474 = EDGE_LOOP ( 'NONE', ( #80203, #54168, #65886, #78025, #97710 ) ) ;
#59475 = VECTOR ( 'NONE', #140575, 1000.000000000000000 ) ;
#59476 = ORIENTED_EDGE ( 'NONE', *, *, #58758, .T. ) ;
#59477 = CARTESIAN_POINT ( 'NONE',  ( -24.75149461641275295, 4.949500604449031727, 4.299609778361313417 ) ) ;
#59478 = CARTESIAN_POINT ( 'NONE',  ( 0.7962364747685526378, 7.934999999999990727, -1.457635852685135314E-15 ) ) ;
#59479 = EDGE_CURVE ( 'NONE', #48159, #42968, #81177, .T. ) ;
#59480 = FILL_AREA_STYLE ('',( #70378 ) ) ;
#59481 = VERTEX_POINT ( 'NONE', #112368 ) ;
#59482 = VECTOR ( 'NONE', #106135, 1000.000000000000000 ) ;
#59483 = VERTEX_POINT ( 'NONE', #36929 ) ;
#59484 = CARTESIAN_POINT ( 'NONE',  ( -32.99451991528749062, 28.92564299267960948, 4.000000000000000000 ) ) ;
#59485 = EDGE_LOOP ( 'NONE', ( #4706, #19640, #7650 ) ) ;
#59486 = ORIENTED_EDGE ( 'NONE', *, *, #65496, .T. ) ;
#59487 = FACE_OUTER_BOUND ( 'NONE', #34858, .T. ) ;
#59488 = CARTESIAN_POINT ( 'NONE',  ( 27.48921356237309155, -27.52281430457074762, 5.000000000000000000 ) ) ;
#59489 = VERTEX_POINT ( 'NONE', #58753 ) ;
#59490 = DIRECTION ( 'NONE',  ( 0.7071067811865487940, 0.7071067811865463515, 0.000000000000000000 ) ) ;
#59491 = DIRECTION ( 'NONE',  ( 0.6830127018922180770, -0.6830127018922204085, -0.2588190451025213501 ) ) ;
#59492 = DIRECTION ( 'NONE',  ( 0.7071067811865486830, -0.7071067811865464625, -0.000000000000000000 ) ) ;
#59493 = DIRECTION ( 'NONE',  ( 0.7071067811865487940, -0.7071067811865463515, 0.000000000000000000 ) ) ;
#59494 = DIRECTION ( 'NONE',  ( 0.000000000000000000, -1.000000000000000000, 0.000000000000000000 ) ) ;
#59496 = FACE_BOUND ( 'NONE', #74357, .T. ) ;
#59495 = VECTOR ( 'NONE', #120760, 999.9999999999998863 ) ;
#59497 = ORIENTED_EDGE ( 'NONE', *, *, #30848, .F. ) ;
#59498 = CARTESIAN_POINT ( 'NONE',  ( 31.49999999999979039, 4.087461875839202285, 4.000000000000000000 ) ) ;
#59499 = DIRECTION ( 'NONE',  ( 1.000000000000000000, 0.000000000000000000, 0.000000000000000000 ) ) ;
#59500 = CARTESIAN_POINT ( 'NONE',  ( -12.48921356237309155, -27.52281430457064104, 5.000000000000000000 ) ) ;
#59501 = ORIENTED_EDGE ( 'NONE', *, *, #112706, .F. ) ;
#59502 = CARTESIAN_POINT ( 'NONE',  ( 8.811592354503320124, -2.500000000000000000, 3.061616997868384127E-16 ) ) ;
#59503 = ORIENTED_EDGE ( 'NONE', *, *, #17190, .F. ) ;
#59504 = VERTEX_POINT ( 'NONE', #111654 ) ;
#59505 = AXIS2_PLACEMENT_3D ( 'NONE', #21479, #109903, #52661 ) ;
#59506 = ORIENTED_EDGE ( 'NONE', *, *, #114859, .F. ) ;
#59507 = VECTOR ( 'NONE', #105956, 1000.000000000000000 ) ;
#59508 = CARTESIAN_POINT ( 'NONE',  ( 35.64126352523145158, 4.472830434245835818, 4.472830434245840259 ) ) ;
#59509 = ORIENTED_EDGE ( 'NONE', *, *, #96244, .F. ) ;
#59510 = CARTESIAN_POINT ( 'NONE',  ( 12.19999999999999574, 0.000000000000000000, -39.50000000000000000 ) ) ;
#59511 = CARTESIAN_POINT ( 'NONE',  ( -26.20710678118636139, -11.24070752338416845, 5.000000000000000000 ) ) ;
#59512 = LINE ( 'NONE', #37755, #12645 ) ;
#59513 = CIRCLE ( 'NONE', #140502, 2.500000000000000888 ) ;
#59514 = VERTEX_POINT ( 'NONE', #69602 ) ;
#59515 = DIRECTION ( 'NONE',  ( -1.000000000000000000, -0.000000000000000000, -0.000000000000000000 ) ) ;
#59516 = FILL_AREA_STYLE ('',( #80550 ) ) ;
#59517 = CONICAL_SURFACE ( 'NONE', #91876, 2.500000000000000888, 0.9599310885968822538 ) ;
#59518 = DIRECTION ( 'NONE',  ( 0.3543493200069162685, -0.000000000000000000, -0.9351131265310288487 ) ) ;
#59519 = CARTESIAN_POINT ( 'NONE',  ( -16.49999999999988631, 21.43112307739196609, 4.000000000000000000 ) ) ;
#59520 = LINE ( 'NONE', #104409, #41701 ) ;
#59521 = CARTESIAN_POINT ( 'NONE',  ( -34.49999999999976552, 18.05432934483075513, 4.994342998332167660 ) ) ;
#59522 = CARTESIAN_POINT ( 'NONE',  ( -39.29974487139159578, -27.71228299555233576, 4.000000000000000000 ) ) ;
#59523 = ORIENTED_EDGE ( 'NONE', *, *, #58480, .T. ) ;
#59524 = EDGE_CURVE ( 'NONE', #44351, #54134, #113055, .T. ) ;
#59525 = VERTEX_POINT ( 'NONE', #102922 ) ;
#59526 = ORIENTED_EDGE ( 'NONE', *, *, #83780, .F. ) ;
#59527 = ORIENTED_EDGE ( 'NONE', *, *, #57998, .F. ) ;
#59528 = DIRECTION ( 'NONE',  ( 0.7071067811865487940, 0.7071067811865463515, -0.000000000000000000 ) ) ;
#59529 = EDGE_LOOP ( 'NONE', ( #56387, #139547, #74839, #9839 ) ) ;
#59531 = EDGE_LOOP ( 'NONE', ( #30549, #20785, #111541, #37962 ) ) ;
#59530 = ADVANCED_FACE ( 'NONE', ( #79060 ), #114481, .F. ) ;
#59532 = DIRECTION ( 'NONE',  ( -0.7071067811865486830, 0.7071067811865464625, 0.000000000000000000 ) ) ;
#59533 = EDGE_CURVE ( 'NONE', #75066, #13817, #57980, .T. ) ;
#59534 = EDGE_CURVE ( 'NONE', #23978, #102891, #101474, .T. ) ;
#59535 = DIRECTION ( 'NONE',  ( 0.7071067811865487940, 0.7071067811865463515, 0.000000000000000000 ) ) ;
#59536 = EDGE_LOOP ( 'NONE', ( #112252, #90942, #103443, #27063 ) ) ;
#59537 = VECTOR ( 'NONE', #2053, 999.9999999999998863 ) ;
#59538 = DIRECTION ( 'NONE',  ( -0.6830127018922180770, -0.6830127018922204085, -0.2588190451025213501 ) ) ;
#59539 = ORIENTED_EDGE ( 'NONE', *, *, #55361, .T. ) ;
#59540 =( BOUNDED_CURVE ( )  B_SPLINE_CURVE ( 2, ( #34527, #66458, #69310, #77357, #110624, #46894, #122966, #79512, #132457, #12750, #57024, #55580, #89610 ),
 .UNSPECIFIED., .F., .T. ) 
 B_SPLINE_CURVE_WITH_KNOTS ( ( 3, 2, 2, 2, 2, 2, 3 ),
 ( 0.3666666666666666963, 0.3694444444444445197, 0.3722222222222222876, 0.3750000000000000555, 0.3777777777777778234, 0.3805555555555555913, 0.3833333333333334147 ),
 .UNSPECIFIED. ) 
 CURVE ( )  GEOMETRIC_REPRESENTATION_ITEM ( )  RATIONAL_B_SPLINE_CURVE ( ( 0.9999999999999993339, 0.9659258262890689783, 1.000000000000000000, 0.9659258262890683122, 1.000000000000000000, 0.9659258262890683122, 1.000000000000000000, 0.9659258262890683122, 1.000000000000000000, 0.9659258262890683122, 1.000000000000000000, 0.9659258262890676461, 1.000000000000000666 ) ) 
 REPRESENTATION_ITEM ( '' )  );
#59541 = ADVANCED_FACE ( 'NONE', ( #23936 ), #100772, .F. ) ;
#59542 = EDGE_CURVE ( 'NONE', #19458, #86645, #89879, .T. ) ;
#59543 = VECTOR ( 'NONE', #116165, 1000.000000000000000 ) ;
#59544 = ORIENTED_EDGE ( 'NONE', *, *, #30079, .F. ) ;
#59546 = DIRECTION ( 'NONE',  ( 0.000000000000000000, 0.000000000000000000, -1.000000000000000000 ) ) ;
#59545 = CARTESIAN_POINT ( 'NONE',  ( 103.7454301918981230, -5.291415217122919401, -3.055000000000000604 ) ) ;
#59547 = EDGE_CURVE ( 'NONE', #98924, #64888, #47169, .T. ) ;
#59548 = CARTESIAN_POINT ( 'NONE',  ( 27.18398860626900060, 28.73617430169806042, 5.000000000000000000 ) ) ;
#59549 = CARTESIAN_POINT ( 'NONE',  ( 6.183988606268994381, 28.73617430169791476, 5.000000000000000000 ) ) ;
#59550 = ORIENTED_EDGE ( 'NONE', *, *, #35190, .T. ) ;
#59551 = EDGE_LOOP ( 'NONE', ( #13455, #1739, #55656, #140820 ) ) ;
#59552 = EDGE_LOOP ( 'NONE', ( #95800, #11119, #90513, #11309 ) ) ;
#59553 = CARTESIAN_POINT ( 'NONE',  ( -74.99451991528749772, 28.92564299267990435, 4.000000000000000000 ) ) ;
#59554 = CARTESIAN_POINT ( 'NONE',  ( 0.000000000000000000, 0.000000000000000000, 5.000000000000000000 ) ) ;
#59555 = DIRECTION ( 'NONE',  ( 0.000000000000000000, -1.000000000000000000, 0.000000000000000000 ) ) ;
#59556 = DIRECTION ( 'NONE',  ( -0.6830127018922180770, -0.6830127018922204085, -0.2588190451025213501 ) ) ;
#59557 = DIRECTION ( 'NONE',  ( -1.000000000000000000, -0.000000000000000000, -0.000000000000000000 ) ) ;
#59558 = VERTEX_POINT ( 'NONE', #58019 ) ;
#59559 = LINE ( 'NONE', #126901, #52903 ) ;
#59560 = EDGE_CURVE ( 'NONE', #125176, #35489, #102219, .T. ) ;
#59561 = CARTESIAN_POINT ( 'NONE',  ( 26.51078643762690845, -27.52281430457036748, 5.000000000000000000 ) ) ;
#59562 = CARTESIAN_POINT ( 'NONE',  ( 48.48921356237309510, -27.52281430457089328, 5.000000000000000000 ) ) ;
#59563 = VECTOR ( 'NONE', #13020, 1000.000000000000000 ) ;
#59564 = ORIENTED_EDGE ( 'NONE', *, *, #97132, .F. ) ;
#59565 = DIRECTION ( 'NONE',  ( 1.000000000000000000, 0.000000000000000000, 0.000000000000000000 ) ) ;
#59566 = CARTESIAN_POINT ( 'NONE',  ( -23.99999999999982592, -6.033600742197678279, 5.000000000000000000 ) ) ;
#59567 = EDGE_LOOP ( 'NONE', ( #2834, #136094, #131770, #84313 ) ) ;
#59568 = VECTOR ( 'NONE', #115768, 999.9999999999998863 ) ;
#59570 = ORIENTED_EDGE ( 'NONE', *, *, #66299, .F. ) ;
#59569 = DIRECTION ( 'NONE',  ( -0.7071067811865486830, -0.7071067811865464625, 0.000000000000000000 ) ) ;
#59571 = ORIENTED_EDGE ( 'NONE', *, *, #54876, .F. ) ;
#59572 = CARTESIAN_POINT ( 'NONE',  ( 3.299744871391591339, -27.71228299555208352, 4.000000000000000000 ) ) ;
#59573 = PLANE ( 'NONE',  #32170 ) ;
#59574 = ADVANCED_FACE ( 'NONE', ( #73160 ), #126105, .F. ) ;
#59575 = ORIENTED_EDGE ( 'NONE', *, *, #10159, .T. ) ;
#59576 = FACE_OUTER_BOUND ( 'NONE', #58050, .T. ) ;
#59577 = DIRECTION ( 'NONE',  ( -0.6830127018922181881, 0.6830127018922202975, -0.2588190451025214056 ) ) ;
#59578 = VECTOR ( 'NONE', #42910, 1000.000000000000000 ) ;
#59579 = EDGE_LOOP ( 'NONE', ( #126645, #140624, #136789, #27889 ) ) ;
#59580 = CARTESIAN_POINT ( 'NONE',  ( -26.99999999999980105, 5.587461875839189851, 4.000000000000000000 ) ) ;
#59581 = LINE ( 'NONE', #103742, #7192 ) ;
#59582 = DIRECTION ( 'NONE',  ( 0.3543493200069162685, -0.000000000000000000, -0.9351131265310288487 ) ) ;
#59584 = EDGE_CURVE ( 'NONE', #113044, #94978, #62276, .T. ) ;
#59583 = DIRECTION ( 'NONE',  ( 0.6830127018922181881, 0.6830127018922202975, -0.2588190451025214056 ) ) ;
#59585 = DIRECTION ( 'NONE',  ( 0.7071067811865486830, -0.7071067811865464625, -0.000000000000000000 ) ) ;
#59586 = DIRECTION ( 'NONE',  ( 0.000000000000000000, -1.000000000000000000, 0.000000000000000000 ) ) ;
#59587 = CARTESIAN_POINT ( 'NONE',  ( 28.37086038379622721, 6.884901960086289741, -3.974999999999993427 ) ) ;
#59588 = PLANE ( 'NONE',  #70902 ) ;
#59589 = ORIENTED_EDGE ( 'NONE', *, *, #30885, .F. ) ;
#59590 = ORIENTED_EDGE ( 'NONE', *, *, #25696, .F. ) ;
#59591 = ORIENTED_EDGE ( 'NONE', *, *, #49428, .F. ) ;
#59592 = EDGE_CURVE ( 'NONE', #129767, #119756, #103598, .T. ) ;
#59593 = CARTESIAN_POINT ( 'NONE',  ( 116.2083333333333286, -3.974999999999999201, -6.884901960086287964 ) ) ;
#59594 = ORIENTED_EDGE ( 'NONE', *, *, #31839, .T. ) ;
#59595 = ORIENTED_EDGE ( 'NONE', *, *, #72735, .T. ) ;
#59596 = ADVANCED_FACE ( 'NONE', ( #139121 ), #83306, .F. ) ;
#59597 = ORIENTED_EDGE ( 'NONE', *, *, #22168, .F. ) ;
#59598 = FACE_OUTER_BOUND ( 'NONE', #124749, .T. ) ;
#59599 = DIRECTION ( 'NONE',  ( -0.000000000000000000, 0.3543493200069153248, 0.9351131265310292928 ) ) ;
#59600 = EDGE_LOOP ( 'NONE', ( #26425, #54611, #6504, #101222 ) ) ;
#59601 = EDGE_CURVE ( 'NONE', #1535, #105294, #106430, .T. ) ;
#59602 = CARTESIAN_POINT ( 'NONE',  ( 16.49999999999988631, 15.43112307739202471, 4.000000000000000000 ) ) ;
#59603 = EDGE_CURVE ( 'NONE', #111091, #131639, #93465, .T. ) ;
#59604 = DIRECTION ( 'NONE',  ( 0.6830127018922181881, 0.6830127018922202975, -0.2588190451025214056 ) ) ;
#59605 = VECTOR ( 'NONE', #49140, 1000.000000000000227 ) ;
#59606 = DIRECTION ( 'NONE',  ( -0.7071067811865487940, 0.7071067811865463515, 0.000000000000000000 ) ) ;
#59607 = CARTESIAN_POINT ( 'NONE',  ( 112.4379301918981184, -6.110000000000001208, 1.637169565754158951 ) ) ;
#59608 = ORIENTED_EDGE ( 'NONE', *, *, #73471, .F. ) ;
#59609 = CARTESIAN_POINT ( 'NONE',  ( 25.49999999999983302, -8.947814304570739452, 5.000000000000000000 ) ) ;
#59610 = DIRECTION ( 'NONE',  ( 0.7071067811865487940, -0.7071067811865463515, 0.000000000000000000 ) ) ;
#59611 = CARTESIAN_POINT ( 'NONE',  ( -53.99451991528749062, 28.92564299267975869, 4.000000000000000000 ) ) ;
#59612 = FACE_OUTER_BOUND ( 'NONE', #135370, .T. ) ;
#59613 = CARTESIAN_POINT ( 'NONE',  ( 39.29974487139159578, -27.71228299555233576, 4.000000000000000000 ) ) ;
#59614 = EDGE_CURVE ( 'NONE', #142939, #28531, #84049, .T. ) ;
#59615 = VECTOR ( 'NONE', #3267, 1000.000000000000227 ) ;
#59616 = FACE_OUTER_BOUND ( 'NONE', #96884, .T. ) ;
#59617 = CARTESIAN_POINT ( 'NONE',  ( 4.288407645496676857, -3.851859888774471706E-31, 2.500000000000001332 ) ) ;
#59618 = VECTOR ( 'NONE', #54670, 1000.000000000000000 ) ;
#59619 = CARTESIAN_POINT ( 'NONE',  ( 34.64169371712954160, -2.130196079827424871, -7.949999999999999289 ) ) ;
#59620 = DIRECTION ( 'NONE',  ( -0.6830127018922180770, -0.6830127018922204085, -0.2588190451025213501 ) ) ;
#59621 = VECTOR ( 'NONE', #140713, 999.9999999999998863 ) ;
#59622 = DIRECTION ( 'NONE',  ( 0.000000000000000000, -1.000000000000000000, 5.075120898959324592E-15 ) ) ;
#59623 = ORIENTED_EDGE ( 'NONE', *, *, #102518, .F. ) ;
#59624 = ORIENTED_EDGE ( 'NONE', *, *, #41950, .F. ) ;
#59625 = CARTESIAN_POINT ( 'NONE',  ( 34.39583333333333570, -2.130196079827427091, 7.949999999999999289 ) ) ;
#59626 = VERTEX_POINT ( 'NONE', #37678 ) ;
#59627 = ORIENTED_EDGE ( 'NONE', *, *, #39758, .F. ) ;
#59628 = EDGE_CURVE ( 'NONE', #100056, #17934, #50666, .T. ) ;
#59629 = PLANE ( 'NONE',  #85666 ) ;
#59630 = DIRECTION ( 'NONE',  ( 0.000000000000000000, 0.000000000000000000, -1.000000000000000000 ) ) ;
#59631 = VECTOR ( 'NONE', #42162, 999.9999999999998863 ) ;
#59632 = ORIENTED_EDGE ( 'NONE', *, *, #13757, .F. ) ;
#59633 = FACE_OUTER_BOUND ( 'NONE', #118, .T. ) ;
#59634 = CARTESIAN_POINT ( 'NONE',  ( 13.49999999999990585, -13.53360074219760101, 5.000000000000000000 ) ) ;
#59635 = CARTESIAN_POINT ( 'NONE',  ( 0.000000000000000000, 0.000000000000000000, 0.000000000000000000 ) ) ;
#59636 = CARTESIAN_POINT ( 'NONE',  ( 26.68793019189810067, 6.110000000000002984, -1.637169565754156730 ) ) ;
#59637 = EDGE_LOOP ( 'NONE', ( #10694, #28330, #119691, #39139 ) ) ;
#59638 = CARTESIAN_POINT ( 'NONE',  ( 63.48921356237309510, -27.52281430457099631, 5.000000000000000000 ) ) ;
#59639 = EDGE_LOOP ( 'NONE', ( #79519, #38838, #30231, #50362, #116520, #29857 ) ) ;
#59640 = FACE_OUTER_BOUND ( 'NONE', #4751, .T. ) ;
#59641 = PLANE ( 'NONE',  #87014 ) ;
#59642 = DIRECTION ( 'NONE',  ( 0.7071067811865487940, 0.7071067811865463515, 0.000000000000000000 ) ) ;
#59643 = ORIENTED_EDGE ( 'NONE', *, *, #48408, .T. ) ;
#59644 = ADVANCED_FACE ( 'NONE', ( #115170 ), #141232, .T. ) ;
#59645 = ORIENTED_EDGE ( 'NONE', *, *, #75911, .T. ) ;
#59646 = CARTESIAN_POINT ( 'NONE',  ( -34.42499999999997584, 0.000000000000000000, 0.000000000000000000 ) ) ;
#59647 = PLANE ( 'NONE',  #60141 ) ;
#59648 = CARTESIAN_POINT ( 'NONE',  ( 1.171830600776468057, 21.75929247661549581, 4.000000000000000000 ) ) ;
#59649 = VECTOR ( 'NONE', #3296, 1000.000000000000227 ) ;
#59650 = LINE ( 'NONE', #102439, #92649 ) ;
#59651 = EDGE_CURVE ( 'NONE', #131487, #28495, #82587, .T. ) ;
#59652 = CARTESIAN_POINT ( 'NONE',  ( 48.76626352523144448, 4.472830434245839371, -4.472830434245838482 ) ) ;
#59653 = EDGE_LOOP ( 'NONE', ( #131702, #94892, #41228, #7907 ) ) ;
#59654 = LINE ( 'NONE', #92232, #113658 ) ;
#59655 = CARTESIAN_POINT ( 'NONE',  ( -45.29974487139158867, -27.71228299555237840, 4.000000000000000000 ) ) ;
#59656 = VERTEX_POINT ( 'NONE', #4977 ) ;
#59657 = ORIENTED_EDGE ( 'NONE', *, *, #135980, .T. ) ;
#59658 = AXIS2_PLACEMENT_3D ( 'NONE', #129490, #99001, #143237 ) ;
#59659 = CARTESIAN_POINT ( 'NONE',  ( 3.299744871391591339, -27.71228299555208352, 4.000000000000000000 ) ) ;
#59660 = ORIENTED_EDGE ( 'NONE', *, *, #56801, .T. ) ;
#59661 = EDGE_CURVE ( 'NONE', #134832, #36043, #15846, .T. ) ;
#59662 =( BOUNDED_CURVE ( )  B_SPLINE_CURVE ( 3, ( #11470, #610, #67334, #33307 ),
 .UNSPECIFIED., .F., .T. ) 
 B_SPLINE_CURVE_WITH_KNOTS ( ( 4, 4 ),
 ( 4.350170835173026163, 4.500739107949258688 ),
 .UNSPECIFIED. ) 
 CURVE ( )  GEOMETRIC_REPRESENTATION_ITEM ( )  RATIONAL_B_SPLINE_CURVE ( ( 1.000000000000000000, 0.9981116584018945304, 0.9981116584018945304, 1.000000000000000000 ) ) 
 REPRESENTATION_ITEM ( '' )  );
#59663 = ADVANCED_FACE ( 'NONE', ( #49278 ), #138393, .F. ) ;
#59664 = CARTESIAN_POINT ( 'NONE',  ( 59.57919371712955581, 3.975000000000002753, -6.884901960086283523 ) ) ;
#59665 = EDGE_LOOP ( 'NONE', ( #88413, #33998, #88805, #130629 ) ) ;
#59666 = FACE_OUTER_BOUND ( 'NONE', #68570, .T. ) ;
#59667 = DIRECTION ( 'NONE',  ( -0.000000000000000000, 1.000000000000000000, -0.000000000000000000 ) ) ;
#59668 = FACE_BOUND ( 'NONE', #45772, .T. ) ;
#59669 = EDGE_CURVE ( 'NONE', #132816, #55582, #16597, .T. ) ;
#59670 = CARTESIAN_POINT ( 'NONE',  ( 9.524999999999991473, -4.870000000000013429, -10.00000000000000178 ) ) ;
#59671 = LINE ( 'NONE', #37916, #83799 ) ;
#59672 = CARTESIAN_POINT ( 'NONE',  ( 25.49999999999982236, -14.56887692260766087, 4.000000000000000000 ) ) ;
#59674 = ORIENTED_EDGE ( 'NONE', *, *, #70586, .T. ) ;
#59673 = LINE ( 'NONE', #50214, #112958 ) ;
#59675 = DIRECTION ( 'NONE',  ( 0.7071067811865487940, 0.7071067811865463515, 0.000000000000000000 ) ) ;
#59676 = ORIENTED_EDGE ( 'NONE', *, *, #59307, .F. ) ;
#59677 = VERTEX_POINT ( 'NONE', #61580 ) ;
#59678 = CARTESIAN_POINT ( 'NONE',  ( 67.72459685856476597, -1.637169565754160949, 6.109999999999997655 ) ) ;
#59679 = ORIENTED_EDGE ( 'NONE', *, *, #122379, .T. ) ;
#59680 = AXIS2_PLACEMENT_3D ( 'NONE', #13446, #57721, #67910 ) ;
#59681 = LINE ( 'NONE', #37190, #6970 ) ;
#59682 = CARTESIAN_POINT ( 'NONE',  ( -22.49999999999983658, 19.46639925780206326, 5.000000000000000000 ) ) ;
#59683 = ORIENTED_EDGE ( 'NONE', *, *, #29537, .T. ) ;
#59684 = FILL_AREA_STYLE ('',( #3124 ) ) ;
#59685 = VECTOR ( 'NONE', #83683, 1000.000000000000000 ) ;
#59686 = EDGE_CURVE ( 'NONE', #38538, #135052, #49974, .T. ) ;
#59687 = LINE ( 'NONE', #60408, #128870 ) ;
#59688 = CARTESIAN_POINT ( 'NONE',  ( 100.8958333333333570, -2.130196079827465283, 7.949999999999977973 ) ) ;
#59689 = CARTESIAN_POINT ( 'NONE',  ( -26.29298673570676925, -21.74070752338405299, 4.999753212805220670 ) ) ;
#59690 = CARTESIAN_POINT ( 'NONE',  ( 32.99999999999977263, 1.761378380278715738, -6.096875308897179657 ) ) ;
#59691 = DIRECTION ( 'NONE',  ( -0.6830127018922180770, -0.6830127018922204085, -0.2588190451025213501 ) ) ;
#59692 = ORIENTED_EDGE ( 'NONE', *, *, #10892, .F. ) ;
#59693 = ORIENTED_EDGE ( 'NONE', *, *, #19898, .F. ) ;
#59694 = LINE ( 'NONE', #39369, #82151 ) ;
#59696 = CARTESIAN_POINT ( 'NONE',  ( 156.1500000000000057, -49.14999999999999147, 53.92499999999997584 ) ) ;
#59695 = VECTOR ( 'NONE', #109798, 1000.000000000000000 ) ;
#59697 = ORIENTED_EDGE ( 'NONE', *, *, #40117, .T. ) ;
#59698 = ORIENTED_EDGE ( 'NONE', *, *, #131636, .F. ) ;
#59700 = VERTEX_POINT ( 'NONE', #137476 ) ;
#59699 = VECTOR ( 'NONE', #76608, 1000.000000000000000 ) ;
#59701 = LINE ( 'NONE', #16133, #4894 ) ;
#59702 = EDGE_CURVE ( 'NONE', #91750, #77043, #6901, .T. ) ;
#59703 = DIRECTION ( 'NONE',  ( 0.7071067811865487940, 0.7071067811865463515, 0.000000000000000000 ) ) ;
#59704 = ORIENTED_EDGE ( 'NONE', *, *, #111232, .F. ) ;
#59705 = CARTESIAN_POINT ( 'NONE',  ( -3.792893218813424117, -17.24070752338410628, 5.000000000000000000 ) ) ;
#59706 = AXIS2_PLACEMENT_3D ( 'NONE', #60206, #103655, #4298 ) ;
#59707 = VECTOR ( 'NONE', #21847, 1000.000000000000000 ) ;
#59709 = EDGE_CURVE ( 'NONE', #130192, #122911, #9253, .T. ) ;
#59708 = LINE ( 'NONE', #50960, #141950 ) ;
#59710 = EDGE_CURVE ( 'NONE', #40577, #138063, #91804, .T. ) ;
#59711 = CARTESIAN_POINT ( 'NONE',  ( 4.733736474768551972, 5.808823158059036373, 5.808823158059032821 ) ) ;
#59712 = DIRECTION ( 'NONE',  ( 0.7071067811865487940, 0.7071067811865463515, -0.000000000000000000 ) ) ;
#59713 = EDGE_CURVE ( 'NONE', #66625, #109461, #116430, .T. ) ;
#59714 = ORIENTED_EDGE ( 'NONE', *, *, #77343, .T. ) ;
#59715 = CARTESIAN_POINT ( 'NONE',  ( -6.656710001662093923, 3.759292476615674783, 13.27625715073264168 ) ) ;
#59716 = ADVANCED_FACE ( 'NONE', ( #6190 ), #128042, .T. ) ;
#59717 = CARTESIAN_POINT ( 'NONE',  ( 118.7875270504628986, 0.000000000000000000, -7.949999999999998401 ) ) ;
#59718 = CARTESIAN_POINT ( 'NONE',  ( -32.99999999999976552, -11.35517001088074629, -1.126524801160187161 ) ) ;
#59720 = EDGE_LOOP ( 'NONE', ( #138054, #100681, #134379, #102987 ) ) ;
#59719 = PLANE ( 'NONE',  #58805 ) ;
#59721 = CARTESIAN_POINT ( 'NONE',  ( 14.86920357848291196, 0.000000000000000000, 2.500000000000000444 ) ) ;
#59722 = ORIENTED_EDGE ( 'NONE', *, *, #121354, .F. ) ;
#59723 = EDGE_CURVE ( 'NONE', #32684, #7267, #49046, .T. ) ;
#59724 = DIRECTION ( 'NONE',  ( -0.000000000000000000, 0.000000000000000000, 1.000000000000000000 ) ) ;
#59725 = PLANE ( 'NONE',  #141942 ) ;
#59726 = CARTESIAN_POINT ( 'NONE',  ( 108.1874999999999716, -5.819803920172573974, 5.819803920172573086 ) ) ;
#59727 = ORIENTED_EDGE ( 'NONE', *, *, #52834, .T. ) ;
#59728 =( LENGTH_UNIT ( ) NAMED_UNIT ( * ) SI_UNIT ( .MILLI., .METRE. ) );
#59729 = EDGE_CURVE ( 'NONE', #31893, #78216, #136734, .T. ) ;
#59730 = DIRECTION ( 'NONE',  ( -0.3543493200069162685, -0.000000000000000000, -0.9351131265310288487 ) ) ;
#59731 = CARTESIAN_POINT ( 'NONE',  ( -25.39999999999996305, 0.000000000000000000, 2.500000000000000000 ) ) ;
#59732 = DIRECTION ( 'NONE',  ( -0.7071067811865486830, -0.7071067811865464625, 0.000000000000000000 ) ) ;
#59733 = VERTEX_POINT ( 'NONE', #117122 ) ;
#59734 = CARTESIAN_POINT ( 'NONE',  ( 36.18398860626899705, 28.73617430169812437, 5.000000000000000000 ) ) ;
#59735 = DIRECTION ( 'NONE',  ( 0.3543493200069163240, -0.000000000000000000, -0.9351131265310288487 ) ) ;
#59736 = CARTESIAN_POINT ( 'NONE',  ( 7.774972949537104938, 4.461849672132300881, 4.461849672132299105 ) ) ;
#59737 = EDGE_CURVE ( 'NONE', #25222, #51133, #138185, .T. ) ;
#59738 = LINE ( 'NONE', #60460, #44943 ) ;
#59739 = LINE ( 'NONE', #16171, #20590 ) ;
#59740 = ORIENTED_EDGE ( 'NONE', *, *, #46059, .T. ) ;
#59741 = ORIENTED_EDGE ( 'NONE', *, *, #35081, .F. ) ;
#59742 = CIRCLE ( 'NONE', #126852, 5.999999999999998224 ) ;
#59743 = CARTESIAN_POINT ( 'NONE',  ( -42.48921356237308800, -27.52281430457085065, 5.000000000000000000 ) ) ;
#59744 = FILL_AREA_STYLE_COLOUR ( '', #108389 ) ;
#59745 = ADVANCED_FACE ( 'NONE', ( #14951 ), #104828, .F. ) ;
#59746 = CARTESIAN_POINT ( 'NONE',  ( 9.312069808101886892, 7.934999999999993392, 2.126176841940951689 ) ) ;
#59747 = LINE ( 'NONE', #103907, #99101 ) ;
#59748 = CARTESIAN_POINT ( 'NONE',  ( 25.82816939922335209, -20.24070752338407431, 4.000000000000000000 ) ) ;
#59749 = CARTESIAN_POINT ( 'NONE',  ( 184.1499999999998067, -49.85820393249939286, 34.92500000000001847 ) ) ;
#59750 = DIRECTION ( 'NONE',  ( -0.7071067811865486830, 0.7071067811865464625, 0.000000000000000000 ) ) ;
#59751 = ORIENTED_EDGE ( 'NONE', *, *, #1664, .F. ) ;
#59752 = DIRECTION ( 'NONE',  ( -0.7071067811865486830, 0.7071067811865464625, 0.000000000000000000 ) ) ;
#59753 = CARTESIAN_POINT ( 'NONE',  ( 0.1839886062690032631, 28.73617430169787568, 5.000000000000000000 ) ) ;
#59754 = CARTESIAN_POINT ( 'NONE',  ( 8.585466709768445170, 0.000000000000000000, 2.500000000000000444 ) ) ;
#59755 = CARTESIAN_POINT ( 'NONE',  ( 45.55793019189811588, 6.110000000000001208, -1.637169565754156286 ) ) ;
#59756 =( BOUNDED_CURVE ( )  B_SPLINE_CURVE ( 3, ( #118946, #87757, #87045, #55868 ),
 .UNSPECIFIED., .F., .F. ) 
 B_SPLINE_CURVE_WITH_KNOTS ( ( 4, 4 ),
 ( 0.6873533248919960759, 0.6988790395524697718 ),
 .UNSPECIFIED. ) 
 CURVE ( )  GEOMETRIC_REPRESENTATION_ITEM ( )  RATIONAL_B_SPLINE_CURVE ( ( 1.000000000000000000, 0.9999889298557675943, 0.9999889298557675943, 1.000000000000000000 ) ) 
 REPRESENTATION_ITEM ( '' )  );
#59757 = DIRECTION ( 'NONE',  ( 0.6830127018922180770, -0.6830127018922204085, -0.2588190451025213501 ) ) ;
#59758 = ORIENTED_EDGE ( 'NONE', *, *, #44240, .T. ) ;
#59759 = CARTESIAN_POINT ( 'NONE',  ( -34.75611968250421313, 5.812934254707314174, 4.955485411084895375 ) ) ;
#59760 = VERTEX_POINT ( 'NONE', #125153 ) ;
#59761 = LINE ( 'NONE', #59074, #122407 ) ;
#59762 = EDGE_CURVE ( 'NONE', #77708, #139000, #62070, .T. ) ;
#59763 = VERTEX_POINT ( 'NONE', #48310 ) ;
#59764 = DIRECTION ( 'NONE',  ( 1.000000000000000000, 0.000000000000000000, 0.000000000000000000 ) ) ;
#59765 = DIRECTION ( 'NONE',  ( -0.000000000000000000, 0.000000000000000000, 1.000000000000000000 ) ) ;
#59766 = CARTESIAN_POINT ( 'NONE',  ( -34.92500000000001137, 12.85612307739231497, 4.000000000000000000 ) ) ;
#59767 = CARTESIAN_POINT ( 'NONE',  ( -25.49999999999982236, -12.08601207473290451, -10.46905243149087994 ) ) ;
#59768 = FACE_OUTER_BOUND ( 'NONE', #137908, .T. ) ;
#59769 = CARTESIAN_POINT ( 'NONE',  ( -36.48921356237310221, -27.52281430457080802, 5.000000000000000000 ) ) ;
#59770 = ORIENTED_EDGE ( 'NONE', *, *, #56358, .F. ) ;
#59771 = CARTESIAN_POINT ( 'NONE',  ( 20.65000000000000213, 0.000000000000000000, 0.000000000000000000 ) ) ;
#59772 = DIRECTION ( 'NONE',  ( -0.7071067811865486830, 0.7071067811865464625, 0.000000000000000000 ) ) ;
#59773 = DIRECTION ( 'NONE',  ( 0.000000000000000000, 1.000000000000000000, 0.000000000000000000 ) ) ;
#59774 = EDGE_CURVE ( 'NONE', #7223, #120796, #2311, .T. ) ;
#59775 = LINE ( 'NONE', #123621, #38772 ) ;
#59776 = CARTESIAN_POINT ( 'NONE',  ( 68.18336038379622721, -2.130196079827426203, 7.949999999999997513 ) ) ;
#59777 = CARTESIAN_POINT ( 'NONE',  ( 0.000000000000000000, 0.000000000000000000, 0.000000000000000000 ) ) ;
#59778 = VERTEX_POINT ( 'NONE', #114952 ) ;
#59779 = ORIENTED_EDGE ( 'NONE', *, *, #38097, .T. ) ;
#59780 = VECTOR ( 'NONE', #11666, 1000.000000000000227 ) ;
#59781 = CARTESIAN_POINT ( 'NONE',  ( 67.06249999999997158, -5.819803920172572198, -5.819803920172573086 ) ) ;
#59782 = FACE_OUTER_BOUND ( 'NONE', #36733, .T. ) ;
#59783 = EDGE_CURVE ( 'NONE', #24699, #135809, #6954, .T. ) ;
#59784 = DIRECTION ( 'NONE',  ( 1.000000000000000000, 0.000000000000000000, 0.000000000000000000 ) ) ;
#59785 = CARTESIAN_POINT ( 'NONE',  ( 12.00548008471251293, 28.92564299267929684, 4.000000000000000000 ) ) ;
#59786 = ORIENTED_EDGE ( 'NONE', *, *, #69458, .T. ) ;
#59787 = DIRECTION ( 'NONE',  ( 0.3543493200069163240, 0.000000000000000000, 0.9351131265310288487 ) ) ;
#59788 = EDGE_CURVE ( 'NONE', #140843, #43910, #30867, .T. ) ;
#59789 = LINE ( 'NONE', #17666, #120779 ) ;
#59790 = CARTESIAN_POINT ( 'NONE',  ( 56.00043019189809712, -3.055000000000002380, 5.291415217122920289 ) ) ;
#59791 = FACE_OUTER_BOUND ( 'NONE', #2887, .T. ) ;
#59792 = ORIENTED_EDGE ( 'NONE', *, *, #14861, .T. ) ;
#59793 = ORIENTED_EDGE ( 'NONE', *, *, #23196, .T. ) ;
#59794 =( LENGTH_UNIT ( ) NAMED_UNIT ( * ) SI_UNIT ( .MILLI., .METRE. ) );
#59795 = AXIS2_PLACEMENT_3D ( 'NONE', #51337, #40472, #6335 ) ;
#59796 = DIRECTION ( 'NONE',  ( 0.7071067811865487940, 0.7071067811865463515, 0.000000000000000000 ) ) ;
#59797 = CARTESIAN_POINT ( 'NONE',  ( -28.49999999999980460, -14.70932175296479549, -11.46312253303830353 ) ) ;
#59798 = AXIS2_PLACEMENT_3D ( 'NONE', #140932, #41626, #87288 ) ;
#59799 = DIRECTION ( 'NONE',  ( 0.7071067811865487940, -0.7071067811865463515, -0.000000000000000000 ) ) ;
#59800 = EDGE_CURVE ( 'NONE', #14639, #83008, #18505, .T. ) ;
#59801 = DIRECTION ( 'NONE',  ( -0.6830127018922180770, -0.6830127018922204085, -0.2588190451025213501 ) ) ;
#59803 = EDGE_LOOP ( 'NONE', ( #33088, #100254, #34384, #90280 ) ) ;
#59802 = DIRECTION ( 'NONE',  ( 0.000000000000000000, 0.000000000000000000, 1.000000000000000000 ) ) ;
#59804 = DIRECTION ( 'NONE',  ( -0.7071067811865486830, 0.7071067811865464625, 0.000000000000000000 ) ) ;
#59805 = CARTESIAN_POINT ( 'NONE',  ( -30.00000000000000355, -2.375000000000000000, -4.320000000000002061 ) ) ;
#59806 = VECTOR ( 'NONE', #18620, 1000.000000000000227 ) ;
#59807 = CARTESIAN_POINT ( 'NONE',  ( 1.499999999999994449, 10.94296225409026668, -9.576120664313254593 ) ) ;
#59808 = VECTOR ( 'NONE', #48604, 1000.000000000000000 ) ;
#59809 = ORIENTED_EDGE ( 'NONE', *, *, #111933, .F. ) ;
#59810 = ORIENTED_EDGE ( 'NONE', *, *, #110697, .T. ) ;
#59811 = CARTESIAN_POINT ( 'NONE',  ( 61.46640106136302961, -49.14999999999999147, -40.92499999999998295 ) ) ;
#59812 = DIRECTION ( 'NONE',  ( 0.3543493200069162685, -0.000000000000000000, -0.9351131265310288487 ) ) ;
#59813 = CARTESIAN_POINT ( 'NONE',  ( 17.84878961325748037, 4.584330080086930965E-16, 0.000000000000000000 ) ) ;
#59814 = LINE ( 'NONE', #17010, #136063 ) ;
#59815 = CARTESIAN_POINT ( 'NONE',  ( -34.92500000000001137, 14.71849043720408190, 4.759050581649336920 ) ) ;
#59816 = VERTEX_POINT ( 'NONE', #74366 ) ;
#59817 = EDGE_LOOP ( 'NONE', ( #134197, #6642, #19596, #138617 ) ) ;
#59818 = CARTESIAN_POINT ( 'NONE',  ( 0.000000000000000000, 0.000000000000000000, 5.000000000000000000 ) ) ;
#59819 = CARTESIAN_POINT ( 'NONE',  ( -57.18398860626899705, 28.73617430169827358, 5.000000000000000000 ) ) ;
#59820 = EDGE_CURVE ( 'NONE', #55488, #96120, #96082, .T. ) ;
#59821 = VERTEX_POINT ( 'NONE', #31568 ) ;
#59822 = EDGE_CURVE ( 'NONE', #50417, #41659, #19953, .T. ) ;
#59823 = CARTESIAN_POINT ( 'NONE',  ( 29.99451991528749417, 28.92564299267958816, 4.000000000000000000 ) ) ;
#59824 = VERTEX_POINT ( 'NONE', #73640 ) ;
#59825 = PLANE ( 'NONE',  #91962 ) ;
#59826 = DIRECTION ( 'NONE',  ( 0.000000000000000000, -1.000000000000000000, 0.000000000000000000 ) ) ;
#59827 = VECTOR ( 'NONE', #49960, 1000.000000000000000 ) ;
#59828 = VECTOR ( 'NONE', #5316, 999.9999999999998863 ) ;
#59829 = AXIS2_PLACEMENT_3D ( 'NONE', #139220, #109417, #40610 ) ;
#59830 = FACE_BOUND ( 'NONE', #16424, .T. ) ;
#59831 = ADVANCED_FACE ( 'NONE', ( #41007 ), #62780, .T. ) ;
#59832 = FACE_OUTER_BOUND ( 'NONE', #64495, .T. ) ;
#59833 = PLANE ( 'NONE',  #23532 ) ;
#59834 = DIRECTION ( 'NONE',  ( -0.3543493200069162685, -0.000000000000000000, -0.9351131265310288487 ) ) ;
#59835 = DIRECTION ( 'NONE',  ( 0.7071067811865487940, 0.7071067811865463515, 0.000000000000000000 ) ) ;
#59836 = CARTESIAN_POINT ( 'NONE',  ( -9.707106781186469746, 20.25929247661551713, 5.000000000000000000 ) ) ;
#59837 = APPLICATION_PROTOCOL_DEFINITION ( 'draft international standard', 'automotive_design', 1998, #53097 ) ;
#59838 = ORIENTED_EDGE ( 'NONE', *, *, #36333, .T. ) ;
#59839 = ORIENTED_EDGE ( 'NONE', *, *, #5532, .F. ) ;
#59840 = CARTESIAN_POINT ( 'NONE',  ( 95.87043019189810877, -3.055000000000001492, 5.291415217122917625 ) ) ;
#59841 = ORIENTED_EDGE ( 'NONE', *, *, #81638, .F. ) ;
#59842 = DIRECTION ( 'NONE',  ( 0.000000000000000000, 1.000000000000000000, 0.000000000000000000 ) ) ;
#59843 = DIRECTION ( 'NONE',  ( -0.6830127018922181881, 0.6830127018922202975, -0.2588190451025214056 ) ) ;
#59844 = AXIS2_PLACEMENT_3D ( 'NONE', #117405, #31162, #16685 ) ;
#59845 = VECTOR ( 'NONE', #16359, 999.9999999999998863 ) ;
#59846 = CARTESIAN_POINT ( 'NONE',  ( 0.000000000000000000, 8.616843969807042924, 0.000000000000000000 ) ) ;
#59847 = ORIENTED_EDGE ( 'NONE', *, *, #78528, .T. ) ;
#59848 = DIRECTION ( 'NONE',  ( -0.3543493200069162685, -0.000000000000000000, -0.9351131265310288487 ) ) ;
#59849 = CARTESIAN_POINT ( 'NONE',  ( 8.207106781186489286, 12.75929247661558996, 5.000000000000000000 ) ) ;
#59850 = LINE ( 'NONE', #27194, #75903 ) ;
#59852 = LINE ( 'NONE', #116361, #72904 ) ;
#59851 = CARTESIAN_POINT ( 'NONE',  ( 68.08333333333332860, 6.884901960086290629, -3.974999999999994316 ) ) ;
#59853 = FACE_OUTER_BOUND ( 'NONE', #47816, .T. ) ;
#59854 = CARTESIAN_POINT ( 'NONE',  ( 17.99999999999988276, -13.44781430457068794, 5.000000000000000000 ) ) ;
#59855 = VERTEX_POINT ( 'NONE', #76515 ) ;
#59856 = CARTESIAN_POINT ( 'NONE',  ( -63.18398860626900415, 28.73617430169831621, 5.000000000000000000 ) ) ;
#59857 = PLANE ( 'NONE',  #102087 ) ;
#59858 = VERTEX_POINT ( 'NONE', #51180 ) ;
#59859 = ORIENTED_EDGE ( 'NONE', *, *, #91218, .F. ) ;
#59860 = ORIENTED_EDGE ( 'NONE', *, *, #92806, .T. ) ;
#59861 = CARTESIAN_POINT ( 'NONE',  ( 48.27126352523143993, 4.472830434245838482, 4.472830434245842035 ) ) ;
#59862 = ORIENTED_EDGE ( 'NONE', *, *, #110427, .T. ) ;
#59863 = EDGE_CURVE ( 'NONE', #98856, #9144, #75791, .T. ) ;
#59864 = CARTESIAN_POINT ( 'NONE',  ( 13.75413961620377457, 3.047499999999993214, -5.278424836066146320 ) ) ;
#59865 = CARTESIAN_POINT ( 'NONE',  ( -15.78892356518500328, 2.636128110293266769, -32.92760517736494563 ) ) ;
#59866 = ORIENTED_EDGE ( 'NONE', *, *, #73135, .T. ) ;
#59867 = EDGE_CURVE ( 'NONE', #101632, #15581, #139645, .T. ) ;
#59868 = LINE ( 'NONE', #59187, #1628 ) ;
#59870 = EDGE_LOOP ( 'NONE', ( #104385, #92405, #123854, #99229 ) ) ;
#59869 = ADVANCED_FACE ( 'NONE', ( #52587, #20665 ), #40325, .F. ) ;
#59871 = CARTESIAN_POINT ( 'NONE',  ( -2.200031220168353840, 8.259292476615634371, 16.85664084051841627 ) ) ;
#59872 = CARTESIAN_POINT ( 'NONE',  ( -1.499999999999987566, -4.533600742197694267, 5.000000000000000000 ) ) ;
#59874 = ORIENTED_EDGE ( 'NONE', *, *, #137724, .F. ) ;
#59873 = CYLINDRICAL_SURFACE ( 'NONE', #128107, 0.5000000000000005551 ) ;
#59875 = ORIENTED_EDGE ( 'NONE', *, *, #27567, .F. ) ;
#59876 = EDGE_CURVE ( 'NONE', #28133, #34213, #86670, .T. ) ;
#59877 = CARTESIAN_POINT ( 'NONE',  ( 13.96000000000000085, 9.521314400968980422E-16, 0.000000000000000000 ) ) ;
#59878 = DIRECTION ( 'NONE',  ( -0.3543493200069162685, -0.000000000000000000, -0.9351131265310288487 ) ) ;
#59879 = ORIENTED_EDGE ( 'NONE', *, *, #17301, .F. ) ;
#59880 = LINE ( 'NONE', #38136, #64334 ) ;
#59881 = VERTEX_POINT ( 'NONE', #32283 ) ;
#59882 = VECTOR ( 'NONE', #93596, 1000.000000000000000 ) ;
#59883 = EDGE_LOOP ( 'NONE', ( #110060, #52395, #59958, #62127, #133541 ) ) ;
#59884 = VERTEX_POINT ( 'NONE', #117816 ) ;
#59885 = ORIENTED_EDGE ( 'NONE', *, *, #102476, .F. ) ;
#59886 = CARTESIAN_POINT ( 'NONE',  ( 30.48921356237309510, -27.52281430457076894, 5.000000000000000000 ) ) ;
#59887 = AXIS2_PLACEMENT_3D ( 'NONE', #41823, #65763, #86043 ) ;
#59888 = AXIS2_PLACEMENT_3D ( 'NONE', #23689, #90369, #36697 ) ;
#59889 = VECTOR ( 'NONE', #41438, 1000.000000000000000 ) ;
#59890 = DIRECTION ( 'NONE',  ( 0.7071067811865486830, 0.7071067811865464625, 0.000000000000000000 ) ) ;
#59891 = AXIS2_PLACEMENT_3D ( 'NONE', #125804, #124361, #25030 ) ;
#59892 = EDGE_CURVE ( 'NONE', #98193, #105689, #30118, .T. ) ;
#59893 = LINE ( 'NONE', #58512, #88793 ) ;
#59894 = CARTESIAN_POINT ( 'NONE',  ( -29.20710678118633652, 18.75929247661552779, 5.000000000000000000 ) ) ;
#59895 = EDGE_CURVE ( 'NONE', #62344, #8091, #9793, .T. ) ;
#59896 = AXIS2_PLACEMENT_3D ( 'NONE', #56379, #23699, #10653 ) ;
#59897 = LINE ( 'NONE', #67954, #136824 ) ;
#59898 = ORIENTED_EDGE ( 'NONE', *, *, #138396, .F. ) ;
#59899 = AXIS2_PLACEMENT_3D ( 'NONE', #82003, #5790, #128337 ) ;
#59900 = VECTOR ( 'NONE', #116245, 1000.000000000000227 ) ;
#59901 = DIRECTION ( 'NONE',  ( 0.000000000000000000, 0.000000000000000000, 1.000000000000000000 ) ) ;
#59902 = EDGE_CURVE ( 'NONE', #101225, #19552, #141017, .T. ) ;
#59903 = CARTESIAN_POINT ( 'NONE',  ( 19.08290314143522437, 3.967499999999992699, -6.871911579029513994 ) ) ;
#59904 = CARTESIAN_POINT ( 'NONE',  ( 18.32266436734346726, 4.202752102959690472E-16, 0.000000000000000000 ) ) ;
#59905 = LINE ( 'NONE', #49759, #32145 ) ;
#59906 =( BOUNDED_CURVE ( )  B_SPLINE_CURVE ( 3, ( #136159, #80385, #78961, #126018 ),
 .UNSPECIFIED., .F., .T. ) 
 B_SPLINE_CURVE_WITH_KNOTS ( ( 4, 4 ),
 ( 4.257860004652494368, 4.307247239014357021 ),
 .UNSPECIFIED. ) 
 CURVE ( )  GEOMETRIC_REPRESENTATION_ITEM ( )  RATIONAL_B_SPLINE_CURVE ( ( 1.000000000000000000, 0.9997967520851089862, 0.9997967520851089862, 1.000000000000000000 ) ) 
 REPRESENTATION_ITEM ( '' )  );
#59907 = FACE_OUTER_BOUND ( 'NONE', #71881, .T. ) ;
#59908 = ORIENTED_EDGE ( 'NONE', *, *, #4569, .T. ) ;
#59909 = ORIENTED_EDGE ( 'NONE', *, *, #108251, .T. ) ;
#59910 = VERTEX_POINT ( 'NONE', #65667 ) ;
#59911 = CARTESIAN_POINT ( 'NONE',  ( 14.28769006033961375, -21.73547319004781642, 4.999917730833664642 ) ) ;
#59912 = CARTESIAN_POINT ( 'NONE',  ( 34.92499999999998295, 1.821246448331339307, 12.73174495308783705 ) ) ;
#59913 = ADVANCED_FACE ( 'NONE', ( #128728 ), #51124, .T. ) ;
#59914 = PLANE ( 'NONE',  #84702 ) ;
#59915 = STYLED_ITEM ( 'NONE', ( #37257 ), #46666 ) ;
#59916 = STYLED_ITEM ( 'NONE', ( #6758 ), #36322 ) ;
#59917 = DIRECTION ( 'NONE',  ( -0.000000000000000000, -0.3543493200069152693, 0.9351131265310292928 ) ) ;
#59918 = FACE_OUTER_BOUND ( 'NONE', #95906, .T. ) ;
#59919 = CARTESIAN_POINT ( 'NONE',  ( 77.93293019189812298, 1.637169565754156730, 6.110000000000001208 ) ) ;
#59920 = DIRECTION ( 'NONE',  ( -0.7071067811865487940, 0.7071067811865463515, -0.000000000000000000 ) ) ;
#59921 = PLANE ( 'NONE',  #131740 ) ;
#59922 = DIRECTION ( 'NONE',  ( 0.7071067811865487940, -0.7071067811865463515, 0.000000000000000000 ) ) ;
#59923 = DIRECTION ( 'NONE',  ( -0.7071067811865487940, 0.7071067811865463515, 0.000000000000000000 ) ) ;
#59924 = CARTESIAN_POINT ( 'NONE',  ( 48.29974487139158867, -27.71228299555239971, 4.000000000000000000 ) ) ;
#59925 = EDGE_CURVE ( 'NONE', #128596, #5408, #130173, .T. ) ;
#59926 = ORIENTED_EDGE ( 'NONE', *, *, #131646, .T. ) ;
#59927 = VECTOR ( 'NONE', #129088, 1000.000000000000000 ) ;
#59928 = CARTESIAN_POINT ( 'NONE',  ( -34.42500000000001137, 22.22500000000000142, 4.165035510187088619 ) ) ;
#59929 = EDGE_LOOP ( 'NONE', ( #520, #126514, #102062, #65351 ) ) ;
#59930 = VECTOR ( 'NONE', #121274, 1000.000000000000000 ) ;
#59931 = VECTOR ( 'NONE', #108367, 1000.000000000000000 ) ;
#59932 = AXIS2_PLACEMENT_3D ( 'NONE', #52058, #140475, #130341 ) ;
#59933 = CARTESIAN_POINT ( 'NONE',  ( 0.2782545156857219038, 8.259292476615637923, 11.78515199841150363 ) ) ;
#59935 = EDGE_LOOP ( 'NONE', ( #27971, #41840, #78943, #76677 ) ) ;
#59934 = CARTESIAN_POINT ( 'NONE',  ( 8.423184310185783730, 4.584330080086930965E-16, 0.000000000000000000 ) ) ;
#59936 = CARTESIAN_POINT ( 'NONE',  ( 26.47599861414532185, 22.03583458319438293, 4.979811245910084949 ) ) ;
#59937 = CARTESIAN_POINT ( 'NONE',  ( 4.911592354503321545, -2.500000000000000000, 3.061616997868384127E-16 ) ) ;
#59938 = VERTEX_POINT ( 'NONE', #119262 ) ;
#59939 = DIRECTION ( 'NONE',  ( 0.6830127018922181881, 0.6830127018922202975, -0.2588190451025214056 ) ) ;
#59940 = VERTEX_POINT ( 'NONE', #51902 ) ;
#59941 = DIRECTION ( 'NONE',  ( -0.000000000000000000, -1.000000000000000000, -0.000000000000000000 ) ) ;
#59942 = VERTEX_POINT ( 'NONE', #64197 ) ;
#59943 = VECTOR ( 'NONE', #33397, 1000.000000000000000 ) ;
#59944 = CONICAL_SURFACE ( 'NONE', #73789, 2.055000000000001048, 0.9599310885968758145 ) ;
#59945 = DIRECTION ( 'NONE',  ( 0.6830127018922181881, 0.6830127018922202975, -0.2588190451025214056 ) ) ;
#59946 = ADVANCED_FACE ( 'NONE', ( #108356 ), #9032, .F. ) ;
#59947 = CARTESIAN_POINT ( 'NONE',  ( 103.4750270504628702, -5.819803920172572198, 5.819803920172572198 ) ) ;
#59948 = LINE ( 'NONE', #102728, #111076 ) ;
#59949 = FACE_OUTER_BOUND ( 'NONE', #119880, .T. ) ;
#59950 = ORIENTED_EDGE ( 'NONE', *, *, #14392, .T. ) ;
#59951 = DIRECTION ( 'NONE',  ( 0.000000000000000000, -1.000000000000000000, 0.000000000000000000 ) ) ;
#59952 = ADVANCED_FACE ( 'NONE', ( #123600 ), #46029, .F. ) ;
#59953 = CARTESIAN_POINT ( 'NONE',  ( -66.18398860626901126, 28.73617430169833753, 5.000000000000000000 ) ) ;
#59954 = CARTESIAN_POINT ( 'NONE',  ( 23.33333333333333570, 5.278424836066143655, -3.047499999999997655 ) ) ;
#59955 = AXIS2_PLACEMENT_3D ( 'NONE', #119240, #8315, #52565 ) ;
#59956 = ORIENTED_EDGE ( 'NONE', *, *, #77670, .F. ) ;
#59957 = CARTESIAN_POINT ( 'NONE',  ( 11.56505274454301357, -2.500000000000000000, 3.061616997868383634E-16 ) ) ;
#59958 = ORIENTED_EDGE ( 'NONE', *, *, #74694, .T. ) ;
#59959 = EDGE_CURVE ( 'NONE', #97151, #79079, #34414, .T. ) ;
#59960 = CARTESIAN_POINT ( 'NONE',  ( 80.50043019189810423, -3.055000000000002380, 5.291415217122920289 ) ) ;
#59961 = DIRECTION ( 'NONE',  ( -0.7071067811865486830, -0.7071067811865464625, 0.000000000000000000 ) ) ;
#59962 = CARTESIAN_POINT ( 'NONE',  ( -27.79289321881325847, -5.240707523384227073, 5.000000000000000000 ) ) ;
#59963 = CARTESIAN_POINT ( 'NONE',  ( 26.99999999999980815, -9.412538124160658271, 4.000000000000000000 ) ) ;
#59964 = ORIENTED_EDGE ( 'NONE', *, *, #11265, .T. ) ;
#59965 = LINE ( 'NONE', #128085, #127609 ) ;
#59966 = CARTESIAN_POINT ( 'NONE',  ( 1.500000000000000000, 0.000000000000000000, 0.000000000000000000 ) ) ;
#59967 = DIRECTION ( 'NONE',  ( -0.6830127018922180770, -0.6830127018922204085, -0.2588190451025213501 ) ) ;
#59968 = EDGE_CURVE ( 'NONE', #111985, #94939, #89504, .T. ) ;
#59969 = CARTESIAN_POINT ( 'NONE',  ( -24.18398860626899705, 28.73617430169804265, 5.000000000000000000 ) ) ;
#59970 = ORIENTED_EDGE ( 'NONE', *, *, #132773, .F. ) ;
#59971 = LINE ( 'NONE', #51951, #48640 ) ;
#59972 = FACE_OUTER_BOUND ( 'NONE', #65194, .T. ) ;
#59973 = PRESENTATION_STYLE_ASSIGNMENT (( #104885 ) ) ;
#59974 = DIRECTION ( 'NONE',  ( 0.000000000000000000, 0.000000000000000000, 1.000000000000000000 ) ) ;
#59975 = ORIENTED_EDGE ( 'NONE', *, *, #38366, .T. ) ;
#59976 = EDGE_LOOP ( 'NONE', ( #55835, #51821, #121152, #129110 ) ) ;
#59977 = ORIENTED_EDGE ( 'NONE', *, *, #128762, .T. ) ;
#59978 = CARTESIAN_POINT ( 'NONE',  ( 80.35459685856474721, -1.637169565754161615, 6.110000000000000320 ) ) ;
#59979 = ORIENTED_EDGE ( 'NONE', *, *, #79749, .T. ) ;
#59980 = FILL_AREA_STYLE ('',( #105585 ) ) ;
#59981 = EDGE_CURVE ( 'NONE', #49206, #108133, #90214, .T. ) ;
#59982 = FACE_OUTER_BOUND ( 'NONE', #51278, .T. ) ;
#59983 = CARTESIAN_POINT ( 'NONE',  ( 25.49999999999982592, 15.43112307739203182, 4.000000000000000000 ) ) ;
#59984 = CARTESIAN_POINT ( 'NONE',  ( -34.92500000000001137, 22.22500000000000142, 4.000000000000000000 ) ) ;
#59985 = ORIENTED_EDGE ( 'NONE', *, *, #102795, .F. ) ;
#59986 = FACE_OUTER_BOUND ( 'NONE', #50429, .T. ) ;
#59987 = CARTESIAN_POINT ( 'NONE',  ( -26.99451991528749417, 28.92564299267956685, 4.000000000000000000 ) ) ;
#59988 = CARTESIAN_POINT ( 'NONE',  ( 79.24543019189810877, -5.291415217122918513, -3.055000000000000160 ) ) ;
#59989 = ORIENTED_EDGE ( 'NONE', *, *, #41185, .F. ) ;
#59990 = AXIS2_PLACEMENT_3D ( 'NONE', #38501, #82723, #27600 ) ;
#59991 = EDGE_CURVE ( 'NONE', #121862, #92108, #133738, .T. ) ;
#59992 = DIRECTION ( 'NONE',  ( -0.7071067811865487940, 0.7071067811865463515, 0.000000000000000000 ) ) ;
#59993 = AXIS2_PLACEMENT_3D ( 'NONE', #29830, #28435, #29133 ) ;
#59994 = CARTESIAN_POINT ( 'NONE',  ( 52.51203195997703688, -49.11957940092398900, -40.22172306649560625 ) ) ;
#59995 = FACE_OUTER_BOUND ( 'NONE', #6404, .T. ) ;
#59996 = AXIS2_PLACEMENT_3D ( 'NONE', #132445, #55570, #122957 ) ;
#59997 = VECTOR ( 'NONE', #132320, 999.9999999999998863 ) ;
#59998 = ORIENTED_EDGE ( 'NONE', *, *, #13634, .F. ) ;
#59999 = ORIENTED_EDGE ( 'NONE', *, *, #64213, .T. ) ;
#60000 = AXIS2_PLACEMENT_3D ( 'NONE', #136302, #124721, #69660 ) ;
#60001 = EDGE_CURVE ( 'NONE', #139533, #43222, #69197, .T. ) ;
#60002 = CARTESIAN_POINT ( 'NONE',  ( 65.60416666666665719, 2.130196079827422206, 7.950000000000001954 ) ) ;
#60003 = EDGE_CURVE ( 'NONE', #25969, #39717, #124277, .T. ) ;
#60004 = CARTESIAN_POINT ( 'NONE',  ( 5.999999999999959144, 13.55218569542903140, 5.000000000000000000 ) ) ;
#60005 = FACE_OUTER_BOUND ( 'NONE', #86361, .T. ) ;
#60006 = DIRECTION ( 'NONE',  ( 0.7071067811865487940, 0.7071067811865463515, 0.000000000000000000 ) ) ;
#60007 = VECTOR ( 'NONE', #64013, 1000.000000000000000 ) ;
#60008 = CARTESIAN_POINT ( 'NONE',  ( -8.700255128608413102, -27.71228299555199825, 4.000000000000000000 ) ) ;
#60009 = DIRECTION ( 'NONE',  ( -0.6830127018922181881, 0.6830127018922202975, -0.2588190451025214056 ) ) ;
#60010 = PLANE ( 'NONE',  #92814 ) ;
#60011 = SURFACE_STYLE_FILL_AREA ( #18595 ) ;
#60012 = VERTEX_POINT ( 'NONE', #2466 ) ;
#60013 = ORIENTED_EDGE ( 'NONE', *, *, #99509, .T. ) ;
#60014 = ORIENTED_EDGE ( 'NONE', *, *, #94034, .F. ) ;
#60015 = VECTOR ( 'NONE', #132911, 1000.000000000000000 ) ;
#60016 = EDGE_CURVE ( 'NONE', #22653, #103007, #33026, .T. ) ;
#60017 = CARTESIAN_POINT ( 'NONE',  ( -51.29974487139158867, -27.71228299555242103, 4.000000000000000000 ) ) ;
#60018 = AXIS2_PLACEMENT_3D ( 'NONE', #69794, #4417, #72665 ) ;
#60019 = LINE ( 'NONE', #26659, #135379 ) ;
#60020 = EDGE_LOOP ( 'NONE', ( #24655, #143554, #16026, #128775 ) ) ;
#60021 = LINE ( 'NONE', #4854, #57525 ) ;
#60022 = DIRECTION ( 'NONE',  ( -0.3543493200069162685, -0.000000000000000000, -0.9351131265310288487 ) ) ;
#60023 = LINE ( 'NONE', #117212, #45712 ) ;
#60024 = CARTESIAN_POINT ( 'NONE',  ( -15.18398860626900237, 28.73617430169797871, 5.000000000000000000 ) ) ;
#60025 = AXIS2_PLACEMENT_3D ( 'NONE', #141820, #32335, #75842 ) ;
#60026 = CARTESIAN_POINT ( 'NONE',  ( 44.99451991528749772, 28.92564299267969474, 4.000000000000000000 ) ) ;
#60027 = ORIENTED_EDGE ( 'NONE', *, *, #83584, .T. ) ;
#60028 = VECTOR ( 'NONE', #24263, 1000.000000000000000 ) ;
#60029 = CARTESIAN_POINT ( 'NONE',  ( 6.489213562373093325, -27.52281430457059841, 5.000000000000000000 ) ) ;
#60030 = LINE ( 'NONE', #125275, #51083 ) ;
#60031 = AXIS2_PLACEMENT_3D ( 'NONE', #79765, #68174, #37655 ) ;
#60032 = ORIENTED_EDGE ( 'NONE', *, *, #66937, .T. ) ;
#60033 = CARTESIAN_POINT ( 'NONE',  ( 34.92499999999998295, -21.72500000000000142, 0.4999999999999995559 ) ) ;
#60034 = ORIENTED_EDGE ( 'NONE', *, *, #24807, .F. ) ;
#60035 = ORIENTED_EDGE ( 'NONE', *, *, #85773, .T. ) ;
#60036 = CARTESIAN_POINT ( 'NONE',  ( -1.499999999999987566, 10.94296225409026668, -9.576120664313261699 ) ) ;
#60037 = ORIENTED_EDGE ( 'NONE', *, *, #71256, .F. ) ;
#60038 = ORIENTED_EDGE ( 'NONE', *, *, #16365, .T. ) ;
#60039 = EDGE_CURVE ( 'NONE', #143112, #81113, #133045, .T. ) ;
#60041 = VECTOR ( 'NONE', #78131, 1000.000000000000000 ) ;
#60040 = CARTESIAN_POINT ( 'NONE',  ( 73.79209685856477563, -5.291415217122921177, 3.054999999999999272 ) ) ;
#60042 = ORIENTED_EDGE ( 'NONE', *, *, #45952, .T. ) ;
#60043 = AXIS2_PLACEMENT_3D ( 'NONE', #71466, #83797, #28689 ) ;
#60044 = CARTESIAN_POINT ( 'NONE',  ( 15.48921356237309510, -27.52281430457066236, 5.000000000000000000 ) ) ;
#60045 = EDGE_CURVE ( 'NONE', #121396, #72622, #135189, .T. ) ;
#60046 = CARTESIAN_POINT ( 'NONE',  ( 33.32816939922329169, -3.740707523384255495, 4.000000000000000000 ) ) ;
#60047 = CARTESIAN_POINT ( 'NONE',  ( 109.5212635252314470, -4.472830434245838482, -4.472830434245840259 ) ) ;
#60048 = DIRECTION ( 'NONE',  ( -0.6830127018922181881, 0.6830127018922202975, -0.2588190451025214056 ) ) ;
#60049 = ADVANCED_FACE ( 'NONE', ( #10499 ), #77934, .F. ) ;
#60050 = CARTESIAN_POINT ( 'NONE',  ( 10.77958563595370833, 4.584330080086930965E-16, 0.000000000000000000 ) ) ;
#60051 = FACE_OUTER_BOUND ( 'NONE', #85976, .T. ) ;
#60052 = LINE ( 'NONE', #15081, #106504 ) ;
#60053 = VECTOR ( 'NONE', #2263, 1000.000000000000000 ) ;
#60054 = CARTESIAN_POINT ( 'NONE',  ( -18.48921356237309510, -27.52281430457068367, 5.000000000000000000 ) ) ;
#60055 = EDGE_CURVE ( 'NONE', #12218, #70973, #11187, .T. ) ;
#60056 = EDGE_CURVE ( 'NONE', #32830, #33782, #78639, .T. ) ;
#60057 = DIRECTION ( 'NONE',  ( -0.7071067811865487940, 0.7071067811865463515, -0.000000000000000000 ) ) ;
#60058 = CARTESIAN_POINT ( 'NONE',  ( 2.306730066903996068, -3.740707523384241728, 12.88036043432867039 ) ) ;
#60059 = ORIENTED_EDGE ( 'NONE', *, *, #42293, .F. ) ;
#60060 = FACE_OUTER_BOUND ( 'NONE', #5795, .T. ) ;
#60061 = EDGE_LOOP ( 'NONE', ( #37404, #70433, #77685, #48836 ) ) ;
#60062 = EDGE_LOOP ( 'NONE', ( #26621, #5626, #15810, #89293 ) ) ;
#60063 = LINE ( 'NONE', #59363, #137429 ) ;
#60064 = ORIENTED_EDGE ( 'NONE', *, *, #91449, .T. ) ;
#60065 = LINE ( 'NONE', #14403, #102351 ) ;
#60066 = CARTESIAN_POINT ( 'NONE',  ( 113.8750000000000000, 7.950000000000000178, 1.460391307983218535E-15 ) ) ;
#60067 = ADVANCED_FACE ( 'NONE', ( #111993 ), #88089, .T. ) ;
#60068 = CARTESIAN_POINT ( 'NONE',  ( 13.96659967656969314, 6.759292476615649470, 12.28218704918525361 ) ) ;
#60069 = ADVANCED_FACE ( 'NONE', ( #77242 ), #12646, .F. ) ;
#60070 = CARTESIAN_POINT ( 'NONE',  ( 18.79289321881332597, 15.75929247661555976, 5.000000000000000000 ) ) ;
#60071 = VERTEX_POINT ( 'NONE', #55467 ) ;
#60072 = DIRECTION ( 'NONE',  ( 0.7071067811865486830, -0.7071067811865464625, -0.000000000000000000 ) ) ;
#60073 = ORIENTED_EDGE ( 'NONE', *, *, #6083, .T. ) ;
#60074 = CARTESIAN_POINT ( 'NONE',  ( -23.67183060077630330, 20.25929247661551003, 4.000000000000000000 ) ) ;
#60075 = ADVANCED_FACE ( 'NONE', ( #33727 ), #67053, .F. ) ;
#60076 = CARTESIAN_POINT ( 'NONE',  ( 29.52540314143522338, 2.126176841940962348, 7.934999999999989839 ) ) ;
#60077 = CARTESIAN_POINT ( 'NONE',  ( -25.49999999999981526, 6.052185695429106893, 5.000000000000000000 ) ) ;
#60078 = DIRECTION ( 'NONE',  ( -0.000000000000000000, 0.3543493200069153248, 0.9351131265310292928 ) ) ;
#60079 = CARTESIAN_POINT ( 'NONE',  ( 12.99696575335027049, -8.842958852558309601, -3.475790897895063125 ) ) ;
#60080 = ORIENTED_EDGE ( 'NONE', *, *, #130415, .T. ) ;
#60081 = ORIENTED_EDGE ( 'NONE', *, *, #17324, .F. ) ;
#60082 = ORIENTED_EDGE ( 'NONE', *, *, #104923, .F. ) ;
#60083 = CARTESIAN_POINT ( 'NONE',  ( 0.000000000000000000, 0.000000000000000000, 5.000000000000000000 ) ) ;
#60084 = FACE_OUTER_BOUND ( 'NONE', #132853, .T. ) ;
#60085 = ADVANCED_FACE ( 'NONE', ( #1735 ), #93078, .F. ) ;
#60086 = LINE ( 'NONE', #57250, #24214 ) ;
#60087 = PLANE ( 'NONE',  #84343 ) ;
#60088 = DIRECTION ( 'NONE',  ( 0.7071067811865487940, -0.7071067811865463515, 0.000000000000000000 ) ) ;
#60089 = LINE ( 'NONE', #136917, #140627 ) ;
#60090 = CARTESIAN_POINT ( 'NONE',  ( 26.67183060077628198, 5.259292476615659240, 4.000000000000000000 ) ) ;
#60091 = DIRECTION ( 'NONE',  ( -0.7071067811865486830, -0.7071067811865464625, -0.000000000000000000 ) ) ;
#60092 = DIRECTION ( 'NONE',  ( 0.6830127018922181881, 0.6830127018922202975, -0.2588190451025214056 ) ) ;
#60093 = EDGE_LOOP ( 'NONE', ( #48653, #5891, #62298, #57860 ) ) ;
#60094 = LINE ( 'NONE', #39037, #85749 ) ;
#60095 = EDGE_CURVE ( 'NONE', #102270, #50596, #21825, .T. ) ;
#60096 = VECTOR ( 'NONE', #67794, 1000.000000000000000 ) ;
#60097 = CIRCLE ( 'NONE', #129500, 5.968999999999998529 ) ;
#60098 = LINE ( 'NONE', #104268, #56377 ) ;
#60099 = ORIENTED_EDGE ( 'NONE', *, *, #54477, .T. ) ;
#60100 = AXIS2_PLACEMENT_3D ( 'NONE', #57021, #13449, #3297 ) ;
#60101 = DIRECTION ( 'NONE',  ( 0.7071067811865487940, -0.7071067811865463515, 0.000000000000000000 ) ) ;
#60103 = VERTEX_POINT ( 'NONE', #28550 ) ;
#60102 = DIRECTION ( 'NONE',  ( -0.000000000000000000, -0.3543493200069152693, 0.9351131265310292928 ) ) ;
#60104 = ORIENTED_EDGE ( 'NONE', *, *, #16978, .F. ) ;
#60105 = LINE ( 'NONE', #51365, #132540 ) ;
#60106 = EDGE_CURVE ( 'NONE', #23830, #59558, #41803, .T. ) ;
#60107 = DIRECTION ( 'NONE',  ( -0.6830127018922180770, -0.6830127018922204085, -0.2588190451025213501 ) ) ;
#60109 = ADVANCED_FACE ( 'NONE', ( #5328 ), #127115, .F. ) ;
#60108 = DIRECTION ( 'NONE',  ( -0.6830127018922181881, 0.6830127018922202975, -0.2588190451025214056 ) ) ;
#60110 = ORIENTED_EDGE ( 'NONE', *, *, #108528, .T. ) ;
#60111 = DIRECTION ( 'NONE',  ( 0.000000000000000000, 0.000000000000000000, -1.000000000000000000 ) ) ;
#60112 = VECTOR ( 'NONE', #73827, 1000.000000000000000 ) ;
#60113 = ORIENTED_EDGE ( 'NONE', *, *, #140915, .T. ) ;
#60114 = CARTESIAN_POINT ( 'NONE',  ( 13.92145407031093818, 2.500000000000000888, 0.000000000000000000 ) ) ;
#60115 = DIRECTION ( 'NONE',  ( -0.6830127018922181881, 0.6830127018922202975, -0.2588190451025214056 ) ) ;
#60116 = ADVANCED_FACE ( 'NONE', ( #94486 ), #26404, .F. ) ;
#60117 = CARTESIAN_POINT ( 'NONE',  ( 127.3916937171295558, 2.130196079827421762, 7.950000000000001066 ) ) ;
#60118 = CARTESIAN_POINT ( 'NONE',  ( -33.32816939922329880, 2.259292476615694323, 4.000000000000000000 ) ) ;
#60119 = VECTOR ( 'NONE', #16541, 1000.000000000000000 ) ;
#60120 = LINE ( 'NONE', #62981, #78648 ) ;
#60121 = DIRECTION ( 'NONE',  ( 0.6830127018922181881, 0.6830127018922202975, -0.2588190451025214056 ) ) ;
#60122 = DIRECTION ( 'NONE',  ( 0.7071067811865487940, 0.7071067811865463515, -0.000000000000000000 ) ) ;
#60123 = CARTESIAN_POINT ( 'NONE',  ( 1.408325480989996326, -0.7407075233842770334, 14.76736230305380992 ) ) ;
#60124 = CARTESIAN_POINT ( 'NONE',  ( 31.33290314143522082, -3.967499999999994476, 6.871911579029513106 ) ) ;
#60126 = VECTOR ( 'NONE', #7481, 1000.000000000000000 ) ;
#60125 = CARTESIAN_POINT ( 'NONE',  ( 3.332903141435219929, -3.967499999999994476, 6.871911579029513106 ) ) ;
#60127 = LINE ( 'NONE', #93451, #59827 ) ;
#60128 = AXIS2_PLACEMENT_3D ( 'NONE', #12387, #87815, #101537 ) ;
#60129 = DIRECTION ( 'NONE',  ( 0.7071067811865487940, 0.7071067811865463515, 0.000000000000000000 ) ) ;
#60130 = CARTESIAN_POINT ( 'NONE',  ( -60.48921356237309510, -27.52281430457097500, 5.000000000000000000 ) ) ;
#60131 = ORIENTED_EDGE ( 'NONE', *, *, #62008, .T. ) ;
#60132 = ORIENTED_EDGE ( 'NONE', *, *, #132094, .F. ) ;
#60133 = CARTESIAN_POINT ( 'NONE',  ( 93.02083333333331439, 7.949999999999999289, 2.130196079827431532 ) ) ;
#60134 = VECTOR ( 'NONE', #133946, 999.9999999999998863 ) ;
#60135 = ORIENTED_EDGE ( 'NONE', *, *, #15123, .T. ) ;
#60136 = ORIENTED_EDGE ( 'NONE', *, *, #91505, .F. ) ;
#60137 =( LENGTH_UNIT ( ) NAMED_UNIT ( * ) SI_UNIT ( .MILLI., .METRE. ) );
#60138 = LINE ( 'NONE', #16590, #20863 ) ;
#60139 = CARTESIAN_POINT ( 'NONE',  ( 0.8124618758394703821, -22.22500000000000142, 4.000000000000000000 ) ) ;
#60140 = VERTEX_POINT ( 'NONE', #126404 ) ;
#60141 = AXIS2_PLACEMENT_3D ( 'NONE', #48049, #136454, #37154 ) ;
#60142 = DIRECTION ( 'NONE',  ( -0.6830127018922180770, -0.6830127018922204085, -0.2588190451025213501 ) ) ;
#60143 = AXIS2_PLACEMENT_3D ( 'NONE', #47332, #112524, #91503 ) ;
#60144 = DIRECTION ( 'NONE',  ( 0.000000000000000000, -1.000000000000000000, -1.137193330093851361E-16 ) ) ;
#60145 = VECTOR ( 'NONE', #108017, 1000.000000000000227 ) ;
#60146 = DIRECTION ( 'NONE',  ( -0.7071067811865486830, -0.7071067811865464625, -0.000000000000000000 ) ) ;
#60147 = CARTESIAN_POINT ( 'NONE',  ( 125.7294590726101546, -0.005845708547400866630, -7.736937294360648920 ) ) ;
#60148 = VECTOR ( 'NONE', #137901, 1000.000000000000000 ) ;
#60149 = DIRECTION ( 'NONE',  ( 0.7071067811865487940, 0.7071067811865463515, 0.000000000000000000 ) ) ;
#60150 = CARTESIAN_POINT ( 'NONE',  ( 51.18398860626899705, 28.73617430169823095, 5.000000000000000000 ) ) ;
#60151 = VECTOR ( 'NONE', #133076, 1000.000000000000000 ) ;
#60152 = FACE_OUTER_BOUND ( 'NONE', #102668, .T. ) ;
#60153 = CARTESIAN_POINT ( 'NONE',  ( -15.81246187583935914, -22.22500000000000142, 4.000000000000000000 ) ) ;
#60154 = CARTESIAN_POINT ( 'NONE',  ( 13.11017322888201697, -22.22500000000000497, 4.785647885939354751 ) ) ;
#60155 = DIRECTION ( 'NONE',  ( 0.7071067811865487940, 0.7071067811865463515, 0.000000000000000000 ) ) ;
#60156 = PLANE ( 'NONE',  #102457 ) ;
#60157 = ORIENTED_EDGE ( 'NONE', *, *, #114383, .F. ) ;
#60158 = ORIENTED_EDGE ( 'NONE', *, *, #105621, .T. ) ;
#60159 = CARTESIAN_POINT ( 'NONE',  ( 111.2712635252314612, 4.472830434245839371, 4.472830434245842035 ) ) ;
#60160 = ORIENTED_EDGE ( 'NONE', *, *, #20126, .F. ) ;
#60161 = VECTOR ( 'NONE', #3533, 1000.000000000000000 ) ;
#60162 = FACE_OUTER_BOUND ( 'NONE', #107882, .T. ) ;
#60163 = VERTEX_POINT ( 'NONE', #105364 ) ;
#60164 = CARTESIAN_POINT ( 'NONE',  ( 18.00548008471250583, 28.92564299267925776, 4.000000000000000000 ) ) ;
#60165 = DIRECTION ( 'NONE',  ( -1.000000000000000000, -1.224606353822377258E-16, -0.000000000000000000 ) ) ;
#60166 = CARTESIAN_POINT ( 'NONE',  ( 109.2870968585647944, 3.054999999999997495, 5.291415217122919401 ) ) ;
#60167 = EDGE_LOOP ( 'NONE', ( #80879, #107152, #80739, #72709 ) ) ;
#60168 = CARTESIAN_POINT ( 'NONE',  ( -13.08100000000000307, 3.174999999999997158, 5.000000000000000000 ) ) ;
#60169 = VERTEX_POINT ( 'NONE', #38701 ) ;
#60170 = CARTESIAN_POINT ( 'NONE',  ( -11.84387692260750136, -22.22500000000000497, 4.000000000000000000 ) ) ;
#60171 = LINE ( 'NONE', #37709, #30668 ) ;
#60172 = CARTESIAN_POINT ( 'NONE',  ( -24.59263130292903554, 0.9595543924999635488, 5.000000000000000000 ) ) ;
#60173 = VERTEX_POINT ( 'NONE', #135871 ) ;
#60174 = ORIENTED_EDGE ( 'NONE', *, *, #97573, .F. ) ;
#60175 = EDGE_CURVE ( 'NONE', #128354, #70446, #27815, .T. ) ;
#60176 = ORIENTED_EDGE ( 'NONE', *, *, #136558, .T. ) ;
#60177 = DIRECTION ( 'NONE',  ( -0.7071067811865486830, -0.7071067811865464625, 0.000000000000000000 ) ) ;
#60178 = ADVANCED_FACE ( 'NONE', ( #80786 ), #48873, .F. ) ;
#60179 = DIRECTION ( 'NONE',  ( -0.3543493200069162685, -0.000000000000000000, -0.9351131265310288487 ) ) ;
#60180 = CARTESIAN_POINT ( 'NONE',  ( 7.796236474768553748, 7.934999999999990727, -1.457635852685135314E-15 ) ) ;
#60181 = CARTESIAN_POINT ( 'NONE',  ( 21.00000000000000000, 0.000000000000000000, 6.094999999999989981 ) ) ;
#60182 = VERTEX_POINT ( 'NONE', #93790 ) ;
#60184 = VERTEX_POINT ( 'NONE', #38006 ) ;
#60183 = EDGE_CURVE ( 'NONE', #134905, #119311, #139862, .T. ) ;
#60185 = FACE_OUTER_BOUND ( 'NONE', #47413, .T. ) ;
#60186 = ORIENTED_EDGE ( 'NONE', *, *, #16788, .F. ) ;
#60187 = ORIENTED_EDGE ( 'NONE', *, *, #13506, .F. ) ;
#60188 = DIRECTION ( 'NONE',  ( 0.3543493200069162685, -0.000000000000000000, -0.9351131265310288487 ) ) ;
#60189 = EDGE_CURVE ( 'NONE', #24896, #106536, #36551, .T. ) ;
#60190 = VECTOR ( 'NONE', #68641, 999.9999999999998863 ) ;
#60191 = DIRECTION ( 'NONE',  ( 1.000000000000000000, 0.000000000000000000, 0.000000000000000000 ) ) ;
#60192 = CARTESIAN_POINT ( 'NONE',  ( 34.49999999999976552, 3.073033219394661675, -6.593910359670890564 ) ) ;
#60193 = ORIENTED_EDGE ( 'NONE', *, *, #21591, .T. ) ;
#60194 = CARTESIAN_POINT ( 'NONE',  ( 6.562500000000000888, 4.461849672132300881, 4.461849672132299105 ) ) ;
#60195 = CARTESIAN_POINT ( 'NONE',  ( -26.99999999999982236, -2.904428200921339354, -6.989807076074882275 ) ) ;
#60197 = ADVANCED_FACE ( 'NONE', ( #3198 ), #82232, .F. ) ;
#60196 = VECTOR ( 'NONE', #125489, 1000.000000000000227 ) ;
#60198 = VECTOR ( 'NONE', #9946, 1000.000000000000000 ) ;
#60199 =( BOUNDED_CURVE ( )  B_SPLINE_CURVE ( 3, ( #135103, #121322, #90122, #67710 ),
 .UNSPECIFIED., .F., .T. ) 
 B_SPLINE_CURVE_WITH_KNOTS ( ( 4, 4 ),
 ( 4.517163242187656635, 4.562733109340372906 ),
 .UNSPECIFIED. ) 
 CURVE ( )  GEOMETRIC_REPRESENTATION_ITEM ( )  RATIONAL_B_SPLINE_CURVE ( ( 1.000000000000000000, 0.9998269564205118920, 0.9998269564205118920, 1.000000000000000000 ) ) 
 REPRESENTATION_ITEM ( '' )  );
#60200 = DIRECTION ( 'NONE',  ( -0.3543493200069162685, -0.000000000000000000, -0.9351131265310288487 ) ) ;
#60201 = AXIS2_PLACEMENT_3D ( 'NONE', #53226, #64848, #66989 ) ;
#60202 = CARTESIAN_POINT ( 'NONE',  ( 23.99451991528749062, 28.92564299267954908, 4.000000000000000000 ) ) ;
#60203 = FACE_BOUND ( 'NONE', #49266, .T. ) ;
#60204 = ORIENTED_EDGE ( 'NONE', *, *, #70681, .T. ) ;
#60205 = DIRECTION ( 'NONE',  ( 0.7071067811865487940, 0.7071067811865463515, 0.000000000000000000 ) ) ;
#60206 = CARTESIAN_POINT ( 'NONE',  ( -75.48921356237309510, -27.52281430457107803, 5.000000000000000000 ) ) ;
#60207 =( LENGTH_UNIT ( ) NAMED_UNIT ( * ) SI_UNIT ( .MILLI., .METRE. ) );
#60208 = ORIENTED_EDGE ( 'NONE', *, *, #79733, .F. ) ;
#60209 = DIRECTION ( 'NONE',  ( 0.000000000000000000, 0.000000000000000000, 1.000000000000000000 ) ) ;
#60210 = ORIENTED_EDGE ( 'NONE', *, *, #32857, .F. ) ;
#60212 = ORIENTED_EDGE ( 'NONE', *, *, #90372, .F. ) ;
#60211 = EDGE_CURVE ( 'NONE', #26318, #44215, #83661, .T. ) ;
#60213 = VECTOR ( 'NONE', #49797, 999.9999999999998863 ) ;
#60214 = VERTEX_POINT ( 'NONE', #114114 ) ;
#60215 = CARTESIAN_POINT ( 'NONE',  ( 40.74543019189810877, -5.291415217122918513, -3.055000000000000160 ) ) ;
#60216 = ORIENTED_EDGE ( 'NONE', *, *, #235, .F. ) ;
#60217 = CARTESIAN_POINT ( 'NONE',  ( 21.48921356237309155, -27.52281430457070499, 5.000000000000000000 ) ) ;
#60218 = LINE ( 'NONE', #5061, #138741 ) ;
#60219 = DIRECTION ( 'NONE',  ( 0.3543493200069162685, -0.000000000000000000, -0.9351131265310288487 ) ) ;
#60220 = EDGE_CURVE ( 'NONE', #63482, #89870, #14797, .T. ) ;
#60221 = ORIENTED_EDGE ( 'NONE', *, *, #108255, .F. ) ;
#60222 = CARTESIAN_POINT ( 'NONE',  ( -45.18398860626900415, 28.73617430169818832, 5.000000000000000000 ) ) ;
#60223 =( NAMED_UNIT ( * ) PLANE_ANGLE_UNIT ( ) SI_UNIT ( $, .RADIAN. ) );
#60224 = VECTOR ( 'NONE', #119108, 1000.000000000000000 ) ;
#60225 = AXIS2_PLACEMENT_3D ( 'NONE', #31309, #62522, #108108 ) ;
#60226 = DIRECTION ( 'NONE',  ( 0.000000000000000000, -0.3543493200069153248, -0.9351131265310291818 ) ) ;
#60227 = EDGE_CURVE ( 'NONE', #71803, #42501, #31986, .T. ) ;
#60228 = EDGE_CURVE ( 'NONE', #22767, #87580, #57852, .T. ) ;
#60229 = VECTOR ( 'NONE', #101133, 1000.000000000000000 ) ;
#60230 = DIRECTION ( 'NONE',  ( 0.000000000000000000, 0.000000000000000000, 1.000000000000000000 ) ) ;
#60231 = DIRECTION ( 'NONE',  ( -0.000000000000000000, 0.3543493200069153248, 0.9351131265310292928 ) ) ;
#60232 = LINE ( 'NONE', #139936, #22799 ) ;
#60233 = DIRECTION ( 'NONE',  ( -0.000000000000000000, 0.000000000000000000, 1.000000000000000000 ) ) ;
#60234 = ORIENTED_EDGE ( 'NONE', *, *, #98211, .F. ) ;
#60235 = CIRCLE ( 'NONE', #118123, 2.500000000000000444 ) ;
#60236 = EDGE_LOOP ( 'NONE', ( #56273, #67738, #79722, #116225 ) ) ;
#60237 = ORIENTED_EDGE ( 'NONE', *, *, #44337, .F. ) ;
#60238 = EDGE_LOOP ( 'NONE', ( #104099, #113786, #98854, #23575 ) ) ;
#60239 = DIRECTION ( 'NONE',  ( 1.000000000000000000, 0.000000000000000000, 0.000000000000000000 ) ) ;
#60240 = ORIENTED_EDGE ( 'NONE', *, *, #128865, .T. ) ;
#60241 = EDGE_CURVE ( 'NONE', #78067, #22380, #129988, .T. ) ;
#60242 = ORIENTED_EDGE ( 'NONE', *, *, #18021, .F. ) ;
#60243 = DIRECTION ( 'NONE',  ( -0.7071067811865486830, 0.7071067811865464625, 0.000000000000000000 ) ) ;
#60244 = ADVANCED_FACE ( 'NONE', ( #40839 ), #19783, .F. ) ;
#60245 = AXIS2_PLACEMENT_3D ( 'NONE', #73116, #5663, #84682 ) ;
#60246 = EDGE_CURVE ( 'NONE', #123521, #105758, #106056, .T. ) ;
#60247 = CARTESIAN_POINT ( 'NONE',  ( -34.92500000000001137, -19.29806943317879586, 4.500000000000000888 ) ) ;
#60248 = ORIENTED_EDGE ( 'NONE', *, *, #121353, .F. ) ;
#60249 = VECTOR ( 'NONE', #120354, 1000.000000000000114 ) ;
#60250 = CARTESIAN_POINT ( 'NONE',  ( -33.29974487139158867, -27.71228299555229313, 4.000000000000000000 ) ) ;
#60251 = ORIENTED_EDGE ( 'NONE', *, *, #38549, .T. ) ;
#60252 = LINE ( 'NONE', #104427, #53663 ) ;
#60253 = CARTESIAN_POINT ( 'NONE',  ( 33.02540314143521272, 2.126176841940962348, 7.934999999999989839 ) ) ;
#60254 = CARTESIAN_POINT ( 'NONE',  ( -1.537096858564780844, -3.967499999999994476, 6.871911579029513106 ) ) ;
#60255 = VERTEX_POINT ( 'NONE', #42994 ) ;
#60257 = CARTESIAN_POINT ( 'NONE',  ( -0.2800196798940397525, 0.7592924766157104211, 14.27032725228008836 ) ) ;
#60256 = CARTESIAN_POINT ( 'NONE',  ( 104.7662635252314516, 4.472830434245839371, -4.472830434245839371 ) ) ;
#60258 = EDGE_CURVE ( 'NONE', #76705, #15400, #136679, .T. ) ;
#60259 = LINE ( 'NONE', #39943, #7266 ) ;
#60260 = LINE ( 'NONE', #29035, #90604 ) ;
#60261 = EDGE_LOOP ( 'NONE', ( #59527, #44833, #39328, #93085 ) ) ;
#60262 = ORIENTED_EDGE ( 'NONE', *, *, #63416, .T. ) ;
#60263 = DIRECTION ( 'NONE',  ( -0.3543493200069162685, -0.000000000000000000, -0.9351131265310288487 ) ) ;
#60264 = ORIENTED_EDGE ( 'NONE', *, *, #98636, .T. ) ;
#60265 = FILL_AREA_STYLE ('',( #16728 ) ) ;
#60266 = CARTESIAN_POINT ( 'NONE',  ( -2.287690060339689690, -21.73547319004780931, 4.999917730833664642 ) ) ;
#60267 = DIRECTION ( 'NONE',  ( 0.7071067811865487940, 0.7071067811865463515, 0.000000000000000000 ) ) ;
#60269 = EDGE_CURVE ( 'NONE', #104004, #71281, #92689, .T. ) ;
#60268 = PLANE ( 'NONE',  #98594 ) ;
#60270 = CARTESIAN_POINT ( 'NONE',  ( 84.48921356237309510, -27.52281430457114197, 5.000000000000000000 ) ) ;
#60271 = DIRECTION ( 'NONE',  ( 0.7071067811865487940, 0.7071067811865463515, -0.000000000000000000 ) ) ;
#60272 = VERTEX_POINT ( 'NONE', #86496 ) ;
#60273 = CARTESIAN_POINT ( 'NONE',  ( 36.29974487139159578, -27.71228299555231445, 4.000000000000000000 ) ) ;
#60274 = CARTESIAN_POINT ( 'NONE',  ( 34.42499999999998295, 0.000000000000000000, 0.000000000000000000 ) ) ;
#60275 = LINE ( 'NONE', #71868, #30666 ) ;
#60276 = VERTEX_POINT ( 'NONE', #75614 ) ;
#60277 = LINE ( 'NONE', #28349, #32738 ) ;
#60278 = AXIS2_PLACEMENT_3D ( 'NONE', #54705, #126693, #43114 ) ;
#60279 = FACE_OUTER_BOUND ( 'NONE', #15621, .T. ) ;
#60280 = ORIENTED_EDGE ( 'NONE', *, *, #99965, .F. ) ;
#60282 = ORIENTED_EDGE ( 'NONE', *, *, #46669, .T. ) ;
#60281 = FACE_OUTER_BOUND ( 'NONE', #88161, .T. ) ;
#60283 = ORIENTED_EDGE ( 'NONE', *, *, #76128, .F. ) ;
#60284 = CARTESIAN_POINT ( 'NONE',  ( -14.50845100080809225, 8.197497501871428227, -27.90950007455948523 ) ) ;
#60285 = CARTESIAN_POINT ( 'NONE',  ( -34.92500000000001137, -19.29806943317879586, 4.500000000000000888 ) ) ;
#60287 = ORIENTED_EDGE ( 'NONE', *, *, #131479, .F. ) ;
#60286 = VECTOR ( 'NONE', #131609, 1000.000000000000000 ) ;
#60288 = LINE ( 'NONE', #93612, #95141 ) ;
#60289 = CLOSED_SHELL ( 'NONE', ( #136780, #40747, #44563, #86884, #767, #110031, #3830, #69897, #63794, #74783, #135732, #123440, #13722, #120977, #84162, #80307, #92646, #10928, #43764, #123985, #107148, #23995, #35482, #35032, #23692, #103096, #11118, #135962, #132670, #16493, #99237, #26156, #77890, #51575, #109987, #52130, #39802, #62497, #73745, #43203, #37432, #66096, #29220, #94713, #105376, #59207, #1075, #74319, #107280, #134189, #136629, #108422, #20043, #88261, #73224, #77279, #26633, #128635, #89651, #59913, #27376, #18636, #117047, #56333, #57921, #128175, #141480, #12391, #36709, #77865, #71633, #94604, #81511, #11124, #117908, #79290, #79884, #35155, #10800, #29825, #17139, #101974, #33436, #6633, #127766, #107630, #75300, #74789, #107913, #34741, #116879, #36130, #74894, #129780, #10316, #129212, #88006, #3826, #61535, #143359, #113872, #49425, #105725, #134714, #102260, #91349, #67626, #34464, #91999, #124332, #91267, #129577, #101593, #71532, #13456, #14402, #110923, #48256, #46425, #100085, #77676, #67029, #125870, #101944, #135543, #64190, #76644, #91604, #56664, #25386, #130442, #142986, #80989, #104668, #12052, #142591, #35537, #142801, #118651, #29021, #61982, #112573, #126156, #77361, #102446, #123903, #76442, #90111, #4424, #125631, #132211, #52359, #137284, #109567, #45854, #24957, #44886, #127588, #112775, #11739, #59644, #85193, #105087, #54828, #96266, #32266, #57131, #60681, #69390, #45985, #110576, #88214, #110985, #120420, #114234, #59096, #44482, #21504, #23168, #79961, #14520, #21146, #56989, #37185, #133824, #120266, #137992, #100440, #33561, #22863, #37800, #81283, #125952, #135135, #76583 ) ) ;
#60290 = EDGE_CURVE ( 'NONE', #50064, #86945, #117643, .T. ) ;
#60291 = LINE ( 'NONE', #62425, #75323 ) ;
#60292 = ADVANCED_FACE ( 'NONE', ( #140837 ), #9602, .T. ) ;
#60293 = DIRECTION ( 'NONE',  ( -0.7071067811865487940, 0.7071067811865463515, -0.000000000000000000 ) ) ;
#60294 = ORIENTED_EDGE ( 'NONE', *, *, #120268, .T. ) ;
#60295 = DIRECTION ( 'NONE',  ( 0.7071067811865487940, 0.7071067811865463515, 0.000000000000000000 ) ) ;
#60296 = DIRECTION ( 'NONE',  ( -0.7071067811865487940, 0.7071067811865463515, -0.000000000000000000 ) ) ;
#60297 = CARTESIAN_POINT ( 'NONE',  ( 14.27159235450332098, 9.902892378096218942E-16, 0.000000000000000000 ) ) ;
#60298 = CARTESIAN_POINT ( 'NONE',  ( -48.18398860626899705, 28.73617430169820608, 5.000000000000000000 ) ) ;
#60299 = CARTESIAN_POINT ( 'NONE',  ( -24.48921356237309510, -27.52281430457072631, 5.000000000000000000 ) ) ;
#60300 = DIRECTION ( 'NONE',  ( 0.7071067811865486830, -0.7071067811865464625, -0.000000000000000000 ) ) ;
#60301 = DIRECTION ( 'NONE',  ( 1.000000000000000000, 0.000000000000000000, 0.000000000000000000 ) ) ;
#60302 = LINE ( 'NONE', #137130, #22214 ) ;
#60303 = EDGE_LOOP ( 'NONE', ( #93382, #18190, #113443 ) ) ;
#60304 = VERTEX_POINT ( 'NONE', #30693 ) ;
#60305 = ORIENTED_EDGE ( 'NONE', *, *, #94390, .T. ) ;
#60306 = COLOUR_RGB ( '', 0.31764706, 0.68627451, 0.89019608) ;
#60307 = CARTESIAN_POINT ( 'NONE',  ( 122.1875000000000000, -5.819803920172573086, 5.819803920172572198 ) ) ;
#60308 = AXIS2_PLACEMENT_3D ( 'NONE', #31459, #30757, #74249 ) ;
#60309 = ORIENTED_EDGE ( 'NONE', *, *, #93283, .F. ) ;
#60310 = ORIENTED_EDGE ( 'NONE', *, *, #64921, .T. ) ;
#60311 = ORIENTED_EDGE ( 'NONE', *, *, #94469, .F. ) ;
#60312 = AXIS2_PLACEMENT_3D ( 'NONE', #140058, #38586, #129876 ) ;
#60313 = CARTESIAN_POINT ( 'NONE',  ( 5.443598275411213550, 3.061616997868383634E-16, -2.500000000000000444 ) ) ;
#60314 = PRESENTATION_LAYER_ASSIGNMENT (  '', '', ( #69517 ) ) ;
#60315 = VECTOR ( 'NONE', #21751, 1000.000000000000227 ) ;
#60316 = CIRCLE ( 'NONE', #16265, 0.5000000000000004441 ) ;
#60317 = VERTEX_POINT ( 'NONE', #74922 ) ;
#60318 = DIRECTION ( 'NONE',  ( 0.7071067811865486830, -0.7071067811865464625, -0.000000000000000000 ) ) ;
#60319 = VECTOR ( 'NONE', #33849, 1000.000000000000000 ) ;
#60320 = LINE ( 'NONE', #69780, #34797 ) ;
#60321 = DIRECTION ( 'NONE',  ( -0.000000000000000000, 0.000000000000000000, 1.000000000000000000 ) ) ;
#60322 = CARTESIAN_POINT ( 'NONE',  ( 116.6670968585647756, -3.055000000000000160, -5.291415217122921177 ) ) ;
#60323 = VERTEX_POINT ( 'NONE', #7469 ) ;
#60324 = DIRECTION ( 'NONE',  ( 0.3543493200069163240, 0.000000000000000000, -0.9351131265310288487 ) ) ;
#60325 = PLANE ( 'NONE',  #130348 ) ;
#60326 = CARTESIAN_POINT ( 'NONE',  ( -30.71230993966007716, -21.73547319004781286, 4.999917730833664642 ) ) ;
#60327 = AXIS2_PLACEMENT_3D ( 'NONE', #79788, #58755, #70337 ) ;
#60328 = CARTESIAN_POINT ( 'NONE',  ( 0.000000000000000000, 0.000000000000000000, 5.000000000000000000 ) ) ;
#60329 = DIRECTION ( 'NONE',  ( 0.7071067811865487940, 0.7071067811865463515, -0.000000000000000000 ) ) ;
#60330 = CARTESIAN_POINT ( 'NONE',  ( 35.66252705046288440, 7.949999999999998401, 1.460391307983218338E-15 ) ) ;
#60331 = DIRECTION ( 'NONE',  ( -1.000000000000000000, -1.224606353822377258E-16, -0.000000000000000000 ) ) ;
#60332 = FACE_OUTER_BOUND ( 'NONE', #129686, .T. ) ;
#60333 = ORIENTED_EDGE ( 'NONE', *, *, #105114, .T. ) ;
#60334 = ORIENTED_EDGE ( 'NONE', *, *, #28115, .T. ) ;
#60335 = CARTESIAN_POINT ( 'NONE',  ( 34.10416666666665719, 2.130196079827422206, 7.950000000000001954 ) ) ;
#60336 = ORIENTED_EDGE ( 'NONE', *, *, #41539, .F. ) ;
#60337 = EDGE_LOOP ( 'NONE', ( #13652, #51085, #93754, #130257 ) ) ;
#60338 = CARTESIAN_POINT ( 'NONE',  ( 0.000000000000000000, 0.000000000000000000, 5.000000000000000000 ) ) ;
#60339 = LINE ( 'NONE', #126284, #80251 ) ;
#60340 = ORIENTED_EDGE ( 'NONE', *, *, #48125, .F. ) ;
#60341 = FACE_OUTER_BOUND ( 'NONE', #140307, .T. ) ;
#60342 =( NAMED_UNIT ( * ) PLANE_ANGLE_UNIT ( ) SI_UNIT ( $, .RADIAN. ) );
#60343 = CARTESIAN_POINT ( 'NONE',  ( 66.48921356237309510, -27.52281430457101763, 5.000000000000000000 ) ) ;
#60344 = VECTOR ( 'NONE', #91226, 1000.000000000000000 ) ;
#60345 = CIRCLE ( 'NONE', #9347, 2.552699999999997971 ) ;
#60346 = CARTESIAN_POINT ( 'NONE',  ( 29.45876352523143993, 0.000000000000000000, -6.110000000000001208 ) ) ;
#60347 = EDGE_LOOP ( 'NONE', ( #85366, #4691, #105284, #133215 ) ) ;
#60348 = AXIS2_PLACEMENT_3D ( 'NONE', #119118, #109673, #130005 ) ;
#60349 = LINE ( 'NONE', #59638, #31762 ) ;
#60350 = VERTEX_POINT ( 'NONE', #108192 ) ;
#60351 = DIRECTION ( 'NONE',  ( -1.000000000000000000, -1.224606353822377258E-16, -0.000000000000000000 ) ) ;
#60352 = VECTOR ( 'NONE', #84373, 1000.000000000000000 ) ;
#60353 = DIRECTION ( 'NONE',  ( -0.7071067811865486830, -0.7071067811865464625, 0.000000000000000000 ) ) ;
#60354 = DIRECTION ( 'NONE',  ( 0.7071067811865487940, 0.7071067811865463515, 0.000000000000000000 ) ) ;
#60355 = EDGE_CURVE ( 'NONE', #42461, #18811, #97598, .T. ) ;
#60356 = PLANE ( 'NONE',  #125197 ) ;
#60357 = ORIENTED_EDGE ( 'NONE', *, *, #17579, .T. ) ;
#60358 = EDGE_CURVE ( 'NONE', #51588, #129879, #129746, .T. ) ;
#60359 = EDGE_CURVE ( 'NONE', #121292, #89747, #97315, .T. ) ;
#60360 = VERTEX_POINT ( 'NONE', #116961 ) ;
#60361 = MECHANICAL_DESIGN_GEOMETRIC_PRESENTATION_REPRESENTATION (  '', ( #41807 ), #141342 ) ;
#60362 = DIRECTION ( 'NONE',  ( -1.000000000000000000, -0.000000000000000000, -0.000000000000000000 ) ) ;
#60363 = FACE_OUTER_BOUND ( 'NONE', #42533, .T. ) ;
#60364 = LINE ( 'NONE', #14690, #8321 ) ;
#60365 = CARTESIAN_POINT ( 'NONE',  ( 10.49999999999993605, -2.173586137069121627, -4.605770156576090457 ) ) ;
#60366 = EDGE_CURVE ( 'NONE', #108894, #104436, #17628, .T. ) ;
#60367 = EDGE_CURVE ( 'NONE', #43828, #72705, #31392, .T. ) ;
#60368 = VECTOR ( 'NONE', #44628, 1000.000000000000000 ) ;
#60369 = CARTESIAN_POINT ( 'NONE',  ( 50.95376352523145158, -6.109999999999998543, -3.741295971395162543E-16 ) ) ;
#60370 = ORIENTED_EDGE ( 'NONE', *, *, #127772, .T. ) ;
#60371 = CARTESIAN_POINT ( 'NONE',  ( 124.8125000000000142, 5.819803920172571310, 5.819803920172576639 ) ) ;
#60372 = EDGE_CURVE ( 'NONE', #127035, #16309, #20482, .T. ) ;
#60373 = LINE ( 'NONE', #104553, #57235 ) ;
#60374 = VERTEX_POINT ( 'NONE', #95923 ) ;
#60375 = ORIENTED_EDGE ( 'NONE', *, *, #48896, .T. ) ;
#60376 = VECTOR ( 'NONE', #86343, 999.9999999999998863 ) ;
#60377 = LINE ( 'NONE', #137208, #35436 ) ;
#60378 = ORIENTED_EDGE ( 'NONE', *, *, #37913, .F. ) ;
#60379 = EDGE_CURVE ( 'NONE', #43144, #133750, #112513, .T. ) ;
#60380 = FACE_OUTER_BOUND ( 'NONE', #85164, .T. ) ;
#60381 = ORIENTED_EDGE ( 'NONE', *, *, #11903, .F. ) ;
#60382 = DIRECTION ( 'NONE',  ( -0.7071067811865487940, 0.7071067811865463515, 0.000000000000000000 ) ) ;
#60383 = AXIS2_PLACEMENT_3D ( 'NONE', #16714, #68981, #17421 ) ;
#60384 = EDGE_CURVE ( 'NONE', #123770, #98954, #120620, .T. ) ;
#60385 = LINE ( 'NONE', #81431, #132260 ) ;
#60386 = FACE_BOUND ( 'NONE', #32102, .T. ) ;
#60387 = DIRECTION ( 'NONE',  ( 0.000000000000000000, 0.000000000000000000, -1.000000000000000000 ) ) ;
#60388 = CARTESIAN_POINT ( 'NONE',  ( -42.48921356237308800, -27.52281430457085065, 5.000000000000000000 ) ) ;
#60389 = DIRECTION ( 'NONE',  ( -0.000000000000000000, 0.3543493200069153248, 0.9351131265310292928 ) ) ;
#60390 = ORIENTED_EDGE ( 'NONE', *, *, #96006, .F. ) ;
#60392 = ORIENTED_EDGE ( 'NONE', *, *, #94086, .F. ) ;
#60391 = DIRECTION ( 'NONE',  ( 0.3240768213499726214, 0.9146165434626271074, 0.2417659866237898969 ) ) ;
#60393 = EDGE_CURVE ( 'NONE', #134254, #11791, #56029, .T. ) ;
#60394 = AXIS2_PLACEMENT_3D ( 'NONE', #111828, #54597, #143016 ) ;
#60395 = DIRECTION ( 'NONE',  ( 0.7071067811865487940, -0.7071067811865463515, 0.000000000000000000 ) ) ;
#60396 = EDGE_LOOP ( 'NONE', ( #128323, #108763, #28601, #102253 ) ) ;
#60397 = VERTEX_POINT ( 'NONE', #21928 ) ;
#60398 = CARTESIAN_POINT ( 'NONE',  ( 66.84959685856478018, 6.109999999999996767, 1.637169565754163836 ) ) ;
#60399 = ORIENTED_EDGE ( 'NONE', *, *, #92964, .T. ) ;
#60400 = CARTESIAN_POINT ( 'NONE',  ( -29.99999999999978684, -3.485240976185105310, -4.108735105802465704 ) ) ;
#60401 = EDGE_CURVE ( 'NONE', #136233, #46484, #56756, .T. ) ;
#60402 = ORIENTED_EDGE ( 'NONE', *, *, #102224, .F. ) ;
#60403 = CARTESIAN_POINT ( 'NONE',  ( -34.92499999999999005, 2.729999999999986215, -36.39086428169088094 ) ) ;
#60404 = VECTOR ( 'NONE', #61038, 1000.000000000000000 ) ;
#60406 = EDGE_CURVE ( 'NONE', #110693, #3604, #88269, .T. ) ;
#60405 =( GEOMETRIC_REPRESENTATION_CONTEXT ( 3 ) GLOBAL_UNCERTAINTY_ASSIGNED_CONTEXT ( ( #47637 ) ) GLOBAL_UNIT_ASSIGNED_CONTEXT ( ( #86232, #108641, #31836 ) ) REPRESENTATION_CONTEXT ( 'NONE', 'WORKASPACE' ) );
#60407 = VECTOR ( 'NONE', #131484, 999.9999999999998863 ) ;
#60408 = CARTESIAN_POINT ( 'NONE',  ( -29.99999999999979039, 7.007997736742422212, -8.085015511992182269 ) ) ;
#60409 = DIRECTION ( 'NONE',  ( -0.000000000000000000, 0.000000000000000000, 1.000000000000000000 ) ) ;
#60410 = PLANE ( 'NONE',  #115304 ) ;
#60411 = EDGE_CURVE ( 'NONE', #35909, #48454, #869, .T. ) ;
#60412 = DIRECTION ( 'NONE',  ( -0.7071067811865486830, -0.7071067811865464625, 0.000000000000000000 ) ) ;
#60413 = FACE_OUTER_BOUND ( 'NONE', #124529, .T. ) ;
#60414 = ORIENTED_EDGE ( 'NONE', *, *, #106144, .T. ) ;
#60415 = VECTOR ( 'NONE', #53849, 1000.000000000000000 ) ;
#60416 = VECTOR ( 'NONE', #73636, 999.9999999999998863 ) ;
#60417 = EDGE_LOOP ( 'NONE', ( #96692, #20169, #104112, #112586 ) ) ;
#60418 = VECTOR ( 'NONE', #121808, 1000.000000000000000 ) ;
#60419 = DIRECTION ( 'NONE',  ( -1.000000000000000000, -1.224606353822377258E-16, -0.000000000000000000 ) ) ;
#60420 = DIRECTION ( 'NONE',  ( -1.000000000000000000, -7.992108492102899539E-15, 0.000000000000000000 ) ) ;
#60421 = ORIENTED_EDGE ( 'NONE', *, *, #123223, .F. ) ;
#60422 = EDGE_CURVE ( 'NONE', #116174, #121547, #90033, .T. ) ;
#60423 = VECTOR ( 'NONE', #65050, 1000.000000000000000 ) ;
#60424 = ORIENTED_EDGE ( 'NONE', *, *, #141234, .T. ) ;
#60425 = ORIENTED_EDGE ( 'NONE', *, *, #38820, .F. ) ;
#60426 = PLANE ( 'NONE',  #72158 ) ;
#60427 = CARTESIAN_POINT ( 'NONE',  ( -7.940000000000007496, -35.56014942880460694, -10.00000000000000178 ) ) ;
#60428 = ORIENTED_EDGE ( 'NONE', *, *, #9613, .T. ) ;
#60429 = AXIS2_PLACEMENT_3D ( 'NONE', #46257, #134685, #68706 ) ;
#60430 = DIRECTION ( 'NONE',  ( -0.7071067811865487940, 0.7071067811865463515, 0.000000000000000000 ) ) ;
#60431 = LINE ( 'NONE', #29189, #67877 ) ;
#60432 = CARTESIAN_POINT ( 'NONE',  ( 9.546236474768553748, -7.934999999999990727, 4.858786175617117713E-16 ) ) ;
#60433 = CARTESIAN_POINT ( 'NONE',  ( 5.671830600776438303, 11.25929247661560950, 4.000000000000000000 ) ) ;
#60434 = ORIENTED_EDGE ( 'NONE', *, *, #8369, .F. ) ;
#60436 = EDGE_CURVE ( 'NONE', #128691, #103116, #123423, .T. ) ;
#60435 = AXIS2_PLACEMENT_3D ( 'NONE', #948, #100990, #47390 ) ;
#60437 = CARTESIAN_POINT ( 'NONE',  ( 9.722814304570524868, -21.72500000000000497, 5.000000000000000000 ) ) ;
#60438 = PLANE ( 'NONE',  #4863 ) ;
#60439 = AXIS2_PLACEMENT_3D ( 'NONE', #100570, #1214, #78817 ) ;
#60440 = LINE ( 'NONE', #82195, #112280 ) ;
#60442 = ORIENTED_EDGE ( 'NONE', *, *, #99245, .T. ) ;
#60441 = CARTESIAN_POINT ( 'NONE',  ( 17.70025512860841488, -27.71228299555193786, 4.000000000000000000 ) ) ;
#60443 = CARTESIAN_POINT ( 'NONE',  ( 10.98330628287044064, 6.094999999999991758, 1.633150327867686880 ) ) ;
#60444 = VERTEX_POINT ( 'NONE', #13170 ) ;
#60445 = CARTESIAN_POINT ( 'NONE',  ( -8.999999999999932498, 14.87792677143808362, -11.06722581663441929 ) ) ;
#60446 = EDGE_CURVE ( 'NONE', #36066, #119351, #127580, .T. ) ;
#60447 = CARTESIAN_POINT ( 'NONE',  ( 0.000000000000000000, 0.000000000000000000, 5.000000000000000000 ) ) ;
#60448 = CARTESIAN_POINT ( 'NONE',  ( 108.3333333333333428, -6.884901960086287964, 3.974999999999998312 ) ) ;
#60449 = VERTEX_POINT ( 'NONE', #46600 ) ;
#60450 = CIRCLE ( 'NONE', #69765, 2.055000000000001048 ) ;
#60451 = VECTOR ( 'NONE', #39477, 999.9999999999998863 ) ;
#60452 = DIRECTION ( 'NONE',  ( -0.6830127018922181881, 0.6830127018922202975, -0.2588190451025214056 ) ) ;
#60453 = CARTESIAN_POINT ( 'NONE',  ( 120.5375270504628844, -9.735942053221456900E-16, 7.949999999999998401 ) ) ;
#60454 = CARTESIAN_POINT ( 'NONE',  ( -30.48921356237309510, -27.52281430457076894, 5.000000000000000000 ) ) ;
#60455 = ORIENTED_EDGE ( 'NONE', *, *, #97347, .T. ) ;
#60456 = DIRECTION ( 'NONE',  ( -0.000000000000000000, 0.000000000000000000, 1.000000000000000000 ) ) ;
#60457 = CIRCLE ( 'NONE', #34991, 3.999999999999989786 ) ;
#60458 = CARTESIAN_POINT ( 'NONE',  ( 2.816011393730999401, 28.73617430169785436, 5.000000000000000000 ) ) ;
#60459 = DIRECTION ( 'NONE',  ( 0.3543493200069162685, -0.000000000000000000, -0.9351131265310288487 ) ) ;
#60460 = CARTESIAN_POINT ( 'NONE',  ( -12.69999999999999929, -59.76999999999998892, -40.00000000000000000 ) ) ;
#60461 = CARTESIAN_POINT ( 'NONE',  ( 12.48921356237309155, -27.52281430457064104, 5.000000000000000000 ) ) ;
#60462 = ORIENTED_EDGE ( 'NONE', *, *, #36474, .F. ) ;
#60463 = ADVANCED_FACE ( 'NONE', ( #24085 ), #78470, .F. ) ;
#60464 = ORIENTED_EDGE ( 'NONE', *, *, #122066, .F. ) ;
#60465 = DIRECTION ( 'NONE',  ( -0.5735764363510507113, 0.8191520442889885789, 1.003171929053520926E-16 ) ) ;
#60466 =( NAMED_UNIT ( * ) PLANE_ANGLE_UNIT ( ) SI_UNIT ( $, .RADIAN. ) );
#60467 = CARTESIAN_POINT ( 'NONE',  ( 0.5620698081018862258, -7.934999999999991616, -2.126176841940955242 ) ) ;
#60468 = DIRECTION ( 'NONE',  ( 0.7071067811865486830, -0.7071067811865464625, -0.000000000000000000 ) ) ;
#60469 = ADVANCED_FACE ( 'NONE', ( #44439 ), #57444, .T. ) ;
#60470 = VECTOR ( 'NONE', #15717, 1000.000000000000000 ) ;
#60471 = FACE_OUTER_BOUND ( 'NONE', #105493, .T. ) ;
#60472 = CARTESIAN_POINT ( 'NONE',  ( 34.47516574401890210, -13.50948238788423872, 4.998110765256833510 ) ) ;
#60473 = DIRECTION ( 'NONE',  ( 0.7071067811865487940, -0.7071067811865463515, 0.000000000000000000 ) ) ;
#60474 = ORIENTED_EDGE ( 'NONE', *, *, #28660, .F. ) ;
#60475 = CARTESIAN_POINT ( 'NONE',  ( 2.816011393730999401, 28.73617430169785436, 5.000000000000000000 ) ) ;
#60476 = VECTOR ( 'NONE', #55513, 1000.000000000000000 ) ;
#60477 = DIRECTION ( 'NONE',  ( -1.000000000000000000, -1.224606353822377258E-16, -0.000000000000000000 ) ) ;
#60478 = VECTOR ( 'NONE', #109285, 1000.000000000000000 ) ;
#60479 = CARTESIAN_POINT ( 'NONE',  ( 12.69999999999999574, -22.33999999999998565, -0.5000000000000000000 ) ) ;
#60480 = CARTESIAN_POINT ( 'NONE',  ( 44.82876352523145158, 0.000000000000000000, -6.109999999999999432 ) ) ;
#60481 = EDGE_CURVE ( 'NONE', #66027, #52394, #89334, .T. ) ;
#60482 = DIRECTION ( 'NONE',  ( 0.6830127018922181881, 0.6830127018922202975, -0.2588190451025214056 ) ) ;
#60483 = EDGE_CURVE ( 'NONE', #78861, #137915, #66174, .T. ) ;
#60484 = EDGE_LOOP ( 'NONE', ( #79267, #36427, #82666, #1603 ) ) ;
#60485 = CARTESIAN_POINT ( 'NONE',  ( 156.1499999999997783, -49.14999999999999147, 34.92500000000004690 ) ) ;
#60486 = VERTEX_POINT ( 'NONE', #21219 ) ;
#60487 = ORIENTED_EDGE ( 'NONE', *, *, #91855, .T. ) ;
#60488 = DIRECTION ( 'NONE',  ( -0.6830127018922180770, -0.6830127018922204085, -0.2588190451025213501 ) ) ;
#60489 = CARTESIAN_POINT ( 'NONE',  ( 60.18398860626900415, 28.73617430169829490, 5.000000000000000000 ) ) ;
#60490 = DIRECTION ( 'NONE',  ( 0.3543493200069162685, -0.000000000000000000, -0.9351131265310288487 ) ) ;
#60491 = LINE ( 'NONE', #70660, #99430 ) ;
#60492 = ADVANCED_FACE ( 'NONE', ( #32840 ), #143001, .F. ) ;
#60493 = CARTESIAN_POINT ( 'NONE',  ( -34.92500000000001137, -16.29806943317882073, 4.500000000000000888 ) ) ;
#60494 = FACE_OUTER_BOUND ( 'NONE', #113053, .T. ) ;
#60495 = EDGE_LOOP ( 'NONE', ( #87946, #110865, #115460, #12506 ) ) ;
#60496 = CARTESIAN_POINT ( 'NONE',  ( 9.489213562373095101, -27.52281430457062328, 5.000000000000000000 ) ) ;
#60497 = CARTESIAN_POINT ( 'NONE',  ( -29.20710678118633297, -20.24070752338407075, 5.000000000000000000 ) ) ;
#60498 = UNCERTAINTY_MEASURE_WITH_UNIT (LENGTH_MEASURE( 1.000000000000000082E-05 ), #69301, 'distance_accuracy_value', 'NONE');
#60499 = VECTOR ( 'NONE', #109507, 1000.000000000000000 ) ;
#60500 = DIRECTION ( 'NONE',  ( 0.3543493200069162685, -0.000000000000000000, -0.9351131265310288487 ) ) ;
#60501 = DIRECTION ( 'NONE',  ( -0.7071067811865486830, 0.7071067811865464625, 0.000000000000000000 ) ) ;
#60502 = LINE ( 'NONE', #104679, #13276 ) ;
#60503 = CARTESIAN_POINT ( 'NONE',  ( 62.78752705046289151, 0.000000000000000000, -7.949999999999998401 ) ) ;
#60504 = LINE ( 'NONE', #50321, #73878 ) ;
#60505 = VERTEX_POINT ( 'NONE', #122661 ) ;
#60506 = ORIENTED_EDGE ( 'NONE', *, *, #58024, .F. ) ;
#60507 = CARTESIAN_POINT ( 'NONE',  ( 61.81249999999998579, 5.819803920172571310, 5.819803920172575751 ) ) ;
#60508 = FACE_OUTER_BOUND ( 'NONE', #92886, .T. ) ;
#60509 = CARTESIAN_POINT ( 'NONE',  ( -6.499999999999999112, 0.000000000000000000, 10.00000000000000000 ) ) ;
#60510 = CARTESIAN_POINT ( 'NONE',  ( -2.510786437626908008, -27.52281430457053446, 5.000000000000000000 ) ) ;
#60511 = VERTEX_POINT ( 'NONE', #10328 ) ;
#60512 = CARTESIAN_POINT ( 'NONE',  ( 33.95833333333332860, 3.974999999999997424, 6.884901960086288852 ) ) ;
#60513 = VECTOR ( 'NONE', #7008, 1000.000000000000000 ) ;
#60514 = AXIS2_PLACEMENT_3D ( 'NONE', #102069, #112935, #14343 ) ;
#60515 = DIRECTION ( 'NONE',  ( -1.369518533665900312E-16, 1.000000000000000000, -0.000000000000000000 ) ) ;
#60516 = CARTESIAN_POINT ( 'NONE',  ( 57.60459685856477563, 1.637169565754164946, -6.109999999999999432 ) ) ;
#60517 = EDGE_CURVE ( 'NONE', #99825, #7978, #54583, .T. ) ;
#60518 = DIRECTION ( 'NONE',  ( -1.000000000000000000, -0.000000000000000000, -0.000000000000000000 ) ) ;
#60519 = VERTEX_POINT ( 'NONE', #11742 ) ;
#60521 = VERTEX_POINT ( 'NONE', #137 ) ;
#60520 = VECTOR ( 'NONE', #107310, 999.9999999999998863 ) ;
#60522 = VECTOR ( 'NONE', #53128, 999.9999999999998863 ) ;
#60523 = AXIS2_PLACEMENT_3D ( 'NONE', #82560, #126750, #62247 ) ;
#60524 = VECTOR ( 'NONE', #139150, 1000.000000000000000 ) ;
#60525 = CARTESIAN_POINT ( 'NONE',  ( -60.48921356237309510, -27.52281430457097500, 5.000000000000000000 ) ) ;
#60527 = LINE ( 'NONE', #51774, #128713 ) ;
#60526 = CIRCLE ( 'NONE', #58272, 2.500000000000000444 ) ;
#60528 = CARTESIAN_POINT ( 'NONE',  ( -42.48921356237308800, -27.52281430457085065, 5.000000000000000000 ) ) ;
#60529 = CARTESIAN_POINT ( 'NONE',  ( 15.18079593298623564, 4.202752102959690472E-16, 0.000000000000000000 ) ) ;
#60530 = CARTESIAN_POINT ( 'NONE',  ( -15.67180000000000639, 3.174999999999997158, 5.000000000000000000 ) ) ;
#60531 = EDGE_CURVE ( 'NONE', #43404, #63283, #113711, .T. ) ;
#60532 = EDGE_CURVE ( 'NONE', #28611, #83522, #23345, .T. ) ;
#60534 = ORIENTED_EDGE ( 'NONE', *, *, #50171, .T. ) ;
#60533 = LINE ( 'NONE', #93834, #91548 ) ;
#60535 = CARTESIAN_POINT ( 'NONE',  ( -1.499999999999987566, -4.216083040037250207, -7.486842126848652690 ) ) ;
#60536 = FACE_OUTER_BOUND ( 'NONE', #124604, .T. ) ;
#60537 = CARTESIAN_POINT ( 'NONE',  ( 6.005480084712508493, 28.92564299267933947, 4.000000000000000000 ) ) ;
#60538 = VECTOR ( 'NONE', #8901, 1000.000000000000000 ) ;
#60539 = DIRECTION ( 'NONE',  ( 0.7071067811865487940, 0.7071067811865463515, 0.000000000000000000 ) ) ;
#60541 = ORIENTED_EDGE ( 'NONE', *, *, #3341, .T. ) ;
#60540 = EDGE_CURVE ( 'NONE', #45681, #37108, #16766, .T. ) ;
#60542 = EDGE_CURVE ( 'NONE', #143176, #12388, #51472, .T. ) ;
#60543 = EDGE_LOOP ( 'NONE', ( #109149, #8998, #120935 ) ) ;
#60544 = EDGE_CURVE ( 'NONE', #51106, #140375, #16016, .T. ) ;
#60545 = AXIS2_PLACEMENT_3D ( 'NONE', #126157, #17374, #26124 ) ;
#60546 = LINE ( 'NONE', #104718, #126398 ) ;
#60547 = LINE ( 'NONE', #80854, #125156 ) ;
#60548 = EDGE_CURVE ( 'NONE', #38530, #107625, #66294, .T. ) ;
#60549 = CARTESIAN_POINT ( 'NONE',  ( 0.000000000000000000, 0.000000000000000000, 5.000000000000000000 ) ) ;
#60550 = ORIENTED_EDGE ( 'NONE', *, *, #29927, .T. ) ;
#60551 = ORIENTED_EDGE ( 'NONE', *, *, #7015, .T. ) ;
#60552 = ADVANCED_FACE ( 'NONE', ( #92168 ), #81340, .F. ) ;
#60553 = CARTESIAN_POINT ( 'NONE',  ( -2.999999999999979128, 19.55218569542897100, 5.000000000000000000 ) ) ;
#60554 =( LENGTH_UNIT ( ) NAMED_UNIT ( * ) SI_UNIT ( .MILLI., .METRE. ) );
#60555 = EDGE_LOOP ( 'NONE', ( #135250, #116194, #19154, #40750 ) ) ;
#60556 = ADVANCED_FACE ( 'NONE', ( #116069 ), #61044, .T. ) ;
#60557 = ORIENTED_EDGE ( 'NONE', *, *, #47032, .F. ) ;
#60558 = AXIS2_PLACEMENT_3D ( 'NONE', #94184, #105759, #41236 ) ;
#60559 = LINE ( 'NONE', #28629, #16624 ) ;
#60560 = ORIENTED_EDGE ( 'NONE', *, *, #101580, .T. ) ;
#60561 = VECTOR ( 'NONE', #56339, 1000.000000000000000 ) ;
#60562 = DIRECTION ( 'NONE',  ( 1.000000000000000000, 0.000000000000000000, 0.000000000000000000 ) ) ;
#60563 = DIRECTION ( 'NONE',  ( 0.000000000000000000, 0.000000000000000000, 1.000000000000000000 ) ) ;
#60564 = AXIS2_PLACEMENT_3D ( 'NONE', #140507, #62989, #41194 ) ;
#60565 = EDGE_CURVE ( 'NONE', #46809, #119897, #2547, .T. ) ;
#60566 = FACE_BOUND ( 'NONE', #9902, .T. ) ;
#60567 = VECTOR ( 'NONE', #46594, 1000.000000000000000 ) ;
#60568 = FACE_OUTER_BOUND ( 'NONE', #21315, .T. ) ;
#60569 = APPLICATION_CONTEXT ( 'automotive_design' ) ;
#60570 = CARTESIAN_POINT ( 'NONE',  ( 34.42499999999998295, -6.022814304570537125, 5.000000000000000000 ) ) ;
#60571 = LINE ( 'NONE', #5406, #138537 ) ;
#60573 = ORIENTED_EDGE ( 'NONE', *, *, #111323, .F. ) ;
#60572 = LINE ( 'NONE', #40238, #57423 ) ;
#60574 = EDGE_CURVE ( 'NONE', #94828, #125282, #35711, .T. ) ;
#60575 = DIRECTION ( 'NONE',  ( -0.000000000000000000, 0.000000000000000000, 1.000000000000000000 ) ) ;
#60576 = PRODUCT_CONTEXT ( 'NONE', #121683, 'mechanical' ) ;
#60577 = ORIENTED_EDGE ( 'NONE', *, *, #49012, .F. ) ;
#60578 = ORIENTED_EDGE ( 'NONE', *, *, #113531, .T. ) ;
#60579 = CARTESIAN_POINT ( 'NONE',  ( 91.64126352523143737, 4.472830434245835818, 4.472830434245840259 ) ) ;
#60580 = VERTEX_POINT ( 'NONE', #79934 ) ;
#60581 = FACE_OUTER_BOUND ( 'NONE', #119079, .T. ) ;
#60582 = VECTOR ( 'NONE', #78336, 999.9999999999998863 ) ;
#60583 = DIRECTION ( 'NONE',  ( -0.7071067811865487940, 0.7071067811865463515, 0.000000000000000000 ) ) ;
#60584 = VECTOR ( 'NONE', #79929, 999.9999999999998863 ) ;
#60585 = CARTESIAN_POINT ( 'NONE',  ( 21.87889065874226091, 8.431076354171498366, 5.000000000000000000 ) ) ;
#60586 = PLANE ( 'NONE',  #109573 ) ;
#60588 = VERTEX_POINT ( 'NONE', #102376 ) ;
#60587 = EDGE_CURVE ( 'NONE', #13630, #22921, #58908, .T. ) ;
#60589 = LINE ( 'NONE', #116357, #101675 ) ;
#60590 = CARTESIAN_POINT ( 'NONE',  ( 0.000000000000000000, 0.000000000000000000, 5.000000000000000000 ) ) ;
#60591 = PLANE ( 'NONE',  #64315 ) ;
#60592 = VECTOR ( 'NONE', #141901, 1000.000000000000227 ) ;
#60594 = CARTESIAN_POINT ( 'NONE',  ( 35.99451991528749772, 28.92564299267963079, 4.000000000000000000 ) ) ;
#60593 = DIRECTION ( 'NONE',  ( -0.6830127018922181881, 0.6830127018922202975, -0.2588190451025214056 ) ) ;
#60595 = EDGE_CURVE ( 'NONE', #50924, #79752, #3025, .T. ) ;
#60596 = FACE_OUTER_BOUND ( 'NONE', #107493, .T. ) ;
#60597 = DIRECTION ( 'NONE',  ( 0.6830127018922181881, 0.6830127018922202975, -0.2588190451025214056 ) ) ;
#60598 = AXIS2_PLACEMENT_3D ( 'NONE', #6522, #20290, #52224 ) ;
#60599 = DIRECTION ( 'NONE',  ( 0.3543493200069163240, -0.000000000000000000, 0.9351131265310288487 ) ) ;
#60600 = ORIENTED_EDGE ( 'NONE', *, *, #25058, .T. ) ;
#60601 = DIRECTION ( 'NONE',  ( -0.6830127018922180770, -0.6830127018922204085, -0.2588190451025213501 ) ) ;
#60602 = EDGE_CURVE ( 'NONE', #47430, #140430, #91489, .T. ) ;
#60603 = LINE ( 'NONE', #49714, #30365 ) ;
#60604 = VERTEX_POINT ( 'NONE', #26227 ) ;
#60605 = EDGE_LOOP ( 'NONE', ( #97324, #121088, #3306, #132034 ) ) ;
#60606 = ORIENTED_EDGE ( 'NONE', *, *, #84406, .T. ) ;
#60607 = CARTESIAN_POINT ( 'NONE',  ( 46.37543019189810423, -5.291415217122920289, -3.055000000000001492 ) ) ;
#60608 = AXIS2_PLACEMENT_3D ( 'NONE', #35195, #125022, #11970 ) ;
#60609 = ORIENTED_EDGE ( 'NONE', *, *, #12251, .T. ) ;
#60610 = CARTESIAN_POINT ( 'NONE',  ( 18.71247294953710494, 0.000000000000000000, 6.094999999999989981 ) ) ;
#60611 = CARTESIAN_POINT ( 'NONE',  ( -9.486600348837527008, 9.794720693715408544, -29.02262996827379737 ) ) ;
#60612 = VERTEX_POINT ( 'NONE', #36387 ) ;
#60613 = ADVANCED_FACE ( 'NONE', ( #80617 ), #124816, .F. ) ;
#60614 = CARTESIAN_POINT ( 'NONE',  ( 9.208651418775088970, 4.584330080086930965E-16, 0.000000000000000000 ) ) ;
#60615 = ORIENTED_EDGE ( 'NONE', *, *, #63238, .T. ) ;
#60616 = DIRECTION ( 'NONE',  ( 0.000000000000000000, 0.000000000000000000, 1.000000000000000000 ) ) ;
#60617 = VECTOR ( 'NONE', #95366, 1000.000000000000000 ) ;
#60618 = VECTOR ( 'NONE', #116011, 1000.000000000000000 ) ;
#60620 = ORIENTED_EDGE ( 'NONE', *, *, #84945, .T. ) ;
#60619 = LINE ( 'NONE', #5451, #109551 ) ;
#60621 = EDGE_LOOP ( 'NONE', ( #132120, #130417, #73130, #109347 ) ) ;
#60622 =( BOUNDED_CURVE ( )  B_SPLINE_CURVE ( 3, ( #19386, #10629, #143304, #141151 ),
 .UNSPECIFIED., .F., .F. ) 
 B_SPLINE_CURVE_WITH_KNOTS ( ( 4, 4 ),
 ( 2.779374508378133601, 4.199602562396795413 ),
 .UNSPECIFIED. ) 
 CURVE ( )  GEOMETRIC_REPRESENTATION_ITEM ( )  RATIONAL_B_SPLINE_CURVE ( ( 1.000000000000000000, 0.8388583629366719308, 0.8388583629366719308, 1.000000000000000000 ) ) 
 REPRESENTATION_ITEM ( '' )  );
#60623 = LINE ( 'NONE', #38834, #60832 ) ;
#60624 = CARTESIAN_POINT ( 'NONE',  ( 24.87999999999999901, 9.521314400968980422E-16, 0.000000000000000000 ) ) ;
#60625 = AXIS2_PLACEMENT_3D ( 'NONE', #80043, #124218, #24894 ) ;
#60627 = ORIENTED_EDGE ( 'NONE', *, *, #13522, .F. ) ;
#60626 = VECTOR ( 'NONE', #91723, 1000.000000000000114 ) ;
#60628 = DIRECTION ( 'NONE',  ( -0.7071067811865486830, -0.7071067811865464625, 0.000000000000000000 ) ) ;
#60629 = VERTEX_POINT ( 'NONE', #70490 ) ;
#60630 = VERTEX_POINT ( 'NONE', #4392 ) ;
#60631 = EDGE_CURVE ( 'NONE', #237, #64363, #109038, .T. ) ;
#60632 = ORIENTED_EDGE ( 'NONE', *, *, #66247, .T. ) ;
#60633 = ORIENTED_EDGE ( 'NONE', *, *, #46227, .T. ) ;
#60634 = DIRECTION ( 'NONE',  ( -0.3543493200069162685, -0.000000000000000000, -0.9351131265310288487 ) ) ;
#60635 = VECTOR ( 'NONE', #119266, 1000.000000000000000 ) ;
#60636 = AXIS2_PLACEMENT_3D ( 'NONE', #43702, #45171, #58201 ) ;
#60637 = AXIS2_PLACEMENT_3D ( 'NONE', #134474, #133063, #131615 ) ;
#60638 = STYLED_ITEM ( 'NONE', ( #69271 ), #143376 ) ;
#60639 = VECTOR ( 'NONE', #89199, 1000.000000000000000 ) ;
#60640 = VECTOR ( 'NONE', #107296, 999.9999999999998863 ) ;
#60641 = LINE ( 'NONE', #93925, #137212 ) ;
#60642 = DIRECTION ( 'NONE',  ( -0.7071067811865487940, 0.7071067811865463515, -0.000000000000000000 ) ) ;
#60643 = EDGE_CURVE ( 'NONE', #87975, #129879, #8690, .T. ) ;
#60644 = CARTESIAN_POINT ( 'NONE',  ( -1.499999999999989120, 16.77039438581778796, 0.4657186855307757778 ) ) ;
#60645 = CARTESIAN_POINT ( 'NONE',  ( 6.799968779831584875, 8.259292476615627265, 16.85664084051839495 ) ) ;
#60647 = EDGE_LOOP ( 'NONE', ( #105658, #43759, #93233, #142205 ) ) ;
#60646 = VECTOR ( 'NONE', #122718, 999.9999999999998863 ) ;
#60648 = DIRECTION ( 'NONE',  ( -0.7071067811865487940, 0.7071067811865463515, -0.000000000000000000 ) ) ;
#60649 = CARTESIAN_POINT ( 'NONE',  ( 28.41623647476855652, -7.934999999999990727, 4.858786175617117713E-16 ) ) ;
#60650 = EDGE_CURVE ( 'NONE', #112059, #98928, #117480, .T. ) ;
#60651 = DIRECTION ( 'NONE',  ( -0.000000000000000000, -0.3543493200069152693, 0.9351131265310292928 ) ) ;
#60652 = LINE ( 'NONE', #117108, #46039 ) ;
#60653 = CARTESIAN_POINT ( 'NONE',  ( 1.500000000000000000, 0.000000000000000000, 3.113037248396092416 ) ) ;
#60654 = VERTEX_POINT ( 'NONE', #96431 ) ;
#60655 = EDGE_LOOP ( 'NONE', ( #35435, #40685, #61628, #30497 ) ) ;
#60656 = ORIENTED_EDGE ( 'NONE', *, *, #74756, .F. ) ;
#60657 = CARTESIAN_POINT ( 'NONE',  ( 60.29974487139158867, -27.71228299555248142, 4.000000000000000000 ) ) ;
#60658 = DIRECTION ( 'NONE',  ( 0.7071067811865487940, 0.7071067811865463515, 0.000000000000000000 ) ) ;
#60659 = UNCERTAINTY_MEASURE_WITH_UNIT (LENGTH_MEASURE( 1.000000000000000082E-05 ), #123568, 'distance_accuracy_value', 'NONE');
#60660 = CARTESIAN_POINT ( 'NONE',  ( -0.4892135623730947680, -27.52281430457055578, 5.000000000000000000 ) ) ;
#60661 = DIRECTION ( 'NONE',  ( -1.000000000000000000, -1.224606353822377258E-16, -0.000000000000000000 ) ) ;
#60662 = CARTESIAN_POINT ( 'NONE',  ( 0.4397996348738452688, -49.08473565290605478, -39.91868829876771230 ) ) ;
#60663 = CARTESIAN_POINT ( 'NONE',  ( 71.66209685856478018, -5.291415217122919401, 3.054999999999998384 ) ) ;
#60664 = EDGE_CURVE ( 'NONE', #63809, #31526, #9418, .T. ) ;
#60665 = VECTOR ( 'NONE', #64298, 1000.000000000000000 ) ;
#60666 = CARTESIAN_POINT ( 'NONE',  ( 74.89169371712955581, 2.130196079827421762, 7.950000000000000178 ) ) ;
#60667 = VECTOR ( 'NONE', #74998, 1000.000000000000000 ) ;
#60668 = LINE ( 'NONE', #93954, #32184 ) ;
#60669 = EDGE_CURVE ( 'NONE', #95099, #41659, #64557, .T. ) ;
#60670 = CARTESIAN_POINT ( 'NONE',  ( 20.36747333860806819, 2.499999999999998224, 3.061616997868380183E-16 ) ) ;
#60671 = LINE ( 'NONE', #104831, #136964 ) ;
#60672 = VECTOR ( 'NONE', #32604, 1000.000000000000000 ) ;
#60673 = LINE ( 'NONE', #14956, #85855 ) ;
#60674 = ORIENTED_EDGE ( 'NONE', *, *, #58095, .T. ) ;
#60676 = VECTOR ( 'NONE', #140351, 1000.000000000000000 ) ;
#60675 = DIRECTION ( 'NONE',  ( -0.7071067811865487940, 0.7071067811865463515, -0.000000000000000000 ) ) ;
#60677 = ORIENTED_EDGE ( 'NONE', *, *, #110587, .F. ) ;
#60678 = CARTESIAN_POINT ( 'NONE',  ( -6.299744871391586898, -27.71228299555210484, 4.000000000000000000 ) ) ;
#60680 = ORIENTED_EDGE ( 'NONE', *, *, #10444, .T. ) ;
#60679 = CARTESIAN_POINT ( 'NONE',  ( 2.139447441471317379, 4.584330080086930965E-16, 0.000000000000000000 ) ) ;
#60681 = ADVANCED_FACE ( 'NONE', ( #107340 ), #48851, .T. ) ;
#60682 = DIRECTION ( 'NONE',  ( -0.6830127018922181881, 0.6830127018922202975, -0.2588190451025214056 ) ) ;
#60683 = ORIENTED_EDGE ( 'NONE', *, *, #124157, .F. ) ;
#60684 = LINE ( 'NONE', #85055, #101701 ) ;
#60685 = VERTEX_POINT ( 'NONE', #105887 ) ;
#60686 = CARTESIAN_POINT ( 'NONE',  ( -6.792893218813405909, -11.24070752338416845, 5.000000000000000000 ) ) ;
#60687 = ORIENTED_EDGE ( 'NONE', *, *, #126316, .F. ) ;
#60688 = AXIS2_PLACEMENT_3D ( 'NONE', #7566, #40941, #41638 ) ;
#60689 = LINE ( 'NONE', #80276, #137604 ) ;
#60690 = CARTESIAN_POINT ( 'NONE',  ( 92.97502705046289861, -5.819803920172572198, 5.819803920172572198 ) ) ;
#60691 = CARTESIAN_POINT ( 'NONE',  ( 72.02083333333334281, 7.949999999999998401, 2.130196079827431532 ) ) ;
#60692 = DIRECTION ( 'NONE',  ( 0.6830127018922180770, -0.6830127018922204085, -0.2588190451025213501 ) ) ;
#60693 = ORIENTED_EDGE ( 'NONE', *, *, #95661, .F. ) ;
#60694 = CARTESIAN_POINT ( 'NONE',  ( 12.69999999999999574, -35.13237070076361590, 17.62370837922860645 ) ) ;
#60695 = CARTESIAN_POINT ( 'NONE',  ( -3.299744871391591339, -27.71228299555208352, 4.000000000000000000 ) ) ;
#60697 = VECTOR ( 'NONE', #56462, 1000.000000000000000 ) ;
#60696 = CARTESIAN_POINT ( 'NONE',  ( 23.04166666666666785, 3.047499999999993214, -5.278424836066146320 ) ) ;
#60698 =( NAMED_UNIT ( * ) SI_UNIT ( $, .STERADIAN. ) SOLID_ANGLE_UNIT ( ) );
#60700 = AXIS2_PLACEMENT_3D ( 'NONE', #30323, #85397, #31060 ) ;
#60699 = DIRECTION ( 'NONE',  ( 0.6830127018922181881, 0.6830127018922202975, -0.2588190451025214056 ) ) ;
#60701 = ORIENTED_EDGE ( 'NONE', *, *, #108086, .F. ) ;
#60702 = PLANE ( 'NONE',  #67670 ) ;
#60703 = ORIENTED_EDGE ( 'NONE', *, *, #67098, .T. ) ;
#60704 = CARTESIAN_POINT ( 'NONE',  ( 81.66709685856477563, -3.055000000000000160, -5.291415217122921177 ) ) ;
#60705 = FACE_OUTER_BOUND ( 'NONE', #125317, .T. ) ;
#60707 = AXIS2_PLACEMENT_3D ( 'NONE', #49580, #28523, #59732 ) ;
#60706 = CARTESIAN_POINT ( 'NONE',  ( -60.48921356237309510, -27.52281430457097500, 5.000000000000000000 ) ) ;
#60708 = DIRECTION ( 'NONE',  ( -0.000000000000000000, 0.000000000000000000, 1.000000000000000000 ) ) ;
#60709 = ORIENTED_EDGE ( 'NONE', *, *, #15992, .T. ) ;
#60710 = DIRECTION ( 'NONE',  ( -0.6830127018922181881, 0.6830127018922202975, -0.2588190451025214056 ) ) ;
#60711 = CARTESIAN_POINT ( 'NONE',  ( 36.18398860626899705, 28.73617430169812437, 5.000000000000000000 ) ) ;
#60712 = CARTESIAN_POINT ( 'NONE',  ( 1.516262732464673579, 3.821174125832445049E-16, 0.000000000000000000 ) ) ;
#60713 = DIRECTION ( 'NONE',  ( -0.6830127018922180770, -0.6830127018922204085, -0.2588190451025213501 ) ) ;
#60715 = ORIENTED_EDGE ( 'NONE', *, *, #72986, .T. ) ;
#60714 = FACE_OUTER_BOUND ( 'NONE', #63383, .T. ) ;
#60716 = LINE ( 'NONE', #17170, #124791 ) ;
#60717 = FACE_OUTER_BOUND ( 'NONE', #66842, .T. ) ;
#60718 = EDGE_LOOP ( 'NONE', ( #10883, #83384, #110967, #5556 ) ) ;
#60719 = ORIENTED_EDGE ( 'NONE', *, *, #87769, .T. ) ;
#60720 = VERTEX_POINT ( 'NONE', #72631 ) ;
#60721 = ADVANCED_FACE ( 'NONE', ( #84204 ), #127689, .T. ) ;
#60722 = CARTESIAN_POINT ( 'NONE',  ( 70.43793019189810423, -6.110000000000001208, 1.637169565754158951 ) ) ;
#60723 = VERTEX_POINT ( 'NONE', #6551 ) ;
#60724 = EDGE_CURVE ( 'NONE', #49304, #31707, #94321, .T. ) ;
#60725 = FACE_OUTER_BOUND ( 'NONE', #137226, .T. ) ;
#60726 = CARTESIAN_POINT ( 'NONE',  ( 8.816011393731004731, 28.73617430169781173, 5.000000000000000000 ) ) ;
#60727 = EDGE_CURVE ( 'NONE', #53759, #96641, #95021, .T. ) ;
#60728 = LINE ( 'NONE', #17182, #122075 ) ;
#60729 = CARTESIAN_POINT ( 'NONE',  ( -23.99999999999982592, -3.412538124160721331, 4.000000000000000000 ) ) ;
#60730 = ORIENTED_EDGE ( 'NONE', *, *, #24011, .F. ) ;
#60731 = VECTOR ( 'NONE', #26397, 1000.000000000000000 ) ;
#60732 = CIRCLE ( 'NONE', #81609, 2.055000000000000604 ) ;
#60733 = AXIS2_PLACEMENT_3D ( 'NONE', #3599, #124000, #45051 ) ;
#60734 = ADVANCED_FACE ( 'NONE', ( #28375 ), #99739, .T. ) ;
#60735 = DIRECTION ( 'NONE',  ( -0.7071067811865486830, -0.7071067811865464625, 0.000000000000000000 ) ) ;
#60736 = FACE_OUTER_BOUND ( 'NONE', #39971, .T. ) ;
#60737 = VECTOR ( 'NONE', #142255, 1000.000000000000000 ) ;
#60738 = AXIS2_PLACEMENT_3D ( 'NONE', #101719, #135105, #110431 ) ;
#60739 = VERTEX_POINT ( 'NONE', #39988 ) ;
#60740 = EDGE_CURVE ( 'NONE', #128218, #132831, #116790, .T. ) ;
#60741 = CARTESIAN_POINT ( 'NONE',  ( -6.183988606268994381, 28.73617430169791476, 5.000000000000000000 ) ) ;
#60743 = PLANE ( 'NONE',  #87220 ) ;
#60742 = AXIS2_PLACEMENT_3D ( 'NONE', #140192, #40879, #72113 ) ;
#60744 = DIRECTION ( 'NONE',  ( 1.000000000000000000, 0.000000000000000000, 0.000000000000000000 ) ) ;
#60745 = VECTOR ( 'NONE', #24961, 1000.000000000000000 ) ;
#60746 = COLOUR_RGB ( '', 0.72549020, 0.75294118, 0.79215686) ;
#60747 = EDGE_LOOP ( 'NONE', ( #80350, #25038, #46910, #92751 ) ) ;
#60748 = ORIENTED_EDGE ( 'NONE', *, *, #54209, .F. ) ;
#60749 = EDGE_CURVE ( 'NONE', #79680, #53418, #29766, .T. ) ;
#60750 = CARTESIAN_POINT ( 'NONE',  ( 65.16666666666667140, 6.884901960086285300, 3.975000000000003642 ) ) ;
#60751 = EDGE_CURVE ( 'NONE', #21250, #33900, #8010, .T. ) ;
#60752 = CARTESIAN_POINT ( 'NONE',  ( 31.40832548098981647, -0.7407075233842735917, 14.76736230305387920 ) ) ;
#60753 = DIRECTION ( 'NONE',  ( 0.7071067811865486830, -0.7071067811865464625, -0.000000000000000000 ) ) ;
#60754 = CARTESIAN_POINT ( 'NONE',  ( 25.39999999999999858, -5.131256043349313067, -6.052638797879072108 ) ) ;
#60755 = CARTESIAN_POINT ( 'NONE',  ( 54.03752705046288440, -9.735942053221456900E-16, 7.949999999999998401 ) ) ;
#60756 = ADVANCED_FACE ( 'NONE', ( #17473 ), #128400, .F. ) ;
#60757 = CARTESIAN_POINT ( 'NONE',  ( 36.18398860626899705, 28.73617430169812437, 5.000000000000000000 ) ) ;
#60758 = VERTEX_POINT ( 'NONE', #42116 ) ;
#60759 = VERTEX_POINT ( 'NONE', #119619 ) ;
#60760 = ORIENTED_EDGE ( 'NONE', *, *, #2288, .T. ) ;
#60761 = ORIENTED_EDGE ( 'NONE', *, *, #34335, .T. ) ;
#60762 = AXIS2_PLACEMENT_3D ( 'NONE', #71107, #2954, #81268 ) ;
#60763 = LINE ( 'NONE', #49861, #29333 ) ;
#60764 = AXIS2_PLACEMENT_3D ( 'NONE', #20384, #76224, #142901 ) ;
#60765 = DIRECTION ( 'NONE',  ( 0.7071067811865487940, -0.7071067811865463515, 0.000000000000000000 ) ) ;
#60766 = VERTEX_POINT ( 'NONE', #63168 ) ;
#60767 = CARTESIAN_POINT ( 'NONE',  ( 31.82816939922330945, 0.7592924766157138627, 4.000000000000000000 ) ) ;
#60768 = LINE ( 'NONE', #94050, #128167 ) ;
#60769 = VECTOR ( 'NONE', #35304, 1000.000000000000000 ) ;
#60770 = PLANE ( 'NONE',  #87393 ) ;
#60771 = ADVANCED_FACE ( 'NONE', ( #86328 ), #130547, .T. ) ;
#60772 = CARTESIAN_POINT ( 'NONE',  ( -42.18398860626899705, 28.73617430169816700, 5.000000000000000000 ) ) ;
#60773 = VECTOR ( 'NONE', #36943, 1000.000000000000000 ) ;
#60774 = LINE ( 'NONE', #60026, #83834 ) ;
#60775 = ORIENTED_EDGE ( 'NONE', *, *, #31453, .T. ) ;
#60776 = CARTESIAN_POINT ( 'NONE',  ( 20.99999999999985079, 8.816494571476654940, 4.604407763760433703 ) ) ;
#60777 = DIRECTION ( 'NONE',  ( -0.000000000000000000, -1.000000000000000000, -0.000000000000000000 ) ) ;
#60778 = ORIENTED_EDGE ( 'NONE', *, *, #72475, .F. ) ;
#60779 = DIRECTION ( 'NONE',  ( -0.7071067811865486830, 0.7071067811865464625, 0.000000000000000000 ) ) ;
#60780 = VERTEX_POINT ( 'NONE', #140674 ) ;
#60781 = EDGE_LOOP ( 'NONE', ( #111951, #105874, #17577, #8371, #62748 ) ) ;
#60782 = LINE ( 'NONE', #61487, #124569 ) ;
#60783 = ORIENTED_EDGE ( 'NONE', *, *, #71256, .T. ) ;
#60784 = ORIENTED_EDGE ( 'NONE', *, *, #3817, .T. ) ;
#60785 = CARTESIAN_POINT ( 'NONE',  ( 74.95876352523143282, 0.000000000000000000, -6.110000000000001208 ) ) ;
#60786 = VECTOR ( 'NONE', #106701, 1000.000000000000000 ) ;
#60787 = VERTEX_POINT ( 'NONE', #41364 ) ;
#60788 = LINE ( 'NONE', #139759, #49689 ) ;
#60789 = CARTESIAN_POINT ( 'NONE',  ( 109.0837635252314470, -6.110000000000001208, -3.741295971395164515E-16 ) ) ;
#60790 = CARTESIAN_POINT ( 'NONE',  ( -39.48921356237310221, -27.52281430457082934, 5.000000000000000000 ) ) ;
#60791 = EDGE_CURVE ( 'NONE', #106916, #64860, #129808, .T. ) ;
#60792 = AXIS2_PLACEMENT_3D ( 'NONE', #59818, #5392, #49674 ) ;
#60793 = LINE ( 'NONE', #41130, #66137 ) ;
#60794 = VECTOR ( 'NONE', #39804, 1000.000000000000227 ) ;
#60795 = CARTESIAN_POINT ( 'NONE',  ( -39.18398860626899705, 28.73617430169814568, 5.000000000000000000 ) ) ;
#60796 = CARTESIAN_POINT ( 'NONE',  ( 15.65467068707222076, -2.499999999999996447, 0.000000000000000000 ) ) ;
#60797 = SURFACE_SIDE_STYLE ('',( #91268 ) ) ;
#60798 = VERTEX_POINT ( 'NONE', #34800 ) ;
#60799 = CARTESIAN_POINT ( 'NONE',  ( 131.7507865773015112, -49.14999999999999147, 40.57473644908944976 ) ) ;
#60800 = EDGE_CURVE ( 'NONE', #19214, #105592, #13334, .T. ) ;
#60801 = ORIENTED_EDGE ( 'NONE', *, *, #138891, .F. ) ;
#60802 = ORIENTED_EDGE ( 'NONE', *, *, #89071, .T. ) ;
#60803 = VECTOR ( 'NONE', #21744, 1000.000000000000227 ) ;
#60804 = CARTESIAN_POINT ( 'NONE',  ( 113.8291937171295558, -3.975000000000001865, 6.884901960086284411 ) ) ;
#60806 = ORIENTED_EDGE ( 'NONE', *, *, #83262, .T. ) ;
#60805 = AXIS2_PLACEMENT_3D ( 'NONE', #125421, #34301, #78524 ) ;
#60807 = CARTESIAN_POINT ( 'NONE',  ( 32.99451991528749062, 28.92564299267960948, 4.000000000000000000 ) ) ;
#60808 = DIRECTION ( 'NONE',  ( -0.7071067811865486830, -0.7071067811865464625, 0.000000000000000000 ) ) ;
#60809 = ADVANCED_FACE ( 'NONE', ( #53703 ), #142836, .F. ) ;
#60810 = DIRECTION ( 'NONE',  ( -0.6830127018922181881, 0.6830127018922202975, -0.2588190451025214056 ) ) ;
#60811 = CARTESIAN_POINT ( 'NONE',  ( 15.48921356237309510, -27.52281430457066236, 5.000000000000000000 ) ) ;
#60812 = ORIENTED_EDGE ( 'NONE', *, *, #99781, .T. ) ;
#60813 = CARTESIAN_POINT ( 'NONE',  ( -69.48921356237309510, -27.52281430457103895, 5.000000000000000000 ) ) ;
#60814 = VECTOR ( 'NONE', #100242, 1000.000000000000000 ) ;
#60815 = ORIENTED_EDGE ( 'NONE', *, *, #67100, .T. ) ;
#60816 =( BOUNDED_CURVE ( )  B_SPLINE_CURVE ( 3, ( #84126, #41287, #72558, #51477 ),
 .UNSPECIFIED., .F., .F. ) 
 B_SPLINE_CURVE_WITH_KNOTS ( ( 4, 4 ),
 ( 4.350170835173031492, 4.500739107949213391 ),
 .UNSPECIFIED. ) 
 CURVE ( )  GEOMETRIC_REPRESENTATION_ITEM ( )  RATIONAL_B_SPLINE_CURVE ( ( 1.000000000000000000, 0.9981116584018958626, 0.9981116584018958626, 1.000000000000000000 ) ) 
 REPRESENTATION_ITEM ( '' )  );
#60817 = CARTESIAN_POINT ( 'NONE',  ( 28.50456980810189123, 6.871911579029510442, -3.967499999999998916 ) ) ;
#60818 = CARTESIAN_POINT ( 'NONE',  ( 17.99451991528748351, 28.92564299267950645, 4.000000000000000000 ) ) ;
#60819 = LINE ( 'NONE', #138339, #99167 ) ;
#60820 = CARTESIAN_POINT ( 'NONE',  ( 27.18398860626900060, 28.73617430169806042, 5.000000000000000000 ) ) ;
#60821 = VERTEX_POINT ( 'NONE', #89176 ) ;
#60822 = VERTEX_POINT ( 'NONE', #99298 ) ;
#60823 = ORIENTED_EDGE ( 'NONE', *, *, #51814, .T. ) ;
#60824 = DIRECTION ( 'NONE',  ( 0.6830127018922180770, -0.6830127018922204085, -0.2588190451025213501 ) ) ;
#60825 = DIRECTION ( 'NONE',  ( 0.7071067811865486830, -0.7071067811865464625, -0.000000000000000000 ) ) ;
#60826 = VECTOR ( 'NONE', #97706, 1000.000000000000227 ) ;
#60828 = DIRECTION ( 'NONE',  ( 0.9961946980917455452, 1.067350013832299517E-17, 0.08715574274765836016 ) ) ;
#60827 = CIRCLE ( 'NONE', #23842, 2.500000000000000888 ) ;
#60829 = AXIS2_PLACEMENT_3D ( 'NONE', #79302, #35787, #56832 ) ;
#60831 = ADVANCED_FACE ( 'NONE', ( #110883 ), #100054, .F. ) ;
#60830 = PLANE ( 'NONE',  #57859 ) ;
#60832 = VECTOR ( 'NONE', #127251, 1000.000000000000000 ) ;
#60833 = DIRECTION ( 'NONE',  ( -0.000000000000000000, 0.000000000000000000, 1.000000000000000000 ) ) ;
#60834 = AXIS2_PLACEMENT_3D ( 'NONE', #100678, #23826, #44914 ) ;
#60835 = LINE ( 'NONE', #28879, #53177 ) ;
#60836 = ADVANCED_FACE ( 'NONE', ( #42828 ), #33401, .F. ) ;
#60837 = DIRECTION ( 'NONE',  ( -0.3543493200069162685, -0.000000000000000000, -0.9351131265310288487 ) ) ;
#60838 = FACE_OUTER_BOUND ( 'NONE', #9800, .T. ) ;
#60839 = VERTEX_POINT ( 'NONE', #23923 ) ;
#60840 = CARTESIAN_POINT ( 'NONE',  ( 25.08376352523143638, -6.110000000000001208, -3.741295971395164515E-16 ) ) ;
#60841 = VECTOR ( 'NONE', #77102, 1000.000000000000000 ) ;
#60842 = AXIS2_PLACEMENT_3D ( 'NONE', #137327, #136584, #48169 ) ;
#60843 = DIRECTION ( 'NONE',  ( 0.7071067811865486830, -0.7071067811865464625, -0.000000000000000000 ) ) ;
#60844 = ORIENTED_EDGE ( 'NONE', *, *, #12062, .F. ) ;
#60845 = LINE ( 'NONE', #1557, #22724 ) ;
#60846 = EDGE_CURVE ( 'NONE', #27137, #107846, #77602, .T. ) ;
#60848 = ORIENTED_EDGE ( 'NONE', *, *, #101005, .F. ) ;
#60847 = CARTESIAN_POINT ( 'NONE',  ( 55.86145213702158685, -48.75494892434144845, -38.51155878621100470 ) ) ;
#60849 = EDGE_CURVE ( 'NONE', #93195, #80263, #88470, .T. ) ;
#60850 = DIRECTION ( 'NONE',  ( -1.000000000000000000, -1.224606353822377258E-16, -0.000000000000000000 ) ) ;
#60851 = DIRECTION ( 'NONE',  ( -0.3543493200069162685, -0.000000000000000000, -0.9351131265310288487 ) ) ;
#60852 = ORIENTED_EDGE ( 'NONE', *, *, #102377, .F. ) ;
#60853 = PLANE ( 'NONE',  #16474 ) ;
#60854 = VERTEX_POINT ( 'NONE', #76157 ) ;
#60855 = LINE ( 'NONE', #114458, #21995 ) ;
#60856 = CARTESIAN_POINT ( 'NONE',  ( 0.000000000000000000, 0.000000000000000000, 5.000000000000000000 ) ) ;
#60857 = CARTESIAN_POINT ( 'NONE',  ( 122.5791937171295700, 3.975000000000002753, -6.884901960086283523 ) ) ;
#60858 = CARTESIAN_POINT ( 'NONE',  ( 0.4892135623730947680, -27.52281430457055578, 5.000000000000000000 ) ) ;
#60859 = VECTOR ( 'NONE', #80091, 1000.000000000000000 ) ;
#60860 = DIRECTION ( 'NONE',  ( -0.7071067811865487940, 0.7071067811865463515, -0.000000000000000000 ) ) ;
#60861 = CARTESIAN_POINT ( 'NONE',  ( 24.48921356237309510, -27.52281430457072631, 5.000000000000000000 ) ) ;
#60862 = CARTESIAN_POINT ( 'NONE',  ( 7.939999999999994174, -60.26999999999998892, -10.00000000000000178 ) ) ;
#60863 = CARTESIAN_POINT ( 'NONE',  ( 54.48921356237310221, -27.52281430457093236, 5.000000000000000000 ) ) ;
#60864 = CARTESIAN_POINT ( 'NONE',  ( 25.79123647476855652, -9.717572351234235426E-16, -7.934999999999990727 ) ) ;
#60865 = CARTESIAN_POINT ( 'NONE',  ( 6.103736474768552078, 5.808823158059035485, 5.808823158059032821 ) ) ;
#60866 = CARTESIAN_POINT ( 'NONE',  ( -62.99451991528749772, 28.92564299267982264, 4.000000000000000000 ) ) ;
#60867 = CARTESIAN_POINT ( 'NONE',  ( 11.99999999999991296, -8.731860332648832212, -2.120594902707510165 ) ) ;
#60868 = DIRECTION ( 'NONE',  ( 0.3543493200069162685, -0.000000000000000000, -0.9351131265310288487 ) ) ;
#60869 = ORIENTED_EDGE ( 'NONE', *, *, #887, .T. ) ;
#60870 = EDGE_CURVE ( 'NONE', #60255, #133359, #112437, .T. ) ;
#60871 = VECTOR ( 'NONE', #39912, 999.9999999999998863 ) ;
#60872 = EDGE_LOOP ( 'NONE', ( #239, #117484, #38157, #51803 ) ) ;
#60873 = CARTESIAN_POINT ( 'NONE',  ( 78.72916666666667140, 7.950000000000001954, -2.130196079827421762 ) ) ;
#60875 = ORIENTED_EDGE ( 'NONE', *, *, #72299, .T. ) ;
#60874 = FILL_AREA_STYLE_COLOUR ( '', #120694 ) ;
#60876 = ORIENTED_EDGE ( 'NONE', *, *, #59902, .T. ) ;
#60877 = PRODUCT_DEFINITION_SHAPE ( 'NONE', 'NONE',  #91726 ) ;
#60878 = VECTOR ( 'NONE', #114539, 1000.000000000000227 ) ;
#60879 = CARTESIAN_POINT ( 'NONE',  ( 11.28769006033964928, -21.73547319004781642, 4.999917730833663754 ) ) ;
#60880 = CARTESIAN_POINT ( 'NONE',  ( 23.52497294953710849, -4.461849672132299993, -4.461849672132299105 ) ) ;
#60881 = COLOUR_RGB ( '', 0.31764706, 0.68627451, 0.89019608) ;
#60882 = COLOUR_RGB ( '', 0.09019608, 0.27058824, 0.51372549) ;
#60883 = ORIENTED_EDGE ( 'NONE', *, *, #103611, .F. ) ;
#60884 = DIRECTION ( 'NONE',  ( 0.3543493200069163240, 0.000000000000000000, 0.9351131265310288487 ) ) ;
#60885 = CARTESIAN_POINT ( 'NONE',  ( 18.63425672184678916, 3.061616997868383634E-16, -2.500000000000000444 ) ) ;
#60886 = CARTESIAN_POINT ( 'NONE',  ( -39.18398860626899705, 28.73617430169814568, 5.000000000000000000 ) ) ;
#60887 = CARTESIAN_POINT ( 'NONE',  ( 126.1031985511058622, 5.455129984951537558, -4.927627306428293608 ) ) ;
#60888 = CARTESIAN_POINT ( 'NONE',  ( -12.20000000000000284, -34.64999999999999147, 17.49210858042621908 ) ) ;
#60889 = CARTESIAN_POINT ( 'NONE',  ( -53.99451991528749062, 28.92564299267975869, 4.000000000000000000 ) ) ;
#60890 = FILL_AREA_STYLE ('',( #115897 ) ) ;
#60891 = CARTESIAN_POINT ( 'NONE',  ( 6.489213562373093325, -27.52281430457059841, 5.000000000000000000 ) ) ;
#60892 = CARTESIAN_POINT ( 'NONE',  ( 54.18398860626899705, 28.73617430169825226, 5.000000000000000000 ) ) ;
#60893 = DIRECTION ( 'NONE',  ( 0.6830127018922180770, -0.6830127018922204085, -0.2588190451025213501 ) ) ;
#60894 =( LENGTH_UNIT ( ) NAMED_UNIT ( * ) SI_UNIT ( .MILLI., .METRE. ) );
#60895 = ORIENTED_EDGE ( 'NONE', *, *, #121526, .T. ) ;
#60896 = ORIENTED_EDGE ( 'NONE', *, *, #86854, .T. ) ;
#60897 = EDGE_CURVE ( 'NONE', #95607, #10314, #66707, .T. ) ;
#60898 = CARTESIAN_POINT ( 'NONE',  ( 112.0004301918981042, -3.055000000000002380, 5.291415217122920289 ) ) ;
#60899 = ORIENTED_EDGE ( 'NONE', *, *, #125319, .F. ) ;
#60900 = EDGE_CURVE ( 'NONE', #137014, #129906, #60457, .T. ) ;
#60901 = VECTOR ( 'NONE', #16844, 1000.000000000000114 ) ;
#60902 = AXIS2_PLACEMENT_3D ( 'NONE', #131627, #132368, #54098 ) ;
#60903 = DIRECTION ( 'NONE',  ( -0.7071067811865486830, -0.7071067811865464625, 0.000000000000000000 ) ) ;
#60904 = ORIENTED_EDGE ( 'NONE', *, *, #118026, .T. ) ;
#60905 = EDGE_CURVE ( 'NONE', #93164, #125049, #42175, .T. ) ;
#60906 = ADVANCED_FACE ( 'NONE', ( #22449 ), #133403, .T. ) ;
#60907 = CARTESIAN_POINT ( 'NONE',  ( 75.95833333333332860, 3.974999999999997424, 6.884901960086288852 ) ) ;
#60908 = CARTESIAN_POINT ( 'NONE',  ( -12.69999999999998153, 0.000000000000000000, 0.000000000000000000 ) ) ;
#60909 = CARTESIAN_POINT ( 'NONE',  ( 105.7870968585647802, 3.054999999999997495, 5.291415217122919401 ) ) ;
#60910 = ORIENTED_EDGE ( 'NONE', *, *, #7495, .T. ) ;
#60911 = LINE ( 'NONE', #41977, #21188 ) ;
#60912 = ORIENTED_EDGE ( 'NONE', *, *, #22315, .F. ) ;
#60913 = FACE_OUTER_BOUND ( 'NONE', #86849, .T. ) ;
#60914 = AXIS2_PLACEMENT_3D ( 'NONE', #143250, #75863, #42542 ) ;
#60915 = CARTESIAN_POINT ( 'NONE',  ( 39.48921356237310221, -27.52281430457082934, 5.000000000000000000 ) ) ;
#60916 = CARTESIAN_POINT ( 'NONE',  ( 24.59263130292903554, 0.9595543924999635488, 5.000000000000000000 ) ) ;
#60917 = LINE ( 'NONE', #50009, #36988 ) ;
#60918 = ORIENTED_EDGE ( 'NONE', *, *, #84010, .T. ) ;
#60919 = ORIENTED_EDGE ( 'NONE', *, *, #14087, .F. ) ;
#60920 = EDGE_CURVE ( 'NONE', #69887, #123337, #110183, .T. ) ;
#60921 = ORIENTED_EDGE ( 'NONE', *, *, #97145, .F. ) ;
#60922 = LINE ( 'NONE', #105770, #5067 ) ;
#60923 = EDGE_CURVE ( 'NONE', #16634, #127668, #36229, .T. ) ;
#60924 = CARTESIAN_POINT ( 'NONE',  ( -30.70710678118632941, -3.740707523384243505, 5.000000000000000000 ) ) ;
#60925 = CARTESIAN_POINT ( 'NONE',  ( 5.608736474768551972, -5.808823158059033709, 5.808823158059035485 ) ) ;
#60926 = VECTOR ( 'NONE', #47700, 1000.000000000000227 ) ;
#60927 = DIRECTION ( 'NONE',  ( 1.000000000000000000, 0.000000000000000000, 0.000000000000000000 ) ) ;
#60928 = EDGE_CURVE ( 'NONE', #103350, #35337, #82575, .T. ) ;
#60929 = LINE ( 'NONE', #5023, #100957 ) ;
#60930 = VERTEX_POINT ( 'NONE', #49261 ) ;
#60931 = ORIENTED_EDGE ( 'NONE', *, *, #22429, .T. ) ;
#60932 = DIRECTION ( 'NONE',  ( -1.000000000000000000, -1.224606353822377258E-16, -0.000000000000000000 ) ) ;
#60933 = EDGE_LOOP ( 'NONE', ( #39870, #127876, #30655, #50457 ) ) ;
#60934 = VERTEX_POINT ( 'NONE', #126768 ) ;
#60935 = EDGE_CURVE ( 'NONE', #103049, #46733, #37356, .T. ) ;
#60936 = AXIS2_PLACEMENT_3D ( 'NONE', #41512, #8832, #107488 ) ;
#60937 = VECTOR ( 'NONE', #26196, 1000.000000000000000 ) ;
#60938 = CARTESIAN_POINT ( 'NONE',  ( 110.7454301918981088, -5.291415217122918513, -3.055000000000000160 ) ) ;
#60939 = VECTOR ( 'NONE', #69875, 1000.000000000000000 ) ;
#60940 = DIRECTION ( 'NONE',  ( -0.7071067811865487940, 0.7071067811865463515, 0.000000000000000000 ) ) ;
#60941 = CARTESIAN_POINT ( 'NONE',  ( -23.29387692260788612, 22.22500000000000142, 4.000000000000000000 ) ) ;
#60942 = VERTEX_POINT ( 'NONE', #26758 ) ;
#60943 = PLANE ( 'NONE',  #36794 ) ;
#60945 = CARTESIAN_POINT ( 'NONE',  ( -24.81246187583929697, -22.22500000000000142, 4.000000000000000000 ) ) ;
#60944 = AXIS2_PLACEMENT_3D ( 'NONE', #81470, #26351, #90910 ) ;
#60946 = EDGE_CURVE ( 'NONE', #92779, #50212, #102199, .T. ) ;
#60947 = VECTOR ( 'NONE', #133248, 1000.000000000000000 ) ;
#60948 = COLOUR_RGB ( '', 0.31764706, 0.68627451, 0.89019608) ;
#60949 =( NAMED_UNIT ( * ) SI_UNIT ( $, .STERADIAN. ) SOLID_ANGLE_UNIT ( ) );
#60950 = DIRECTION ( 'NONE',  ( -0.7071067811865486830, 0.7071067811865464625, 0.000000000000000000 ) ) ;
#60951 = ORIENTED_EDGE ( 'NONE', *, *, #7319, .T. ) ;
#60952 = DIRECTION ( 'NONE',  ( 0.7071067811865487940, 0.7071067811865463515, 0.000000000000000000 ) ) ;
#60953 = FACE_BOUND ( 'NONE', #121919, .T. ) ;
#60954 = ORIENTED_EDGE ( 'NONE', *, *, #116864, .F. ) ;
#60955 = DIRECTION ( 'NONE',  ( 0.7071067811865486830, -0.7071067811865464625, -0.000000000000000000 ) ) ;
#60956 = DIRECTION ( 'NONE',  ( 0.7071067811865487940, 0.7071067811865463515, -0.000000000000000000 ) ) ;
#60957 = VERTEX_POINT ( 'NONE', #69588 ) ;
#60958 = EDGE_CURVE ( 'NONE', #35148, #61512, #115157, .T. ) ;
#60959 = LINE ( 'NONE', #105118, #34236 ) ;
#60960 = ORIENTED_EDGE ( 'NONE', *, *, #139279, .F. ) ;
#60961 = ORIENTED_EDGE ( 'NONE', *, *, #113419, .F. ) ;
#60962 = ORIENTED_EDGE ( 'NONE', *, *, #53900, .T. ) ;
#60963 = EDGE_CURVE ( 'NONE', #68120, #45628, #123036, .T. ) ;
#60964 = CARTESIAN_POINT ( 'NONE',  ( 33.45376352523145158, -6.109999999999998543, -3.741295971395162543E-16 ) ) ;
#60965 = EDGE_LOOP ( 'NONE', ( #40020, #30887, #78728, #22700 ) ) ;
#60966 = FACE_OUTER_BOUND ( 'NONE', #24748, .T. ) ;
#60967 = LINE ( 'NONE', #107258, #143379 ) ;
#60968 = DIRECTION ( 'NONE',  ( 0.000000000000000000, -1.000000000000000000, 0.000000000000000000 ) ) ;
#60969 = LINE ( 'NONE', #130474, #52866 ) ;
#60970 = CARTESIAN_POINT ( 'NONE',  ( -2.999999999999969802, -0.4125381241607498639, 4.000000000000000000 ) ) ;
#60972 = CARTESIAN_POINT ( 'NONE',  ( 0.000000000000000000, -57.15000000000009095, 34.92499999999998295 ) ) ;
#60971 = VECTOR ( 'NONE', #122419, 1000.000000000000000 ) ;
#60973 = FILL_AREA_STYLE_COLOUR ( '', #120002 ) ;
#60974 = DIRECTION ( 'NONE',  ( 0.6830127018922181881, 0.6830127018922202975, -0.2588190451025214056 ) ) ;
#60975 = FACE_OUTER_BOUND ( 'NONE', #85553, .T. ) ;
#60976 = AXIS2_PLACEMENT_3D ( 'NONE', #124251, #14044, #91626 ) ;
#60977 = CARTESIAN_POINT ( 'NONE',  ( -21.70710678118638270, -6.740707523384218192, 5.000000000000000000 ) ) ;
#60978 = EDGE_CURVE ( 'NONE', #667, #79834, #48516, .T. ) ;
#60979 = ORIENTED_EDGE ( 'NONE', *, *, #41209, .T. ) ;
#60980 = ORIENTED_EDGE ( 'NONE', *, *, #143326, .F. ) ;
#60981 = EDGE_LOOP ( 'NONE', ( #115830, #5228, #32943, #72374, #127642 ) ) ;
#60982 = EDGE_LOOP ( 'NONE', ( #29036, #117426, #11481 ) ) ;
#60983 = ORIENTED_EDGE ( 'NONE', *, *, #80195, .F. ) ;
#60984 = AXIS2_PLACEMENT_3D ( 'NONE', #87687, #101232, #14228 ) ;
#60985 = ORIENTED_EDGE ( 'NONE', *, *, #65994, .T. ) ;
#60986 = LINE ( 'NONE', #28319, #125418 ) ;
#60987 = ADVANCED_FACE ( 'NONE', ( #35542 ), #68870, .F. ) ;
#60988 = CARTESIAN_POINT ( 'NONE',  ( -11.99999999999992006, -3.485240976185087991, -4.108735105802425736 ) ) ;
#60989 = ORIENTED_EDGE ( 'NONE', *, *, #64980, .F. ) ;
#60990 = DIRECTION ( 'NONE',  ( -1.000000000000000000, -0.000000000000000000, -0.000000000000000000 ) ) ;
#60991 = ORIENTED_EDGE ( 'NONE', *, *, #882, .F. ) ;
#60993 = VECTOR ( 'NONE', #68850, 1000.000000000000000 ) ;
#60992 = DIRECTION ( 'NONE',  ( -0.000000000000000000, 0.3543493200069153248, 0.9351131265310292928 ) ) ;
#60994 = CARTESIAN_POINT ( 'NONE',  ( 32.44206980810188412, 7.934999999999993392, 2.126176841940951689 ) ) ;
#60995 = VECTOR ( 'NONE', #124970, 1000.000000000000000 ) ;
#60996 = CARTESIAN_POINT ( 'NONE',  ( 1.962903141435219601, -3.967499999999994476, 6.871911579029513106 ) ) ;
#60997 = ORIENTED_EDGE ( 'NONE', *, *, #28065, .T. ) ;
#60999 = DIRECTION ( 'NONE',  ( -0.7071067811865486830, -0.7071067811865464625, 0.000000000000000000 ) ) ;
#60998 = CARTESIAN_POINT ( 'NONE',  ( 102.7245968585647802, -1.637169565754161171, 6.109999999999998543 ) ) ;
#61000 = CARTESIAN_POINT ( 'NONE',  ( 15.70701326429294475, -21.74070752338405654, 4.999753212805220670 ) ) ;
#61001 = CARTESIAN_POINT ( 'NONE',  ( -11.81601139373100651, 28.73617430169779041, 5.000000000000000000 ) ) ;
#61002 = ORIENTED_EDGE ( 'NONE', *, *, #130615, .F. ) ;
#61003 = ORIENTED_EDGE ( 'NONE', *, *, #95216, .T. ) ;
#61004 = PLANE ( 'NONE',  #86618 ) ;
#61005 = ORIENTED_EDGE ( 'NONE', *, *, #20708, .F. ) ;
#61007 = AXIS2_PLACEMENT_3D ( 'NONE', #106082, #138765, #116282 ) ;
#61006 = FACE_OUTER_BOUND ( 'NONE', #58484, .T. ) ;
#61008 = DIRECTION ( 'NONE',  ( -0.6830127018922181881, 0.6830127018922202975, -0.2588190451025214056 ) ) ;
#61009 = SURFACE_STYLE_USAGE ( .BOTH. , #80586 ) ;
#61010 = LINE ( 'NONE', #2253, #23844 ) ;
#61011 =( LENGTH_UNIT ( ) NAMED_UNIT ( * ) SI_UNIT ( .MILLI., .METRE. ) );
#61012 = EDGE_LOOP ( 'NONE', ( #115933, #42082, #128542, #80411, #131649 ) ) ;
#61013 = CARTESIAN_POINT ( 'NONE',  ( -21.48921356237309155, -27.52281430457070499, 5.000000000000000000 ) ) ;
#61014 = ADVANCED_FACE ( 'NONE', ( #113771 ), #102908, .F. ) ;
#61015 = DIRECTION ( 'NONE',  ( 0.7071067811865487940, 0.7071067811865463515, -0.000000000000000000 ) ) ;
#61016 = LINE ( 'NONE', #71145, #134785 ) ;
#61017 = VERTEX_POINT ( 'NONE', #70321 ) ;
#61018 = LINE ( 'NONE', #103722, #53633 ) ;
#61019 = VECTOR ( 'NONE', #82298, 1000.000000000000000 ) ;
#61020 = CARTESIAN_POINT ( 'NONE',  ( -16.45742106731621845, 0.9613713492673547911, -33.49048331797055766 ) ) ;
#61021 = EDGE_LOOP ( 'NONE', ( #110745, #94558, #101266, #19432, #94093 ) ) ;
#61022 = ADVANCED_FACE ( 'NONE', ( #47847 ), #4221, .F. ) ;
#61024 = ORIENTED_EDGE ( 'NONE', *, *, #30675, .T. ) ;
#61023 = DIRECTION ( 'NONE',  ( -0.000000000000000000, 0.3543493200069153248, 0.9351131265310292928 ) ) ;
#61026 = VERTEX_POINT ( 'NONE', #2855 ) ;
#61025 = EDGE_CURVE ( 'NONE', #32778, #91632, #37662, .T. ) ;
#61027 = VECTOR ( 'NONE', #32337, 1000.000000000000227 ) ;
#61028 = CARTESIAN_POINT ( 'NONE',  ( -16.86802775199585014, 5.611381925338908339, -29.11273303788685141 ) ) ;
#61029 = CARTESIAN_POINT ( 'NONE',  ( -45.18398860626900415, 28.73617430169818832, 5.000000000000000000 ) ) ;
#61030 = ORIENTED_EDGE ( 'NONE', *, *, #92127, .F. ) ;
#61031 = DIRECTION ( 'NONE',  ( 0.7071067811865487940, 0.7071067811865463515, -0.000000000000000000 ) ) ;
#61032 = CARTESIAN_POINT ( 'NONE',  ( 12.79289321881336683, 15.75929247661555976, 5.000000000000000000 ) ) ;
#61033 = CARTESIAN_POINT ( 'NONE',  ( 19.73159235450332005, 9.902892378096218942E-16, 0.000000000000000000 ) ) ;
#61034 = ORIENTED_EDGE ( 'NONE', *, *, #117774, .F. ) ;
#61035 = EDGE_CURVE ( 'NONE', #112837, #71117, #21194, .T. ) ;
#61036 = DIRECTION ( 'NONE',  ( 1.000000000000000000, 0.000000000000000000, 0.000000000000000000 ) ) ;
#61037 = CARTESIAN_POINT ( 'NONE',  ( -51.29974487139158867, -27.71228299555242103, 4.000000000000000000 ) ) ;
#61038 = DIRECTION ( 'NONE',  ( -0.7071067811865486830, -0.7071067811865464625, 0.000000000000000000 ) ) ;
#61039 = CARTESIAN_POINT ( 'NONE',  ( 24.81349135397623584, -15.74070752338412049, 8.904080028138885439 ) ) ;
#61040 = PLANE ( 'NONE',  #44822 ) ;
#61041 = AXIS2_PLACEMENT_3D ( 'NONE', #78279, #31908, #110157 ) ;
#61042 = LINE ( 'NONE', #116788, #21241 ) ;
#61043 = DIRECTION ( 'NONE',  ( -0.000000000000000000, 0.3543493200069153248, 0.9351131265310292928 ) ) ;
#61044 = CYLINDRICAL_SURFACE ( 'NONE', #39655, 2.500000000000000444 ) ;
#61045 = CARTESIAN_POINT ( 'NONE',  ( 19.93618820137057668, -0.2700000000508058218, -36.99999999997771738 ) ) ;
#61046 = ORIENTED_EDGE ( 'NONE', *, *, #65246, .T. ) ;
#61047 = ADVANCED_FACE ( 'NONE', ( #114469 ), #57286, .F. ) ;
#61048 = VECTOR ( 'NONE', #137060, 1000.000000000000227 ) ;
#61049 = ORIENTED_EDGE ( 'NONE', *, *, #20378, .F. ) ;
#61050 = ORIENTED_EDGE ( 'NONE', *, *, #1862, .T. ) ;
#61051 = CARTESIAN_POINT ( 'NONE',  ( 111.6875000000000000, -5.819803920172573086, 5.819803920172572198 ) ) ;
#61052 = VERTEX_POINT ( 'NONE', #92717 ) ;
#61053 = VERTEX_POINT ( 'NONE', #136952 ) ;
#61054 = ORIENTED_EDGE ( 'NONE', *, *, #37186, .T. ) ;
#61055 = VECTOR ( 'NONE', #140729, 999.9999999999998863 ) ;
#61056 = LINE ( 'NONE', #117490, #91913 ) ;
#61057 = LINE ( 'NONE', #113798, #26884 ) ;
#61058 = CARTESIAN_POINT ( 'NONE',  ( -34.92500000000001137, 22.22500000000000142, 4.000000000000000000 ) ) ;
#61059 = ADVANCED_FACE ( 'NONE', ( #46422 ), #27450, .F. ) ;
#61060 = VERTEX_POINT ( 'NONE', #47155 ) ;
#61061 = FACE_OUTER_BOUND ( 'NONE', #103427, .T. ) ;
#61062 = FACE_OUTER_BOUND ( 'NONE', #7039, .T. ) ;
#61063 = FACE_OUTER_BOUND ( 'NONE', #32872, .T. ) ;
#61064 = CARTESIAN_POINT ( 'NONE',  ( -13.17183060077638324, 6.759292476615645917, 4.000000000000000000 ) ) ;
#61065 = CARTESIAN_POINT ( 'NONE',  ( 110.1045968585647756, 1.637169565754164946, -6.109999999999999432 ) ) ;
#61066 = ORIENTED_EDGE ( 'NONE', *, *, #102888, .T. ) ;
#61067 = CARTESIAN_POINT ( 'NONE',  ( -30.41161490594810246, 22.22500000000000497, 4.777194822843814137 ) ) ;
#61068 = DIRECTION ( 'NONE',  ( -0.000000000000000000, 0.3543493200069152138, -0.9351131265310292928 ) ) ;
#61069 = DIRECTION ( 'NONE',  ( 0.7071067811865487940, 0.7071067811865463515, 0.000000000000000000 ) ) ;
#61070 = VECTOR ( 'NONE', #25961, 999.9999999999998863 ) ;
#61071 = DIRECTION ( 'NONE',  ( 0.6830127018922180770, -0.6830127018922204085, -0.2588190451025213501 ) ) ;
#61072 = CARTESIAN_POINT ( 'NONE',  ( 3.792893218813431222, -5.240707523384228850, 5.000000000000000000 ) ) ;
#61073 = CARTESIAN_POINT ( 'NONE',  ( 33.32919371712955581, -3.975000000000001865, 6.884901960086284411 ) ) ;
#61074 = LINE ( 'NONE', #113969, #28244 ) ;
#61076 = LINE ( 'NONE', #105234, #118014 ) ;
#61075 = AXIS2_PLACEMENT_3D ( 'NONE', #127495, #28903, #73142 ) ;
#61077 = ORIENTED_EDGE ( 'NONE', *, *, #79714, .T. ) ;
#61078 = ORIENTED_EDGE ( 'NONE', *, *, #132909, .F. ) ;
#61079 = CARTESIAN_POINT ( 'NONE',  ( 32.20833333333332149, -3.974999999999999201, -6.884901960086287964 ) ) ;
#61080 = ORIENTED_EDGE ( 'NONE', *, *, #57618, .T. ) ;
#61081 = CARTESIAN_POINT ( 'NONE',  ( 48.48921356237309510, -27.52281430457089328, 5.000000000000000000 ) ) ;
#61082 = EDGE_CURVE ( 'NONE', #32915, #48791, #134847, .T. ) ;
#61083 = LINE ( 'NONE', #105242, #13136 ) ;
#61084 = ORIENTED_EDGE ( 'NONE', *, *, #104030, .T. ) ;
#61085 = LINE ( 'NONE', #83514, #13202 ) ;
#61086 = AXIS2_PLACEMENT_3D ( 'NONE', #128001, #28685, #72928 ) ;
#61087 = EDGE_CURVE ( 'NONE', #93683, #35648, #105028, .T. ) ;
#61088 = ADVANCED_FACE ( 'NONE', ( #115878 ), #52773, .F. ) ;
#61089 = DIRECTION ( 'NONE',  ( 0.7071067811865487940, 0.7071067811865463515, 0.000000000000000000 ) ) ;
#61090 = LINE ( 'NONE', #16814, #104346 ) ;
#61091 = CARTESIAN_POINT ( 'NONE',  ( 31.20876352523144348, -7.482591942790329030E-16, 6.110000000000001208 ) ) ;
#61092 = VECTOR ( 'NONE', #111198, 1000.000000000000000 ) ;
#61093 = ORIENTED_EDGE ( 'NONE', *, *, #112417, .F. ) ;
#61094 = B_SPLINE_CURVE_WITH_KNOTS ( 'NONE', 3,
 ( #106293, #107041, #95451, #129496, #19328, #63586, #8403, #49844, #126640, #28066, #27328, #71577 ),
 .UNSPECIFIED., .F., .F.,
 ( 4, 2, 2, 2, 2, 4 ),
 ( 4.076487489278275292E-20, 0.0002600071698628363950, 0.0005200143397256725732, 0.001040028679451345146, 0.001560043019177017503, 0.002080057358902690293 ),
 .UNSPECIFIED. ) ;
#61095 = CARTESIAN_POINT ( 'NONE',  ( -57.18398860626899705, 28.73617430169827358, 5.000000000000000000 ) ) ;
#61096 = ORIENTED_EDGE ( 'NONE', *, *, #35226, .F. ) ;
#61097 = DIRECTION ( 'NONE',  ( -0.7071067811865486830, -0.7071067811865464625, 0.000000000000000000 ) ) ;
#61098 = ADVANCED_FACE ( 'NONE', ( #118009 ), #117313, .F. ) ;
#61099 = CARTESIAN_POINT ( 'NONE',  ( 5.292893218813421896, 8.259292476615636147, 5.000000000000000000 ) ) ;
#61100 = DIRECTION ( 'NONE',  ( 0.000000000000000000, 0.000000000000000000, 1.000000000000000000 ) ) ;
#61101 = AXIS2_PLACEMENT_3D ( 'NONE', #127099, #105350, #84359 ) ;
#61102 = CARTESIAN_POINT ( 'NONE',  ( 0.000000000000000000, 1.142820323027524232, 0.000000000000000000 ) ) ;
#61103 = VERTEX_POINT ( 'NONE', #29597 ) ;
#61105 = ADVANCED_FACE ( 'NONE', ( #96967 ), #116624, .F. ) ;
#61104 = CARTESIAN_POINT ( 'NONE',  ( 51.91709685856476852, 3.054999999999998828, 5.291415217122922066 ) ) ;
#61106 = ORIENTED_EDGE ( 'NONE', *, *, #34237, .F. ) ;
#61107 = DIRECTION ( 'NONE',  ( 0.7071067811865487940, 0.7071067811865463515, 0.000000000000000000 ) ) ;
#61108 = ADVANCED_FACE ( 'NONE', ( #141218 ), #74567, .F. ) ;
#61109 = CARTESIAN_POINT ( 'NONE',  ( -13.49999999999990230, 16.77039438581778086, 0.4657186855308035334 ) ) ;
#61110 = CARTESIAN_POINT ( 'NONE',  ( -38.99451991528749062, 28.92564299267965211, 4.000000000000000000 ) ) ;
#61111 = PLANE ( 'NONE',  #30048 ) ;
#61112 = VECTOR ( 'NONE', #134563, 1000.000000000000227 ) ;
#61113 = ADVANCED_FACE ( 'NONE', ( #16578 ), #41935, .T. ) ;
#61114 = CIRCLE ( 'NONE', #70416, 2.500000000000000888 ) ;
#61115 = EDGE_CURVE ( 'NONE', #38602, #78104, #39066, .T. ) ;
#61116 = CARTESIAN_POINT ( 'NONE',  ( 45.99543019189810877, 5.291415217122916737, 3.055000000000001936 ) ) ;
#61117 = ORIENTED_EDGE ( 'NONE', *, *, #30334, .T. ) ;
#61118 = CARTESIAN_POINT ( 'NONE',  ( -6.792893218813405909, -14.24070752338413826, 5.000000000000000000 ) ) ;
#61119 = DIRECTION ( 'NONE',  ( 0.7071067811865487940, -0.7071067811865463515, 0.000000000000000000 ) ) ;
#61120 = ORIENTED_EDGE ( 'NONE', *, *, #126376, .F. ) ;
#61121 = VERTEX_POINT ( 'NONE', #86147 ) ;
#61122 = VECTOR ( 'NONE', #126613, 1000.000000000000000 ) ;
#61123 = LINE ( 'NONE', #92972, #56249 ) ;
#61124 = EDGE_CURVE ( 'NONE', #104583, #137915, #85983, .T. ) ;
#61125 = ORIENTED_EDGE ( 'NONE', *, *, #34479, .T. ) ;
#61126 = CARTESIAN_POINT ( 'NONE',  ( -31.71896644758168904, 22.22500000000000142, 3.785114039161020738 ) ) ;
#61127 = ORIENTED_EDGE ( 'NONE', *, *, #133868, .T. ) ;
#61129 = ADVANCED_FACE ( 'NONE', ( #61568 ), #139840, .F. ) ;
#61128 = VECTOR ( 'NONE', #133708, 1000.000000000000000 ) ;
#61130 = CARTESIAN_POINT ( 'NONE',  ( 9.119999999999999218, 1.116877880822386018E-15, -10.00000000000000000 ) ) ;
#61131 = FACE_BOUND ( 'NONE', #73208, .T. ) ;
#61132 = DIRECTION ( 'NONE',  ( 0.000000000000000000, 1.000000000000000000, 0.000000000000000000 ) ) ;
#61133 = DIRECTION ( 'NONE',  ( 3.115803279706882722E-16, -1.000000000000000000, 0.000000000000000000 ) ) ;
#61134 = ORIENTED_EDGE ( 'NONE', *, *, #62035, .F. ) ;
#61135 = CIRCLE ( 'NONE', #5154, 0.5000000000000004441 ) ;
#61136 = DIRECTION ( 'NONE',  ( 0.7071067811865486830, -0.7071067811865464625, -0.000000000000000000 ) ) ;
#61138 = ORIENTED_EDGE ( 'NONE', *, *, #9409, .T. ) ;
#61137 = DIRECTION ( 'NONE',  ( -0.7071067811865486830, -0.7071067811865464625, -0.000000000000000000 ) ) ;
#61139 = VERTEX_POINT ( 'NONE', #28908 ) ;
#61140 = CARTESIAN_POINT ( 'NONE',  ( 19.49999999999987210, -11.56887692260768929, 4.000000000000000000 ) ) ;
#61141 = ORIENTED_EDGE ( 'NONE', *, *, #40147, .F. ) ;
#61142 = EDGE_CURVE ( 'NONE', #127177, #62908, #130373, .T. ) ;
#61143 = ORIENTED_EDGE ( 'NONE', *, *, #15645, .T. ) ;
#61144 = CARTESIAN_POINT ( 'NONE',  ( 66.99543019189812298, 5.291415217122916737, 3.055000000000001936 ) ) ;
#61146 = ORIENTED_EDGE ( 'NONE', *, *, #34376, .T. ) ;
#61145 = VECTOR ( 'NONE', #27051, 1000.000000000000000 ) ;
#61147 = CARTESIAN_POINT ( 'NONE',  ( 1.785015802758090020, -3.740707523384244837, 15.76143240460124773 ) ) ;
#61148 = LINE ( 'NONE', #106698, #88950 ) ;
#61149 = ORIENTED_EDGE ( 'NONE', *, *, #20518, .F. ) ;
#61150 = CARTESIAN_POINT ( 'NONE',  ( 22.49999999999984723, -7.420205493532876950, -2.617629953481201088 ) ) ;
#61151 = EDGE_CURVE ( 'NONE', #49472, #116795, #127502, .T. ) ;
#61152 = VECTOR ( 'NONE', #95474, 1000.000000000000000 ) ;
#61153 = CARTESIAN_POINT ( 'NONE',  ( 7.499999999999951150, -11.56887692260769107, 4.000000000000000000 ) ) ;
#61154 = DIRECTION ( 'NONE',  ( 0.7071067811865487940, 0.7071067811865463515, 0.000000000000000000 ) ) ;
#61155 = FACE_OUTER_BOUND ( 'NONE', #131350, .T. ) ;
#61156 = CARTESIAN_POINT ( 'NONE',  ( -36.48921356237310221, -27.52281430457080802, 5.000000000000000000 ) ) ;
#61157 = DIRECTION ( 'NONE',  ( -0.6830127018922180770, -0.6830127018922204085, -0.2588190451025213501 ) ) ;
#61158 = VERTEX_POINT ( 'NONE', #73148 ) ;
#61159 = ORIENTED_EDGE ( 'NONE', *, *, #97640, .F. ) ;
#61160 = CARTESIAN_POINT ( 'NONE',  ( 9.962472949537104938, -7.464222240803106570E-16, -6.094999999999989981 ) ) ;
#61161 = CARTESIAN_POINT ( 'NONE',  ( 12.29974487139158512, -27.71228299555214747, 4.000000000000000000 ) ) ;
#61162 = ORIENTED_EDGE ( 'NONE', *, *, #110888, .F. ) ;
#61163 = ORIENTED_EDGE ( 'NONE', *, *, #75441, .F. ) ;
#61164 = ORIENTED_EDGE ( 'NONE', *, *, #108429, .F. ) ;
#61165 = LINE ( 'NONE', #50243, #102247 ) ;
#61166 = CARTESIAN_POINT ( 'NONE',  ( -34.92500000000001137, 4.512461875839451686, 4.000000000000000000 ) ) ;
#61167 = ORIENTED_EDGE ( 'NONE', *, *, #65826, .T. ) ;
#61168 = CARTESIAN_POINT ( 'NONE',  ( 32.99999999999977263, 4.552185695429122880, 5.000000000000000000 ) ) ;
#61169 = VECTOR ( 'NONE', #108300, 1000.000000000000000 ) ;
#61170 = CARTESIAN_POINT ( 'NONE',  ( -36.18398860626899705, 28.73617430169812437, 5.000000000000000000 ) ) ;
#61171 = AXIS2_PLACEMENT_3D ( 'NONE', #68689, #46972, #125189 ) ;
#61172 = CARTESIAN_POINT ( 'NONE',  ( 12.31706980810188412, -2.126176841940956130, 7.934999999999991616 ) ) ;
#61173 = DIRECTION ( 'NONE',  ( 0.7071067811865487940, 0.7071067811865463515, 0.000000000000000000 ) ) ;
#61174 = ORIENTED_EDGE ( 'NONE', *, *, #103674, .F. ) ;
#61176 = EDGE_CURVE ( 'NONE', #137275, #33570, #56997, .T. ) ;
#61175 = LINE ( 'NONE', #74141, #102220 ) ;
#61177 = LINE ( 'NONE', #69900, #37985 ) ;
#61179 = ORIENTED_EDGE ( 'NONE', *, *, #121238, .F. ) ;
#61178 = CARTESIAN_POINT ( 'NONE',  ( 37.04515773336643036, -21.74070752338406365, 21.72585301388593138 ) ) ;
#61180 = FACE_OUTER_BOUND ( 'NONE', #129884, .T. ) ;
#61181 = ORIENTED_EDGE ( 'NONE', *, *, #59209, .T. ) ;
#61182 = DIRECTION ( 'NONE',  ( 0.000000000000000000, -1.000000000000000000, 0.000000000000000000 ) ) ;
#61183 = FACE_OUTER_BOUND ( 'NONE', #36046, .T. ) ;
#61184 = AXIS2_PLACEMENT_3D ( 'NONE', #123559, #114756, #18292 ) ;
#61185 = CARTESIAN_POINT ( 'NONE',  ( 109.2083333333333428, -3.974999999999999201, -6.884901960086287964 ) ) ;
#61186 = ORIENTED_EDGE ( 'NONE', *, *, #113742, .T. ) ;
#61187 = VECTOR ( 'NONE', #112487, 999.9999999999998863 ) ;
#61188 = DIRECTION ( 'NONE',  ( -0.3543493200069162685, -0.000000000000000000, -0.9351131265310288487 ) ) ;
#61189 = LINE ( 'NONE', #59731, #92763 ) ;
#61190 = FACE_OUTER_BOUND ( 'NONE', #68344, .T. ) ;
#61191 = VERTEX_POINT ( 'NONE', #138380 ) ;
#61192 = PLANE ( 'NONE',  #113369 ) ;
#61193 = CARTESIAN_POINT ( 'NONE',  ( 13.49999999999990763, 9.431123077392092213, 4.000000000000000000 ) ) ;
#61195 = VECTOR ( 'NONE', #102363, 1000.000000000000114 ) ;
#61194 = CARTESIAN_POINT ( 'NONE',  ( -34.92500000000001137, -22.22500000000000142, 4.000000000000000000 ) ) ;
#61196 = ADVANCED_FACE ( 'NONE', ( #17984 ), #50653, .F. ) ;
#61197 = FACE_OUTER_BOUND ( 'NONE', #36389, .T. ) ;
#61198 =( NAMED_UNIT ( * ) PLANE_ANGLE_UNIT ( ) SI_UNIT ( $, .RADIAN. ) );
#61199 = EDGE_CURVE ( 'NONE', #90720, #9222, #40510, .T. ) ;
#61200 = VERTEX_POINT ( 'NONE', #73835 ) ;
#61201 = ORIENTED_EDGE ( 'NONE', *, *, #24635, .F. ) ;
#61202 = CARTESIAN_POINT ( 'NONE',  ( 58.75000000000000000, -9.735942053221458872E-16, 7.950000000000000178 ) ) ;
#61203 = CARTESIAN_POINT ( 'NONE',  ( -6.489213562373093325, -27.52281430457059841, 5.000000000000000000 ) ) ;
#61205 = EDGE_CURVE ( 'NONE', #83008, #33185, #99868, .T. ) ;
#61204 = VECTOR ( 'NONE', #124920, 1000.000000000000000 ) ;
#61206 = EDGE_CURVE ( 'NONE', #35333, #6025, #75284, .T. ) ;
#61207 = CARTESIAN_POINT ( 'NONE',  ( 6.103736474768552078, 5.808823158059036373, 5.808823158059032821 ) ) ;
#61208 = DIRECTION ( 'NONE',  ( 0.6830127018922180770, -0.6830127018922204085, -0.2588190451025213501 ) ) ;
#61209 = VECTOR ( 'NONE', #99610, 1000.000000000000000 ) ;
#61210 = DIRECTION ( 'NONE',  ( -0.7071067811865487940, 0.7071067811865463515, 0.000000000000000000 ) ) ;
#61211 = CARTESIAN_POINT ( 'NONE',  ( -8.293876922607989144, 22.22500000000000142, 4.000000000000000000 ) ) ;
#61212 = LINE ( 'NONE', #48147, #60731 ) ;
#61213 = VERTEX_POINT ( 'NONE', #54958 ) ;
#61214 = EDGE_CURVE ( 'NONE', #99583, #85580, #99122, .T. ) ;
#61215 = PLANE ( 'NONE',  #67382 ) ;
#61216 = CARTESIAN_POINT ( 'NONE',  ( -4.000000000000000000, 8.616843969807042924, -4.898587196589412829E-16 ) ) ;
#61217 = DIRECTION ( 'NONE',  ( -0.6830127018922181881, 0.6830127018922202975, -0.2588190451025214056 ) ) ;
#61218 = DIRECTION ( 'NONE',  ( 0.6830127018922180770, -0.6830127018922204085, -0.2588190451025213501 ) ) ;
#61219 = CARTESIAN_POINT ( 'NONE',  ( 48.32876352523145158, 0.000000000000000000, -6.109999999999999432 ) ) ;
#61220 = CARTESIAN_POINT ( 'NONE',  ( 184.0791405606630917, -51.15040958483975686, -36.98623100868703517 ) ) ;
#61221 = EDGE_CURVE ( 'NONE', #128013, #39184, #92912, .T. ) ;
#61222 = AXIS2_PLACEMENT_3D ( 'NONE', #51835, #32956, #96705 ) ;
#61223 = ORIENTED_EDGE ( 'NONE', *, *, #30777, .T. ) ;
#61224 = DIRECTION ( 'NONE',  ( -0.6830127018922180770, -0.6830127018922204085, -0.2588190451025213501 ) ) ;
#61225 = VERTEX_POINT ( 'NONE', #76722 ) ;
#61226 = ORIENTED_EDGE ( 'NONE', *, *, #70464, .T. ) ;
#61227 = VECTOR ( 'NONE', #117269, 999.9999999999998863 ) ;
#61228 = CARTESIAN_POINT ( 'NONE',  ( -17.01844734635659506, 18.75929247661552424, 20.33588619593446722 ) ) ;
#61229 = EDGE_CURVE ( 'NONE', #21649, #3243, #142665, .T. ) ;
#61230 = FACE_OUTER_BOUND ( 'NONE', #32725, .T. ) ;
#61231 = FACE_OUTER_BOUND ( 'NONE', #69379, .T. ) ;
#61232 = DIRECTION ( 'NONE',  ( 0.7071067811865487940, 0.7071067811865463515, 0.000000000000000000 ) ) ;
#61233 = CARTESIAN_POINT ( 'NONE',  ( -11.20710678118646797, 9.759292476615620160, 5.000000000000000000 ) ) ;
#61234 = PLANE ( 'NONE',  #112557 ) ;
#61235 = EDGE_LOOP ( 'NONE', ( #48188, #48787, #34467, #14264 ) ) ;
#61236 = CARTESIAN_POINT ( 'NONE',  ( 5.999999999999970690, -0.4125381241607533611, 4.000000000000000000 ) ) ;
#61237 = CARTESIAN_POINT ( 'NONE',  ( 0.000000000000000000, -60.26999999999998892, -40.00000000000000000 ) ) ;
#61238 = EDGE_CURVE ( 'NONE', #128126, #71447, #121604, .T. ) ;
#61239 = DIRECTION ( 'NONE',  ( -0.7071067811865486830, 0.7071067811865464625, 0.000000000000000000 ) ) ;
#61240 = DIRECTION ( 'NONE',  ( 0.7071067811865487940, -0.7071067811865463515, 0.000000000000000000 ) ) ;
#61241 = CARTESIAN_POINT ( 'NONE',  ( 1.499999999999992673, 15.05218569542901186, 5.000000000000000000 ) ) ;
#61242 = CARTESIAN_POINT ( 'NONE',  ( 62.35002705046287730, -5.819803920172572198, -5.819803920172572198 ) ) ;
#61243 = DIRECTION ( 'NONE',  ( -0.7071067811865486830, 0.7071067811865464625, 0.000000000000000000 ) ) ;
#61244 = VERTEX_POINT ( 'NONE', #89019 ) ;
#61245 = ORIENTED_EDGE ( 'NONE', *, *, #32180, .T. ) ;
#61246 = CARTESIAN_POINT ( 'NONE',  ( 64.87499999999998579, 7.950000000000000178, 1.460391307983218535E-15 ) ) ;
#61247 = LINE ( 'NONE', #119130, #104925 ) ;
#61248 = CARTESIAN_POINT ( 'NONE',  ( -3.005480084712505828, 28.92564299267936079, 4.000000000000000000 ) ) ;
#61249 = EDGE_CURVE ( 'NONE', #62473, #110860, #54262, .T. ) ;
#61250 = VERTEX_POINT ( 'NONE', #120896 ) ;
#61251 = AXIS2_PLACEMENT_3D ( 'NONE', #42923, #132804, #87122 ) ;
#61253 = EDGE_CURVE ( 'NONE', #138628, #54912, #33915, .T. ) ;
#61252 = DIRECTION ( 'NONE',  ( 0.7071067811865486830, -0.7071067811865464625, -0.000000000000000000 ) ) ;
#61254 = ADVANCED_FACE ( 'NONE', ( #77440 ), #21601, .F. ) ;
#61255 = DIRECTION ( 'NONE',  ( -1.000000000000000000, -0.000000000000000000, -0.000000000000000000 ) ) ;
#61256 = CARTESIAN_POINT ( 'NONE',  ( 52.50043019189811133, -3.055000000000002380, 5.291415217122920289 ) ) ;
#61257 = EDGE_CURVE ( 'NONE', #45818, #130351, #132543, .T. ) ;
#61258 = CARTESIAN_POINT ( 'NONE',  ( 34.47516574401890921, -10.50948238788426536, 4.998110765256835286 ) ) ;
#61259 = VERTEX_POINT ( 'NONE', #122307 ) ;
#61260 = VERTEX_POINT ( 'NONE', #44829 ) ;
#61261 = LINE ( 'NONE', #95962, #111747 ) ;
#61262 = ADVANCED_FACE ( 'NONE', ( #66540 ), #133238, .F. ) ;
#61263 = LINE ( 'NONE', #126445, #3661 ) ;
#61264 = PLANE ( 'NONE',  #55873 ) ;
#61265 = CARTESIAN_POINT ( 'NONE',  ( 21.46453280170069888, -2.055000000000000160, 0.000000000000000000 ) ) ;
#61266 = EDGE_CURVE ( 'NONE', #132586, #142104, #86865, .T. ) ;
#61267 = CARTESIAN_POINT ( 'NONE',  ( 29.99999999999979750, -13.44781430457068794, 5.000000000000000000 ) ) ;
#61269 = ORIENTED_EDGE ( 'NONE', *, *, #84598, .T. ) ;
#61268 = CARTESIAN_POINT ( 'NONE',  ( 99.53752705046289861, -9.735942053221456900E-16, 7.949999999999998401 ) ) ;
#61270 = LINE ( 'NONE', #15523, #6665 ) ;
#61271 = DIRECTION ( 'NONE',  ( -1.000000000000000000, -0.000000000000000000, -0.000000000000000000 ) ) ;
#61272 = DIRECTION ( 'NONE',  ( -0.000000000000000000, 0.3543493200069153248, 0.9351131265310292928 ) ) ;
#61273 = AXIS2_PLACEMENT_3D ( 'NONE', #142940, #68283, #111750 ) ;
#61274 = DIRECTION ( 'NONE',  ( 0.6830127018922180770, -0.6830127018922204085, -0.2588190451025213501 ) ) ;
#61275 = VERTEX_POINT ( 'NONE', #141974 ) ;
#61276 = VECTOR ( 'NONE', #66728, 1000.000000000000000 ) ;
#61277 = EDGE_LOOP ( 'NONE', ( #5352, #94767, #109921, #76428 ) ) ;
#61278 = EDGE_CURVE ( 'NONE', #88187, #130377, #12133, .T. ) ;
#61279 = DIRECTION ( 'NONE',  ( -0.6830127018922180770, -0.6830127018922202975, -0.2588190451025213501 ) ) ;
#61280 = AXIS2_PLACEMENT_3D ( 'NONE', #56238, #101107, #87401 ) ;
#61281 = DIRECTION ( 'NONE',  ( 1.000000000000000000, 0.000000000000000000, 0.000000000000000000 ) ) ;
#61282 = CARTESIAN_POINT ( 'NONE',  ( 66.48921356237309510, -27.52281430457101763, 5.000000000000000000 ) ) ;
#61283 = CARTESIAN_POINT ( 'NONE',  ( -34.92500000000001137, 1.800094516027185065, 4.759050581649336031 ) ) ;
#61284 = VERTEX_POINT ( 'NONE', #100599 ) ;
#61285 = ORIENTED_EDGE ( 'NONE', *, *, #45562, .T. ) ;
#61286 = DIRECTION ( 'NONE',  ( -1.000000000000000000, -0.000000000000000000, -0.000000000000000000 ) ) ;
#61288 = ADVANCED_FACE ( 'NONE', ( #89704 ), #31764, .T. ) ;
#61287 = CARTESIAN_POINT ( 'NONE',  ( -19.28515664589289003, 1.196650378695324646, -30.59010235425024149 ) ) ;
#61289 = ORIENTED_EDGE ( 'NONE', *, *, #60849, .T. ) ;
#61290 = EDGE_LOOP ( 'NONE', ( #11483, #90898, #98995, #123464 ) ) ;
#61291 = VECTOR ( 'NONE', #22241, 1000.000000000000000 ) ;
#61293 = VECTOR ( 'NONE', #102430, 1000.000000000000114 ) ;
#61292 = DIRECTION ( 'NONE',  ( 0.7071067811865487940, -0.7071067811865463515, 0.000000000000000000 ) ) ;
#61294 = ORIENTED_EDGE ( 'NONE', *, *, #2035, .T. ) ;
#61295 = CARTESIAN_POINT ( 'NONE',  ( -34.92500000000001137, 22.22500000000000142, 4.000000000000000000 ) ) ;
#61296 = DIRECTION ( 'NONE',  ( -0.000000000000000000, 0.3543493200069153248, 0.9351131265310292928 ) ) ;
#61297 = FACE_BOUND ( 'NONE', #123536, .T. ) ;
#61298 = DIRECTION ( 'NONE',  ( 0.7071067811865486830, -0.7071067811865464625, -0.000000000000000000 ) ) ;
#61299 = DIRECTION ( 'NONE',  ( -0.7071067811865486830, 0.7071067811865464625, 0.000000000000000000 ) ) ;
#61301 = EDGE_LOOP ( 'NONE', ( #97845, #36493, #49323, #73226 ) ) ;
#61300 = DIRECTION ( 'NONE',  ( 0.7071067811865486830, -0.7071067811865464625, -0.000000000000000000 ) ) ;
#61302 = VECTOR ( 'NONE', #10120, 999.9999999999998863 ) ;
#61303 = PRODUCT_CONTEXT ( 'NONE', #60569, 'mechanical' ) ;
#61304 = ORIENTED_EDGE ( 'NONE', *, *, #43242, .T. ) ;
#61305 = ADVANCED_FACE ( 'NONE', ( #109316 ), #9238, .F. ) ;
#61306 = PRESENTATION_LAYER_ASSIGNMENT (  '', '', ( #137743 ) ) ;
#61308 = ORIENTED_EDGE ( 'NONE', *, *, #139821, .T. ) ;
#61307 = AXIS2_PLACEMENT_3D ( 'NONE', #77226, #3185, #102535 ) ;
#61309 = CARTESIAN_POINT ( 'NONE',  ( 93.24543019189812298, -5.291415217122918513, -3.055000000000000160 ) ) ;
#61310 = ORIENTED_EDGE ( 'NONE', *, *, #75131, .T. ) ;
#61311 = VECTOR ( 'NONE', #134003, 1000.000000000000000 ) ;
#61312 = CARTESIAN_POINT ( 'NONE',  ( 34.49999999999975842, 1.030536316426539756, -5.498701923753880116 ) ) ;
#61313 = CARTESIAN_POINT ( 'NONE',  ( 72.48921356237309510, -27.52281430457106026, 5.000000000000000000 ) ) ;
#61314 = CARTESIAN_POINT ( 'NONE',  ( -17.20710678118642889, -20.24070752338407075, 5.000000000000000000 ) ) ;
#61315 = CARTESIAN_POINT ( 'NONE',  ( -28.49999999999980815, -17.56887692260762535, 4.000000000000000000 ) ) ;
#61316 = ORIENTED_EDGE ( 'NONE', *, *, #62982, .T. ) ;
#61317 = CARTESIAN_POINT ( 'NONE',  ( 181.1500000000000057, -43.14999999999999147, -34.92499999999998295 ) ) ;
#61318 = CARTESIAN_POINT ( 'NONE',  ( 66.29974487139159578, -27.71228299555252406, 4.000000000000000000 ) ) ;
#61319 = CARTESIAN_POINT ( 'NONE',  ( -27.70710678118634718, 17.25929247661554555, 5.000000000000000000 ) ) ;
#61321 = CARTESIAN_POINT ( 'NONE',  ( 0.000000000000000000, 0.000000000000000000, 5.000000000000000000 ) ) ;
#61320 = CARTESIAN_POINT ( 'NONE',  ( -60.48921356237309510, -27.52281430457097500, 5.000000000000000000 ) ) ;
#61322 = CARTESIAN_POINT ( 'NONE',  ( 2.999999999999992450, 17.58746187583906107, 4.000000000000000000 ) ) ;
#61323 = CARTESIAN_POINT ( 'NONE',  ( -36.18398860626899705, 28.73617430169812437, 5.000000000000000000 ) ) ;
#61324 = LINE ( 'NONE', #128668, #56214 ) ;
#61325 = ORIENTED_EDGE ( 'NONE', *, *, #84598, .F. ) ;
#61326 = DIRECTION ( 'NONE',  ( -0.7071067811865486830, 0.7071067811865464625, 0.000000000000000000 ) ) ;
#61327 = PLANE ( 'NONE',  #39604 ) ;
#61328 = ORIENTED_EDGE ( 'NONE', *, *, #77386, .T. ) ;
#61329 = ORIENTED_EDGE ( 'NONE', *, *, #86200, .F. ) ;
#61330 = ORIENTED_EDGE ( 'NONE', *, *, #28178, .F. ) ;
#61331 = CARTESIAN_POINT ( 'NONE',  ( 41.27126352523144703, 4.472830434245838482, 4.472830434245842035 ) ) ;
#61332 = ORIENTED_EDGE ( 'NONE', *, *, #7669, .T. ) ;
#61333 = CARTESIAN_POINT ( 'NONE',  ( 13.31663961620377279, -1.633150327867691987, -6.094999999999989093 ) ) ;
#61334 = CARTESIAN_POINT ( 'NONE',  ( -8.807277435403058519, 10.22259551701957214, -26.82144004025722950 ) ) ;
#61335 = EDGE_LOOP ( 'NONE', ( #70786, #19222, #133502 ) ) ;
#61336 = CARTESIAN_POINT ( 'NONE',  ( 17.70025512860841488, -27.71228299555193786, 4.000000000000000000 ) ) ;
#61337 = ORIENTED_EDGE ( 'NONE', *, *, #104730, .F. ) ;
#61338 = DIRECTION ( 'NONE',  ( -0.7071067811865487940, 0.7071067811865463515, 0.000000000000000000 ) ) ;
#61339 = CARTESIAN_POINT ( 'NONE',  ( 0.000000000000000000, 0.000000000000000000, 0.000000000000000000 ) ) ;
#61341 = ORIENTED_EDGE ( 'NONE', *, *, #1344, .F. ) ;
#61340 = CARTESIAN_POINT ( 'NONE',  ( 24.70701326429286482, -21.74070752338406365, 4.999753212805220670 ) ) ;
#61342 = ORIENTED_EDGE ( 'NONE', *, *, #110263, .F. ) ;
#61343 = VECTOR ( 'NONE', #103507, 1000.000000000000227 ) ;
#61344 = DIRECTION ( 'NONE',  ( -0.7071067811865486830, -0.7071067811865464625, 0.000000000000000000 ) ) ;
#61345 = CARTESIAN_POINT ( 'NONE',  ( 20.99451991528748707, 28.92564299267952777, 4.000000000000000000 ) ) ;
#61346 = ORIENTED_EDGE ( 'NONE', *, *, #107026, .T. ) ;
#61347 = DIRECTION ( 'NONE',  ( 0.6830127018922181881, 0.6830127018922202975, -0.2588190451025214056 ) ) ;
#61348 = ORIENTED_EDGE ( 'NONE', *, *, #102947, .F. ) ;
#61349 = VERTEX_POINT ( 'NONE', #103417 ) ;
#61350 = ORIENTED_EDGE ( 'NONE', *, *, #20847, .F. ) ;
#61351 = EDGE_LOOP ( 'NONE', ( #76051, #54432, #69016, #133675 ) ) ;
#61352 = ADVANCED_FACE ( 'NONE', ( #69401 ), #80987, .F. ) ;
#61353 = DIRECTION ( 'NONE',  ( -0.7071067811865486830, -0.7071067811865464625, 0.000000000000000000 ) ) ;
#61354 = DIRECTION ( 'NONE',  ( -0.7071067811865487940, 0.7071067811865463515, 0.000000000000000000 ) ) ;
#61355 = ADVANCED_FACE ( 'NONE', ( #102014 ), #113587, .F. ) ;
#61356 = DIRECTION ( 'NONE',  ( -1.000000000000000000, -0.000000000000000000, -0.000000000000000000 ) ) ;
#61357 = CARTESIAN_POINT ( 'NONE',  ( -7.134088674951100550, -39.92999999999999261, 19.02448003456068548 ) ) ;
#61358 = ADVANCED_FACE ( 'NONE', ( #13545 ), #4782, .F. ) ;
#61360 = ORIENTED_EDGE ( 'NONE', *, *, #64493, .F. ) ;
#61359 = ADVANCED_FACE ( 'NONE', ( #25878 ), #92537, .F. ) ;
#61361 = CARTESIAN_POINT ( 'NONE',  ( 66.47916666666665719, -7.950000000000000178, 2.130196079827424427 ) ) ;
#61362 = EDGE_LOOP ( 'NONE', ( #116927, #53014, #26816, #63547 ) ) ;
#61363 = DIRECTION ( 'NONE',  ( -0.7071067811865486830, -0.7071067811865464625, 0.000000000000000000 ) ) ;
#61364 = EDGE_CURVE ( 'NONE', #62795, #103277, #70150, .T. ) ;
#61365 = EDGE_CURVE ( 'NONE', #51943, #3084, #102738, .T. ) ;
#61366 = AXIS2_PLACEMENT_3D ( 'NONE', #110727, #65877, #131814 ) ;
#61367 = CARTESIAN_POINT ( 'NONE',  ( 31.18706980810189222, -2.126176841940956130, 7.934999999999991616 ) ) ;
#61368 = CARTESIAN_POINT ( 'NONE',  ( -34.49999999999975842, -13.53574439159936915, 4.994342998332166772 ) ) ;
#61369 = DIRECTION ( 'NONE',  ( -0.6830127018922180770, -0.6830127018922204085, -0.2588190451025213501 ) ) ;
#61370 = CARTESIAN_POINT ( 'NONE',  ( 10.49999999999992539, -4.216083040037235996, -7.486842126848680223 ) ) ;
#61371 = ORIENTED_EDGE ( 'NONE', *, *, #138395, .F. ) ;
#61372 = MECHANICAL_DESIGN_GEOMETRIC_PRESENTATION_REPRESENTATION (  '', ( #21987 ), #3447 ) ;
#61373 = ORIENTED_EDGE ( 'NONE', *, *, #21080, .F. ) ;
#61374 = EDGE_CURVE ( 'NONE', #61485, #6222, #136775, .T. ) ;
#61375 = EDGE_LOOP ( 'NONE', ( #105357, #10820, #47071, #69694 ) ) ;
#61376 = CARTESIAN_POINT ( 'NONE',  ( -25.39999999999996305, 0.000000000000000000, 2.500000000000000000 ) ) ;
#61377 = CARTESIAN_POINT ( 'NONE',  ( 15.83159235450332147, 9.902892378096218942E-16, 0.000000000000000000 ) ) ;
#61378 = DIRECTION ( 'NONE',  ( 0.000000000000000000, 0.000000000000000000, -1.000000000000000000 ) ) ;
#61379 = ADVANCED_FACE ( 'NONE', ( #36747 ), #112192, .T. ) ;
#61380 = LINE ( 'NONE', #105525, #35911 ) ;
#61381 = CARTESIAN_POINT ( 'NONE',  ( 1.301042606982605163E-14, -47.62213595499957819, -36.92499999999998295 ) ) ;
#61382 = CARTESIAN_POINT ( 'NONE',  ( 78.22459685856479439, -1.637169565754161171, 6.109999999999998543 ) ) ;
#61383 = CARTESIAN_POINT ( 'NONE',  ( -33.18398860626899705, 28.73617430169810305, 5.000000000000000000 ) ) ;
#61384 = EDGE_CURVE ( 'NONE', #101064, #137064, #114988, .T. ) ;
#61385 = LINE ( 'NONE', #4030, #96917 ) ;
#61386 = CARTESIAN_POINT ( 'NONE',  ( 7.499999999999947597, 11.52377502935403619, -1.522421517564102267 ) ) ;
#61387 = DIRECTION ( 'NONE',  ( 0.7071067811865486830, -0.7071067811865464625, -0.000000000000000000 ) ) ;
#61388 = DIRECTION ( 'NONE',  ( 0.7071067811865487940, 0.7071067811865463515, 0.000000000000000000 ) ) ;
#61389 = ORIENTED_EDGE ( 'NONE', *, *, #87274, .T. ) ;
#61390 = DIRECTION ( 'NONE',  ( -0.6830127018922181881, 0.6830127018922202975, -0.2588190451025214056 ) ) ;
#61391 = EDGE_LOOP ( 'NONE', ( #36234, #88786, #28542, #60778 ) ) ;
#61392 = EDGE_CURVE ( 'NONE', #61677, #140803, #101294, .T. ) ;
#61393 = DIRECTION ( 'NONE',  ( 0.7071067811865486830, -0.7071067811865464625, -0.000000000000000000 ) ) ;
#61395 = ORIENTED_EDGE ( 'NONE', *, *, #69542, .F. ) ;
#61394 = CARTESIAN_POINT ( 'NONE',  ( -9.792893218813388145, 0.7592924766157104211, 5.000000000000000000 ) ) ;
#61396 = DIRECTION ( 'NONE',  ( -0.7071067811865486830, -0.7071067811865464625, 0.000000000000000000 ) ) ;
#61397 = DIRECTION ( 'NONE',  ( -0.6830127018922181881, 0.6830127018922202975, -0.2588190451025214056 ) ) ;
#61398 = VERTEX_POINT ( 'NONE', #93275 ) ;
#61399 = ORIENTED_EDGE ( 'NONE', *, *, #125814, .T. ) ;
#61400 = CARTESIAN_POINT ( 'NONE',  ( 12.79289321881337216, 6.759292476615651246, 5.000000000000000000 ) ) ;
#61401 = EDGE_CURVE ( 'NONE', #10796, #37388, #35362, .T. ) ;
#61402 = CARTESIAN_POINT ( 'NONE',  ( 5.287690060339683029, -21.73547319004781642, 4.999917730833664642 ) ) ;
#61403 = VECTOR ( 'NONE', #87412, 1000.000000000000000 ) ;
#61404 = CARTESIAN_POINT ( 'NONE',  ( 95.60002705046287019, 5.819803920172570422, 5.819803920172574863 ) ) ;
#61406 = VECTOR ( 'NONE', #28508, 1000.000000000000000 ) ;
#61405 = CARTESIAN_POINT ( 'NONE',  ( 6.489213562373093325, -27.52281430457059841, 5.000000000000000000 ) ) ;
#61407 = CONICAL_SURFACE ( 'NONE', #130821, 2.500000000000000888, 0.9599310885968822538 ) ;
#61408 = DIRECTION ( 'NONE',  ( 0.7071067811865487940, 0.7071067811865463515, 0.000000000000000000 ) ) ;
#61409 = ORIENTED_EDGE ( 'NONE', *, *, #14611, .T. ) ;
#61410 = AXIS2_PLACEMENT_3D ( 'NONE', #101524, #46497, #132776 ) ;
#61411 = DIRECTION ( 'NONE',  ( -1.000000000000000000, -0.000000000000000000, -0.000000000000000000 ) ) ;
#61412 = FACE_OUTER_BOUND ( 'NONE', #113803, .T. ) ;
#61413 = CARTESIAN_POINT ( 'NONE',  ( 22.60416666666666430, -1.633150327867691987, -6.094999999999989093 ) ) ;
#61414 = ADVANCED_FACE ( 'NONE', ( #134667 ), #123790, .F. ) ;
#61415 = LINE ( 'NONE', #14986, #134794 ) ;
#61416 = DIRECTION ( 'NONE',  ( -0.7071067811865486830, 0.7071067811865464625, 0.000000000000000000 ) ) ;
#61417 = VERTEX_POINT ( 'NONE', #39642 ) ;
#61418 = CARTESIAN_POINT ( 'NONE',  ( 46.60002705046288440, 5.819803920172570422, 5.819803920172575751 ) ) ;
#61419 = EDGE_CURVE ( 'NONE', #87121, #31173, #72697, .T. ) ;
#61420 = ORIENTED_EDGE ( 'NONE', *, *, #35279, .T. ) ;
#61421 = CARTESIAN_POINT ( 'NONE',  ( 86.62543019189811844, 5.291415217122919401, 3.055000000000002824 ) ) ;
#61422 = EDGE_CURVE ( 'NONE', #22237, #126442, #116459, .T. ) ;
#61423 = CARTESIAN_POINT ( 'NONE',  ( -51.29974487139158867, -27.71228299555242103, 4.000000000000000000 ) ) ;
#61424 = LINE ( 'NONE', #82421, #121006 ) ;
#61425 = FACE_OUTER_BOUND ( 'NONE', #104772, .T. ) ;
#61426 = VERTEX_POINT ( 'NONE', #93981 ) ;
#61427 = FACE_OUTER_BOUND ( 'NONE', #115657, .T. ) ;
#61428 = EDGE_CURVE ( 'NONE', #12779, #25917, #83868, .T. ) ;
#61429 = DIRECTION ( 'NONE',  ( -1.000000000000000000, 0.000000000000000000, 0.000000000000000000 ) ) ;
#61430 = LINE ( 'NONE', #105570, #138874 ) ;
#61432 = EDGE_LOOP ( 'NONE', ( #49165, #79385, #28950, #78584 ) ) ;
#61431 = LINE ( 'NONE', #52632, #33617 ) ;
#61433 = CARTESIAN_POINT ( 'NONE',  ( 14.00000000000000178, 0.000000000000000000, 6.094999999999989981 ) ) ;
#61434 = CARTESIAN_POINT ( 'NONE',  ( -19.00193056682084247, -22.22500000000000142, 4.500000000000000888 ) ) ;
#61435 = CARTESIAN_POINT ( 'NONE',  ( 1.547775330865844623, -2.540876819987784252, 6.037041738182785444 ) ) ;
#61436 = EDGE_CURVE ( 'NONE', #7238, #55692, #106998, .T. ) ;
#61437 = CARTESIAN_POINT ( 'NONE',  ( -34.49999999999976552, 19.39370406404964342, 1.459788787078281080 ) ) ;
#61438 = EDGE_LOOP ( 'NONE', ( #23400, #11496, #9493, #141199 ) ) ;
#61439 = VERTEX_POINT ( 'NONE', #7678 ) ;
#61440 = CARTESIAN_POINT ( 'NONE',  ( 74.52126352523141861, -4.472830434245839371, -4.472830434245840259 ) ) ;
#61441 = VERTEX_POINT ( 'NONE', #21247 ) ;
#61442 = ADVANCED_FACE ( 'NONE', ( #128758 ), #17150, .F. ) ;
#61443 = LINE ( 'NONE', #81758, #103129 ) ;
#61444 = CARTESIAN_POINT ( 'NONE',  ( -34.49999999999976552, 1.464255608400471642, 4.994342998332163219 ) ) ;
#61445 = LINE ( 'NONE', #105587, #43443 ) ;
#61446 = ORIENTED_EDGE ( 'NONE', *, *, #12704, .T. ) ;
#61447 = DIRECTION ( 'NONE',  ( -0.000000000000000000, 0.000000000000000000, 1.000000000000000000 ) ) ;
#61448 = DIRECTION ( 'NONE',  ( 1.000000000000000000, 1.224606353822377258E-16, 0.000000000000000000 ) ) ;
#61449 = EDGE_LOOP ( 'NONE', ( #76658, #51285, #75530, #98444 ) ) ;
#61450 = EDGE_CURVE ( 'NONE', #31939, #142484, #50496, .T. ) ;
#61451 = CARTESIAN_POINT ( 'NONE',  ( -11.99999999999992362, 2.342191155542436842, -5.001666872980057299 ) ) ;
#61452 = CARTESIAN_POINT ( 'NONE',  ( 27.79289321881327268, -20.24070752338406720, 5.000000000000000000 ) ) ;
#61453 = LINE ( 'NONE', #95454, #118699 ) ;
#61454 = ORIENTED_EDGE ( 'NONE', *, *, #293, .T. ) ;
#61455 = EDGE_LOOP ( 'NONE', ( #138813, #99169, #26341, #106038 ) ) ;
#61456 = EDGE_CURVE ( 'NONE', #133319, #54084, #6221, .T. ) ;
#61457 = DIRECTION ( 'NONE',  ( -0.000000000000000000, -0.3543493200069152693, 0.9351131265310292928 ) ) ;
#61458 = LINE ( 'NONE', #18588, #34627 ) ;
#61459 = DIRECTION ( 'NONE',  ( -1.000000000000000000, -1.224606353822377258E-16, -0.000000000000000000 ) ) ;
#61460 = CARTESIAN_POINT ( 'NONE',  ( -3.005480084712505828, 28.92564299267936079, 4.000000000000000000 ) ) ;
#61461 = DIRECTION ( 'NONE',  ( -0.9707728879609257566, 0.000000000000000000, -0.2400000000000086786 ) ) ;
#61463 = ORIENTED_EDGE ( 'NONE', *, *, #118850, .T. ) ;
#61462 = CIRCLE ( 'NONE', #47596, 5.968999999999998529 ) ;
#61464 = VERTEX_POINT ( 'NONE', #51934 ) ;
#61465 = ORIENTED_EDGE ( 'NONE', *, *, #27152, .F. ) ;
#61466 = AXIS2_PLACEMENT_3D ( 'NONE', #123656, #69262, #101148 ) ;
#61467 = ORIENTED_EDGE ( 'NONE', *, *, #34508, .F. ) ;
#61469 = ADVANCED_FACE ( 'NONE', ( #51216 ), #6931, .T. ) ;
#61468 =( BOUNDED_CURVE ( )  B_SPLINE_CURVE ( 3, ( #31037, #120868, #96943, #65101 ),
 .UNSPECIFIED., .F., .F. ) 
 B_SPLINE_CURVE_WITH_KNOTS ( ( 4, 4 ),
 ( 1.862445515227526327, 1.909667095125054725 ),
 .UNSPECIFIED. ) 
 CURVE ( )  GEOMETRIC_REPRESENTATION_ITEM ( )  RATIONAL_B_SPLINE_CURVE ( ( 1.000000000000000000, 0.9998141854983972898, 0.9998141854983972898, 1.000000000000000000 ) ) 
 REPRESENTATION_ITEM ( '' )  );
#61470 = DIRECTION ( 'NONE',  ( -0.7071067811865486830, -0.7071067811865464625, 0.000000000000000000 ) ) ;
#61472 = EDGE_CURVE ( 'NONE', #110860, #56431, #105558, .T. ) ;
#61471 = DIRECTION ( 'NONE',  ( -0.7071067811865486830, -0.7071067811865464625, 0.000000000000000000 ) ) ;
#61473 = ORIENTED_EDGE ( 'NONE', *, *, #421, .F. ) ;
#61474 = VECTOR ( 'NONE', #127676, 1000.000000000000000 ) ;
#61475 = FILL_AREA_STYLE ('',( #104187 ) ) ;
#61476 = FACE_OUTER_BOUND ( 'NONE', #84480, .T. ) ;
#61477 = CARTESIAN_POINT ( 'NONE',  ( 34.75611968250419181, -7.294349301475873126, 4.955485411084881164 ) ) ;
#61478 = SPHERICAL_SURFACE ( 'NONE', #115604, 0.5000000000000000000 ) ;
#61479 = CARTESIAN_POINT ( 'NONE',  ( 27.00000000000000711, -4.501766353396367215, -4.693270563879029744 ) ) ;
#61480 = ORIENTED_EDGE ( 'NONE', *, *, #82196, .T. ) ;
#61481 = CARTESIAN_POINT ( 'NONE',  ( 33.77004279457769798, 21.73644205237998506, 5.000000000000000888 ) ) ;
#61482 = DIRECTION ( 'NONE',  ( 0.000000000000000000, 0.000000000000000000, 1.000000000000000000 ) ) ;
#61483 = ORIENTED_EDGE ( 'NONE', *, *, #120997, .F. ) ;
#61484 = CARTESIAN_POINT ( 'NONE',  ( 16.49999999999988631, -7.420205493532884056, -2.617629953481214855 ) ) ;
#61485 = VERTEX_POINT ( 'NONE', #27288 ) ;
#61486 = EDGE_CURVE ( 'NONE', #43835, #133600, #72294, .T. ) ;
#61487 = CARTESIAN_POINT ( 'NONE',  ( 39.18398860626899705, 28.73617430169814568, 5.000000000000000000 ) ) ;
#61488 = ORIENTED_EDGE ( 'NONE', *, *, #42185, .F. ) ;
#61489 = ORIENTED_EDGE ( 'NONE', *, *, #7147, .F. ) ;
#61490 = CARTESIAN_POINT ( 'NONE',  ( 69.41709685856477563, 3.054999999999998828, 5.291415217122922066 ) ) ;
#61491 = ORIENTED_EDGE ( 'NONE', *, *, #93308, .F. ) ;
#61492 = VECTOR ( 'NONE', #81186, 1000.000000000000000 ) ;
#61493 = CARTESIAN_POINT ( 'NONE',  ( -68.99451991528748351, 28.92564299267986172, 4.000000000000000000 ) ) ;
#61494 = AXIS2_PLACEMENT_3D ( 'NONE', #115181, #60893, #60155 ) ;
#61495 = DIRECTION ( 'NONE',  ( -0.6830127018922180770, -0.6830127018922204085, -0.2588190451025213501 ) ) ;
#61496 = CARTESIAN_POINT ( 'NONE',  ( 107.4795968585647614, 6.109999999999999432, 1.637169565754164280 ) ) ;
#61497 = DIRECTION ( 'NONE',  ( 0.7071067811865487940, 0.7071067811865463515, 0.000000000000000000 ) ) ;
#61498 = AXIS2_PLACEMENT_3D ( 'NONE', #5622, #104954, #39735 ) ;
#61499 = FACE_OUTER_BOUND ( 'NONE', #119736, .T. ) ;
#61500 = DIRECTION ( 'NONE',  ( -0.7071067811865486830, 0.7071067811865464625, 0.000000000000000000 ) ) ;
#61501 = DIRECTION ( 'NONE',  ( -0.7071067811865486830, -0.7071067811865464625, 0.000000000000000000 ) ) ;
#61502 = VECTOR ( 'NONE', #91139, 1000.000000000000227 ) ;
#61503 = LINE ( 'NONE', #117942, #95581 ) ;
#61504 = CARTESIAN_POINT ( 'NONE',  ( 35.66252705046288440, 7.949999999999998401, 1.460391307983218338E-15 ) ) ;
#61505 = CARTESIAN_POINT ( 'NONE',  ( -36.29974487139159578, -27.71228299555231445, 4.000000000000000000 ) ) ;
#61506 = ORIENTED_EDGE ( 'NONE', *, *, #1729, .F. ) ;
#61507 = PRESENTATION_STYLE_ASSIGNMENT (( #4156 ) ) ;
#61508 = ORIENTED_EDGE ( 'NONE', *, *, #72371, .F. ) ;
#61509 = EDGE_LOOP ( 'NONE', ( #87136, #33810, #50773, #8236, #61508 ) ) ;
#61510 = EDGE_CURVE ( 'NONE', #33459, #42329, #40355, .T. ) ;
#61511 = FACE_OUTER_BOUND ( 'NONE', #34104, .T. ) ;
#61512 = VERTEX_POINT ( 'NONE', #29434 ) ;
#61513 = LINE ( 'NONE', #130321, #53712 ) ;
#61514 = LINE ( 'NONE', #124591, #24645 ) ;
#61515 = CARTESIAN_POINT ( 'NONE',  ( 27.22000000000000242, 9.521314400968980422E-16, 0.000000000000000000 ) ) ;
#61516 = CARTESIAN_POINT ( 'NONE',  ( 34.49999999999975842, 12.05432934483081908, 4.994342998332162331 ) ) ;
#61517 = EDGE_CURVE ( 'NONE', #129569, #75615, #71543, .T. ) ;
#61518 = ORIENTED_EDGE ( 'NONE', *, *, #132480, .T. ) ;
#61519 = CARTESIAN_POINT ( 'NONE',  ( 0.1679803408748695992, -48.55783623716597219, 38.28685941347700350 ) ) ;
#61520 = ORIENTED_EDGE ( 'NONE', *, *, #137199, .F. ) ;
#61521 = EDGE_CURVE ( 'NONE', #64622, #36177, #85242, .T. ) ;
#61522 = ADVANCED_FACE ( 'NONE', ( #73000 ), #49808, .F. ) ;
#61523 = CARTESIAN_POINT ( 'NONE',  ( 1.874569808101886226, 6.871911579029510442, -3.967499999999998916 ) ) ;
#61524 = LINE ( 'NONE', #105672, #139580 ) ;
#61525 = EDGE_CURVE ( 'NONE', #68726, #61837, #38901, .T. ) ;
#61526 = CARTESIAN_POINT ( 'NONE',  ( 3.299744871391591339, -27.71228299555208352, 4.000000000000000000 ) ) ;
#61527 = CARTESIAN_POINT ( 'NONE',  ( 12.52996815765592942, -8.713228220513846267, 3.789303709965370359 ) ) ;
#61528 = EDGE_LOOP ( 'NONE', ( #95991, #44155, #81219, #142636 ) ) ;
#61529 = ORIENTED_EDGE ( 'NONE', *, *, #131011, .T. ) ;
#61530 = ADVANCED_FACE ( 'NONE', ( #106259 ), #139675, .F. ) ;
#61531 = EDGE_LOOP ( 'NONE', ( #134554, #112647, #20186, #95439 ) ) ;
#61532 = LINE ( 'NONE', #30287, #88931 ) ;
#61533 = CARTESIAN_POINT ( 'NONE',  ( 34.49999999999976552, -14.94567065516889848, 4.994342998332158778 ) ) ;
#61534 = DIRECTION ( 'NONE',  ( -0.7071067811865486830, -0.7071067811865464625, 0.000000000000000000 ) ) ;
#61535 = ADVANCED_FACE ( 'NONE', ( #112543, #87929 ), #135048, .F. ) ;
#61536 = CARTESIAN_POINT ( 'NONE',  ( 54.18398860626899705, 28.73617430169825226, 5.000000000000000000 ) ) ;
#61537 = CARTESIAN_POINT ( 'NONE',  ( 23.99999999999983302, -7.068876922607743474, 4.000000000000000000 ) ) ;
#61538 = EDGE_CURVE ( 'NONE', #135668, #78193, #24815, .T. ) ;
#61539 = PLANE ( 'NONE',  #127268 ) ;
#61540 = CARTESIAN_POINT ( 'NONE',  ( 20.66652290003515446, 8.920938975803856863, 4.000000000000000000 ) ) ;
#61541 = ORIENTED_EDGE ( 'NONE', *, *, #116955, .F. ) ;
#61542 = DIRECTION ( 'NONE',  ( -0.3543493200069162685, -0.000000000000000000, -0.9351131265310288487 ) ) ;
#61543 = DIRECTION ( 'NONE',  ( -0.000000000000000000, 0.3543493200069153248, 0.9351131265310292928 ) ) ;
#61544 = ORIENTED_EDGE ( 'NONE', *, *, #85869, .T. ) ;
#61545 = EDGE_CURVE ( 'NONE', #25035, #60374, #132902, .T. ) ;
#61546 = DIRECTION ( 'NONE',  ( -0.7071067811865486830, 0.7071067811865464625, 0.000000000000000000 ) ) ;
#61548 = VERTEX_POINT ( 'NONE', #45185 ) ;
#61547 = CARTESIAN_POINT ( 'NONE',  ( 55.49226980200836579, -49.12413125935074731, -39.93743342457434409 ) ) ;
#61549 = EDGE_CURVE ( 'NONE', #65537, #99825, #78494, .T. ) ;
#61550 = CARTESIAN_POINT ( 'NONE',  ( 26.29289321881327268, 8.259292476615639700, 5.000000000000000000 ) ) ;
#61551 = DIRECTION ( 'NONE',  ( 0.6830127018922180770, -0.6830127018922204085, -0.2588190451025213501 ) ) ;
#61552 = ORIENTED_EDGE ( 'NONE', *, *, #120529, .T. ) ;
#61553 = CARTESIAN_POINT ( 'NONE',  ( 17.99999999999989342, 20.58746187583903620, 4.000000000000000000 ) ) ;
#61554 = ORIENTED_EDGE ( 'NONE', *, *, #137481, .T. ) ;
#61555 = EDGE_CURVE ( 'NONE', #117394, #99025, #101658, .T. ) ;
#61556 = PLANE ( 'NONE',  #84536 ) ;
#61557 = VECTOR ( 'NONE', #117354, 1000.000000000000000 ) ;
#61558 = CARTESIAN_POINT ( 'NONE',  ( 121.9958603837962272, -3.974999999999998312, -6.884901960086286188 ) ) ;
#61559 = CARTESIAN_POINT ( 'NONE',  ( 13.82816939922342669, -8.240707523384203981, 4.000000000000000000 ) ) ;
#61560 = DIRECTION ( 'NONE',  ( -0.3543493200069162685, -0.000000000000000000, -0.9351131265310288487 ) ) ;
#61561 = VECTOR ( 'NONE', #202, 1000.000000000000000 ) ;
#61562 = CARTESIAN_POINT ( 'NONE',  ( 0.000000000000000000, 0.000000000000000000, 5.000000000000000000 ) ) ;
#61563 = CARTESIAN_POINT ( 'NONE',  ( 59.99451991528749772, 28.92564299267980132, 4.000000000000000000 ) ) ;
#61564 = DIRECTION ( 'NONE',  ( 0.6830127018922181881, 0.6830127018922202975, -0.2588190451025214056 ) ) ;
#61565 = CARTESIAN_POINT ( 'NONE',  ( 27.97873647476855297, -5.808823158059033709, 5.808823158059035485 ) ) ;
#61566 = CARTESIAN_POINT ( 'NONE',  ( 7.999569808101885116, -3.967499999999998028, -6.871911579029511330 ) ) ;
#61567 = DIRECTION ( 'NONE',  ( -0.7071067811865487940, 0.7071067811865463515, 0.000000000000000000 ) ) ;
#61568 = FACE_OUTER_BOUND ( 'NONE', #96344, .T. ) ;
#61569 = CARTESIAN_POINT ( 'NONE',  ( 4.748455871324219757, -11.24070752338416490, 10.39518518046008211 ) ) ;
#61570 = ORIENTED_EDGE ( 'NONE', *, *, #102124, .T. ) ;
#61571 = ORIENTED_EDGE ( 'NONE', *, *, #45467, .F. ) ;
#61572 = CARTESIAN_POINT ( 'NONE',  ( 82.81250000000000000, 5.819803920172571310, 5.819803920172575751 ) ) ;
#61573 = CARTESIAN_POINT ( 'NONE',  ( 25.39999999999999503, 3.246059068589359775, 5.158694168414005077 ) ) ;
#61574 = ORIENTED_EDGE ( 'NONE', *, *, #136347, .T. ) ;
#61575 = EDGE_CURVE ( 'NONE', #11390, #99127, #90060, .T. ) ;
#61576 = DIRECTION ( 'NONE',  ( 0.000000000000000000, 0.000000000000000000, 1.000000000000000000 ) ) ;
#61577 = DIRECTION ( 'NONE',  ( 1.000000000000000000, -0.000000000000000000, -0.000000000000000000 ) ) ;
#61578 = CARTESIAN_POINT ( 'NONE',  ( 3.469446951953614189E-15, -8.731860332648842871, -2.120594902707538143 ) ) ;
#61579 = ORIENTED_EDGE ( 'NONE', *, *, #11682, .T. ) ;
#61580 = CARTESIAN_POINT ( 'NONE',  ( 15.70710678118643955, -3.740707523384239952, 5.000000000000000000 ) ) ;
#61581 = PLANE ( 'NONE',  #62635 ) ;
#61582 = CARTESIAN_POINT ( 'NONE',  ( -5.292893218813418343, -6.740707523384218192, 5.000000000000000000 ) ) ;
#61583 = DIRECTION ( 'NONE',  ( 1.000000000000000000, 0.000000000000000000, 0.000000000000000000 ) ) ;
#61584 = CARTESIAN_POINT ( 'NONE',  ( 17.51078643762690845, -27.52281430457043143, 5.000000000000000000 ) ) ;
#61585 = DIRECTION ( 'NONE',  ( 0.000000000000000000, -1.000000000000000000, 0.000000000000000000 ) ) ;
#61586 = FACE_OUTER_BOUND ( 'NONE', #80557, .T. ) ;
#61587 = LINE ( 'NONE', #18006, #75540 ) ;
#61588 = CARTESIAN_POINT ( 'NONE',  ( 152.4000000000000057, -14.29000000000013593, -12.70000000000045404 ) ) ;
#61589 = EDGE_CURVE ( 'NONE', #119359, #7710, #90811, .T. ) ;
#61590 = VECTOR ( 'NONE', #107727, 1000.000000000000227 ) ;
#61591 = CARTESIAN_POINT ( 'NONE',  ( 57.90314192168177954, -45.52550609312090302, 35.40428284070832632 ) ) ;
#61592 = ORIENTED_EDGE ( 'NONE', *, *, #71873, .T. ) ;
#61593 = ORIENTED_EDGE ( 'NONE', *, *, #33033, .F. ) ;
#61594 = VECTOR ( 'NONE', #125606, 999.9999999999998863 ) ;
#61595 = CARTESIAN_POINT ( 'NONE',  ( 98.58376352523144703, -6.110000000000001208, -3.741295971395164515E-16 ) ) ;
#61596 = ORIENTED_EDGE ( 'NONE', *, *, #66462, .T. ) ;
#61597 = AXIS2_PLACEMENT_3D ( 'NONE', #19177, #140252, #8262 ) ;
#61598 = AXIS2_PLACEMENT_3D ( 'NONE', #110206, #11593, #110910 ) ;
#61599 = EDGE_CURVE ( 'NONE', #48649, #15762, #13201, .T. ) ;
#61600 = CARTESIAN_POINT ( 'NONE',  ( 0.000000000000000000, -21.76999999999999247, 0.000000000000000000 ) ) ;
#61601 = VECTOR ( 'NONE', #38529, 1000.000000000000000 ) ;
#61602 = CARTESIAN_POINT ( 'NONE',  ( -18.29974487139159223, -27.71228299555219010, 4.000000000000000000 ) ) ;
#61603 = VERTEX_POINT ( 'NONE', #13917 ) ;
#61604 = CARTESIAN_POINT ( 'NONE',  ( -57.48921356237308800, -27.52281430457095368, 5.000000000000000000 ) ) ;
#61605 = FACE_OUTER_BOUND ( 'NONE', #113978, .T. ) ;
#61606 = CARTESIAN_POINT ( 'NONE',  ( 91.49543019189812298, 5.291415217122916737, 3.055000000000001936 ) ) ;
#61607 = VERTEX_POINT ( 'NONE', #46633 ) ;
#61608 = EDGE_CURVE ( 'NONE', #57945, #81077, #900, .T. ) ;
#61609 = CARTESIAN_POINT ( 'NONE',  ( 17.28769006033959954, -21.73547319004781286, 4.999917730833664642 ) ) ;
#61610 = ORIENTED_EDGE ( 'NONE', *, *, #58959, .F. ) ;
#61611 = PLANE ( 'NONE',  #96251 ) ;
#61612 = DIRECTION ( 'NONE',  ( 1.000000000000000000, 0.000000000000000000, 0.000000000000000000 ) ) ;
#61613 = DIRECTION ( 'NONE',  ( 0.7071067811865487940, -0.7071067811865463515, 0.000000000000000000 ) ) ;
#61614 = LINE ( 'NONE', #2349, #138847 ) ;
#61615 = ORIENTED_EDGE ( 'NONE', *, *, #36040, .F. ) ;
#61616 = ORIENTED_EDGE ( 'NONE', *, *, #65951, .F. ) ;
#61617 = EDGE_CURVE ( 'NONE', #53079, #77276, #98790, .T. ) ;
#61618 = ORIENTED_EDGE ( 'NONE', *, *, #24560, .T. ) ;
#61619 = LINE ( 'NONE', #104352, #109315 ) ;
#61620 = PLANE ( 'NONE',  #75506 ) ;
#61621 = CARTESIAN_POINT ( 'NONE',  ( 9.837903141435219823, -6.871911579029513106, -3.967499999999993587 ) ) ;
#61622 = CARTESIAN_POINT ( 'NONE',  ( -21.18398860626899349, 28.73617430169802134, 5.000000000000000000 ) ) ;
#61623 =( NAMED_UNIT ( * ) PLANE_ANGLE_UNIT ( ) SI_UNIT ( $, .RADIAN. ) );
#61624 = ORIENTED_EDGE ( 'NONE', *, *, #136456, .T. ) ;
#61625 = EDGE_LOOP ( 'NONE', ( #59191, #97391, #59402, #9861 ) ) ;
#61626 = PLANE ( 'NONE',  #101281 ) ;
#61627 = ORIENTED_EDGE ( 'NONE', *, *, #1573, .T. ) ;
#61628 = ORIENTED_EDGE ( 'NONE', *, *, #1166, .F. ) ;
#61629 = VECTOR ( 'NONE', #44084, 1000.000000000000000 ) ;
#61630 = CARTESIAN_POINT ( 'NONE',  ( 115.7037635252314516, 6.109999999999998543, 1.122388791418548911E-15 ) ) ;
#61631 = FACE_OUTER_BOUND ( 'NONE', #47034, .T. ) ;
#61633 = ADVANCED_FACE ( 'NONE', ( #24114 ), #32869, .F. ) ;
#61632 = LINE ( 'NONE', #115220, #12487 ) ;
#61634 = ORIENTED_EDGE ( 'NONE', *, *, #1970, .T. ) ;
#61635 = LINE ( 'NONE', #105789, #94628 ) ;
#61636 = CARTESIAN_POINT ( 'NONE',  ( -7.499999999999944045, -10.04351517176479014, -1.623559851933840337 ) ) ;
#61637 = ORIENTED_EDGE ( 'NONE', *, *, #52347, .F. ) ;
#61638 = DIRECTION ( 'NONE',  ( -0.7071067811865487940, 0.7071067811865463515, 0.000000000000000000 ) ) ;
#61639 = DIRECTION ( 'NONE',  ( 0.000000000000000000, -1.000000000000000000, 0.000000000000000000 ) ) ;
#61640 = ORIENTED_EDGE ( 'NONE', *, *, #103290, .T. ) ;
#61641 = DIRECTION ( 'NONE',  ( -0.000000000000000000, -1.000000000000000000, -0.000000000000000000 ) ) ;
#61642 = CARTESIAN_POINT ( 'NONE',  ( 14.99999999999989519, 9.631307414974335401, -9.079085613539508159 ) ) ;
#61643 = CARTESIAN_POINT ( 'NONE',  ( -26.99999999999980815, 19.55218569542896390, 5.000000000000000000 ) ) ;
#61644 = ADVANCED_FACE ( 'NONE', ( #133596 ), #77090, .F. ) ;
#61645 = ORIENTED_EDGE ( 'NONE', *, *, #130693, .T. ) ;
#61646 = CARTESIAN_POINT ( 'NONE',  ( 1.516262732464673579, 0.4000000000000001887, -2.467792535850613866 ) ) ;
#61647 = VERTEX_POINT ( 'NONE', #11773 ) ;
#61648 = ORIENTED_EDGE ( 'NONE', *, *, #113154, .F. ) ;
#61649 =( BOUNDED_CURVE ( )  B_SPLINE_CURVE ( 3, ( #134302, #53902, #90053, #67640 ),
 .UNSPECIFIED., .F., .T. ) 
 B_SPLINE_CURVE_WITH_KNOTS ( ( 4, 4 ),
 ( 5.106027341939277875, 6.645403452391244414 ),
 .UNSPECIFIED. ) 
 CURVE ( )  GEOMETRIC_REPRESENTATION_ITEM ( )  RATIONAL_B_SPLINE_CURVE ( ( 1.000000000000000000, 0.8120851936182275077, 0.8120851936182275077, 1.000000000000000000 ) ) 
 REPRESENTATION_ITEM ( '' )  );
#61650 = ORIENTED_EDGE ( 'NONE', *, *, #87367, .T. ) ;
#61651 = CARTESIAN_POINT ( 'NONE',  ( 28.34959685856477662, 6.109999999999996767, 1.637169565754163836 ) ) ;
#61652 = ORIENTED_EDGE ( 'NONE', *, *, #28139, .T. ) ;
#61653 = LINE ( 'NONE', #138481, #55279 ) ;
#61654 = CARTESIAN_POINT ( 'NONE',  ( 7.139999999999984581, -39.92999999999998550, -39.79289321881344677 ) ) ;
#61655 = AXIS2_PLACEMENT_3D ( 'NONE', #3437, #47728, #91223 ) ;
#61656 = CARTESIAN_POINT ( 'NONE',  ( -41.99451991528749062, 28.92564299267967343, 4.000000000000000000 ) ) ;
#61657 = DIRECTION ( 'NONE',  ( -1.000000000000000000, -0.000000000000000000, -0.000000000000000000 ) ) ;
#61658 = FACE_OUTER_BOUND ( 'NONE', #92413, .T. ) ;
#61659 = DIRECTION ( 'NONE',  ( -0.000000000000000000, 0.3543493200069153248, 0.9351131265310292928 ) ) ;
#61660 = FACE_OUTER_BOUND ( 'NONE', #52755, .T. ) ;
#61661 = LINE ( 'NONE', #29697, #76036 ) ;
#61662 = FACE_OUTER_BOUND ( 'NONE', #21848, .T. ) ;
#61663 = CIRCLE ( 'NONE', #142672, 5.968999999999998529 ) ;
#61664 = VERTEX_POINT ( 'NONE', #57475 ) ;
#61665 = ORIENTED_EDGE ( 'NONE', *, *, #39053, .F. ) ;
#61666 = ORIENTED_EDGE ( 'NONE', *, *, #134560, .F. ) ;
#61667 = VERTEX_POINT ( 'NONE', #100943 ) ;
#61668 = CARTESIAN_POINT ( 'NONE',  ( -0.8069443138166949581, 1.049154855905557238, 3.918431363226604347 ) ) ;
#61669 = ORIENTED_EDGE ( 'NONE', *, *, #90091, .T. ) ;
#61670 = ORIENTED_EDGE ( 'NONE', *, *, #122692, .T. ) ;
#61671 = DIRECTION ( 'NONE',  ( -0.000000000000000000, 0.000000000000000000, 1.000000000000000000 ) ) ;
#61672 = CARTESIAN_POINT ( 'NONE',  ( -35.99451991528749772, 28.92564299267963079, 4.000000000000000000 ) ) ;
#61673 = VECTOR ( 'NONE', #36780, 999.9999999999998863 ) ;
#61674 = CARTESIAN_POINT ( 'NONE',  ( -32.99999999999976552, 13.55218569542903140, 5.000000000000000000 ) ) ;
#61675 = ORIENTED_EDGE ( 'NONE', *, *, #128694, .F. ) ;
#61676 = DIRECTION ( 'NONE',  ( 0.7071067811865487940, 0.7071067811865463515, 0.000000000000000000 ) ) ;
#61677 = VERTEX_POINT ( 'NONE', #111841 ) ;
#61678 = VECTOR ( 'NONE', #7523, 1000.000000000000227 ) ;
#61680 = CARTESIAN_POINT ( 'NONE',  ( 54.29974487139159578, -27.71228299555243879, 4.000000000000000000 ) ) ;
#61679 = AXIS2_PLACEMENT_3D ( 'NONE', #109722, #24148, #54649 ) ;
#61681 = DIRECTION ( 'NONE',  ( -0.000000000000000000, 0.000000000000000000, 1.000000000000000000 ) ) ;
#61682 = ADVANCED_FACE ( 'NONE', ( #110373 ), #100245, .F. ) ;
#61683 = CARTESIAN_POINT ( 'NONE',  ( 6.629569808101885897, -3.967499999999998028, -6.871911579029511330 ) ) ;
#61684 = EDGE_LOOP ( 'NONE', ( #142619, #69495, #138429, #23983 ) ) ;
#61686 = DIRECTION ( 'NONE',  ( -0.3543493200069162685, -0.000000000000000000, -0.9351131265310288487 ) ) ;
#61685 = CARTESIAN_POINT ( 'NONE',  ( 100.9745968585647660, 1.637169565754164280, -6.109999999999997655 ) ) ;
#61687 = EDGE_CURVE ( 'NONE', #104985, #114666, #77786, .T. ) ;
#61688 = CARTESIAN_POINT ( 'NONE',  ( -45.48921356237309510, -27.52281430457087197, 5.000000000000000000 ) ) ;
#61689 = EDGE_LOOP ( 'NONE', ( #75856, #109993, #48264, #136510 ) ) ;
#61690 = ORIENTED_EDGE ( 'NONE', *, *, #70095, .F. ) ;
#61691 = EDGE_CURVE ( 'NONE', #74078, #50218, #34273, .T. ) ;
#61692 = CARTESIAN_POINT ( 'NONE',  ( 21.18398860626899349, 28.73617430169802134, 5.000000000000000000 ) ) ;
#61693 = ORIENTED_EDGE ( 'NONE', *, *, #101440, .T. ) ;
#61694 = CARTESIAN_POINT ( 'NONE',  ( -12.70710678118645731, -3.740707523384243505, 5.000000000000000000 ) ) ;
#61695 = LINE ( 'NONE', #7248, #48789 ) ;
#61696 = CARTESIAN_POINT ( 'NONE',  ( 0.000000000000000000, 21.72500000000000142, 4.500000000000000888 ) ) ;
#61697 = EDGE_CURVE ( 'NONE', #94785, #3074, #67648, .T. ) ;
#61698 = DIRECTION ( 'NONE',  ( -0.7071067811865487940, 0.7071067811865463515, -0.000000000000000000 ) ) ;
#61699 = ORIENTED_EDGE ( 'NONE', *, *, #133464, .T. ) ;
#61700 = CARTESIAN_POINT ( 'NONE',  ( -9.299744871391588674, -27.71228299555212971, 4.000000000000000000 ) ) ;
#61701 = LINE ( 'NONE', #5830, #25599 ) ;
#61702 = CARTESIAN_POINT ( 'NONE',  ( 19.41972383043609440, 0.000000000000000000, 2.500000000000000444 ) ) ;
#61703 = ORIENTED_EDGE ( 'NONE', *, *, #23331, .T. ) ;
#61704 = LINE ( 'NONE', #47294, #55920 ) ;
#61705 = CARTESIAN_POINT ( 'NONE',  ( 56.99451991528749062, 28.92564299267978001, 4.000000000000000000 ) ) ;
#61706 = VERTEX_POINT ( 'NONE', #47349 ) ;
#61707 = EDGE_CURVE ( 'NONE', #99872, #81380, #92926, .T. ) ;
#61709 = ORIENTED_EDGE ( 'NONE', *, *, #46487, .T. ) ;
#61708 = CARTESIAN_POINT ( 'NONE',  ( -5.510786437626906675, -27.52281430457051314, 5.000000000000000000 ) ) ;
#61710 = EDGE_CURVE ( 'NONE', #78277, #86576, #61074, .T. ) ;
#61711 = ORIENTED_EDGE ( 'NONE', *, *, #115960, .T. ) ;
#61712 = CARTESIAN_POINT ( 'NONE',  ( -31.49999999999977263, -17.94781430457064531, 5.000000000000000000 ) ) ;
#61713 = FACE_OUTER_BOUND ( 'NONE', #125280, .T. ) ;
#61714 = ORIENTED_EDGE ( 'NONE', *, *, #121114, .F. ) ;
#61715 = CARTESIAN_POINT ( 'NONE',  ( 2.816011393730999401, 28.73617430169785436, 5.000000000000000000 ) ) ;
#61716 = ADVANCED_FACE ( 'NONE', ( #16797 ), #42130, .T. ) ;
#61717 = CARTESIAN_POINT ( 'NONE',  ( 24.48921356237309510, -27.52281430457072631, 5.000000000000000000 ) ) ;
#61718 = VECTOR ( 'NONE', #143479, 1000.000000000000000 ) ;
#61719 = CARTESIAN_POINT ( 'NONE',  ( 8.999999999999937828, -19.44781430457063465, 5.000000000000000000 ) ) ;
#61720 = DIRECTION ( 'NONE',  ( -0.6830127018922180770, -0.6830127018922204085, -0.2588190451025213501 ) ) ;
#61721 = CARTESIAN_POINT ( 'NONE',  ( -12.72281430457050710, -21.72500000000000142, 5.000000000000000000 ) ) ;
#61722 = DIRECTION ( 'NONE',  ( -1.000000000000000000, -0.000000000000000000, -0.000000000000000000 ) ) ;
#61723 = CARTESIAN_POINT ( 'NONE',  ( 6.489213562373093325, -27.52281430457059841, 5.000000000000000000 ) ) ;
#61724 = EDGE_CURVE ( 'NONE', #130915, #76045, #58938, .T. ) ;
#61726 = VECTOR ( 'NONE', #28941, 1000.000000000000000 ) ;
#61725 = DIRECTION ( 'NONE',  ( 0.7071067811865486830, -0.7071067811865464625, -0.000000000000000000 ) ) ;
#61727 = DIRECTION ( 'NONE',  ( -0.7071067811865486830, 0.7071067811865464625, 0.000000000000000000 ) ) ;
#61728 = DIRECTION ( 'NONE',  ( -0.000000000000000000, 0.000000000000000000, 1.000000000000000000 ) ) ;
#61729 = CARTESIAN_POINT ( 'NONE',  ( -12.18398860626900060, 28.73617430169795739, 5.000000000000000000 ) ) ;
#61730 = ORIENTED_EDGE ( 'NONE', *, *, #132268, .F. ) ;
#61731 = ORIENTED_EDGE ( 'NONE', *, *, #114669, .F. ) ;
#61732 = ORIENTED_EDGE ( 'NONE', *, *, #4457, .F. ) ;
#61733 = CARTESIAN_POINT ( 'NONE',  ( 109.2083333333333428, -3.974999999999999201, -6.884901960086287964 ) ) ;
#61734 = ORIENTED_EDGE ( 'NONE', *, *, #27693, .F. ) ;
#61735 = ORIENTED_EDGE ( 'NONE', *, *, #20414, .T. ) ;
#61736 = ORIENTED_EDGE ( 'NONE', *, *, #142016, .F. ) ;
#61737 = EDGE_CURVE ( 'NONE', #117017, #121969, #111529, .T. ) ;
#61738 = VECTOR ( 'NONE', #102554, 999.9999999999998863 ) ;
#61739 = DIRECTION ( 'NONE',  ( -0.7071067811865486830, -0.7071067811865464625, 0.000000000000000000 ) ) ;
#61740 = DIRECTION ( 'NONE',  ( 0.7071067811865486830, -0.7071067811865464625, -0.000000000000000000 ) ) ;
#61741 = ORIENTED_EDGE ( 'NONE', *, *, #12988, .T. ) ;
#61742 = DIRECTION ( 'NONE',  ( 0.000000000000000000, 1.000000000000000000, 0.000000000000000000 ) ) ;
#61743 = DIRECTION ( 'NONE',  ( 0.3543493200069163240, 0.000000000000000000, -0.9351131265310288487 ) ) ;
#61744 = CARTESIAN_POINT ( 'NONE',  ( -42.48921356237308800, -27.52281430457085065, 5.000000000000000000 ) ) ;
#61745 = DIRECTION ( 'NONE',  ( 0.000000000000000000, 0.000000000000000000, -1.000000000000000000 ) ) ;
#61746 = CARTESIAN_POINT ( 'NONE',  ( 107.4795968585647614, 6.109999999999999432, 1.637169565754164280 ) ) ;
#61747 = ORIENTED_EDGE ( 'NONE', *, *, #114502, .F. ) ;
#61748 = CARTESIAN_POINT ( 'NONE',  ( -7.213366709350353290, 11.05501350725457499, -28.05856295898191632 ) ) ;
#61749 = SURFACE_STYLE_USAGE ( .BOTH. , #18926 ) ;
#61750 = LINE ( 'NONE', #95049, #82154 ) ;
#61751 = DIRECTION ( 'NONE',  ( 0.000000000000000000, 0.000000000000000000, 1.000000000000000000 ) ) ;
#61752 = DIRECTION ( 'NONE',  ( 0.000000000000000000, -1.000000000000000000, 0.000000000000000000 ) ) ;
#61753 = DIRECTION ( 'NONE',  ( -0.7071067811865486830, 0.7071067811865464625, 0.000000000000000000 ) ) ;
#61754 = CARTESIAN_POINT ( 'NONE',  ( 36.82919371712956291, -3.975000000000001865, 6.884901960086284411 ) ) ;
#61755 = EDGE_CURVE ( 'NONE', #131987, #37298, #58216, .T. ) ;
#61756 = VECTOR ( 'NONE', #44551, 1000.000000000000227 ) ;
#61757 = DIRECTION ( 'NONE',  ( 0.6830127018922180770, -0.6830127018922204085, -0.2588190451025213501 ) ) ;
#61758 = LINE ( 'NONE', #125582, #66950 ) ;
#61759 = ORIENTED_EDGE ( 'NONE', *, *, #133838, .F. ) ;
#61760 = ORIENTED_EDGE ( 'NONE', *, *, #58108, .F. ) ;
#61761 = CARTESIAN_POINT ( 'NONE',  ( 126.5837635252314612, -6.110000000000001208, -3.741295971395164515E-16 ) ) ;
#61762 = VECTOR ( 'NONE', #121654, 1000.000000000000000 ) ;
#61763 = ORIENTED_EDGE ( 'NONE', *, *, #139385, .T. ) ;
#61764 = DIRECTION ( 'NONE',  ( -0.6830127018922180770, -0.6830127018922204085, -0.2588190451025213501 ) ) ;
#61765 = DIRECTION ( 'NONE',  ( -0.5735764363510503783, -0.8191520442889886899, 0.000000000000000000 ) ) ;
#61766 = PLANE ( 'NONE',  #119778 ) ;
#61767 = SURFACE_STYLE_FILL_AREA ( #126288 ) ;
#61768 = DIRECTION ( 'NONE',  ( 0.7071067811865486830, -0.7071067811865464625, -0.000000000000000000 ) ) ;
#61769 = CARTESIAN_POINT ( 'NONE',  ( 27.56293019189811133, 1.637169565754157174, 6.110000000000002984 ) ) ;
#61771 = ORIENTED_EDGE ( 'NONE', *, *, #9284, .T. ) ;
#61770 = VECTOR ( 'NONE', #39699, 999.9999999999998863 ) ;
#61772 = EDGE_CURVE ( 'NONE', #98208, #67296, #137883, .T. ) ;
#61773 = CARTESIAN_POINT ( 'NONE',  ( 18.29974487139159223, -27.71228299555219010, 4.000000000000000000 ) ) ;
#61774 = VERTEX_POINT ( 'NONE', #38557 ) ;
#61775 = LINE ( 'NONE', #29121, #60148 ) ;
#61776 = CARTESIAN_POINT ( 'NONE',  ( -8.207106781186478628, -11.24070752338416845, 5.000000000000000000 ) ) ;
#61777 = DIRECTION ( 'NONE',  ( 0.6830127018922181881, 0.6830127018922202975, -0.2588190451025214056 ) ) ;
#61778 = PLANE ( 'NONE',  #4671 ) ;
#61779 = ORIENTED_EDGE ( 'NONE', *, *, #68538, .T. ) ;
#61780 = CARTESIAN_POINT ( 'NONE',  ( 59.79209685856477563, -5.291415217122921177, 3.054999999999999272 ) ) ;
#61781 = EDGE_CURVE ( 'NONE', #116410, #101064, #50155, .T. ) ;
#61782 = VERTEX_POINT ( 'NONE', #3054 ) ;
#61783 = CARTESIAN_POINT ( 'NONE',  ( -11.99999999999990585, 2.587461875839209391, 4.000000000000000000 ) ) ;
#61784 = CARTESIAN_POINT ( 'NONE',  ( -10.49999999999992184, -5.947814304570770538, 5.000000000000000000 ) ) ;
#61785 = CYLINDRICAL_SURFACE ( 'NONE', #84942, 0.5000000000000000000 ) ;
#61786 = CARTESIAN_POINT ( 'NONE',  ( -25.39999999999996305, 0.000000000000000000, 0.000000000000000000 ) ) ;
#61787 = AXIS2_PLACEMENT_3D ( 'NONE', #129151, #63915, #108081 ) ;
#61789 = AXIS2_PLACEMENT_3D ( 'NONE', #119121, #77779, #19802 ) ;
#61788 = VECTOR ( 'NONE', #125434, 1000.000000000000000 ) ;
#61790 = VECTOR ( 'NONE', #44473, 1000.000000000000000 ) ;
#61791 = CARTESIAN_POINT ( 'NONE',  ( 51.24543019189811588, -5.291415217122918513, -3.055000000000000160 ) ) ;
#61792 = ORIENTED_EDGE ( 'NONE', *, *, #28788, .T. ) ;
#61793 = DIRECTION ( 'NONE',  ( 1.000000000000000000, 0.000000000000000000, 0.000000000000000000 ) ) ;
#61794 = EDGE_CURVE ( 'NONE', #74659, #87168, #39281, .T. ) ;
#61795 = LINE ( 'NONE', #30582, #36310 ) ;
#61796 = ORIENTED_EDGE ( 'NONE', *, *, #46901, .T. ) ;
#61797 = ORIENTED_EDGE ( 'NONE', *, *, #19423, .T. ) ;
#61798 = AXIS2_PLACEMENT_3D ( 'NONE', #126769, #105719, #28198 ) ;
#61799 = DIRECTION ( 'NONE',  ( -1.000000000000000000, -8.718663809566799855E-16, 0.000000000000000000 ) ) ;
#61800 = ORIENTED_EDGE ( 'NONE', *, *, #126753, .T. ) ;
#61801 = CARTESIAN_POINT ( 'NONE',  ( 60.89169371712955581, 2.130196079827421762, 7.950000000000000178 ) ) ;
#61802 = PRODUCT_DEFINITION_CONTEXT ( 'detailed design', #72652, 'design' ) ;
#61803 = ADVANCED_FACE ( 'NONE', ( #83504 ), #124843, .F. ) ;
#61804 = ORIENTED_EDGE ( 'NONE', *, *, #123288, .T. ) ;
#61805 = CARTESIAN_POINT ( 'NONE',  ( 45.14169371712955581, -2.130196079827424871, -7.949999999999998401 ) ) ;
#61806 = PLANE ( 'NONE',  #141449 ) ;
#61807 = EDGE_CURVE ( 'NONE', #132626, #19726, #103100, .T. ) ;
#61808 = FACE_BOUND ( 'NONE', #3151, .T. ) ;
#61809 = DIRECTION ( 'NONE',  ( 0.7071067811865486830, -0.7071067811865464625, -0.000000000000000000 ) ) ;
#61810 =( LENGTH_UNIT ( ) NAMED_UNIT ( * ) SI_UNIT ( .MILLI., .METRE. ) );
#61812 = EDGE_CURVE ( 'NONE', #118545, #68539, #127719, .T. ) ;
#61811 = CARTESIAN_POINT ( 'NONE',  ( -11.24139925780195171, 21.72500000000000142, 5.000000000000000000 ) ) ;
#61813 = ORIENTED_EDGE ( 'NONE', *, *, #28768, .F. ) ;
#61814 = PLANE ( 'NONE',  #105918 ) ;
#61816 = EDGE_LOOP ( 'NONE', ( #102644, #40626, #13071, #85389 ) ) ;
#61815 = LINE ( 'NONE', #72727, #22687 ) ;
#61817 = CIRCLE ( 'NONE', #75775, 5.968999999999998529 ) ;
#61818 = ORIENTED_EDGE ( 'NONE', *, *, #96029, .T. ) ;
#61819 = FACE_OUTER_BOUND ( 'NONE', #76321, .T. ) ;
#61820 = ORIENTED_EDGE ( 'NONE', *, *, #55459, .T. ) ;
#61821 = CARTESIAN_POINT ( 'NONE',  ( 52.99543019189811588, 5.291415217122916737, 3.055000000000001936 ) ) ;
#61822 = CIRCLE ( 'NONE', #38724, 2.500000000000000444 ) ;
#61823 = ORIENTED_EDGE ( 'NONE', *, *, #67709, .F. ) ;
#61824 = LINE ( 'NONE', #61147, #115840 ) ;
#61825 = CARTESIAN_POINT ( 'NONE',  ( 151.4000000000000057, -18.48000000000005372, -34.92499999999998295 ) ) ;
#61826 = VERTEX_POINT ( 'NONE', #72663 ) ;
#61827 = DIRECTION ( 'NONE',  ( -1.000000000000000000, 0.000000000000000000, -0.000000000000000000 ) ) ;
#61828 = AXIS2_PLACEMENT_3D ( 'NONE', #96469, #87776, #1 ) ;
#61829 = ADVANCED_FACE ( 'NONE', ( #48025 ), #37118, .F. ) ;
#61830 = PLANE ( 'NONE',  #112740 ) ;
#61831 = CARTESIAN_POINT ( 'NONE',  ( 14.72063736826143732, 7.288814752023356824, 4.957798599204235046 ) ) ;
#61832 = FACE_OUTER_BOUND ( 'NONE', #644, .T. ) ;
#61833 = CARTESIAN_POINT ( 'NONE',  ( -26.99999999999980105, 4.552185695429119328, 5.000000000000000000 ) ) ;
#61834 = FACE_OUTER_BOUND ( 'NONE', #132820, .T. ) ;
#61835 = ORIENTED_EDGE ( 'NONE', *, *, #62820, .T. ) ;
#61836 = VECTOR ( 'NONE', #65316, 1000.000000000000227 ) ;
#61837 = VERTEX_POINT ( 'NONE', #4416 ) ;
#61838 = LINE ( 'NONE', #8797, #77182 ) ;
#61839 = DIRECTION ( 'NONE',  ( -0.000000000000000000, 0.000000000000000000, 1.000000000000000000 ) ) ;
#61840 = ORIENTED_EDGE ( 'NONE', *, *, #111043, .F. ) ;
#61841 = VERTEX_POINT ( 'NONE', #48725 ) ;
#61842 = ORIENTED_EDGE ( 'NONE', *, *, #23184, .F. ) ;
#61843 = CARTESIAN_POINT ( 'NONE',  ( -63.18398860626900415, 28.73617430169831621, 5.000000000000000000 ) ) ;
#61844 = CARTESIAN_POINT ( 'NONE',  ( 54.91252705046288440, -7.949999999999998401, -4.867971026610728450E-16 ) ) ;
#61845 = AXIS2_PLACEMENT_3D ( 'NONE', #87101, #31999, #98674 ) ;
#61846 = DIRECTION ( 'NONE',  ( 1.000000000000000000, 1.224606353822377258E-16, 0.000000000000000000 ) ) ;
#61847 = ORIENTED_EDGE ( 'NONE', *, *, #60542, .F. ) ;
#61848 = CARTESIAN_POINT ( 'NONE',  ( 23.99451991528749062, 28.92564299267954908, 4.000000000000000000 ) ) ;
#61850 = EDGE_CURVE ( 'NONE', #138986, #136777, #82784, .T. ) ;
#61849 = DIRECTION ( 'NONE',  ( -1.000000000000000000, -0.000000000000000000, -0.000000000000000000 ) ) ;
#61851 = CARTESIAN_POINT ( 'NONE',  ( 9.254569808101885897, -6.871911579029512218, 3.967499999999996252 ) ) ;
#61852 = ADVANCED_FACE ( 'NONE', ( #82096 ), #126970, .F. ) ;
#61853 = DIRECTION ( 'NONE',  ( -0.7071067811865486830, -0.7071067811865464625, -0.000000000000000000 ) ) ;
#61854 = ORIENTED_EDGE ( 'NONE', *, *, #112766, .F. ) ;
#61855 = DIRECTION ( 'NONE',  ( 1.000000000000000000, 0.000000000000000000, 0.000000000000000000 ) ) ;
#61856 = AXIS2_PLACEMENT_3D ( 'NONE', #43954, #141096, #8410 ) ;
#61857 = EDGE_CURVE ( 'NONE', #110059, #107725, #118461, .T. ) ;
#61858 = DIRECTION ( 'NONE',  ( -1.000000000000000000, -1.224606353822377258E-16, -0.000000000000000000 ) ) ;
#61859 = DIRECTION ( 'NONE',  ( 1.000000000000000000, 1.224606353822377258E-16, 0.000000000000000000 ) ) ;
#61861 = EDGE_LOOP ( 'NONE', ( #94171, #122202, #44140, #6740 ) ) ;
#61860 = DIRECTION ( 'NONE',  ( 0.7071067811865487940, 0.7071067811865463515, 0.000000000000000000 ) ) ;
#61862 = FACE_OUTER_BOUND ( 'NONE', #75554, .T. ) ;
#61863 = ORIENTED_EDGE ( 'NONE', *, *, #2387, .T. ) ;
#61864 = CARTESIAN_POINT ( 'NONE',  ( -24.70710678118636494, -3.740707523384241728, 5.000000000000000000 ) ) ;
#61865 = CARTESIAN_POINT ( 'NONE',  ( 23.99999999999983302, -12.41253812416062274, 4.000000000000000000 ) ) ;
#61866 = EDGE_CURVE ( 'NONE', #5681, #43625, #5170, .T. ) ;
#61867 = EDGE_CURVE ( 'NONE', #80457, #73777, #139327, .T. ) ;
#61868 = LINE ( 'NONE', #106025, #91066 ) ;
#61869 = ORIENTED_EDGE ( 'NONE', *, *, #33403, .F. ) ;
#61870 = CARTESIAN_POINT ( 'NONE',  ( 6.793339364578431017, 21.75929247661549226, 4.998822639870705409 ) ) ;
#61871 = CARTESIAN_POINT ( 'NONE',  ( -24.48921356237309510, -27.52281430457072631, 5.000000000000000000 ) ) ;
#61872 = FACE_OUTER_BOUND ( 'NONE', #40457, .T. ) ;
#61873 = ORIENTED_EDGE ( 'NONE', *, *, #2716, .T. ) ;
#61874 = FACE_OUTER_BOUND ( 'NONE', #127702, .T. ) ;
#61875 = DIRECTION ( 'NONE',  ( -1.000000000000000000, -0.000000000000000000, -0.000000000000000000 ) ) ;
#61876 = PLANE ( 'NONE',  #58569 ) ;
#61877 = DIRECTION ( 'NONE',  ( -0.7071067811865486830, 0.7071067811865464625, 0.000000000000000000 ) ) ;
#61878 = ADVANCED_FACE ( 'NONE', ( #30545 ), #84908, .T. ) ;
#61879 = CARTESIAN_POINT ( 'NONE',  ( -27.32816939922334143, -0.7407075233842683737, 4.000000000000000000 ) ) ;
#61880 = ORIENTED_EDGE ( 'NONE', *, *, #120898, .F. ) ;
#61881 = EDGE_CURVE ( 'NONE', #17782, #89560, #47701, .T. ) ;
#61882 = VERTEX_POINT ( 'NONE', #76188 ) ;
#61883 = DIRECTION ( 'NONE',  ( 0.000000000000000000, -1.000000000000000000, 0.000000000000000000 ) ) ;
#61884 = CARTESIAN_POINT ( 'NONE',  ( 0.7999687798316279519, 8.259292476615634371, 16.85664084051840916 ) ) ;
#61885 = VECTOR ( 'NONE', #53700, 1000.000000000000000 ) ;
#61886 = AXIS2_PLACEMENT_3D ( 'NONE', #44138, #10057, #54324 ) ;
#61887 = CARTESIAN_POINT ( 'NONE',  ( 2.166236474768552966, 7.934999999999990727, -1.457635852685135314E-15 ) ) ;
#61888 = FACE_OUTER_BOUND ( 'NONE', #12824, .T. ) ;
#61889 = AXIS2_PLACEMENT_3D ( 'NONE', #124142, #81389, #24827 ) ;
#61890 = DIRECTION ( 'NONE',  ( -0.7071067811865487940, 0.7071067811865463515, -0.000000000000000000 ) ) ;
#61891 = ADVANCED_FACE ( 'NONE', ( #53733 ), #95780, .F. ) ;
#61892 = DIRECTION ( 'NONE',  ( 1.000000000000000000, 0.000000000000000000, 0.000000000000000000 ) ) ;
#61893 = ORIENTED_EDGE ( 'NONE', *, *, #70651, .F. ) ;
#61894 = PLANE ( 'NONE',  #71957 ) ;
#61895 = LINE ( 'NONE', #28544, #99869 ) ;
#61896 = LINE ( 'NONE', #118373, #5317 ) ;
#61897 = VECTOR ( 'NONE', #22651, 1000.000000000000000 ) ;
#61898 = EDGE_CURVE ( 'NONE', #13412, #110421, #9453, .T. ) ;
#61899 = DIRECTION ( 'NONE',  ( 1.000000000000000000, 0.000000000000000000, 0.000000000000000000 ) ) ;
#61900 = CARTESIAN_POINT ( 'NONE',  ( 50.80793019189810167, -6.109999999999999432, 1.637169565754158507 ) ) ;
#61901 = CARTESIAN_POINT ( 'NONE',  ( -7.140000000000001457, -39.92999999999999261, -39.50000000000000000 ) ) ;
#61902 = VERTEX_POINT ( 'NONE', #118957 ) ;
#61903 = LINE ( 'NONE', #95208, #81375 ) ;
#61904 = VERTEX_POINT ( 'NONE', #63891 ) ;
#61905 = VERTEX_POINT ( 'NONE', #108054 ) ;
#61906 = EDGE_CURVE ( 'NONE', #83991, #81813, #18185, .T. ) ;
#61907 = DIRECTION ( 'NONE',  ( 0.000000000000000000, 0.000000000000000000, -1.000000000000000000 ) ) ;
#61908 =( BOUNDED_CURVE ( )  B_SPLINE_CURVE ( 2, ( #69886, #126356, #116204, #114746, #105316, #116909, #138689, #103865, #48821, #16894, #103178, #36503, #27045 ),
 .UNSPECIFIED., .F., .T. ) 
 B_SPLINE_CURVE_WITH_KNOTS ( ( 3, 2, 2, 2, 2, 2, 3 ),
 ( 0.9166666666666666297, 0.9194444444444443976, 0.9222222222222222765, 0.9250000000000000444, 0.9277777777777778123, 0.9305555555555555802, 0.9333333333333333481 ),
 .UNSPECIFIED. ) 
 CURVE ( )  GEOMETRIC_REPRESENTATION_ITEM ( )  RATIONAL_B_SPLINE_CURVE ( ( 1.000000000000000000, 0.9659258262890683122, 1.000000000000000000, 0.9659258262890683122, 1.000000000000000000, 0.9659258262890683122, 1.000000000000000000, 0.9659258262890683122, 1.000000000000000000, 0.9659258262890683122, 1.000000000000000000, 0.9659258262890683122, 1.000000000000000000 ) ) 
 REPRESENTATION_ITEM ( '' )  );
#61909 = LINE ( 'NONE', #140848, #80837 ) ;
#61910 = CARTESIAN_POINT ( 'NONE',  ( 34.92499999999998295, 22.22500000000000142, 4.500000000000000888 ) ) ;
#61911 = PLANE ( 'NONE',  #13958 ) ;
#61912 = DIRECTION ( 'NONE',  ( -0.000000000000000000, -0.000000000000000000, 1.000000000000000000 ) ) ;
#61913 = CARTESIAN_POINT ( 'NONE',  ( 10.64583333333333393, -1.633150327867700202, 6.094999999999985540 ) ) ;
#61914 = ORIENTED_EDGE ( 'NONE', *, *, #27960, .F. ) ;
#61915 = EDGE_CURVE ( 'NONE', #74246, #126135, #18933, .T. ) ;
#61916 = LINE ( 'NONE', #8187, #9352 ) ;
#61917 = DIRECTION ( 'NONE',  ( 0.7071067811865487940, 0.7071067811865463515, -0.000000000000000000 ) ) ;
#61919 = EDGE_CURVE ( 'NONE', #82657, #79851, #118226, .T. ) ;
#61918 = VECTOR ( 'NONE', #67005, 1000.000000000000000 ) ;
#61920 = DIRECTION ( 'NONE',  ( -0.6830127018922181881, 0.6830127018922202975, -0.2588190451025214056 ) ) ;
#61921 = FILL_AREA_STYLE_COLOUR ( '', #36286 ) ;
#61922 = DIRECTION ( 'NONE',  ( -1.000000000000000000, -1.224606353822377258E-16, -0.000000000000000000 ) ) ;
#61923 = CARTESIAN_POINT ( 'NONE',  ( -28.49999999999980460, -2.568876922607784774, 4.000000000000000000 ) ) ;
#61924 = CARTESIAN_POINT ( 'NONE',  ( 62.05836038379622011, -7.949999999999997513, -2.130196079827425759 ) ) ;
#61925 = EDGE_CURVE ( 'NONE', #113156, #68517, #53816, .T. ) ;
#61926 = VECTOR ( 'NONE', #114444, 1000.000000000000000 ) ;
#61927 = CARTESIAN_POINT ( 'NONE',  ( -3.516654386410431599, 22.22500000000000142, 4.500000000000000888 ) ) ;
#61928 = ORIENTED_EDGE ( 'NONE', *, *, #96054, .T. ) ;
#61929 = ORIENTED_EDGE ( 'NONE', *, *, #40357, .F. ) ;
#61930 = CARTESIAN_POINT ( 'NONE',  ( 59.77083333333332860, -7.949999999999999289, -2.130196079827426203 ) ) ;
#61931 = DIRECTION ( 'NONE',  ( 0.000000000000000000, -1.000000000000000000, 0.000000000000000000 ) ) ;
#61932 = DIRECTION ( 'NONE',  ( -0.7071067811865486830, -0.7071067811865464625, 0.000000000000000000 ) ) ;
#61933 = VECTOR ( 'NONE', #37522, 1000.000000000000000 ) ;
#61934 = CARTESIAN_POINT ( 'NONE',  ( -14.99451991528749595, 28.92564299267948513, 4.000000000000000000 ) ) ;
#61935 = ORIENTED_EDGE ( 'NONE', *, *, #99420, .T. ) ;
#61936 = EDGE_CURVE ( 'NONE', #93683, #134564, #64589, .T. ) ;
#61937 = CARTESIAN_POINT ( 'NONE',  ( 0.4892135623730947680, -27.52281430457055578, 5.000000000000000000 ) ) ;
#61938 = LINE ( 'NONE', #83698, #81410 ) ;
#61939 = CARTESIAN_POINT ( 'NONE',  ( 55.27126352523143282, 4.472830434245839371, 4.472830434245842035 ) ) ;
#61940 = ORIENTED_EDGE ( 'NONE', *, *, #29127, .F. ) ;
#61941 = VECTOR ( 'NONE', #45010, 1000.000000000000000 ) ;
#61942 = DIRECTION ( 'NONE',  ( -0.3543493200069162685, -0.000000000000000000, -0.9351131265310288487 ) ) ;
#61943 = EDGE_LOOP ( 'NONE', ( #113075, #119475, #52196, #142438 ) ) ;
#61944 = EDGE_LOOP ( 'NONE', ( #19869, #1422, #125221, #33047 ) ) ;
#61945 = FACE_OUTER_BOUND ( 'NONE', #98764, .T. ) ;
#61946 = DIRECTION ( 'NONE',  ( -0.7071067811865487940, 0.7071067811865463515, -0.000000000000000000 ) ) ;
#61947 = PLANE ( 'NONE',  #139277 ) ;
#61948 = VECTOR ( 'NONE', #89767, 1000.000000000000227 ) ;
#61949 = LINE ( 'NONE', #126447, #71821 ) ;
#61950 = CARTESIAN_POINT ( 'NONE',  ( 57.18398860626899705, 28.73617430169827358, 5.000000000000000000 ) ) ;
#61952 = VERTEX_POINT ( 'NONE', #8037 ) ;
#61951 = CARTESIAN_POINT ( 'NONE',  ( 99.82919371712955581, -3.975000000000001865, 6.884901960086284411 ) ) ;
#61953 = CARTESIAN_POINT ( 'NONE',  ( 20.19999999999999929, 2.055000000000001492, 2.516649172247811554E-16 ) ) ;
#61954 = DIRECTION ( 'NONE',  ( 0.2400000000000085398, -0.000000000000000000, 0.9707728879609256456 ) ) ;
#61955 = DIRECTION ( 'NONE',  ( -1.000000000000000000, -1.224606353822377258E-16, -0.000000000000000000 ) ) ;
#61956 = ORIENTED_EDGE ( 'NONE', *, *, #110691, .T. ) ;
#61957 = ORIENTED_EDGE ( 'NONE', *, *, #45413, .T. ) ;
#61958 = AXIS2_PLACEMENT_3D ( 'NONE', #105969, #60387, #5235 ) ;
#61959 = DIRECTION ( 'NONE',  ( 0.000000000000000000, -0.000000000000000000, -1.000000000000000000 ) ) ;
#61960 = DIRECTION ( 'NONE',  ( 0.3543493200069162685, -0.000000000000000000, -0.9351131265310288487 ) ) ;
#61961 = CARTESIAN_POINT ( 'NONE',  ( -34.49999999999974420, -20.94567065516883275, 4.994342998332162331 ) ) ;
#61962 = ADVANCED_FACE ( 'NONE', ( #96461 ), #140703, .F. ) ;
#61963 = VECTOR ( 'NONE', #11041, 1000.000000000000000 ) ;
#61964 = DIRECTION ( 'NONE',  ( 0.3543493200069164351, 2.781805975412904658E-17, -0.9351131265310288487 ) ) ;
#61965 = CARTESIAN_POINT ( 'NONE',  ( 71.82919371712957002, -3.975000000000001865, 6.884901960086284411 ) ) ;
#61966 = ORIENTED_EDGE ( 'NONE', *, *, #128395, .F. ) ;
#61967 = EDGE_LOOP ( 'NONE', ( #23054, #52941, #50554, #14369 ) ) ;
#61968 = LINE ( 'NONE', #38068, #70108 ) ;
#61969 = CARTESIAN_POINT ( 'NONE',  ( -34.42500000000001137, 8.977185695429334089, 5.000000000000000000 ) ) ;
#61970 = ORIENTED_EDGE ( 'NONE', *, *, #91994, .T. ) ;
#61971 = VERTEX_POINT ( 'NONE', #97934 ) ;
#61972 = CARTESIAN_POINT ( 'NONE',  ( 22.63753812416082667, 22.22500000000000142, 4.000000000000000000 ) ) ;
#61973 = ORIENTED_EDGE ( 'NONE', *, *, #137370, .F. ) ;
#61974 = CARTESIAN_POINT ( 'NONE',  ( 62.78752705046289151, 0.000000000000000000, -7.949999999999998401 ) ) ;
#61975 = CARTESIAN_POINT ( 'NONE',  ( 34.92499999999997584, 4.800094516027123781, 4.759050581649322709 ) ) ;
#61976 = AXIS2_PLACEMENT_3D ( 'NONE', #126025, #26698, #104224 ) ;
#61977 = CIRCLE ( 'NONE', #68919, 5.968999999999998529 ) ;
#61978 = ADVANCED_FACE ( 'NONE', ( #131272 ), #31959, .F. ) ;
#61979 = FACE_BOUND ( 'NONE', #63458, .T. ) ;
#61980 = LINE ( 'NONE', #40234, #59482 ) ;
#61981 = DIRECTION ( 'NONE',  ( -0.3543493200069163240, -0.000000000000000000, -0.9351131265310288487 ) ) ;
#61982 = ADVANCED_FACE ( 'NONE', ( #85605 ), #134860, .T. ) ;
#61983 = LINE ( 'NONE', #3448, #142891 ) ;
#61985 = EDGE_LOOP ( 'NONE', ( #52258, #52379 ) ) ;
#61984 = CARTESIAN_POINT ( 'NONE',  ( -66.48921356237309510, -27.52281430457101763, 5.000000000000000000 ) ) ;
#61986 = CONICAL_SURFACE ( 'NONE', #117506, 2.055000000000001048, 0.9599310885968758145 ) ;
#61988 = AXIS2_PLACEMENT_3D ( 'NONE', #58211, #12496, #56778 ) ;
#61987 = VECTOR ( 'NONE', #87817, 1000.000000000000000 ) ;
#61989 = CARTESIAN_POINT ( 'NONE',  ( 2.999999999999981792, 4.384688058510572972, -7.090945410444678743 ) ) ;
#61990 =( NAMED_UNIT ( * ) SI_UNIT ( $, .STERADIAN. ) SOLID_ANGLE_UNIT ( ) );
#61991 = VERTEX_POINT ( 'NONE', #40016 ) ;
#61992 = VECTOR ( 'NONE', #63732, 1000.000000000000000 ) ;
#61993 = ORIENTED_EDGE ( 'NONE', *, *, #78718, .F. ) ;
#61994 = CARTESIAN_POINT ( 'NONE',  ( 92.95376352523145158, -6.109999999999998543, -3.741295971395162543E-16 ) ) ;
#61995 = ORIENTED_EDGE ( 'NONE', *, *, #134644, .F. ) ;
#61996 = DIRECTION ( 'NONE',  ( 1.000000000000000000, 0.000000000000000000, 0.000000000000000000 ) ) ;
#61997 = EDGE_CURVE ( 'NONE', #41151, #115678, #129843, .T. ) ;
#61998 = LINE ( 'NONE', #126493, #118334 ) ;
#61999 = LINE ( 'NONE', #141687, #18929 ) ;
#62000 = EDGE_CURVE ( 'NONE', #63781, #121984, #106913, .T. ) ;
#62001 = FACE_OUTER_BOUND ( 'NONE', #11460, .T. ) ;
#62002 = ORIENTED_EDGE ( 'NONE', *, *, #23717, .F. ) ;
#62003 = DIRECTION ( 'NONE',  ( 0.000000000000000000, 0.000000000000000000, 1.000000000000000000 ) ) ;
#62004 = DIRECTION ( 'NONE',  ( -0.7071067811865487940, 0.7071067811865463515, 0.000000000000000000 ) ) ;
#62005 = CARTESIAN_POINT ( 'NONE',  ( -6.793339364578430128, 21.75929247661548871, 4.998822639870703632 ) ) ;
#62006 = CARTESIAN_POINT ( 'NONE',  ( -42.18398860626899705, 28.73617430169816700, 5.000000000000000000 ) ) ;
#62007 = DIRECTION ( 'NONE',  ( -1.000000000000000000, -1.224606353822377258E-16, -0.000000000000000000 ) ) ;
#62008 = EDGE_CURVE ( 'NONE', #96838, #18115, #51586, .T. ) ;
#62009 = DIRECTION ( 'NONE',  ( -0.6830127018922181881, 0.6830127018922202975, -0.2588190451025214056 ) ) ;
#62010 = EDGE_LOOP ( 'NONE', ( #136378, #135548, #6109, #83618 ) ) ;
#62011 = CARTESIAN_POINT ( 'NONE',  ( -15.29974487139158867, -27.71228299555216879, 4.000000000000000000 ) ) ;
#62012 = CARTESIAN_POINT ( 'NONE',  ( 42.48921356237308800, -27.52281430457085065, 5.000000000000000000 ) ) ;
#62013 = VERTEX_POINT ( 'NONE', #132001 ) ;
#62014 = EDGE_LOOP ( 'NONE', ( #79832, #24493, #80149, #103625 ) ) ;
#62015 = ORIENTED_EDGE ( 'NONE', *, *, #43829, .T. ) ;
#62016 = CARTESIAN_POINT ( 'NONE',  ( 43.75043019189810423, 3.055000000000002824, -5.291415217122919401 ) ) ;
#62017 = VECTOR ( 'NONE', #50401, 999.9999999999998863 ) ;
#62018 = EDGE_CURVE ( 'NONE', #80143, #107445, #112383, .T. ) ;
#62019 = ORIENTED_EDGE ( 'NONE', *, *, #54303, .F. ) ;
#62020 = VECTOR ( 'NONE', #131182, 999.9999999999998863 ) ;
#62021 = CARTESIAN_POINT ( 'NONE',  ( 11.42080628287044064, 3.047499999999997655, 5.278424836066143655 ) ) ;
#62022 =( BOUNDED_CURVE ( )  B_SPLINE_CURVE ( 3, ( #106759, #63315, #142967, #74155 ),
 .UNSPECIFIED., .F., .T. ) 
 B_SPLINE_CURVE_WITH_KNOTS ( ( 4, 4 ),
 ( 4.350170835173026163, 4.500739107949210727 ),
 .UNSPECIFIED. ) 
 CURVE ( )  GEOMETRIC_REPRESENTATION_ITEM ( )  RATIONAL_B_SPLINE_CURVE ( ( 1.000000000000000000, 0.9981116584018956406, 0.9981116584018956406, 1.000000000000000000 ) ) 
 REPRESENTATION_ITEM ( '' )  );
#62023 = CARTESIAN_POINT ( 'NONE',  ( -9.209127552564122965, 9.981455117011716283, -26.96467221759983346 ) ) ;
#62024 = ORIENTED_EDGE ( 'NONE', *, *, #73537, .F. ) ;
#62025 = CARTESIAN_POINT ( 'NONE',  ( 18.63311396761903538, -2.779424156541560276, 4.000000000000000000 ) ) ;
#62026 = EDGE_CURVE ( 'NONE', #41817, #126052, #109517, .T. ) ;
#62027 = ORIENTED_EDGE ( 'NONE', *, *, #51874, .T. ) ;
#62028 = CARTESIAN_POINT ( 'NONE',  ( -24.79593897580385331, 4.791522900035168675, 4.000000000000000000 ) ) ;
#62029 = CARTESIAN_POINT ( 'NONE',  ( 34.49999999999975842, -2.945670655169024155, 4.994342998332159667 ) ) ;
#62031 = EDGE_LOOP ( 'NONE', ( #142196, #105894, #110656, #120132, #65207, #62475, #129396, #40061 ) ) ;
#62030 = DIRECTION ( 'NONE',  ( -0.7071067811865486830, 0.7071067811865464625, 0.000000000000000000 ) ) ;
#62032 = ORIENTED_EDGE ( 'NONE', *, *, #40989, .F. ) ;
#62033 = CARTESIAN_POINT ( 'NONE',  ( -11.51078643762690490, -27.52281430457047406, 5.000000000000000000 ) ) ;
#62034 = DIRECTION ( 'NONE',  ( 0.000000000000000000, -1.000000000000000000, 0.000000000000000000 ) ) ;
#62035 = EDGE_CURVE ( 'NONE', #78067, #73712, #43548, .T. ) ;
#62036 = EDGE_CURVE ( 'NONE', #135574, #111361, #9805, .T. ) ;
#62037 = ORIENTED_EDGE ( 'NONE', *, *, #77957, .T. ) ;
#62038 = DIRECTION ( 'NONE',  ( -0.000000000000000000, 0.3543493200069153248, 0.9351131265310292928 ) ) ;
#62039 = ORIENTED_EDGE ( 'NONE', *, *, #37742, .F. ) ;
#62040 = ORIENTED_EDGE ( 'NONE', *, *, #97011, .F. ) ;
#62041 = VERTEX_POINT ( 'NONE', #121797 ) ;
#62042 = ORIENTED_EDGE ( 'NONE', *, *, #98556, .F. ) ;
#62043 = CARTESIAN_POINT ( 'NONE',  ( 15.48921356237309510, -27.52281430457066236, 5.000000000000000000 ) ) ;
#62044 = EDGE_CURVE ( 'NONE', #109094, #118163, #44636, .T. ) ;
#62045 = LINE ( 'NONE', #72236, #51633 ) ;
#62046 = CARTESIAN_POINT ( 'NONE',  ( 3.469446951953614189E-15, -12.03360074219761700, 5.000000000000000000 ) ) ;
#62047 = EDGE_CURVE ( 'NONE', #59037, #94354, #54455, .T. ) ;
#62048 = CARTESIAN_POINT ( 'NONE',  ( 23.99999999999981881, -13.39766691384881803, -10.96608748226471697 ) ) ;
#62049 = VERTEX_POINT ( 'NONE', #120348 ) ;
#62050 = EDGE_CURVE ( 'NONE', #79253, #46769, #68207, .T. ) ;
#62051 = LINE ( 'NONE', #6883, #129994 ) ;
#62052 = VERTEX_POINT ( 'NONE', #34116 ) ;
#62053 = DIRECTION ( 'NONE',  ( -0.000000000000000000, -0.3543493200069152693, 0.9351131265310292928 ) ) ;
#62054 = DIRECTION ( 'NONE',  ( 1.000000000000000000, 0.000000000000000000, 0.000000000000000000 ) ) ;
#62055 = LINE ( 'NONE', #5479, #34632 ) ;
#62056 = ORIENTED_EDGE ( 'NONE', *, *, #98301, .F. ) ;
#62057 = DIRECTION ( 'NONE',  ( -0.7071067811865487940, 0.7071067811865463515, -0.000000000000000000 ) ) ;
#62058 = VECTOR ( 'NONE', #124022, 1000.000000000000000 ) ;
#62059 = EDGE_CURVE ( 'NONE', #69770, #84967, #101489, .T. ) ;
#62060 = CARTESIAN_POINT ( 'NONE',  ( -34.25456027042017837, 22.27000000000000668, -12.45996461598220506 ) ) ;
#62061 = ORIENTED_EDGE ( 'NONE', *, *, #2759, .F. ) ;
#62062 = ORIENTED_EDGE ( 'NONE', *, *, #35654, .T. ) ;
#62063 = VERTEX_POINT ( 'NONE', #57314 ) ;
#62064 = DIRECTION ( 'NONE',  ( -0.000000000000000000, 0.000000000000000000, 1.000000000000000000 ) ) ;
#62065 = DIRECTION ( 'NONE',  ( -0.3543493200069162685, -0.000000000000000000, -0.9351131265310288487 ) ) ;
#62066 = CARTESIAN_POINT ( 'NONE',  ( 1.629999999999999893, 0.4000000000000001887, -2.500000000000000000 ) ) ;
#62067 = EDGE_CURVE ( 'NONE', #98083, #109689, #110912, .T. ) ;
#62068 = CARTESIAN_POINT ( 'NONE',  ( 0.1679803408763183847, -48.55783623716211395, -38.28685941347502819 ) ) ;
#62069 = CARTESIAN_POINT ( 'NONE',  ( 76.03709685856478018, -3.054999999999999272, -5.291415217122919401 ) ) ;
#62070 = LINE ( 'NONE', #4029, #34881 ) ;
#62071 = CARTESIAN_POINT ( 'NONE',  ( 0.000000000000000000, 0.000000000000000000, 5.000000000000000000 ) ) ;
#62072 = LINE ( 'NONE', #141021, #20990 ) ;
#62073 = DIRECTION ( 'NONE',  ( -0.7071067811865487940, 0.7071067811865463515, 0.000000000000000000 ) ) ;
#62074 = LINE ( 'NONE', #51186, #44179 ) ;
#62075 = ORIENTED_EDGE ( 'NONE', *, *, #57881, .F. ) ;
#62076 = CARTESIAN_POINT ( 'NONE',  ( 19.93618820068612152, -3.269999999999996909, -36.05349808876643181 ) ) ;
#62077 = ORIENTED_EDGE ( 'NONE', *, *, #70327, .T. ) ;
#62078 = AXIS2_PLACEMENT_3D ( 'NONE', #37410, #125861, #26532 ) ;
#62079 = CARTESIAN_POINT ( 'NONE',  ( 32.99999999999976552, 9.631307414974347836, -9.079085613539465527 ) ) ;
#62081 = ORIENTED_EDGE ( 'NONE', *, *, #15872, .T. ) ;
#62080 = DIRECTION ( 'NONE',  ( 1.000000000000000000, -0.000000000000000000, -0.000000000000000000 ) ) ;
#62082 = VECTOR ( 'NONE', #90125, 1000.000000000000000 ) ;
#62083 = CARTESIAN_POINT ( 'NONE',  ( 3.156123077392388065, -22.22500000000000142, 4.000000000000000000 ) ) ;
#62084 = DIRECTION ( 'NONE',  ( -0.3543493200069162685, -0.000000000000000000, -0.9351131265310288487 ) ) ;
#62085 = ORIENTED_EDGE ( 'NONE', *, *, #122030, .F. ) ;
#62086 = EDGE_LOOP ( 'NONE', ( #128714, #132849, #5606, #141594 ) ) ;
#62087 = CARTESIAN_POINT ( 'NONE',  ( -33.48921356237309510, -27.52281430457078670, 5.000000000000000000 ) ) ;
#62088 = DIRECTION ( 'NONE',  ( 0.000000000000000000, -1.000000000000000000, 0.000000000000000000 ) ) ;
#62089 = VECTOR ( 'NONE', #42580, 1000.000000000000000 ) ;
#62090 = VECTOR ( 'NONE', #11480, 1000.000000000000227 ) ;
#62091 = DIRECTION ( 'NONE',  ( -0.3543493200069163240, 4.681814790819596721E-17, -0.9351131265310288487 ) ) ;
#62092 = EDGE_CURVE ( 'NONE', #27734, #119393, #130184, .T. ) ;
#62093 = CARTESIAN_POINT ( 'NONE',  ( 96.03752705046289861, -9.735942053221456900E-16, 7.949999999999998401 ) ) ;
#62094 = CARTESIAN_POINT ( 'NONE',  ( 19.41999999999999815, 2.055000000000001492, 0.000000000000000000 ) ) ;
#62095 = CARTESIAN_POINT ( 'NONE',  ( 25.82816939922335209, -14.24070752338412937, 4.000000000000000000 ) ) ;
#62096 = ORIENTED_EDGE ( 'NONE', *, *, #131237, .T. ) ;
#62097 = CARTESIAN_POINT ( 'NONE',  ( 25.39999999999999858, -16.48000000000005016, 33.92499999999998295 ) ) ;
#62098 = LINE ( 'NONE', #38200, #4375 ) ;
#62099 = CARTESIAN_POINT ( 'NONE',  ( 30.04166666666666785, 3.047499999999993214, -5.278424836066146320 ) ) ;
#62100 = DIRECTION ( 'NONE',  ( 0.7071067811865487940, -0.7071067811865463515, 0.000000000000000000 ) ) ;
#62101 = ORIENTED_EDGE ( 'NONE', *, *, #49876, .F. ) ;
#62102 = CARTESIAN_POINT ( 'NONE',  ( 22.41489890804854568, -1.755427004171022709, 4.190031470807595859 ) ) ;
#62103 = ORIENTED_EDGE ( 'NONE', *, *, #66247, .F. ) ;
#62104 = CARTESIAN_POINT ( 'NONE',  ( 89.39626352523144703, 4.472830434245840259, -4.472830434245839371 ) ) ;
#62105 = CARTESIAN_POINT ( 'NONE',  ( 5.281315875828549444, 4.584330080086930965E-16, 0.000000000000000000 ) ) ;
#62106 = CARTESIAN_POINT ( 'NONE',  ( -4.069960254864057880, -0.7407075233842770334, 13.87443053587611708 ) ) ;
#62107 = CARTESIAN_POINT ( 'NONE',  ( -36.29974487139159578, -27.71228299555231445, 4.000000000000000000 ) ) ;
#62108 = EDGE_LOOP ( 'NONE', ( #132879, #126158, #2593, #105433 ) ) ;
#62109 = DIRECTION ( 'NONE',  ( 0.000000000000000000, 0.000000000000000000, 1.000000000000000000 ) ) ;
#62110 = CARTESIAN_POINT ( 'NONE',  ( -34.92500000000001137, 22.22500000000000142, 4.000000000000000000 ) ) ;
#62111 = DIRECTION ( 'NONE',  ( -0.7071067811865486830, -0.7071067811865464625, 0.000000000000000000 ) ) ;
#62113 = ORIENTED_EDGE ( 'NONE', *, *, #3822, .F. ) ;
#62112 = PLANE ( 'NONE',  #137806 ) ;
#62115 = VECTOR ( 'NONE', #49707, 1000.000000000000227 ) ;
#62114 = DIRECTION ( 'NONE',  ( 0.7071067811865487940, 0.7071067811865463515, -0.000000000000000000 ) ) ;
#62116 = CARTESIAN_POINT ( 'NONE',  ( 10.03163515922185844, 2.259292476615701428, 13.77329220150639522 ) ) ;
#62117 = DIRECTION ( 'NONE',  ( -1.000000000000000000, -0.000000000000000000, -0.000000000000000000 ) ) ;
#62118 = CARTESIAN_POINT ( 'NONE',  ( -57.18398860626899705, 28.73617430169827358, 5.000000000000000000 ) ) ;
#62119 = ORIENTED_EDGE ( 'NONE', *, *, #44779, .F. ) ;
#62120 = ORIENTED_EDGE ( 'NONE', *, *, #23410, .T. ) ;
#62121 = CARTESIAN_POINT ( 'NONE',  ( 73.50043019189811844, -3.055000000000002380, 5.291415217122920289 ) ) ;
#62122 = ORIENTED_EDGE ( 'NONE', *, *, #127417, .F. ) ;
#62123 = LINE ( 'NONE', #104148, #68301 ) ;
#62124 = EDGE_CURVE ( 'NONE', #50272, #61349, #65336, .T. ) ;
#62125 = LINE ( 'NONE', #18569, #101293 ) ;
#62126 = CARTESIAN_POINT ( 'NONE',  ( -5.510786437626906675, -27.52281430457051314, 5.000000000000000000 ) ) ;
#62127 = ORIENTED_EDGE ( 'NONE', *, *, #91107, .F. ) ;
#62128 = VECTOR ( 'NONE', #108657, 1000.000000000000000 ) ;
#62129 = CARTESIAN_POINT ( 'NONE',  ( 0.000000000000000000, 0.000000000000000000, 5.000000000000000000 ) ) ;
#62130 = LINE ( 'NONE', #83903, #81429 ) ;
#62131 = STYLED_ITEM ( 'NONE', ( #123598 ), #38134 ) ;
#62132 = ADVANCED_FACE ( 'NONE', ( #99329 ), #98630, .F. ) ;
#62133 = ORIENTED_EDGE ( 'NONE', *, *, #17903, .F. ) ;
#62134 = CARTESIAN_POINT ( 'NONE',  ( -42.18398860626899705, 28.73617430169816700, 5.000000000000000000 ) ) ;
#62135 = CARTESIAN_POINT ( 'NONE',  ( 0.000000000000000000, 0.000000000000000000, 5.000000000000000000 ) ) ;
#62136 = DIRECTION ( 'NONE',  ( -0.000000000000000000, 0.3543493200069153248, 0.9351131265310292928 ) ) ;
#62137 = ORIENTED_EDGE ( 'NONE', *, *, #21118, .F. ) ;
#62138 = ORIENTED_EDGE ( 'NONE', *, *, #75562, .F. ) ;
#62139 = EDGE_CURVE ( 'NONE', #22706, #7595, #77628, .T. ) ;
#62140 = ADVANCED_FACE ( 'NONE', ( #134142 ), #56389, .T. ) ;
#62141 = EDGE_CURVE ( 'NONE', #104460, #34275, #66044, .T. ) ;
#62142 = CARTESIAN_POINT ( 'NONE',  ( -57.29974487139158157, -27.71228299555246011, 4.000000000000000000 ) ) ;
#62143 = DIRECTION ( 'NONE',  ( 0.000000000000000000, 0.000000000000000000, -1.000000000000000000 ) ) ;
#62144 = LINE ( 'NONE', #138992, #11819 ) ;
#62145 = LINE ( 'NONE', #117892, #86054 ) ;
#62146 = DIRECTION ( 'NONE',  ( -0.000000000000000000, -0.3543493200069152138, 0.9351131265310292928 ) ) ;
#62147 = EDGE_CURVE ( 'NONE', #57540, #131273, #123261, .T. ) ;
#62148 = ADVANCED_FACE ( 'NONE', ( #111667 ), #91363, .F. ) ;
#62149 = CARTESIAN_POINT ( 'NONE',  ( 20.99999999999986855, 20.96639925780205616, 5.000000000000000000 ) ) ;
#62150 =( NAMED_UNIT ( * ) SI_UNIT ( $, .STERADIAN. ) SOLID_ANGLE_UNIT ( ) );
#62151 = EDGE_LOOP ( 'NONE', ( #21992, #46601, #20381, #34802 ) ) ;
#62152 = ORIENTED_EDGE ( 'NONE', *, *, #117610, .F. ) ;
#62153 = AXIS2_PLACEMENT_3D ( 'NONE', #132079, #53050, #131346 ) ;
#62154 = ORIENTED_EDGE ( 'NONE', *, *, #27763, .F. ) ;
#62155 = EDGE_CURVE ( 'NONE', #6816, #38440, #4250, .T. ) ;
#62156 = VERTEX_POINT ( 'NONE', #115904 ) ;
#62157 = CARTESIAN_POINT ( 'NONE',  ( 63.29974487139158867, -27.71228299555250274, 4.000000000000000000 ) ) ;
#62158 = EDGE_CURVE ( 'NONE', #131471, #83058, #47181, .T. ) ;
#62159 = ORIENTED_EDGE ( 'NONE', *, *, #90529, .F. ) ;
#62160 = FACE_OUTER_BOUND ( 'NONE', #83356, .T. ) ;
#62161 = DIRECTION ( 'NONE',  ( 1.000000000000000000, 0.000000000000000000, 0.000000000000000000 ) ) ;
#62162 = VECTOR ( 'NONE', #103717, 1000.000000000000000 ) ;
#62163 = DIRECTION ( 'NONE',  ( -0.000000000000000000, -0.3543493200069152693, 0.9351131265310292928 ) ) ;
#62164 = DIRECTION ( 'NONE',  ( -0.7071067811865486830, -0.7071067811865464625, -0.000000000000000000 ) ) ;
#62165 = AXIS2_PLACEMENT_3D ( 'NONE', #51286, #72357, #48412 ) ;
#62166 = AXIS2_PLACEMENT_3D ( 'NONE', #129763, #70625, #82205 ) ;
#62167 = LINE ( 'NONE', #106330, #137097 ) ;
#62168 = EDGE_LOOP ( 'NONE', ( #26504, #30713, #126703, #34982 ) ) ;
#62169 = FACE_OUTER_BOUND ( 'NONE', #131426, .T. ) ;
#62170 = DIRECTION ( 'NONE',  ( -0.6830127018922181881, 0.6830127018922202975, -0.2588190451025214056 ) ) ;
#62171 = CIRCLE ( 'NONE', #136244, 3.000000000000000888 ) ;
#62172 = ORIENTED_EDGE ( 'NONE', *, *, #71672, .F. ) ;
#62173 = DIRECTION ( 'NONE',  ( 0.7071067811865486830, -0.7071067811865464625, -0.000000000000000000 ) ) ;
#62174 = ORIENTED_EDGE ( 'NONE', *, *, #56140, .F. ) ;
#62175 = VECTOR ( 'NONE', #118718, 1000.000000000000000 ) ;
#62176 = DIRECTION ( 'NONE',  ( 0.7071067811865487940, 0.7071067811865463515, -0.000000000000000000 ) ) ;
#62177 = ORIENTED_EDGE ( 'NONE', *, *, #62155, .T. ) ;
#62178 = CARTESIAN_POINT ( 'NONE',  ( 75.39626352523141861, 4.472830434245840259, -4.472830434245838482 ) ) ;
#62179 = ADVANCED_FACE ( 'NONE', ( #82600 ), #60156, .T. ) ;
#62180 = AXIS2_PLACEMENT_3D ( 'NONE', #97833, #99980, #10789 ) ;
#62181 = ORIENTED_EDGE ( 'NONE', *, *, #7285, .F. ) ;
#62183 = VECTOR ( 'NONE', #69788, 999.9999999999998863 ) ;
#62182 = VECTOR ( 'NONE', #127, 1000.000000000000000 ) ;
#62184 = CARTESIAN_POINT ( 'NONE',  ( 104.4170968585647756, 3.054999999999998828, 5.291415217122922066 ) ) ;
#62185 = CARTESIAN_POINT ( 'NONE',  ( 23.00840764549667483, 9.139736423841732040E-16, 0.000000000000000000 ) ) ;
#62186 = DIRECTION ( 'NONE',  ( -0.6830127018922180770, -0.6830127018922204085, -0.2588190451025213501 ) ) ;
#62187 = ADVANCED_FACE ( 'NONE', ( #4988 ), #3576, .F. ) ;
#62188 = FACE_OUTER_BOUND ( 'NONE', #37079, .T. ) ;
#62189 = DIRECTION ( 'NONE',  ( 0.3543493200069162685, -0.000000000000000000, -0.9351131265310288487 ) ) ;
#62190 = VECTOR ( 'NONE', #40826, 1000.000000000000000 ) ;
#62191 = DIRECTION ( 'NONE',  ( -0.6830127018922181881, 0.6830127018922202975, -0.2588190451025214056 ) ) ;
#62192 = CARTESIAN_POINT ( 'NONE',  ( 23.99999999999983302, -10.77435723561691994, -9.972017380717284496 ) ) ;
#62194 = ADVANCED_FACE ( 'NONE', ( #104322 ), #102234, .F. ) ;
#62193 = DIRECTION ( 'NONE',  ( -1.000000000000000000, -0.000000000000000000, -0.000000000000000000 ) ) ;
#62195 = ORIENTED_EDGE ( 'NONE', *, *, #38779, .T. ) ;
#62196 = VECTOR ( 'NONE', #60860, 1000.000000000000000 ) ;
#62197 = CARTESIAN_POINT ( 'NONE',  ( -36.18398860626899705, 28.73617430169812437, 5.000000000000000000 ) ) ;
#62198 = B_SPLINE_CURVE_WITH_KNOTS ( 'NONE', 3,
 ( #132734, #9450, #52971, #141433, #108760, #31258, #20340, #66041, #142859, #54452 ),
 .UNSPECIFIED., .F., .F.,
 ( 4, 2, 2, 2, 4 ),
 ( 0.008920163802561175553, 0.009434751658411365260, 0.009949339514261554968, 0.01046392737011174294, 0.01097851522596193265 ),
 .UNSPECIFIED. ) ;
#62199 = VERTEX_POINT ( 'NONE', #137711 ) ;
#62200 = EDGE_CURVE ( 'NONE', #97682, #136003, #123978, .T. ) ;
#62201 = VERTEX_POINT ( 'NONE', #81929 ) ;
#62202 = CIRCLE ( 'NONE', #80733, 3.378199999999994319 ) ;
#62203 = CARTESIAN_POINT ( 'NONE',  ( 113.9750270504628844, -5.819803920172573086, 5.819803920172573086 ) ) ;
#62204 = ORIENTED_EDGE ( 'NONE', *, *, #91967, .F. ) ;
#62206 = ADVANCED_FACE ( 'NONE', ( #15175 ), #127236, .T. ) ;
#62205 = VECTOR ( 'NONE', #4934, 1000.000000000000000 ) ;
#62207 = DIRECTION ( 'NONE',  ( -0.6830127018922180770, -0.6830127018922204085, -0.2588190451025213501 ) ) ;
#62208 = DIRECTION ( 'NONE',  ( 0.7071067811865487940, 0.7071067811865463515, 0.000000000000000000 ) ) ;
#62209 =( GEOMETRIC_REPRESENTATION_CONTEXT ( 3 ) GLOBAL_UNCERTAINTY_ASSIGNED_CONTEXT ( ( #137328 ) ) GLOBAL_UNIT_ASSIGNED_CONTEXT ( ( #94250, #124745, #4317 ) ) REPRESENTATION_CONTEXT ( 'NONE', 'WORKASPACE' ) );
#62210 = DIRECTION ( 'NONE',  ( -1.000000000000000000, -1.224606353822377258E-16, -0.000000000000000000 ) ) ;
#62211 = DIRECTION ( 'NONE',  ( -0.000000000000000000, 0.000000000000000000, 1.000000000000000000 ) ) ;
#62212 = ORIENTED_EDGE ( 'NONE', *, *, #100311, .F. ) ;
#62213 = CARTESIAN_POINT ( 'NONE',  ( 0.01167931549069121423, -50.55966373066888053, 35.89041033429500516 ) ) ;
#62214 = ORIENTED_EDGE ( 'NONE', *, *, #80448, .T. ) ;
#62215 = VECTOR ( 'NONE', #114800, 1000.000000000000114 ) ;
#62216 = CARTESIAN_POINT ( 'NONE',  ( 1.437069808101885782, 2.126176841940952134, -7.934999999999993392 ) ) ;
#62217 = DIRECTION ( 'NONE',  ( 0.7071067811865486830, -0.7071067811865464625, -0.000000000000000000 ) ) ;
#62218 = DIRECTION ( 'NONE',  ( 0.7071067811865486830, -0.7071067811865464625, -0.000000000000000000 ) ) ;
#62219 = EDGE_CURVE ( 'NONE', #78214, #39230, #86173, .T. ) ;
#62220 = CARTESIAN_POINT ( 'NONE',  ( -9.299744871391588674, -27.71228299555212971, 4.000000000000000000 ) ) ;
#62221 = VERTEX_POINT ( 'NONE', #128952 ) ;
#62222 = ORIENTED_EDGE ( 'NONE', *, *, #19624, .F. ) ;
#62223 = EDGE_LOOP ( 'NONE', ( #133432, #26974, #12048, #26717 ) ) ;
#62224 = DIRECTION ( 'NONE',  ( 0.7071067811865487940, 0.7071067811865463515, 0.000000000000000000 ) ) ;
#62226 = VECTOR ( 'NONE', #3176, 1000.000000000000000 ) ;
#62225 = DIRECTION ( 'NONE',  ( -0.7071067811865486830, 0.7071067811865464625, 0.000000000000000000 ) ) ;
#62227 = CARTESIAN_POINT ( 'NONE',  ( 34.92499999999998295, 1.701930566820966773, 4.500000000000000888 ) ) ;
#62228 = AXIS2_PLACEMENT_3D ( 'NONE', #9600, #8850, #111049 ) ;
#62229 = CARTESIAN_POINT ( 'NONE',  ( 21.18398860626899349, 28.73617430169802134, 5.000000000000000000 ) ) ;
#62230 = CARTESIAN_POINT ( 'NONE',  ( -0.1839886062690032631, 28.73617430169787568, 5.000000000000000000 ) ) ;
#62231 = CARTESIAN_POINT ( 'NONE',  ( 24.48921356237309510, -27.52281430457072631, 5.000000000000000000 ) ) ;
#62232 = ADVANCED_FACE ( 'NONE', ( #64409 ), #62290, .F. ) ;
#62233 = B_SPLINE_CURVE_WITH_KNOTS ( 'NONE', 3,
 ( #11785, #66913, #110384, #45194, #33595, #111092, #121978, #122705, #108953, #79261, #22646, #76364, #132913, #120533 ),
 .UNSPECIFIED., .F., .F.,
 ( 4, 2, 2, 2, 2, 2, 4 ),
 ( 0.006237562923353405335, 0.006757314257999464183, 0.007277065592645523030, 0.007536941259968552020, 0.007796816927291581878, 0.008056692594614611735, 0.008316568261937639858 ),
 .UNSPECIFIED. ) ;
#62234 = CARTESIAN_POINT ( 'NONE',  ( -27.70710678118634718, -6.740707523384212863, 5.000000000000000000 ) ) ;
#62235 = FACE_OUTER_BOUND ( 'NONE', #94147, .T. ) ;
#62236 = ORIENTED_EDGE ( 'NONE', *, *, #37426, .T. ) ;
#62237 = DIRECTION ( 'NONE',  ( -0.000000000000000000, 0.3543493200069153248, 0.9351131265310292928 ) ) ;
#62238 = CARTESIAN_POINT ( 'NONE',  ( -6.489213562373093325, -27.52281430457059841, 5.000000000000000000 ) ) ;
#62239 = ORIENTED_EDGE ( 'NONE', *, *, #93, .T. ) ;
#62240 = LINE ( 'NONE', #40493, #78448 ) ;
#62243 = EDGE_CURVE ( 'NONE', #23479, #72219, #19476, .T. ) ;
#62242 = ORIENTED_EDGE ( 'NONE', *, *, #80724, .T. ) ;
#62241 = LINE ( 'NONE', #7082, #122892 ) ;
#62244 = CARTESIAN_POINT ( 'NONE',  ( -5.999999999999956479, 4.384688058510558761, -7.090945410444697394 ) ) ;
#62245 = EDGE_CURVE ( 'NONE', #20046, #36553, #140530, .T. ) ;
#62246 = ORIENTED_EDGE ( 'NONE', *, *, #132268, .T. ) ;
#62247 = DIRECTION ( 'NONE',  ( 1.000000000000000000, 0.000000000000000000, 0.000000000000000000 ) ) ;
#62248 = VERTEX_POINT ( 'NONE', #6403 ) ;
#62249 = DIRECTION ( 'NONE',  ( 0.000000000000000000, -0.3543493200069153248, -0.9351131265310291818 ) ) ;
#62250 = EDGE_CURVE ( 'NONE', #126389, #74597, #41222, .T. ) ;
#62251 = CARTESIAN_POINT ( 'NONE',  ( 120.6833603837962414, -2.130196079827426203, 7.949999999999997513 ) ) ;
#62252 = PLANE ( 'NONE',  #129508 ) ;
#62253 = DIRECTION ( 'NONE',  ( 0.7071067811865487940, 0.7071067811865463515, 0.000000000000000000 ) ) ;
#62254 = CARTESIAN_POINT ( 'NONE',  ( -10.49999999999991296, -17.94781430457065241, 5.000000000000000000 ) ) ;
#62255 = SURFACE_STYLE_FILL_AREA ( #84030 ) ;
#62256 = DIRECTION ( 'NONE',  ( -1.000000000000000000, -1.224606353822377258E-16, -0.000000000000000000 ) ) ;
#62257 = CARTESIAN_POINT ( 'NONE',  ( 4.229166666666666963, -6.094999999999989093, 1.633150327867691765 ) ) ;
#62258 = CARTESIAN_POINT ( 'NONE',  ( 5.520403141435219929, 7.934999999999988951, -2.126176841940961904 ) ) ;
#62259 = CARTESIAN_POINT ( 'NONE',  ( -60.48921356237309510, -27.52281430457097500, 5.000000000000000000 ) ) ;
#62260 = CARTESIAN_POINT ( 'NONE',  ( -34.47516574401891631, 16.49051761211544331, 4.998110765256835286 ) ) ;
#62261 = PLANE ( 'NONE',  #61798 ) ;
#62262 = EDGE_LOOP ( 'NONE', ( #137193, #72509, #64676, #3741 ) ) ;
#62263 = EDGE_CURVE ( 'NONE', #105769, #64475, #20166, .T. ) ;
#62264 = ORIENTED_EDGE ( 'NONE', *, *, #86758, .F. ) ;
#62265 = CARTESIAN_POINT ( 'NONE',  ( 82.22916666666665719, 7.950000000000001954, -2.130196079827421762 ) ) ;
#62266 = EDGE_CURVE ( 'NONE', #71647, #94488, #9268, .T. ) ;
#62267 = CARTESIAN_POINT ( 'NONE',  ( -33.48921356237309510, -27.52281430457078670, 5.000000000000000000 ) ) ;
#62268 = EDGE_LOOP ( 'NONE', ( #116376, #93201, #115697, #18596 ) ) ;
#62269 = VECTOR ( 'NONE', #107997, 999.9999999999998863 ) ;
#62270 = CARTESIAN_POINT ( 'NONE',  ( 8.188407645496676324, 9.139736423841732040E-16, 0.000000000000000000 ) ) ;
#62271 = DIRECTION ( 'NONE',  ( -0.7071067811865486830, -0.7071067811865464625, 0.000000000000000000 ) ) ;
#62272 = EDGE_LOOP ( 'NONE', ( #134201, #101871, #108812, #130846, #5367 ) ) ;
#62273 = AXIS2_PLACEMENT_3D ( 'NONE', #67152, #121505, #12033 ) ;
#62274 = VECTOR ( 'NONE', #142464, 1000.000000000000000 ) ;
#62276 = LINE ( 'NONE', #17319, #111102 ) ;
#62275 = AXIS2_PLACEMENT_3D ( 'NONE', #22517, #21116, #65378 ) ;
#62277 = LINE ( 'NONE', #52095, #67293 ) ;
#62278 = AXIS2_PLACEMENT_3D ( 'NONE', #1480, #66082, #110248 ) ;
#62279 = CARTESIAN_POINT ( 'NONE',  ( 14.99999999999990230, 12.25461709320622639, -10.07315571508693708 ) ) ;
#62280 = DIRECTION ( 'NONE',  ( 0.000000000000000000, -1.000000000000000000, 0.000000000000000000 ) ) ;
#62281 = EDGE_CURVE ( 'NONE', #131664, #130620, #83322, .T. ) ;
#62282 = CARTESIAN_POINT ( 'NONE',  ( 0.2153679725188470950, -51.67626207039724306, 38.40320453011149482 ) ) ;
#62283 = CARTESIAN_POINT ( 'NONE',  ( -32.99999999999976552, 19.55218569542897100, 5.000000000000000000 ) ) ;
#62285 = PLANE ( 'NONE',  #29063 ) ;
#62284 = VECTOR ( 'NONE', #75917, 1000.000000000000000 ) ;
#62286 = CARTESIAN_POINT ( 'NONE',  ( -47.99451991528749062, 28.92564299267971251, 4.000000000000000000 ) ) ;
#62287 = FACE_OUTER_BOUND ( 'NONE', #98716, .T. ) ;
#62288 = AXIS2_PLACEMENT_3D ( 'NONE', #24074, #3017, #13161 ) ;
#62289 = LINE ( 'NONE', #120741, #137844 ) ;
#62290 = PLANE ( 'NONE',  #83940 ) ;
#62291 = ORIENTED_EDGE ( 'NONE', *, *, #16957, .F. ) ;
#62292 = ORIENTED_EDGE ( 'NONE', *, *, #66457, .F. ) ;
#62293 = CARTESIAN_POINT ( 'NONE',  ( 106.4587635252314328, 0.000000000000000000, -6.110000000000001208 ) ) ;
#62294 = VERTEX_POINT ( 'NONE', #117337 ) ;
#62295 = VECTOR ( 'NONE', #7274, 1000.000000000000000 ) ;
#62296 = AXIS2_PLACEMENT_3D ( 'NONE', #34626, #122316, #123073 ) ;
#62297 = CARTESIAN_POINT ( 'NONE',  ( 12.69999999999999574, -40.43000000000000682, 19.45086547876359617 ) ) ;
#62298 = ORIENTED_EDGE ( 'NONE', *, *, #99072, .F. ) ;
#62299 = CARTESIAN_POINT ( 'NONE',  ( 19.49999999999986500, -20.56887692260759337, 4.000000000000000000 ) ) ;
#62301 =( BOUNDED_CURVE ( )  B_SPLINE_CURVE ( 2, ( #106294, #114358, #6973, #51259, #138258, #38943, #95453, #104906, #125964, #5574, #49845, #107745, #62859 ),
 .UNSPECIFIED., .F., .F. ) 
 B_SPLINE_CURVE_WITH_KNOTS ( ( 3, 2, 2, 2, 2, 2, 3 ),
 ( 0.9000000000000000222, 0.9027777777777777901, 0.9055555555555555580, 0.9083333333333333259, 0.9111111111111110938, 0.9138888888888888618, 0.9166666666666666297 ),
 .UNSPECIFIED. ) 
 CURVE ( )  GEOMETRIC_REPRESENTATION_ITEM ( )  RATIONAL_B_SPLINE_CURVE ( ( 1.000000000000000000, 0.9659258262890683122, 1.000000000000000000, 0.9659258262890683122, 1.000000000000000000, 0.9659258262890683122, 1.000000000000000000, 0.9659258262890683122, 1.000000000000000000, 0.9659258262890683122, 1.000000000000000000, 0.9659258262890683122, 1.000000000000000000 ) ) 
 REPRESENTATION_ITEM ( '' )  );
#62300 = DIRECTION ( 'NONE',  ( 0.000000000000000000, 0.000000000000000000, 1.000000000000000000 ) ) ;
#62302 = VECTOR ( 'NONE', #12670, 1000.000000000000000 ) ;
#62303 = CARTESIAN_POINT ( 'NONE',  ( 94.84959685856476597, 6.109999999999996767, 1.637169565754163836 ) ) ;
#62304 = EDGE_LOOP ( 'NONE', ( #11963, #7702, #113164, #10194 ) ) ;
#62305 = PLANE ( 'NONE',  #60558 ) ;
#62306 = EDGE_LOOP ( 'NONE', ( #92647, #24339, #44430, #36657 ) ) ;
#62307 = LINE ( 'NONE', #41237, #140274 ) ;
#62308 = CARTESIAN_POINT ( 'NONE',  ( 66.48921356237309510, -27.52281430457101763, 5.000000000000000000 ) ) ;
#62309 = CIRCLE ( 'NONE', #25227, 2.500000000000000888 ) ;
#62310 =( BOUNDED_CURVE ( )  B_SPLINE_CURVE ( 2, ( #58057, #33446, #58789, #122539, #91380, #132756, #69636, #750, #77647, #13760, #121816, #134895, #2903 ),
 .UNSPECIFIED., .F., .F. ) 
 B_SPLINE_CURVE_WITH_KNOTS ( ( 3, 2, 2, 2, 2, 2, 3 ),
 ( 0.2666666666666666075, 0.2694444444444443754, 0.2722222222222221433, 0.2750000000000000222, 0.2777777777777777901, 0.2805555555555555580, 0.2833333333333333259 ),
 .UNSPECIFIED. ) 
 CURVE ( )  GEOMETRIC_REPRESENTATION_ITEM ( )  RATIONAL_B_SPLINE_CURVE ( ( 1.000000000000000666, 0.9659258262890676461, 1.000000000000000000, 0.9659258262890683122, 1.000000000000000000, 0.9659258262890683122, 1.000000000000000000, 0.9659258262890683122, 1.000000000000000000, 0.9659258262890683122, 1.000000000000000000, 0.9659258262890683122, 1.000000000000000000 ) ) 
 REPRESENTATION_ITEM ( '' )  );
#62311 = CARTESIAN_POINT ( 'NONE',  ( 128.1437635252314351, 0.000000000000000000, -6.109999999999999432 ) ) ;
#62312 = VECTOR ( 'NONE', #101820, 1000.000000000000000 ) ;
#62313 = VECTOR ( 'NONE', #19257, 999.9999999999998863 ) ;
#62314 = ORIENTED_EDGE ( 'NONE', *, *, #81284, .T. ) ;
#62315 = ORIENTED_EDGE ( 'NONE', *, *, #37954, .T. ) ;
#62316 = B_SPLINE_CURVE_WITH_KNOTS ( 'NONE', 3,
 ( #130724, #56026, #85751, #119097, #19781, #31389, #108190, #141584, #75612, #136396, #124104, #24780, #23342, #3024, #69028, #133564, #25483, #89332, #70489, #81339, #134274, #114636, #123422, #36386, #3704, #24082, #67616, #12471 ),
 .UNSPECIFIED., .F., .F.,
 ( 4, 2, 2, 2, 2, 2, 2, 2, 2, 2, 2, 2, 2, 4 ),
 ( 0.000000000000000000, 0.001834580916944877167, 0.002751871375417315642, 0.003669161833889754334, 0.004586452292362193026, 0.005503742750834631284, 0.006421033209307069542, 0.007338323667779508667, 0.008255614126251946058, 0.009172904584724386051, 0.01100748550166926257, 0.01192477596014169909, 0.01284206641861413561, 0.01467664733555900693 ),
 .UNSPECIFIED. ) ;
#62317 = VERTEX_POINT ( 'NONE', #132565 ) ;
#62318 = LINE ( 'NONE', #49315, #111597 ) ;
#62319 = EDGE_CURVE ( 'NONE', #115069, #141369, #133263, .T. ) ;
#62320 = LINE ( 'NONE', #5018, #24571 ) ;
#62321 = CARTESIAN_POINT ( 'NONE',  ( 10.27540314143522160, -2.126176841940958351, -7.934999999999988951 ) ) ;
#62322 = AXIS2_PLACEMENT_3D ( 'NONE', #27285, #71538, #93978 ) ;
#62323 = VECTOR ( 'NONE', #20235, 1000.000000000000000 ) ;
#62324 = DIRECTION ( 'NONE',  ( -0.000000000000000000, 0.000000000000000000, 1.000000000000000000 ) ) ;
#62325 = EDGE_CURVE ( 'NONE', #58304, #56879, #57145, .T. ) ;
#62326 = EDGE_CURVE ( 'NONE', #87749, #38833, #43382, .T. ) ;
#62327 = EDGE_CURVE ( 'NONE', #52815, #78350, #33260, .T. ) ;
#62328 = ORIENTED_EDGE ( 'NONE', *, *, #85716, .F. ) ;
#62329 = EDGE_LOOP ( 'NONE', ( #56283, #61127, #89932, #104068 ) ) ;
#62331 = EDGE_CURVE ( 'NONE', #93380, #77093, #23771, .T. ) ;
#62330 = CARTESIAN_POINT ( 'NONE',  ( 0.000000000000000000, -7.600000000000055600, -28.92499999999998650 ) ) ;
#62332 = ORIENTED_EDGE ( 'NONE', *, *, #50078, .F. ) ;
#62333 = ORIENTED_EDGE ( 'NONE', *, *, #122586, .T. ) ;
#62334 = AXIS2_PLACEMENT_3D ( 'NONE', #41514, #53094, #74904 ) ;
#62335 = ADVANCED_FACE ( 'NONE', ( #42688 ), #110040, .F. ) ;
#62336 = EDGE_CURVE ( 'NONE', #108896, #48371, #78885, .T. ) ;
#62337 = CARTESIAN_POINT ( 'NONE',  ( 17.93750000000000355, -4.461849672132299105, 4.461849672132299993 ) ) ;
#62338 = LINE ( 'NONE', #40580, #107392 ) ;
#62339 = VERTEX_POINT ( 'NONE', #133953 ) ;
#62340 = LINE ( 'NONE', #81968, #120059 ) ;
#62341 = CARTESIAN_POINT ( 'NONE',  ( 34.92499999999998295, 22.22500000000000142, 4.500000000000000888 ) ) ;
#62342 = DIRECTION ( 'NONE',  ( 0.3543493200069162685, -0.000000000000000000, -0.9351131265310288487 ) ) ;
#62343 = CARTESIAN_POINT ( 'NONE',  ( 66.48921356237309510, -27.52281430457101763, 5.000000000000000000 ) ) ;
#62344 = VERTEX_POINT ( 'NONE', #131820 ) ;
#62345 = ADVANCED_FACE ( 'NONE', ( #77464 ), #98464, .F. ) ;
#62346 = CARTESIAN_POINT ( 'NONE',  ( 5.207106781186508826, -11.24070752338417556, 5.000000000000000000 ) ) ;
#62347 = FACE_BOUND ( 'NONE', #43113, .T. ) ;
#62348 = ORIENTED_EDGE ( 'NONE', *, *, #112748, .F. ) ;
#62349 = CARTESIAN_POINT ( 'NONE',  ( 39.48921356237310221, -27.52281430457082934, 5.000000000000000000 ) ) ;
#62350 = CARTESIAN_POINT ( 'NONE',  ( 66.18398860626901126, 28.73617430169833753, 5.000000000000000000 ) ) ;
#62351 = CARTESIAN_POINT ( 'NONE',  ( 27.70710678118635428, 2.259292476615694323, 5.000000000000000000 ) ) ;
#62352 = VERTEX_POINT ( 'NONE', #99149 ) ;
#62353 = DIRECTION ( 'NONE',  ( 0.5735764363510451602, 0.8191520442889924647, 0.000000000000000000 ) ) ;
#62354 = ORIENTED_EDGE ( 'NONE', *, *, #86231, .T. ) ;
#62355 = ORIENTED_EDGE ( 'NONE', *, *, #13852, .F. ) ;
#62356 = EDGE_CURVE ( 'NONE', #39995, #100143, #28183, .T. ) ;
#62357 = ORIENTED_EDGE ( 'NONE', *, *, #121722, .T. ) ;
#62358 = CARTESIAN_POINT ( 'NONE',  ( 30.39126352523144448, -4.472830434245838482, -4.472830434245838482 ) ) ;
#62359 = CARTESIAN_POINT ( 'NONE',  ( 34.92499999999998295, 10.70193056682087906, 4.500000000000000888 ) ) ;
#62360 = CARTESIAN_POINT ( 'NONE',  ( 6.932893218813437564, -40.13710678118655295, -40.00000000000000000 ) ) ;
#62361 = DIRECTION ( 'NONE',  ( -0.000000000000000000, -1.000000000000000000, -0.000000000000000000 ) ) ;
#62362 = LINE ( 'NONE', #7936, #119133 ) ;
#62363 = PLANE ( 'NONE',  #13437 ) ;
#62364 = CARTESIAN_POINT ( 'NONE',  ( -29.57672154193627989, 11.25929247661560240, 17.85071094206591269 ) ) ;
#62365 = DIRECTION ( 'NONE',  ( 0.7071067811865487940, 0.7071067811865463515, 0.000000000000000000 ) ) ;
#62366 = CARTESIAN_POINT ( 'NONE',  ( 6.183988606268994381, 28.73617430169791476, 5.000000000000000000 ) ) ;
#62367 = LINE ( 'NONE', #7944, #19291 ) ;
#62368 = VERTEX_POINT ( 'NONE', #89729 ) ;
#62369 = EDGE_CURVE ( 'NONE', #106778, #59322, #121627, .T. ) ;
#62370 = VERTEX_POINT ( 'NONE', #22296 ) ;
#62371 = AXIS2_PLACEMENT_3D ( 'NONE', #77655, #76212, #31291 ) ;
#62372 = ORIENTED_EDGE ( 'NONE', *, *, #39163, .F. ) ;
#62373 = ORIENTED_EDGE ( 'NONE', *, *, #130750, .T. ) ;
#62374 = PLANE ( 'NONE',  #107403 ) ;
#62375 = VECTOR ( 'NONE', #86817, 1000.000000000000000 ) ;
#62376 = VERTEX_POINT ( 'NONE', #56447 ) ;
#62377 = CIRCLE ( 'NONE', #117882, 0.5000000000000004441 ) ;
#62378 = EDGE_CURVE ( 'NONE', #76266, #24327, #67282, .T. ) ;
#62380 = ORIENTED_EDGE ( 'NONE', *, *, #91620, .T. ) ;
#62379 = VECTOR ( 'NONE', #36135, 1000.000000000000000 ) ;
#62381 = DIRECTION ( 'NONE',  ( 0.7071067811865487940, 0.7071067811865463515, 0.000000000000000000 ) ) ;
#62382 = DIRECTION ( 'NONE',  ( 0.7071067811865487940, -0.7071067811865463515, 0.000000000000000000 ) ) ;
#62383 = ORIENTED_EDGE ( 'NONE', *, *, #22971, .F. ) ;
#62384 = DIRECTION ( 'NONE',  ( 0.000000000000000000, -1.000000000000000000, 0.000000000000000000 ) ) ;
#62386 = ORIENTED_EDGE ( 'NONE', *, *, #79247, .F. ) ;
#62385 = VECTOR ( 'NONE', #21594, 1000.000000000000227 ) ;
#62387 = EDGE_CURVE ( 'NONE', #91753, #113725, #121045, .T. ) ;
#62388 = CARTESIAN_POINT ( 'NONE',  ( -24.18398860626899705, 28.73617430169804265, 5.000000000000000000 ) ) ;
#62389 = CARTESIAN_POINT ( 'NONE',  ( 30.18398860626900060, 28.73617430169808173, 5.000000000000000000 ) ) ;
#62390 = CARTESIAN_POINT ( 'NONE',  ( 6.046236474768552860, -7.934999999999990727, 4.858786175617117713E-16 ) ) ;
#62391 = VERTEX_POINT ( 'NONE', #1270 ) ;
#62392 = CARTESIAN_POINT ( 'NONE',  ( 92.07876352523145158, -7.482591942790327058E-16, 6.109999999999999432 ) ) ;
#62393 = CARTESIAN_POINT ( 'NONE',  ( -32.99999999999976552, 4.552185695429122880, 5.000000000000000000 ) ) ;
#62394 = ADVANCED_FACE ( 'NONE', ( #110734 ), #11418, .T. ) ;
#62395 = CARTESIAN_POINT ( 'NONE',  ( -29.99999999999979039, 15.45873954670182115, -0.03131636524287412238 ) ) ;
#62396 = ORIENTED_EDGE ( 'NONE', *, *, #26127, .F. ) ;
#62397 = ORIENTED_EDGE ( 'NONE', *, *, #25611, .F. ) ;
#62398 = LINE ( 'NONE', #64518, #17166 ) ;
#62399 = VERTEX_POINT ( 'NONE', #563 ) ;
#62400 = VECTOR ( 'NONE', #8509, 999.9999999999998863 ) ;
#62401 = CARTESIAN_POINT ( 'NONE',  ( 27.18398860626900060, 28.73617430169806042, 5.000000000000000000 ) ) ;
#62402 = DIRECTION ( 'NONE',  ( -1.000000000000000000, -0.000000000000000000, -0.000000000000000000 ) ) ;
#62403 = FACE_OUTER_BOUND ( 'NONE', #142625, .T. ) ;
#62404 = DIRECTION ( 'NONE',  ( -0.000000000000000000, 0.3543493200069153248, 0.9351131265310292928 ) ) ;
#62405 = VERTEX_POINT ( 'NONE', #44855 ) ;
#62406 = CARTESIAN_POINT ( 'NONE',  ( 2.999999999999999112, -7.600000000000053824, -34.92499999999998295 ) ) ;
#62407 = CONICAL_SURFACE ( 'NONE', #27602, 2.055000000000001048, 0.9599310885968758145 ) ;
#62408 = CARTESIAN_POINT ( 'NONE',  ( 12.48921356237309155, -27.52281430457064104, 5.000000000000000000 ) ) ;
#62409 = DIRECTION ( 'NONE',  ( -0.6830127018922180770, -0.6830127018922204085, -0.2588190451025213501 ) ) ;
#62410 = ORIENTED_EDGE ( 'NONE', *, *, #70626, .T. ) ;
#62411 = CARTESIAN_POINT ( 'NONE',  ( 34.92499999999998295, -4.487538124160487030, 4.000000000000000000 ) ) ;
#62412 = VECTOR ( 'NONE', #121995, 1000.000000000000000 ) ;
#62414 =( GEOMETRIC_REPRESENTATION_CONTEXT ( 3 ) GLOBAL_UNCERTAINTY_ASSIGNED_CONTEXT ( ( #98431 ) ) GLOBAL_UNIT_ASSIGNED_CONTEXT ( ( #119110, #53127, #108200 ) ) REPRESENTATION_CONTEXT ( 'NONE', 'WORKASPACE' ) );
#62413 = CARTESIAN_POINT ( 'NONE',  ( -22.82816939922337340, -2.240707523384255939, 4.000000000000000000 ) ) ;
#62415 = ORIENTED_EDGE ( 'NONE', *, *, #103346, .T. ) ;
#62416 = VECTOR ( 'NONE', #71888, 1000.000000000000000 ) ;
#62419 = ADVANCED_FACE ( 'NONE', ( #10024 ), #20888, .F. ) ;
#62418 = VERTEX_POINT ( 'NONE', #100622 ) ;
#62417 = LINE ( 'NONE', #41340, #53230 ) ;
#62420 = FACE_OUTER_BOUND ( 'NONE', #65607, .T. ) ;
#62421 = AXIS2_PLACEMENT_3D ( 'NONE', #58223, #68372, #112551 ) ;
#62422 = PLANE ( 'NONE',  #18256 ) ;
#62423 = VERTEX_POINT ( 'NONE', #111480 ) ;
#62424 = DIRECTION ( 'NONE',  ( -0.7071067811865487940, 0.7071067811865463515, 0.000000000000000000 ) ) ;
#62425 = CARTESIAN_POINT ( 'NONE',  ( -0.005480084712502889671, 28.92564299267938210, 4.000000000000000000 ) ) ;
#62426 = ADVANCED_FACE ( 'NONE', ( #69431 ), #135410, .F. ) ;
#62427 = DIRECTION ( 'NONE',  ( -0.000000000000000000, 0.3543493200069153248, 0.9351131265310292928 ) ) ;
#62428 = CARTESIAN_POINT ( 'NONE',  ( -42.29974487139158157, -27.71228299555235708, 4.000000000000000000 ) ) ;
#62429 = LINE ( 'NONE', #106587, #25752 ) ;
#62430 = CARTESIAN_POINT ( 'NONE',  ( -12.69999999999998153, 0.000000000000000000, 0.000000000000000000 ) ) ;
#62431 = CARTESIAN_POINT ( 'NONE',  ( 19.05000000000000071, 3.174999999999997158, 4.000000000000000000 ) ) ;
#62432 = FACE_OUTER_BOUND ( 'NONE', #15062, .T. ) ;
#62433 = VECTOR ( 'NONE', #136938, 1000.000000000000227 ) ;
#62434 = FACE_OUTER_BOUND ( 'NONE', #9000, .T. ) ;
#62435 = DIRECTION ( 'NONE',  ( -0.7071067811865487940, 0.7071067811865463515, -0.000000000000000000 ) ) ;
#62436 = DIRECTION ( 'NONE',  ( 0.000000000000000000, 0.000000000000000000, 1.000000000000000000 ) ) ;
#62437 = ORIENTED_EDGE ( 'NONE', *, *, #134281, .F. ) ;
#62438 = ADVANCED_FACE ( 'NONE', ( #36767 ), #102765, .F. ) ;
#62439 = ORIENTED_EDGE ( 'NONE', *, *, #20299, .T. ) ;
#62440 = VERTEX_POINT ( 'NONE', #25177 ) ;
#62441 = CARTESIAN_POINT ( 'NONE',  ( 109.7916666666666572, 3.975000000000003642, -6.884901960086285300 ) ) ;
#62442 = ADVANCED_FACE ( 'NONE', ( #81018 ), #3410, .T. ) ;
#62443 = EDGE_LOOP ( 'NONE', ( #91028, #77925, #45923, #113521 ) ) ;
#62444 = VERTEX_POINT ( 'NONE', #24471 ) ;
#62445 = EDGE_LOOP ( 'NONE', ( #25471, #9252, #133656, #121846 ) ) ;
#62446 = DIRECTION ( 'NONE',  ( -0.000000000000000000, -0.000000000000000000, 1.000000000000000000 ) ) ;
#62447 = DIRECTION ( 'NONE',  ( 0.000000000000000000, 1.000000000000000000, 0.000000000000000000 ) ) ;
#62448 = ORIENTED_EDGE ( 'NONE', *, *, #93232, .F. ) ;
#62449 = PLANE ( 'NONE',  #90222 ) ;
#62450 = CARTESIAN_POINT ( 'NONE',  ( -21.18398860626899349, 28.73617430169802134, 5.000000000000000000 ) ) ;
#62451 = CARTESIAN_POINT ( 'NONE',  ( 0.000000000000000000, 0.000000000000000000, 5.000000000000000000 ) ) ;
#62452 = DIRECTION ( 'NONE',  ( -0.000000000000000000, 0.3543493200069153248, 0.9351131265310292928 ) ) ;
#62453 = CARTESIAN_POINT ( 'NONE',  ( 106.4587635252314328, 0.000000000000000000, -6.110000000000001208 ) ) ;
#62454 = ORIENTED_EDGE ( 'NONE', *, *, #107315, .F. ) ;
#62455 = EDGE_CURVE ( 'NONE', #42067, #126713, #90450, .T. ) ;
#62456 = LINE ( 'NONE', #40697, #116366 ) ;
#62457 = CARTESIAN_POINT ( 'NONE',  ( 7.139999999999955271, -35.56014942880460694, -8.278119684037269721 ) ) ;
#62458 = FACE_OUTER_BOUND ( 'NONE', #875, .T. ) ;
#62459 = CARTESIAN_POINT ( 'NONE',  ( 41.35002705046288440, -5.819803920172572198, -5.819803920172572198 ) ) ;
#62460 = DIRECTION ( 'NONE',  ( -0.7071067811865486830, 0.7071067811865464625, 0.000000000000000000 ) ) ;
#62461 = DIRECTION ( 'NONE',  ( 0.000000000000000000, 1.000000000000000000, 0.000000000000000000 ) ) ;
#62462 = EDGE_LOOP ( 'NONE', ( #40512, #33407, #140248, #38857 ) ) ;
#62463 = ORIENTED_EDGE ( 'NONE', *, *, #18487, .F. ) ;
#62464 = CARTESIAN_POINT ( 'NONE',  ( 25.79166666666665719, 3.975000000000003642, -6.884901960086285300 ) ) ;
#62465 = ORIENTED_EDGE ( 'NONE', *, *, #135610, .F. ) ;
#62466 = CYLINDRICAL_SURFACE ( 'NONE', #29781, 0.5000000000000004441 ) ;
#62467 = CARTESIAN_POINT ( 'NONE',  ( -30.18398860626900060, 28.73617430169808173, 5.000000000000000000 ) ) ;
#62468 = DIRECTION ( 'NONE',  ( 0.7071067811865487940, 0.7071067811865463515, 0.000000000000000000 ) ) ;
#62469 = FACE_OUTER_BOUND ( 'NONE', #70410, .T. ) ;
#62470 = CARTESIAN_POINT ( 'NONE',  ( -12.69999999999998153, 3.061616997868383634E-16, -2.500000000000000444 ) ) ;
#62471 = CARTESIAN_POINT ( 'NONE',  ( 32.14818355038125475, 17.25929247661554200, 8.802941693769275489 ) ) ;
#62472 = CARTESIAN_POINT ( 'NONE',  ( 124.8912635252314516, -4.472830434245839371, -4.472830434245839371 ) ) ;
#62473 = VERTEX_POINT ( 'NONE', #26617 ) ;
#62474 = CARTESIAN_POINT ( 'NONE',  ( 27.48921356237309155, -27.52281430457074762, 5.000000000000000000 ) ) ;
#62475 = ORIENTED_EDGE ( 'NONE', *, *, #50570, .T. ) ;
#62476 = DIRECTION ( 'NONE',  ( -0.000000000000000000, 0.3543493200069153248, 0.9351131265310292928 ) ) ;
#62477 = VECTOR ( 'NONE', #32787, 1000.000000000000000 ) ;
#62478 = VECTOR ( 'NONE', #20818, 1000.000000000000000 ) ;
#62479 = VECTOR ( 'NONE', #94897, 1000.000000000000000 ) ;
#62480 = SURFACE_STYLE_FILL_AREA ( #40041 ) ;
#62481 = VECTOR ( 'NONE', #130837, 1000.000000000000227 ) ;
#62482 = DIRECTION ( 'NONE',  ( -0.3543493200069162685, -0.000000000000000000, -0.9351131265310288487 ) ) ;
#62483 = EDGE_LOOP ( 'NONE', ( #92531, #68041, #82078, #21957 ) ) ;
#62484 = CARTESIAN_POINT ( 'NONE',  ( 49.00043019189810423, -3.055000000000002380, 5.291415217122920289 ) ) ;
#62485 = ORIENTED_EDGE ( 'NONE', *, *, #99589, .F. ) ;
#62486 = DIRECTION ( 'NONE',  ( 0.7071067811865486830, -0.7071067811865464625, -0.000000000000000000 ) ) ;
#62487 = CARTESIAN_POINT ( 'NONE',  ( -10.17183060077639212, 21.75929247661549581, 4.000000000000000000 ) ) ;
#62488 = DIRECTION ( 'NONE',  ( 1.000000000000000000, 0.000000000000000000, 0.000000000000000000 ) ) ;
#62489 = FACE_OUTER_BOUND ( 'NONE', #122133, .T. ) ;
#62490 = AXIS2_PLACEMENT_3D ( 'NONE', #79596, #57816, #123779 ) ;
#62491 =( BOUNDED_CURVE ( )  B_SPLINE_CURVE ( 3, ( #111871, #12535, #56813, #1631 ),
 .UNSPECIFIED., .F., .T. ) 
 B_SPLINE_CURVE_WITH_KNOTS ( ( 4, 4 ),
 ( 1.901594255663624056, 1.933014472006554740 ),
 .UNSPECIFIED. ) 
 CURVE ( )  GEOMETRIC_REPRESENTATION_ITEM ( )  RATIONAL_B_SPLINE_CURVE ( ( 1.000000000000000000, 0.9999177325257868620, 0.9999177325257868620, 1.000000000000000000 ) ) 
 REPRESENTATION_ITEM ( '' )  );
#62492 = ADVANCED_FACE ( 'NONE', ( #25906 ), #38219, .F. ) ;
#62493 = AXIS2_PLACEMENT_3D ( 'NONE', #84349, #62578, #106761 ) ;
#62494 = CARTESIAN_POINT ( 'NONE',  ( 43.37043019189810877, -3.055000000000001492, 5.291415217122917625 ) ) ;
#62495 = ADVANCED_FACE ( 'NONE', ( #13571 ), #123358, .T. ) ;
#62497 = ADVANCED_FACE ( 'NONE', ( #59286 ), #68718, .T. ) ;
#62496 = ORIENTED_EDGE ( 'NONE', *, *, #34402, .F. ) ;
#62498 = PLANE ( 'NONE',  #74368 ) ;
#62500 = EDGE_CURVE ( 'NONE', #4447, #136109, #104141, .T. ) ;
#62499 = DIRECTION ( 'NONE',  ( 0.6830127018922181881, 0.6830127018922202975, -0.2588190451025214056 ) ) ;
#62501 = VERTEX_POINT ( 'NONE', #126619 ) ;
#62502 = ORIENTED_EDGE ( 'NONE', *, *, #102313, .T. ) ;
#62503 = CIRCLE ( 'NONE', #74080, 2.247900000000000453 ) ;
#62504 = VECTOR ( 'NONE', #10009, 1000.000000000000000 ) ;
#62505 = ORIENTED_EDGE ( 'NONE', *, *, #19322, .T. ) ;
#62506 = EDGE_CURVE ( 'NONE', #56761, #100010, #79634, .T. ) ;
#62507 = VECTOR ( 'NONE', #49821, 1000.000000000000000 ) ;
#62508 = CARTESIAN_POINT ( 'NONE',  ( -34.42500000000001137, 1.541399257802000822, 5.000000000000000000 ) ) ;
#62509 = LINE ( 'NONE', #71246, #104361 ) ;
#62510 = ORIENTED_EDGE ( 'NONE', *, *, #48583, .T. ) ;
#62511 = CARTESIAN_POINT ( 'NONE',  ( -36.29974487139159578, -27.71228299555231445, 4.000000000000000000 ) ) ;
#62512 = ADVANCED_FACE ( 'NONE', ( #2708 ), #47007, .F. ) ;
#62513 = VECTOR ( 'NONE', #108405, 1000.000000000000000 ) ;
#62514 = VECTOR ( 'NONE', #34814, 1000.000000000000227 ) ;
#62515 = CARTESIAN_POINT ( 'NONE',  ( 34.92500000000002558, -21.76999999999999247, 0.000000000000000000 ) ) ;
#62516 = ADVANCED_FACE ( 'NONE', ( #129483 ), #128094, .F. ) ;
#62517 = FACE_BOUND ( 'NONE', #137669, .T. ) ;
#62518 = EDGE_CURVE ( 'NONE', #80963, #124390, #140369, .T. ) ;
#62519 = CARTESIAN_POINT ( 'NONE',  ( -71.99451991528749772, 28.92564299267988304, 4.000000000000000000 ) ) ;
#62520 = AXIS2_PLACEMENT_3D ( 'NONE', #15936, #48623, #115248 ) ;
#62521 = CARTESIAN_POINT ( 'NONE',  ( 3.102554694470387897, -48.63825160239814949, 38.47250499286694492 ) ) ;
#62522 = DIRECTION ( 'NONE',  ( -0.000000000000000000, -1.000000000000000000, -0.000000000000000000 ) ) ;
#62523 = ORIENTED_EDGE ( 'NONE', *, *, #47251, .F. ) ;
#62524 = EDGE_LOOP ( 'NONE', ( #56331, #110330, #54704 ) ) ;
#62525 = AXIS2_PLACEMENT_3D ( 'NONE', #113612, #109522, #47002 ) ;
#62526 = ORIENTED_EDGE ( 'NONE', *, *, #111409, .F. ) ;
#62527 = FACE_OUTER_BOUND ( 'NONE', #73866, .T. ) ;
#62528 = EDGE_CURVE ( 'NONE', #130484, #18319, #30920, .T. ) ;
#62529 = ORIENTED_EDGE ( 'NONE', *, *, #93760, .T. ) ;
#62530 = CARTESIAN_POINT ( 'NONE',  ( 55.91209685856478018, 5.291415217122921177, -3.054999999999994831 ) ) ;
#62531 = ORIENTED_EDGE ( 'NONE', *, *, #74448, .T. ) ;
#62532 = FACE_OUTER_BOUND ( 'NONE', #69697, .T. ) ;
#62533 = CARTESIAN_POINT ( 'NONE',  ( -19.49999999999985079, -4.912538124160707120, 4.000000000000000000 ) ) ;
#62534 = EDGE_LOOP ( 'NONE', ( #141128, #1684, #104983, #121310 ) ) ;
#62535 = DIRECTION ( 'NONE',  ( -0.7071067811865486830, -0.7071067811865464625, 0.000000000000000000 ) ) ;
#62536 = AXIS2_PLACEMENT_3D ( 'NONE', #83673, #73488, #128571 ) ;
#62537 = DIRECTION ( 'NONE',  ( 0.5735764363510453823, -0.8191520442889923537, 1.003171929053525486E-16 ) ) ;
#62538 = CARTESIAN_POINT ( 'NONE',  ( 5.816011393731002066, 28.73617430169783304, 5.000000000000000000 ) ) ;
#62539 = CARTESIAN_POINT ( 'NONE',  ( -14.24139925780194105, 21.72500000000000142, 5.000000000000000000 ) ) ;
#62540 = LINE ( 'NONE', #59690, #72528 ) ;
#62541 = PLANE ( 'NONE',  #11503 ) ;
#62542 = ORIENTED_EDGE ( 'NONE', *, *, #130967, .T. ) ;
#62543 = EDGE_CURVE ( 'NONE', #106767, #109446, #8388, .T. ) ;
#62544 = CIRCLE ( 'NONE', #44014, 2.500000000000000444 ) ;
#62545 = ORIENTED_EDGE ( 'NONE', *, *, #2570, .F. ) ;
#62546 = DIRECTION ( 'NONE',  ( -1.000000000000000000, 3.654646145370261567E-15, 0.000000000000000000 ) ) ;
#62547 = PLANE ( 'NONE',  #30479 ) ;
#62548 = ORIENTED_EDGE ( 'NONE', *, *, #15646, .F. ) ;
#62549 = ORIENTED_EDGE ( 'NONE', *, *, #27339, .F. ) ;
#62550 = ORIENTED_EDGE ( 'NONE', *, *, #27860, .T. ) ;
#62551 = DIRECTION ( 'NONE',  ( -0.6830127018922181881, 0.6830127018922202975, -0.2588190451025214056 ) ) ;
#62552 = CARTESIAN_POINT ( 'NONE',  ( 159.7320121765528711, 26.96999999999993847, -34.92499999999998295 ) ) ;
#62553 = ORIENTED_EDGE ( 'NONE', *, *, #126744, .T. ) ;
#62554 = PLANE ( 'NONE',  #99551 ) ;
#62555 = VECTOR ( 'NONE', #104843, 1000.000000000000227 ) ;
#62556 = CARTESIAN_POINT ( 'NONE',  ( 14.06706980810188412, 2.126176841940952134, -7.934999999999993392 ) ) ;
#62557 = DIRECTION ( 'NONE',  ( 0.3543493200069162685, -0.000000000000000000, -0.9351131265310288487 ) ) ;
#62558 = ORIENTED_EDGE ( 'NONE', *, *, #38155, .F. ) ;
#62559 = CARTESIAN_POINT ( 'NONE',  ( -34.92500000000001137, 22.22500000000000142, 4.000000000000000000 ) ) ;
#62561 = ADVANCED_FACE ( 'NONE', ( #60717 ), #118669, .T. ) ;
#62560 = DIRECTION ( 'NONE',  ( 0.7071067811865487940, 0.7071067811865463515, 0.000000000000000000 ) ) ;
#62562 = DIRECTION ( 'NONE',  ( -0.7071067811865486830, -0.7071067811865464625, 0.000000000000000000 ) ) ;
#62564 = ORIENTED_EDGE ( 'NONE', *, *, #91941, .T. ) ;
#62563 = CARTESIAN_POINT ( 'NONE',  ( 0.000000000000000000, 0.000000000000000000, 5.000000000000000000 ) ) ;
#62565 = CARTESIAN_POINT ( 'NONE',  ( 11.71247294953710671, 0.000000000000000000, 6.094999999999989981 ) ) ;
#62566 = ORIENTED_EDGE ( 'NONE', *, *, #91434, .T. ) ;
#62567 = PLANE ( 'NONE',  #28780 ) ;
#62568 = DIRECTION ( 'NONE',  ( -0.000000000000000000, 0.000000000000000000, 1.000000000000000000 ) ) ;
#62569 = DIRECTION ( 'NONE',  ( 0.7071067811865487940, 0.7071067811865463515, 0.000000000000000000 ) ) ;
#62570 = ORIENTED_EDGE ( 'NONE', *, *, #108828, .F. ) ;
#62571 = EDGE_CURVE ( 'NONE', #67893, #10128, #87466, .T. ) ;
#62572 = FACE_OUTER_BOUND ( 'NONE', #116010, .T. ) ;
#62573 = CARTESIAN_POINT ( 'NONE',  ( 34.92499999999998295, 12.85612307739228477, 4.000000000000000000 ) ) ;
#62574 = ORIENTED_EDGE ( 'NONE', *, *, #2969, .T. ) ;
#62575 = AXIS2_PLACEMENT_3D ( 'NONE', #13659, #36174, #113717 ) ;
#62576 = VECTOR ( 'NONE', #26208, 1000.000000000000000 ) ;
#62577 = VECTOR ( 'NONE', #39950, 999.9999999999998863 ) ;
#62578 = DIRECTION ( 'NONE',  ( 0.6830127018922181881, 0.6830127018922202975, -0.2588190451025214056 ) ) ;
#62579 = DIRECTION ( 'NONE',  ( 0.000000000000000000, 1.000000000000000000, 0.000000000000000000 ) ) ;
#62580 = LINE ( 'NONE', #30670, #12230 ) ;
#62581 = VECTOR ( 'NONE', #15755, 1000.000000000000000 ) ;
#62582 = CARTESIAN_POINT ( 'NONE',  ( -20.99999999999985079, 20.96639925780204905, 5.000000000000000000 ) ) ;
#62584 = EDGE_CURVE ( 'NONE', #61664, #74056, #116481, .T. ) ;
#62583 = EDGE_LOOP ( 'NONE', ( #59550, #110665, #52480, #6871 ) ) ;
#62585 = ORIENTED_EDGE ( 'NONE', *, *, #96012, .T. ) ;
#62586 = DIRECTION ( 'NONE',  ( 0.000000000000000000, 0.000000000000000000, 1.000000000000000000 ) ) ;
#62587 = VECTOR ( 'NONE', #68524, 1000.000000000000227 ) ;
#62588 = DIRECTION ( 'NONE',  ( 0.000000000000000000, -1.000000000000000000, 0.000000000000000000 ) ) ;
#62589 = CARTESIAN_POINT ( 'NONE',  ( 14.41623647476855297, -7.934999999999990727, 4.858786175617117713E-16 ) ) ;
#62590 = CARTESIAN_POINT ( 'NONE',  ( -8.816011393731004731, 28.73617430169781173, 5.000000000000000000 ) ) ;
#62591 = FACE_OUTER_BOUND ( 'NONE', #57008, .T. ) ;
#62592 = PLANE ( 'NONE',  #111594 ) ;
#62593 = ORIENTED_EDGE ( 'NONE', *, *, #99858, .F. ) ;
#62594 = LINE ( 'NONE', #106779, #55791 ) ;
#62595 = DIRECTION ( 'NONE',  ( 0.000000000000000000, -1.000000000000000000, 0.000000000000000000 ) ) ;
#62596 = CARTESIAN_POINT ( 'NONE',  ( 5.004139616203772789, -3.047499999999994547, 5.278424836066145431 ) ) ;
#62597 = VECTOR ( 'NONE', #59399, 1000.000000000000227 ) ;
#62598 = DIRECTION ( 'NONE',  ( 0.000000000000000000, -5.075120898959323014E-15, -1.000000000000000000 ) ) ;
#62599 = CARTESIAN_POINT ( 'NONE',  ( 40.74543019189810877, -5.291415217122919401, -3.055000000000000604 ) ) ;
#62600 = CARTESIAN_POINT ( 'NONE',  ( 5.691592354503320905, 9.902892378096218942E-16, 0.000000000000000000 ) ) ;
#62601 = VECTOR ( 'NONE', #124870, 1000.000000000000000 ) ;
#62602 = ORIENTED_EDGE ( 'NONE', *, *, #6687, .T. ) ;
#62603 = FACE_OUTER_BOUND ( 'NONE', #41662, .T. ) ;
#62604 = AXIS2_PLACEMENT_3D ( 'NONE', #81261, #124738, #89261 ) ;
#62605 = EDGE_CURVE ( 'NONE', #40303, #64278, #49829, .T. ) ;
#62606 = ORIENTED_EDGE ( 'NONE', *, *, #37252, .F. ) ;
#62607 = ADVANCED_FACE ( 'NONE', ( #73693 ), #105577, .F. ) ;
#62608 = VECTOR ( 'NONE', #20689, 1000.000000000000000 ) ;
#62609 = ORIENTED_EDGE ( 'NONE', *, *, #58312, .F. ) ;
#62610 = LINE ( 'NONE', #7479, #52388 ) ;
#62611 = VECTOR ( 'NONE', #27990, 1000.000000000000000 ) ;
#62612 = CARTESIAN_POINT ( 'NONE',  ( -7.940000000000007496, -35.76999999999998892, -10.00000000000000178 ) ) ;
#62613 = CARTESIAN_POINT ( 'NONE',  ( 3.005480084712505828, 28.92564299267936079, 4.000000000000000000 ) ) ;
#62614 = CARTESIAN_POINT ( 'NONE',  ( 156.1500000000000057, -49.14999999999999147, -53.92499999999968452 ) ) ;
#62615 = EDGE_CURVE ( 'NONE', #88778, #95164, #138238, .T. ) ;
#62616 = CARTESIAN_POINT ( 'NONE',  ( -16.49999999999988276, 8.319652575858368593, -8.582050562765862978 ) ) ;
#62617 = CARTESIAN_POINT ( 'NONE',  ( -29.20710678118634362, 12.75929247661559351, 5.000000000000000000 ) ) ;
#62618 = VECTOR ( 'NONE', #84675, 1000.000000000000000 ) ;
#62619 = ORIENTED_EDGE ( 'NONE', *, *, #2753, .T. ) ;
#62620 = EDGE_CURVE ( 'NONE', #105795, #100461, #30177, .T. ) ;
#62621 = LINE ( 'NONE', #60496, #102256 ) ;
#62622 = CARTESIAN_POINT ( 'NONE',  ( 14.51078643762690490, -27.52281430457045275, 5.000000000000000000 ) ) ;
#62623 = LINE ( 'NONE', #119120, #40348 ) ;
#62624 = CARTESIAN_POINT ( 'NONE',  ( 66.48921356237309510, -27.52281430457101763, 5.000000000000000000 ) ) ;
#62625 = CYLINDRICAL_SURFACE ( 'NONE', #40444, 7.950000000000000178 ) ;
#62626 = CARTESIAN_POINT ( 'NONE',  ( 104.6416937171295416, -2.130196079827424871, -7.949999999999998401 ) ) ;
#62627 = CARTESIAN_POINT ( 'NONE',  ( 65.70419371712955581, -6.884901960086285300, -3.975000000000000089 ) ) ;
#62628 = DIRECTION ( 'NONE',  ( -0.7071067811865486830, -0.7071067811865464625, 0.000000000000000000 ) ) ;
#62629 = VECTOR ( 'NONE', #87290, 999.9999999999998863 ) ;
#62630 = EDGE_LOOP ( 'NONE', ( #77300, #26103, #55882, #120929 ) ) ;
#62631 = EDGE_LOOP ( 'NONE', ( #14500, #9297, #110345, #83210 ) ) ;
#62632 = CARTESIAN_POINT ( 'NONE',  ( 52.62499999999999289, -7.950000000000000178, -4.867971026610729436E-16 ) ) ;
#62633 = CARTESIAN_POINT ( 'NONE',  ( 32.29289321881324071, -12.74070752338415069, 5.000000000000000000 ) ) ;
#62634 = CARTESIAN_POINT ( 'NONE',  ( 22.82816939922337340, 21.75929247661548516, 4.000000000000000000 ) ) ;
#62635 = AXIS2_PLACEMENT_3D ( 'NONE', #7856, #127516, #94158 ) ;
#62636 = DIRECTION ( 'NONE',  ( -0.7071067811865486830, 0.7071067811865464625, 0.000000000000000000 ) ) ;
#62637 = EDGE_LOOP ( 'NONE', ( #21663, #80433, #19734, #31090, #12927 ) ) ;
#62638 = ADVANCED_FACE ( 'NONE', ( #6955 ), #67813, .T. ) ;
#62639 = CARTESIAN_POINT ( 'NONE',  ( 34.10416666666665719, 2.130196079827498146, 7.949999999999958433 ) ) ;
#62640 = CARTESIAN_POINT ( 'NONE',  ( 42.87543019189810423, -5.291415217122920289, -3.055000000000001492 ) ) ;
#62641 = VERTEX_POINT ( 'NONE', #19310 ) ;
#62642 = ORIENTED_EDGE ( 'NONE', *, *, #135821, .F. ) ;
#62643 = ORIENTED_EDGE ( 'NONE', *, *, #86110, .F. ) ;
#62644 = AXIS2_PLACEMENT_3D ( 'NONE', #50076, #60990, #14575 ) ;
#62645 = CARTESIAN_POINT ( 'NONE',  ( 36.48921356237310221, -27.52281430457080802, 5.000000000000000000 ) ) ;
#62646 = CARTESIAN_POINT ( 'NONE',  ( -31.49999999999978684, 8.319652575858354382, -8.582050562765896728 ) ) ;
#62647 = CARTESIAN_POINT ( 'NONE',  ( -3.489213562373097322, -27.52281430457057709, 5.000000000000000000 ) ) ;
#62648 = DIRECTION ( 'NONE',  ( -1.000000000000000000, -1.224606353822377258E-16, -0.000000000000000000 ) ) ;
#62649 = DIRECTION ( 'NONE',  ( 0.7071067811865487940, 0.7071067811865463515, 0.000000000000000000 ) ) ;
#62650 = DIRECTION ( 'NONE',  ( -0.7071067811865486830, -0.7071067811865464625, 0.000000000000000000 ) ) ;
#62652 = ORIENTED_EDGE ( 'NONE', *, *, #104680, .T. ) ;
#62651 = CARTESIAN_POINT ( 'NONE',  ( -16.55914779396249514, 0.6742760034310938400, -33.57941237570724979 ) ) ;
#62653 = CARTESIAN_POINT ( 'NONE',  ( 21.29974487139158512, -27.71228299555221142, 4.000000000000000000 ) ) ;
#62654 = DIRECTION ( 'NONE',  ( 0.7071067811865487940, 0.7071067811865463515, 0.000000000000000000 ) ) ;
#62655 = CARTESIAN_POINT ( 'NONE',  ( 27.29974487139158512, -27.71228299555225405, 4.000000000000000000 ) ) ;
#62656 = CONICAL_SURFACE ( 'NONE', #111258, 1.749999999999999778, 0.7853981633974480570 ) ;
#62657 = LINE ( 'NONE', #139532, #53024 ) ;
#62658 = AXIS2_PLACEMENT_3D ( 'NONE', #110840, #34055, #131937 ) ;
#62659 = ORIENTED_EDGE ( 'NONE', *, *, #102259, .T. ) ;
#62660 = EDGE_CURVE ( 'NONE', #28277, #57736, #131654, .T. ) ;
#62661 = ORIENTED_EDGE ( 'NONE', *, *, #106155, .T. ) ;
#62662 = CARTESIAN_POINT ( 'NONE',  ( 88.74586038379622721, 3.974999999999996980, 6.884901960086287964 ) ) ;
#62663 = CARTESIAN_POINT ( 'NONE',  ( 79.53709685856478018, -3.054999999999998828, -5.291415217122919401 ) ) ;
#62664 = EDGE_CURVE ( 'NONE', #36664, #88273, #73950, .T. ) ;
#62665 = DIRECTION ( 'NONE',  ( 0.6830127018922180770, -0.6830127018922204085, -0.2588190451025213501 ) ) ;
#62666 = LINE ( 'NONE', #52477, #75534 ) ;
#62667 = CARTESIAN_POINT ( 'NONE',  ( 72.99586038379622721, -3.974999999999998312, -6.884901960086286188 ) ) ;
#62668 = ORIENTED_EDGE ( 'NONE', *, *, #85923, .T. ) ;
#62669 = ORIENTED_EDGE ( 'NONE', *, *, #95824, .T. ) ;
#62670 = DIRECTION ( 'NONE',  ( 0.7071067811865487940, -0.7071067811865463515, 0.000000000000000000 ) ) ;
#62672 = CIRCLE ( 'NONE', #67326, 2.500000000000000444 ) ;
#62671 = CARTESIAN_POINT ( 'NONE',  ( -23.99999999999983658, 18.08204922493371214, 0.9627537363045436392 ) ) ;
#62673 = ORIENTED_EDGE ( 'NONE', *, *, #136031, .F. ) ;
#62674 = EDGE_CURVE ( 'NONE', #58061, #55041, #127124, .T. ) ;
#62675 = EDGE_CURVE ( 'NONE', #84892, #111297, #89556, .T. ) ;
#62677 = ORIENTED_EDGE ( 'NONE', *, *, #79496, .F. ) ;
#62676 = AXIS2_PLACEMENT_3D ( 'NONE', #127927, #72868, #103981 ) ;
#62678 = PLANE ( 'NONE',  #130069 ) ;
#62679 = VERTEX_POINT ( 'NONE', #143230 ) ;
#62680 = CARTESIAN_POINT ( 'NONE',  ( 0.4436723136282649804, 0.5999999999999987566, 4.148801034132802990 ) ) ;
#62681 = CIRCLE ( 'NONE', #110, 5.968999999999998529 ) ;
#62682 = VECTOR ( 'NONE', #62798, 1000.000000000000000 ) ;
#62683 = VECTOR ( 'NONE', #139065, 1000.000000000000000 ) ;
#62684 = VECTOR ( 'NONE', #87364, 1000.000000000000000 ) ;
#62685 = VECTOR ( 'NONE', #14913, 1000.000000000000000 ) ;
#62686 = DIRECTION ( 'NONE',  ( 0.6830127018922181881, 0.6830127018922202975, -0.2588190451025214056 ) ) ;
#62687 = EDGE_CURVE ( 'NONE', #63098, #61017, #43929, .T. ) ;
#62688 = FACE_BOUND ( 'NONE', #7199, .T. ) ;
#62689 = ADVANCED_FACE ( 'NONE', ( #98309 ), #11985, .F. ) ;
#62690 = DIRECTION ( 'NONE',  ( 1.000000000000000000, 0.000000000000000000, 0.000000000000000000 ) ) ;
#62691 = CARTESIAN_POINT ( 'NONE',  ( 0.000000000000000000, -21.72500000000000142, 4.500000000000000888 ) ) ;
#62693 = DIRECTION ( 'NONE',  ( -0.7071067811865487940, 0.7071067811865463515, 0.000000000000000000 ) ) ;
#62692 = AXIS2_PLACEMENT_3D ( 'NONE', #116638, #40524, #28215 ) ;
#62695 = ORIENTED_EDGE ( 'NONE', *, *, #49638, .T. ) ;
#62694 = CARTESIAN_POINT ( 'NONE',  ( 0.1839886062690032631, 28.73617430169787568, 5.000000000000000000 ) ) ;
#62696 =( NAMED_UNIT ( * ) PLANE_ANGLE_UNIT ( ) SI_UNIT ( $, .RADIAN. ) );
#62698 = EDGE_CURVE ( 'NONE', #39646, #109641, #9093, .T. ) ;
#62697 = APPLICATION_PROTOCOL_DEFINITION ( 'draft international standard', 'automotive_design', 1998, #57807 ) ;
#62699 = VERTEX_POINT ( 'NONE', #88150 ) ;
#62700 = ORIENTED_EDGE ( 'NONE', *, *, #113244, .T. ) ;
#62701 = CARTESIAN_POINT ( 'NONE',  ( 82.74543019189812298, -5.291415217122918513, -3.055000000000000160 ) ) ;
#62702 = ORIENTED_EDGE ( 'NONE', *, *, #108791, .F. ) ;
#62703 = CARTESIAN_POINT ( 'NONE',  ( -34.42500000000001137, -22.22500000000000142, 5.000000000000000000 ) ) ;
#62704 = LINE ( 'NONE', #27909, #242 ) ;
#62705 = AXIS2_PLACEMENT_3D ( 'NONE', #128732, #130904, #9801 ) ;
#62706 = DIRECTION ( 'NONE',  ( -0.3543493200069162685, -0.000000000000000000, -0.9351131265310288487 ) ) ;
#62707 = EDGE_CURVE ( 'NONE', #100524, #81804, #88875, .T. ) ;
#62708 = VECTOR ( 'NONE', #107910, 1000.000000000000000 ) ;
#62709 = CARTESIAN_POINT ( 'NONE',  ( 45.29974487139158867, -27.71228299555237840, 4.000000000000000000 ) ) ;
#62710 = DIRECTION ( 'NONE',  ( 0.7071067811865486830, -0.7071067811865464625, -0.000000000000000000 ) ) ;
#62711 = VECTOR ( 'NONE', #49655, 1000.000000000000000 ) ;
#62712 = CARTESIAN_POINT ( 'NONE',  ( 11.20710678118647152, -2.240707523384259492, 5.000000000000000000 ) ) ;
#62713 = CARTESIAN_POINT ( 'NONE',  ( 9.370933818357753964, 3.061616997868383634E-16, -2.500000000000000444 ) ) ;
#62714 = PLANE ( 'NONE',  #75169 ) ;
#62715 = AXIS2_PLACEMENT_3D ( 'NONE', #13907, #14652, #89353 ) ;
#62716 = CARTESIAN_POINT ( 'NONE',  ( 39.29974487139159578, -27.71228299555233576, 4.000000000000000000 ) ) ;
#62717 = DIRECTION ( 'NONE',  ( 0.6830127018922181881, 0.6830127018922202975, -0.2588190451025214056 ) ) ;
#62718 = EDGE_CURVE ( 'NONE', #13719, #124122, #132394, .T. ) ;
#62719 = CARTESIAN_POINT ( 'NONE',  ( -34.49999999999976552, 0.4311230773921780335, 4.000000000000000000 ) ) ;
#62720 = ORIENTED_EDGE ( 'NONE', *, *, #36611, .F. ) ;
#62721 = AXIS2_PLACEMENT_3D ( 'NONE', #108737, #140002, #83466 ) ;
#62722 = DIRECTION ( 'NONE',  ( -0.000000000000000000, 0.3543493200069153248, 0.9351131265310292928 ) ) ;
#62723 = DIRECTION ( 'NONE',  ( -0.7071067811865486830, 0.7071067811865464625, 0.000000000000000000 ) ) ;
#62724 = EDGE_LOOP ( 'NONE', ( #40917, #62602, #2901, #34311 ) ) ;
#62725 = EDGE_LOOP ( 'NONE', ( #102447, #43521, #122974, #94509 ) ) ;
#62726 = AXIS2_PLACEMENT_3D ( 'NONE', #124270, #16184, #138012 ) ;
#62727 = ORIENTED_EDGE ( 'NONE', *, *, #3778, .T. ) ;
#62728 = ADVANCED_FACE ( 'NONE', ( #87436 ), #11251, .F. ) ;
#62729 = CARTESIAN_POINT ( 'NONE',  ( 32.08376352523143993, -6.110000000000001208, -3.741295971395164515E-16 ) ) ;
#62730 = ADVANCED_FACE ( 'NONE', ( #121464 ), #9851, .F. ) ;
#62731 = ORIENTED_EDGE ( 'NONE', *, *, #111556, .T. ) ;
#62732 = DIRECTION ( 'NONE',  ( 0.7071067811865487940, 0.7071067811865463515, 0.000000000000000000 ) ) ;
#62733 = EDGE_CURVE ( 'NONE', #42516, #138332, #124866, .T. ) ;
#62734 = AXIS2_PLACEMENT_3D ( 'NONE', #3877, #37277, #126406 ) ;
#62735 = CARTESIAN_POINT ( 'NONE',  ( 14.04580628287044064, 5.278424836066143655, -3.047499999999997655 ) ) ;
#62736 = CARTESIAN_POINT ( 'NONE',  ( 12.10645530542133841, 7.761932032390377323, -28.16843179005226006 ) ) ;
#62737 = ORIENTED_EDGE ( 'NONE', *, *, #52215, .T. ) ;
#62738 = DIRECTION ( 'NONE',  ( -0.7071067811865487940, 0.7071067811865463515, 0.000000000000000000 ) ) ;
#62739 = ORIENTED_EDGE ( 'NONE', *, *, #71853, .T. ) ;
#62740 = FACE_OUTER_BOUND ( 'NONE', #133154, .T. ) ;
#62741 = CYLINDRICAL_SURFACE ( 'NONE', #19740, 0.5000000000000004441 ) ;
#62743 = VERTEX_POINT ( 'NONE', #78690 ) ;
#62742 = CARTESIAN_POINT ( 'NONE',  ( 15.99507522778795909, -5.240707523384225297, 12.38332538355492218 ) ) ;
#62744 = ORIENTED_EDGE ( 'NONE', *, *, #139622, .T. ) ;
#62745 = PLANE ( 'NONE',  #537 ) ;
#62746 = VERTEX_POINT ( 'NONE', #64249 ) ;
#62747 = DIRECTION ( 'NONE',  ( -0.6830127018922180770, -0.6830127018922204085, -0.2588190451025213501 ) ) ;
#62748 = ORIENTED_EDGE ( 'NONE', *, *, #112443, .F. ) ;
#62749 = VERTEX_POINT ( 'NONE', #54121 ) ;
#62750 = ORIENTED_EDGE ( 'NONE', *, *, #125600, .T. ) ;
#62751 = VERTEX_POINT ( 'NONE', #110571 ) ;
#62752 = LINE ( 'NONE', #49018, #30973 ) ;
#62753 = VECTOR ( 'NONE', #31708, 1000.000000000000000 ) ;
#62754 = DIRECTION ( 'NONE',  ( -0.7071067811865487940, 0.7071067811865463515, 0.000000000000000000 ) ) ;
#62755 = CARTESIAN_POINT ( 'NONE',  ( 62.99451991528749772, 28.92564299267982264, 4.000000000000000000 ) ) ;
#62756 = LINE ( 'NONE', #106942, #107275 ) ;
#62757 = CARTESIAN_POINT ( 'NONE',  ( -34.49999999999975842, -6.839392718269155402, -8.480912228396004338 ) ) ;
#62758 = ORIENTED_EDGE ( 'NONE', *, *, #83919, .T. ) ;
#62759 = CARTESIAN_POINT ( 'NONE',  ( -45.18398860626900415, 28.73617430169818832, 5.000000000000000000 ) ) ;
#62760 = EDGE_LOOP ( 'NONE', ( #9621, #6729, #76450 ) ) ;
#62761 = AXIS2_PLACEMENT_3D ( 'NONE', #52265, #97159, #141424 ) ;
#62762 = LINE ( 'NONE', #106949, #44862 ) ;
#62763 = CARTESIAN_POINT ( 'NONE',  ( 32.93706980810188156, 2.126176841940952134, -7.934999999999993392 ) ) ;
#62764 = CARTESIAN_POINT ( 'NONE',  ( -66.48921356237309510, -27.52281430457101763, 5.000000000000000000 ) ) ;
#62765 = ORIENTED_EDGE ( 'NONE', *, *, #17777, .T. ) ;
#62766 = PLANE ( 'NONE',  #66923 ) ;
#62767 = PRESENTATION_STYLE_ASSIGNMENT (( #117803 ) ) ;
#62768 = ORIENTED_EDGE ( 'NONE', *, *, #105168, .F. ) ;
#62769 = VERTEX_POINT ( 'NONE', #108412 ) ;
#62770 = ADVANCED_FACE ( 'NONE', ( #111296 ), #53360, .F. ) ;
#62771 = EDGE_LOOP ( 'NONE', ( #119194, #116691, #71340, #20007 ) ) ;
#62772 = DIRECTION ( 'NONE',  ( -0.6830127018922181881, 0.6830127018922202975, -0.2588190451025214056 ) ) ;
#62773 = FACE_OUTER_BOUND ( 'NONE', #10311, .T. ) ;
#62774 = EDGE_CURVE ( 'NONE', #121745, #112217, #114849, .T. ) ;
#62775 = DIRECTION ( 'NONE',  ( -1.000000000000000000, 0.000000000000000000, 0.000000000000000000 ) ) ;
#62776 = DIRECTION ( 'NONE',  ( -0.000000000000000000, 0.000000000000000000, 1.000000000000000000 ) ) ;
#62777 = VECTOR ( 'NONE', #34209, 1000.000000000000000 ) ;
#62778 = CARTESIAN_POINT ( 'NONE',  ( 3.298144211979623819, -48.98056306480231825, -39.49745726092410791 ) ) ;
#62779 = CARTESIAN_POINT ( 'NONE',  ( 79.39126352523146579, -4.472830434245839371, -4.472830434245839371 ) ) ;
#62780 = PLANE ( 'NONE',  #127472 ) ;
#62781 = VECTOR ( 'NONE', #45435, 999.9999999999998863 ) ;
#62782 = AXIS2_PLACEMENT_3D ( 'NONE', #43408, #6616, #143422 ) ;
#62783 = CARTESIAN_POINT ( 'NONE',  ( 34.92499999999998295, 3.856123077392373144, 4.000000000000000000 ) ) ;
#62784 = DIRECTION ( 'NONE',  ( 0.6830127018922181881, 0.6830127018922202975, -0.2588190451025214056 ) ) ;
#62785 = LINE ( 'NONE', #96087, #60635 ) ;
#62786 = ORIENTED_EDGE ( 'NONE', *, *, #3323, .T. ) ;
#62787 = CARTESIAN_POINT ( 'NONE',  ( -32.99451991528749062, 28.92564299267960948, 4.000000000000000000 ) ) ;
#62788 = ORIENTED_EDGE ( 'NONE', *, *, #10334, .F. ) ;
#62789 = MECHANICAL_DESIGN_GEOMETRIC_PRESENTATION_REPRESENTATION (  '', ( #141518 ), #122997 ) ;
#62790 = AXIS2_PLACEMENT_3D ( 'NONE', #94494, #5337, #115504 ) ;
#62791 = VECTOR ( 'NONE', #131962, 1000.000000000000000 ) ;
#62792 = CARTESIAN_POINT ( 'NONE',  ( 16.63753812416085509, 22.22500000000000142, 4.000000000000000000 ) ) ;
#62794 = CARTESIAN_POINT ( 'NONE',  ( 26.99451991528749417, 28.92564299267956685, 4.000000000000000000 ) ) ;
#62793 = CIRCLE ( 'NONE', #97523, 2.500000000000000444 ) ;
#62795 = VERTEX_POINT ( 'NONE', #35213 ) ;
#62796 = CIRCLE ( 'NONE', #127665, 2.500000000000000888 ) ;
#62797 = DIRECTION ( 'NONE',  ( 1.000000000000000000, 0.000000000000000000, 0.000000000000000000 ) ) ;
#62799 = VERTEX_POINT ( 'NONE', #4620 ) ;
#62798 = DIRECTION ( 'NONE',  ( -0.7071067811865486830, -0.7071067811865464625, 0.000000000000000000 ) ) ;
#62800 = EDGE_CURVE ( 'NONE', #57534, #84656, #103976, .T. ) ;
#62801 = PLANE ( 'NONE',  #139021 ) ;
#62802 = CARTESIAN_POINT ( 'NONE',  ( -27.29974487139158512, -27.71228299555225405, 4.000000000000000000 ) ) ;
#62803 = EDGE_LOOP ( 'NONE', ( #116910, #86416 ) ) ;
#62804 = EDGE_CURVE ( 'NONE', #49877, #19355, #38055, .T. ) ;
#62805 = EDGE_LOOP ( 'NONE', ( #130112, #132313, #98611, #31842, #106181 ) ) ;
#62806 = LINE ( 'NONE', #106984, #42190 ) ;
#62807 = VECTOR ( 'NONE', #35381, 999.9999999999998863 ) ;
#62808 = LINE ( 'NONE', #84552, #82061 ) ;
#62809 = CARTESIAN_POINT ( 'NONE',  ( 93.85002705046289861, -5.819803920172572198, -5.819803920172572198 ) ) ;
#62810 = LINE ( 'NONE', #109136, #23104 ) ;
#62811 = DIRECTION ( 'NONE',  ( -1.000000000000000000, -0.000000000000000000, -0.000000000000000000 ) ) ;
#62812 = VERTEX_POINT ( 'NONE', #93135 ) ;
#62813 = EDGE_CURVE ( 'NONE', #46898, #15867, #12694, .T. ) ;
#62814 = VECTOR ( 'NONE', #124373, 1000.000000000000000 ) ;
#62815 = CARTESIAN_POINT ( 'NONE',  ( -48.48921356237309510, -27.52281430457089328, 5.000000000000000000 ) ) ;
#62816 = LINE ( 'NONE', #60695, #94766 ) ;
#62817 = LINE ( 'NONE', #84563, #75240 ) ;
#62818 = CARTESIAN_POINT ( 'NONE',  ( -11.70025512860841133, -27.71228299555198049, 4.000000000000000000 ) ) ;
#62819 = EDGE_LOOP ( 'NONE', ( #87800, #135293, #17786, #91579 ) ) ;
#62820 = EDGE_CURVE ( 'NONE', #55970, #111086, #80850, .T. ) ;
#62821 = VECTOR ( 'NONE', #4473, 1000.000000000000000 ) ;
#62822 = CARTESIAN_POINT ( 'NONE',  ( 45.87086038379622721, 6.884901960086289741, -3.974999999999993427 ) ) ;
#62823 = EDGE_LOOP ( 'NONE', ( #142952, #51330, #130065, #42898 ) ) ;
#62824 = VECTOR ( 'NONE', #59992, 1000.000000000000000 ) ;
#62825 = CARTESIAN_POINT ( 'NONE',  ( 86.04209685856477563, 5.291415217122923842, -3.054999999999996163 ) ) ;
#62826 = AXIS2_PLACEMENT_3D ( 'NONE', #66632, #122410, #142065 ) ;
#62827 = DIRECTION ( 'NONE',  ( 0.7071067811865487940, 0.7071067811865463515, 0.000000000000000000 ) ) ;
#62828 = LINE ( 'NONE', #7687, #74802 ) ;
#62829 = ORIENTED_EDGE ( 'NONE', *, *, #129670, .F. ) ;
#62830 = ADVANCED_FACE ( 'NONE', ( #125040 ), #67858, .F. ) ;
#62831 = VECTOR ( 'NONE', #103588, 1000.000000000000000 ) ;
#62832 = DIRECTION ( 'NONE',  ( -0.5735764363510507113, 0.8191520442889885789, 1.003171929053520926E-16 ) ) ;
#62833 = DIRECTION ( 'NONE',  ( -0.7071067811865486830, -0.7071067811865464625, 0.000000000000000000 ) ) ;
#62834 = AXIS2_PLACEMENT_3D ( 'NONE', #115313, #92890, #139287 ) ;
#62836 = ORIENTED_EDGE ( 'NONE', *, *, #25016, .T. ) ;
#62835 = PLANE ( 'NONE',  #75309 ) ;
#62837 = CARTESIAN_POINT ( 'NONE',  ( 12.97916666666666607, 6.094999999999988205, -1.633150327867694651 ) ) ;
#62838 = CARTESIAN_POINT ( 'NONE',  ( 22.49999999999985079, -17.94781430457063820, 5.000000000000000000 ) ) ;
#62839 = DIRECTION ( 'NONE',  ( 0.000000000000000000, -1.000000000000000000, 0.000000000000000000 ) ) ;
#62840 = DIRECTION ( 'NONE',  ( -0.6830127018922180770, -0.6830127018922204085, -0.2588190451025213501 ) ) ;
#62841 = VERTEX_POINT ( 'NONE', #101140 ) ;
#62842 = EDGE_LOOP ( 'NONE', ( #6056, #120385, #22903, #86946 ) ) ;
#62843 = CARTESIAN_POINT ( 'NONE',  ( 78.16709685856476142, -3.055000000000000160, -5.291415217122921177 ) ) ;
#62844 = VERTEX_POINT ( 'NONE', #136622 ) ;
#62845 = LINE ( 'NONE', #130957, #89262 ) ;
#62846 = EDGE_CURVE ( 'NONE', #58174, #3994, #69255, .T. ) ;
#62847 = PLANE ( 'NONE',  #15591 ) ;
#62848 = COLOUR_RGB ( '', 0.40784314, 0.44705882, 0.49803922) ;
#62849 = LINE ( 'NONE', #70872, #98677 ) ;
#62850 = ORIENTED_EDGE ( 'NONE', *, *, #21271, .F. ) ;
#62851 = AXIS2_PLACEMENT_3D ( 'NONE', #91134, #128558, #62595 ) ;
#62852 = DIRECTION ( 'NONE',  ( -1.000000000000000000, -0.000000000000000000, -0.000000000000000000 ) ) ;
#62853 = DIRECTION ( 'NONE',  ( 0.6830127018922180770, -0.6830127018922204085, -0.2588190451025213501 ) ) ;
#62854 = ADVANCED_FACE ( 'NONE', ( #37334 ), #1786, .T. ) ;
#62855 = EDGE_CURVE ( 'NONE', #102772, #129516, #113436, .T. ) ;
#62856 = ORIENTED_EDGE ( 'NONE', *, *, #65433, .F. ) ;
#62857 = PLANE ( 'NONE',  #127695 ) ;
#62858 = VECTOR ( 'NONE', #31783, 1000.000000000000000 ) ;
#62859 = CARTESIAN_POINT ( 'NONE',  ( 33.03752705046289151, -9.735942053221456900E-16, 7.949999999999998401 ) ) ;
#62860 = CARTESIAN_POINT ( 'NONE',  ( -12.48921356237309155, -27.52281430457064104, 5.000000000000000000 ) ) ;
#62861 = VECTOR ( 'NONE', #68154, 1000.000000000000000 ) ;
#62862 = EDGE_CURVE ( 'NONE', #80081, #17782, #39185, .T. ) ;
#62863 = EDGE_LOOP ( 'NONE', ( #68759, #77887, #10321, #50474 ) ) ;
#62864 = ORIENTED_EDGE ( 'NONE', *, *, #116977, .F. ) ;
#62865 = EDGE_CURVE ( 'NONE', #135680, #30212, #112738, .T. ) ;
#62866 = PLANE ( 'NONE',  #8289 ) ;
#62867 = ADVANCED_FACE ( 'NONE', ( #91697 ), #69999, .F. ) ;
#62868 = CARTESIAN_POINT ( 'NONE',  ( -26.99451991528749417, 28.92564299267956685, 4.000000000000000000 ) ) ;
#62869 = CARTESIAN_POINT ( 'NONE',  ( 21.18398860626899349, 28.73617430169802134, 5.000000000000000000 ) ) ;
#62870 = CARTESIAN_POINT ( 'NONE',  ( 8.999999999999932498, 14.87792677143809783, -11.06722581663437843 ) ) ;
#62871 = SURFACE_SIDE_STYLE ('',( #8412 ) ) ;
#62872 = AXIS2_PLACEMENT_3D ( 'NONE', #56952, #77971, #122152 ) ;
#62873 =( LENGTH_UNIT ( ) NAMED_UNIT ( * ) SI_UNIT ( .MILLI., .METRE. ) );
#62874 = DIRECTION ( 'NONE',  ( 1.000000000000000000, 0.000000000000000000, 0.000000000000000000 ) ) ;
#62875 = ORIENTED_EDGE ( 'NONE', *, *, #116127, .T. ) ;
#62876 = ORIENTED_EDGE ( 'NONE', *, *, #113503, .T. ) ;
#62877 = EDGE_LOOP ( 'NONE', ( #128436, #102690, #80511, #50070 ) ) ;
#62878 = EDGE_CURVE ( 'NONE', #88267, #125403, #104715, .T. ) ;
#62879 = ORIENTED_EDGE ( 'NONE', *, *, #32571, .T. ) ;
#62880 = CARTESIAN_POINT ( 'NONE',  ( 184.0378153480267258, -51.37040454773216425, 37.49526731630399468 ) ) ;
#62882 = EDGE_CURVE ( 'NONE', #81729, #122429, #115552, .T. ) ;
#62881 = AXIS2_PLACEMENT_3D ( 'NONE', #42622, #107819, #54911 ) ;
#62883 =( NAMED_UNIT ( * ) SI_UNIT ( $, .STERADIAN. ) SOLID_ANGLE_UNIT ( ) );
#62884 = VECTOR ( 'NONE', #121490, 1000.000000000000000 ) ;
#62885 = ORIENTED_EDGE ( 'NONE', *, *, #141195, .F. ) ;
#62886 = CARTESIAN_POINT ( 'NONE',  ( 0.000000000000000000, 2.375000000000000000, 4.319999999999998508 ) ) ;
#62887 = DIRECTION ( 'NONE',  ( -0.5735764363510503783, -0.8191520442889886899, 0.000000000000000000 ) ) ;
#62888 = CARTESIAN_POINT ( 'NONE',  ( 4.110173228882081808, -22.22499999999999787, 4.785647885939356527 ) ) ;
#62889 = CARTESIAN_POINT ( 'NONE',  ( 38.99451991528749062, 28.92564299267965211, 4.000000000000000000 ) ) ;
#62890 = VECTOR ( 'NONE', #59923, 1000.000000000000000 ) ;
#62891 = AXIS2_PLACEMENT_3D ( 'NONE', #113224, #24098, #88653 ) ;
#62892 = VECTOR ( 'NONE', #118740, 1000.000000000000227 ) ;
#62893 = VECTOR ( 'NONE', #14859, 1000.000000000000000 ) ;
#62894 = CARTESIAN_POINT ( 'NONE',  ( 42.18398860626899705, 28.73617430169816700, 5.000000000000000000 ) ) ;
#62895 = ORIENTED_EDGE ( 'NONE', *, *, #17488, .T. ) ;
#62896 = VECTOR ( 'NONE', #29721, 1000.000000000000000 ) ;
#62897 = LINE ( 'NONE', #54178, #31015 ) ;
#62898 = FACE_OUTER_BOUND ( 'NONE', #109496, .T. ) ;
#62899 = EDGE_LOOP ( 'NONE', ( #38137, #80262, #119342, #42559 ) ) ;
#62900 = CARTESIAN_POINT ( 'NONE',  ( -13.44665057663210028, 2.259292476615697876, 14.86850063742357619 ) ) ;
#62901 = ORIENTED_EDGE ( 'NONE', *, *, #58459, .T. ) ;
#62902 = CARTESIAN_POINT ( 'NONE',  ( -39.18398860626899705, 28.73617430169814568, 5.000000000000000000 ) ) ;
#62903 = ORIENTED_EDGE ( 'NONE', *, *, #87073, .T. ) ;
#62904 = VECTOR ( 'NONE', #30742, 1000.000000000000000 ) ;
#62905 = CARTESIAN_POINT ( 'NONE',  ( 65.04209685856477563, 5.291415217122923842, -3.054999999999996163 ) ) ;
#62906 = EDGE_CURVE ( 'NONE', #92329, #91589, #40899, .T. ) ;
#62907 = ORIENTED_EDGE ( 'NONE', *, *, #54166, .T. ) ;
#62908 = VERTEX_POINT ( 'NONE', #85104 ) ;
#62909 = EDGE_CURVE ( 'NONE', #27017, #141849, #93839, .T. ) ;
#62910 = DIRECTION ( 'NONE',  ( -1.000000000000000000, -1.224606353822377258E-16, -0.000000000000000000 ) ) ;
#62911 = EDGE_CURVE ( 'NONE', #49447, #57736, #29292, .T. ) ;
#62912 = PLANE ( 'NONE',  #12598 ) ;
#62913 = CARTESIAN_POINT ( 'NONE',  ( 113.4587635252314470, 0.000000000000000000, -6.110000000000001208 ) ) ;
#62914 = DIRECTION ( 'NONE',  ( -0.7071067811865486830, -0.7071067811865464625, 0.000000000000000000 ) ) ;
#62915 = VECTOR ( 'NONE', #86597, 1000.000000000000000 ) ;
#62916 = DIRECTION ( 'NONE',  ( -0.6830127018922181881, 0.6830127018922202975, -0.2588190451025214056 ) ) ;
#62917 = LINE ( 'NONE', #107093, #122790 ) ;
#62918 = ADVANCED_FACE ( 'NONE', ( #52467 ), #107565, .F. ) ;
#62919 = DIRECTION ( 'NONE',  ( 0.6830127018922181881, 0.6830127018922202975, -0.2588190451025214056 ) ) ;
#62920 = CARTESIAN_POINT ( 'NONE',  ( -27.48921356237309155, -27.52281430457074762, 5.000000000000000000 ) ) ;
#62921 = VECTOR ( 'NONE', #105105, 1000.000000000000227 ) ;
#62922 = PLANE ( 'NONE',  #86818 ) ;
#62923 = ORIENTED_EDGE ( 'NONE', *, *, #39874, .F. ) ;
#62924 = DIRECTION ( 'NONE',  ( -0.000000000000000000, 0.000000000000000000, 1.000000000000000000 ) ) ;
#62925 = CARTESIAN_POINT ( 'NONE',  ( 0.8348607551137287031, 0.4000000000000001887, -2.317232462839658336 ) ) ;
#62926 = EDGE_LOOP ( 'NONE', ( #79964, #47499, #139014, #138276 ) ) ;
#62927 = VECTOR ( 'NONE', #10613, 1000.000000000000000 ) ;
#62928 = VERTEX_POINT ( 'NONE', #28607 ) ;
#62929 = ORIENTED_EDGE ( 'NONE', *, *, #22242, .T. ) ;
#62930 = EDGE_LOOP ( 'NONE', ( #1178, #5360, #79623, #66525 ) ) ;
#62931 = CARTESIAN_POINT ( 'NONE',  ( 8.671830600776411657, -15.74070752338412049, 4.000000000000000000 ) ) ;
#62932 = DIRECTION ( 'NONE',  ( -0.7071067811865486830, -0.7071067811865464625, -0.000000000000000000 ) ) ;
#62933 = CARTESIAN_POINT ( 'NONE',  ( -33.29974487139158867, -27.71228299555229313, 4.000000000000000000 ) ) ;
#62934 = VERTEX_POINT ( 'NONE', #5381 ) ;
#62935 = CARTESIAN_POINT ( 'NONE',  ( 0.5414528859217531132, -52.10163751122425424, 40.43817685073605617 ) ) ;
#62936 = VERTEX_POINT ( 'NONE', #106113 ) ;
#62937 = AXIS2_PLACEMENT_3D ( 'NONE', #27911, #137401, #38096 ) ;
#62938 =( BOUNDED_CURVE ( )  B_SPLINE_CURVE ( 3, ( #50125, #7290, #39986, #84203 ),
 .UNSPECIFIED., .F., .T. ) 
 B_SPLINE_CURVE_WITH_KNOTS ( ( 4, 4 ),
 ( 5.135034128376270601, 5.164990091338616196 ),
 .UNSPECIFIED. ) 
 CURVE ( )  GEOMETRIC_REPRESENTATION_ITEM ( )  RATIONAL_B_SPLINE_CURVE ( ( 1.000000000000000000, 0.9999252214215840207, 0.9999252214215840207, 1.000000000000000000 ) ) 
 REPRESENTATION_ITEM ( '' )  );
#62939 = CARTESIAN_POINT ( 'NONE',  ( 6.395403141435219929, 2.126176841940962348, 7.934999999999989839 ) ) ;
#62940 = DIRECTION ( 'NONE',  ( -0.7071067811865486830, -0.7071067811865464625, 0.000000000000000000 ) ) ;
#62941 = DIRECTION ( 'NONE',  ( -0.7071067811865486830, -0.7071067811865464625, 0.000000000000000000 ) ) ;
#62942 = CARTESIAN_POINT ( 'NONE',  ( 10.90341945100486143, -8.451216681753212612, -4.339032109071985666 ) ) ;
#62943 = ORIENTED_EDGE ( 'NONE', *, *, #2512, .T. ) ;
#62944 = ORIENTED_EDGE ( 'NONE', *, *, #130924, .T. ) ;
#62945 = EDGE_CURVE ( 'NONE', #114730, #90903, #102295, .T. ) ;
#62946 = VECTOR ( 'NONE', #140545, 1000.000000000000000 ) ;
#62947 = ORIENTED_EDGE ( 'NONE', *, *, #76028, .T. ) ;
#62948 = PLANE ( 'NONE',  #118134 ) ;
#62949 = CARTESIAN_POINT ( 'NONE',  ( 23.99999999999983658, -7.447814304570756327, 5.000000000000000000 ) ) ;
#62950 = CARTESIAN_POINT ( 'NONE',  ( -45.48921356237309510, -27.52281430457087197, 5.000000000000000000 ) ) ;
#62951 = VECTOR ( 'NONE', #112846, 1000.000000000000000 ) ;
#62952 = CARTESIAN_POINT ( 'NONE',  ( -14.48334561358944761, 22.22500000000000142, 4.500000000000000888 ) ) ;
#62953 = DIRECTION ( 'NONE',  ( -0.6830127018922181881, 0.6830127018922202975, -0.2588190451025214056 ) ) ;
#62954 = CARTESIAN_POINT ( 'NONE',  ( 34.92499999999998295, -13.29806943317888468, 4.500000000000000888 ) ) ;
#62955 = CARTESIAN_POINT ( 'NONE',  ( -8.292893218813391698, -3.740707523384241728, 5.000000000000000000 ) ) ;
#62956 = LINE ( 'NONE', #41165, #22928 ) ;
#62957 = CARTESIAN_POINT ( 'NONE',  ( 26.97959685856476497, 6.109999999999999432, 1.637169565754164280 ) ) ;
#62958 = DIRECTION ( 'NONE',  ( -0.000000000000000000, -0.3543493200069152693, 0.9351131265310292928 ) ) ;
#62959 = CARTESIAN_POINT ( 'NONE',  ( 15.47336096364205638, -5.240707523384225297, 16.25846745537499416 ) ) ;
#62960 = EDGE_LOOP ( 'NONE', ( #60309, #15246, #93423, #89099 ) ) ;
#62961 = DIRECTION ( 'NONE',  ( -0.7071067811865486830, -0.7071067811865464625, -0.000000000000000000 ) ) ;
#62962 = CIRCLE ( 'NONE', #88410, 28.00000000000001776 ) ;
#62963 = CARTESIAN_POINT ( 'NONE',  ( -2.999999999999985345, 4.965500833774324718, -4.007596771432649696 ) ) ;
#62964 = ORIENTED_EDGE ( 'NONE', *, *, #109458, .T. ) ;
#62965 = EDGE_CURVE ( 'NONE', #121666, #91502, #73534, .T. ) ;
#62966 = CARTESIAN_POINT ( 'NONE',  ( 33.70701326429281153, -21.74070752338406365, 4.999753212805220670 ) ) ;
#62968 = EDGE_LOOP ( 'NONE', ( #111817, #34611, #86030, #114375 ) ) ;
#62967 = CARTESIAN_POINT ( 'NONE',  ( 54.91896556007530705, -47.51495700085917662, -36.79359617903136126 ) ) ;
#62969 = EDGE_CURVE ( 'NONE', #62317, #20476, #83720, .T. ) ;
#62970 = CYLINDRICAL_SURFACE ( 'NONE', #97825, 0.5000000000000004441 ) ;
#62971 = DIRECTION ( 'NONE',  ( -0.7071067811865487940, 0.7071067811865463515, 0.000000000000000000 ) ) ;
#62973 = ORIENTED_EDGE ( 'NONE', *, *, #50684, .T. ) ;
#62972 = AXIS2_PLACEMENT_3D ( 'NONE', #52936, #21032, #87025 ) ;
#62974 = CARTESIAN_POINT ( 'NONE',  ( 0.000000000000000000, 9.735942053221458872E-16, -7.950000000000000178 ) ) ;
#62975 = ORIENTED_EDGE ( 'NONE', *, *, #97632, .T. ) ;
#62976 = EDGE_CURVE ( 'NONE', #36166, #85105, #38753, .T. ) ;
#62977 = EDGE_CURVE ( 'NONE', #119390, #63799, #94537, .T. ) ;
#62978 = CARTESIAN_POINT ( 'NONE',  ( 93.85002705046288440, -5.819803920172573086, -5.819803920172573086 ) ) ;
#62979 = CARTESIAN_POINT ( 'NONE',  ( 121.8500270504628702, -5.819803920172572198, -5.819803920172572198 ) ) ;
#62980 = CARTESIAN_POINT ( 'NONE',  ( 2.816011393730999401, 28.73617430169785436, 5.000000000000000000 ) ) ;
#62981 = CARTESIAN_POINT ( 'NONE',  ( 41.99451991528749062, 28.92564299267967343, 4.000000000000000000 ) ) ;
#62982 = EDGE_CURVE ( 'NONE', #81345, #138649, #7526, .T. ) ;
#62983 = CARTESIAN_POINT ( 'NONE',  ( 23.99451991528749062, 28.92564299267954908, 4.000000000000000000 ) ) ;
#62984 = FACE_OUTER_BOUND ( 'NONE', #78108, .T. ) ;
#62985 = CARTESIAN_POINT ( 'NONE',  ( 11.25346039003969523, 4.202752102959690472E-16, 0.000000000000000000 ) ) ;
#62986 = CARTESIAN_POINT ( 'NONE',  ( 1.166666666666666741, -5.278424836066145431, -3.047499999999993658 ) ) ;
#62987 = CARTESIAN_POINT ( 'NONE',  ( 6.541236474768552966, 0.000000000000000000, 7.934999999999990727 ) ) ;
#62988 = VECTOR ( 'NONE', #46021, 999.9999999999998863 ) ;
#62989 = DIRECTION ( 'NONE',  ( -0.6830127018922181881, 0.6830127018922202975, -0.2588190451025214056 ) ) ;
#62990 = DIRECTION ( 'NONE',  ( 0.7071067811865486830, -0.7071067811865464625, -0.000000000000000000 ) ) ;
#62991 = ORIENTED_EDGE ( 'NONE', *, *, #85735, .T. ) ;
#62992 = VERTEX_POINT ( 'NONE', #127923 ) ;
#62993 = AXIS2_PLACEMENT_3D ( 'NONE', #89635, #464, #44761 ) ;
#62994 = ADVANCED_FACE ( 'NONE', ( #8224 ), #82979, .F. ) ;
#62995 =( GEOMETRIC_REPRESENTATION_CONTEXT ( 3 ) GLOBAL_UNCERTAINTY_ASSIGNED_CONTEXT ( ( #31919 ) ) GLOBAL_UNIT_ASSIGNED_CONTEXT ( ( #61810, #17547, #48070 ) ) REPRESENTATION_CONTEXT ( 'NONE', 'WORKASPACE' ) );
#62996 = FACE_OUTER_BOUND ( 'NONE', #117086, .T. ) ;
#62997 = ORIENTED_EDGE ( 'NONE', *, *, #115028, .T. ) ;
#62999 = EDGE_CURVE ( 'NONE', #63322, #97308, #17683, .T. ) ;
#62998 = DIRECTION ( 'NONE',  ( -1.000000000000000000, 0.000000000000000000, 0.000000000000000000 ) ) ;
#63000 = CARTESIAN_POINT ( 'NONE',  ( -10.82816939922345867, -20.24070752338406720, 4.000000000000000000 ) ) ;
#63001 = DIRECTION ( 'NONE',  ( -0.6830127018922181881, 0.6830127018922202975, -0.2588190451025214056 ) ) ;
#63002 = VECTOR ( 'NONE', #34450, 1000.000000000000227 ) ;
#63003 = VECTOR ( 'NONE', #63412, 1000.000000000000000 ) ;
#63004 = CARTESIAN_POINT ( 'NONE',  ( -13.49999999999990052, 10.46639925780215918, 5.000000000000000000 ) ) ;
#63005 = EDGE_LOOP ( 'NONE', ( #74253, #113188, #23778, #3552 ) ) ;
#63006 = EDGE_CURVE ( 'NONE', #58831, #37040, #62657, .T. ) ;
#63007 = PLANE ( 'NONE',  #48769 ) ;
#63008 = DIRECTION ( 'NONE',  ( 0.7071067811865486830, -0.7071067811865464625, -0.000000000000000000 ) ) ;
#63009 = DIRECTION ( 'NONE',  ( -1.000000000000000000, -0.000000000000000000, -0.000000000000000000 ) ) ;
#63010 = DIRECTION ( 'NONE',  ( 0.000000000000000000, 0.000000000000000000, 1.000000000000000000 ) ) ;
#63012 = VERTEX_POINT ( 'NONE', #40215 ) ;
#63011 = CARTESIAN_POINT ( 'NONE',  ( -19.05000000000000071, 3.174999999999997158, 5.000000000000000000 ) ) ;
#63013 = EDGE_CURVE ( 'NONE', #139562, #115190, #140211, .T. ) ;
#63014 = CARTESIAN_POINT ( 'NONE',  ( -32.84387692260735747, -22.22499999999999787, 4.000000000000000000 ) ) ;
#63015 = LINE ( 'NONE', #115900, #84090 ) ;
#63016 = LINE ( 'NONE', #139134, #27091 ) ;
#63017 = DIRECTION ( 'NONE',  ( 0.7071067811865487940, 0.7071067811865463515, 0.000000000000000000 ) ) ;
#63018 = CARTESIAN_POINT ( 'NONE',  ( 56.65265948608892188, -50.37061236291013699, 37.32649486623391510 ) ) ;
#63019 = ORIENTED_EDGE ( 'NONE', *, *, #125135, .T. ) ;
#63020 = VERTEX_POINT ( 'NONE', #95973 ) ;
#63021 = CARTESIAN_POINT ( 'NONE',  ( 97.56293019189810423, 1.637169565754157174, 6.110000000000002984 ) ) ;
#63022 = VERTEX_POINT ( 'NONE', #19137 ) ;
#63023 = EDGE_CURVE ( 'NONE', #38372, #68590, #62377, .T. ) ;
#63024 = LINE ( 'NONE', #44866, #34090 ) ;
#63025 = CARTESIAN_POINT ( 'NONE',  ( 27.83652871126532347, 15.75929247661555976, 9.299976744542982843 ) ) ;
#63026 = VERTEX_POINT ( 'NONE', #76393 ) ;
#63027 = CARTESIAN_POINT ( 'NONE',  ( -33.32816939922329880, -9.740707523384182664, 4.000000000000000000 ) ) ;
#63028 = CARTESIAN_POINT ( 'NONE',  ( 57.48921356237308800, -27.52281430457095368, 5.000000000000000000 ) ) ;
#63029 = VECTOR ( 'NONE', #12916, 1000.000000000000227 ) ;
#63030 = EDGE_CURVE ( 'NONE', #89838, #29922, #32159, .T. ) ;
#63031 = AXIS2_PLACEMENT_3D ( 'NONE', #8761, #97216, #109554 ) ;
#63032 = CARTESIAN_POINT ( 'NONE',  ( 96.45376352523145158, -6.109999999999998543, -3.741295971395162543E-16 ) ) ;
#63033 = ORIENTED_EDGE ( 'NONE', *, *, #69893, .T. ) ;
#63034 = ADVANCED_FACE ( 'NONE', ( #54638 ), #143058, .T. ) ;
#63035 = AXIS2_PLACEMENT_3D ( 'NONE', #15250, #71836, #59532 ) ;
#63036 = CARTESIAN_POINT ( 'NONE',  ( 78.29974487139158157, -27.71228299555260577, 4.000000000000000000 ) ) ;
#63037 = VERTEX_POINT ( 'NONE', #56093 ) ;
#63038 = DIRECTION ( 'NONE',  ( 0.000000000000000000, 0.000000000000000000, -1.000000000000000000 ) ) ;
#63039 = DIRECTION ( 'NONE',  ( -0.7071067811865486830, 0.7071067811865464625, 0.000000000000000000 ) ) ;
#63040 = VECTOR ( 'NONE', #14987, 1000.000000000000000 ) ;
#63041 = LINE ( 'NONE', #7156, #20744 ) ;
#63042 = ADVANCED_FACE ( 'NONE', ( #21287 ), #132210, .T. ) ;
#63043 = ORIENTED_EDGE ( 'NONE', *, *, #15646, .T. ) ;
#63044 = ORIENTED_EDGE ( 'NONE', *, *, #113862, .F. ) ;
#63045 = ORIENTED_EDGE ( 'NONE', *, *, #36689, .F. ) ;
#63046 = LINE ( 'NONE', #13598, #54107 ) ;
#63047 = CARTESIAN_POINT ( 'NONE',  ( 34.92499999999998295, 19.51246187583928204, 4.000000000000000000 ) ) ;
#63048 = CARTESIAN_POINT ( 'NONE',  ( 13.48373647476855375, -5.808823158059035485, -5.808823158059033709 ) ) ;
#63049 = VECTOR ( 'NONE', #40089, 1000.000000000000000 ) ;
#63050 = FACE_OUTER_BOUND ( 'NONE', #107931, .T. ) ;
#63051 =( NAMED_UNIT ( * ) PLANE_ANGLE_UNIT ( ) SI_UNIT ( $, .RADIAN. ) );
#63052 = ORIENTED_EDGE ( 'NONE', *, *, #58710, .T. ) ;
#63053 = EDGE_LOOP ( 'NONE', ( #114580, #84250, #71664, #60262 ) ) ;
#63054 = EDGE_CURVE ( 'NONE', #99130, #21326, #77126, .T. ) ;
#63055 = DIRECTION ( 'NONE',  ( -0.7071067811865486830, -0.7071067811865464625, -0.000000000000000000 ) ) ;
#63056 = ORIENTED_EDGE ( 'NONE', *, *, #71990, .F. ) ;
#63057 = ORIENTED_EDGE ( 'NONE', *, *, #71358, .T. ) ;
#63058 = VECTOR ( 'NONE', #24321, 1000.000000000000227 ) ;
#63059 = AXIS2_PLACEMENT_3D ( 'NONE', #124639, #81156, #113764 ) ;
#63060 = EDGE_CURVE ( 'NONE', #122495, #93029, #3183, .T. ) ;
#63061 = DIRECTION ( 'NONE',  ( 1.000000000000000000, -1.248002500702738701E-15, 0.000000000000000000 ) ) ;
#63062 = EDGE_LOOP ( 'NONE', ( #88054, #87344, #51566, #138421 ) ) ;
#63063 = DIRECTION ( 'NONE',  ( -0.3543493200069163795, -9.265275131829747941E-33, -0.9351131265310288487 ) ) ;
#63064 = CARTESIAN_POINT ( 'NONE',  ( 4.828169399223495084, 3.759292476615671230, 4.000000000000000000 ) ) ;
#63065 = DIRECTION ( 'NONE',  ( -0.3543493200069162685, -0.000000000000000000, -0.9351131265310288487 ) ) ;
#63066 = AXIS2_PLACEMENT_3D ( 'NONE', #100732, #133374, #109460 ) ;
#63067 = LINE ( 'NONE', #140577, #113150 ) ;
#63068 = SURFACE_STYLE_USAGE ( .BOTH. , #7185 ) ;
#63069 = ORIENTED_EDGE ( 'NONE', *, *, #108275, .F. ) ;
#63070 = CARTESIAN_POINT ( 'NONE',  ( -15.18398860626900237, 28.73617430169797871, 5.000000000000000000 ) ) ;
#63071 = FACE_BOUND ( 'NONE', #84559, .T. ) ;
#63072 = ORIENTED_EDGE ( 'NONE', *, *, #42409, .T. ) ;
#63073 = DIRECTION ( 'NONE',  ( 0.7071067811865487940, 0.7071067811865463515, 0.000000000000000000 ) ) ;
#63074 = CARTESIAN_POINT ( 'NONE',  ( 36.18398860626899705, 28.73617430169812437, 5.000000000000000000 ) ) ;
#63075 = DIRECTION ( 'NONE',  ( -0.7071067811865486830, -0.7071067811865464625, -0.000000000000000000 ) ) ;
#63076 = ORIENTED_EDGE ( 'NONE', *, *, #114054, .F. ) ;
#63077 = CARTESIAN_POINT ( 'NONE',  ( 23.63159235450331863, 2.500000000000001776, 0.000000000000000000 ) ) ;
#63078 = ORIENTED_EDGE ( 'NONE', *, *, #37604, .T. ) ;
#63079 = ORIENTED_EDGE ( 'NONE', *, *, #71745, .F. ) ;
#63080 = AXIS2_PLACEMENT_3D ( 'NONE', #27658, #28398, #61752 ) ;
#63081 = VERTEX_POINT ( 'NONE', #9675 ) ;
#63082 = ADVANCED_FACE ( 'NONE', ( #110405 ), #141648, .T. ) ;
#63083 = FACE_OUTER_BOUND ( 'NONE', #100163, .T. ) ;
#63084 = CARTESIAN_POINT ( 'NONE',  ( 22.49999999999984368, 14.14708470758593251, -0.5283514160167069873 ) ) ;
#63085 = CARTESIAN_POINT ( 'NONE',  ( -21.18398860626899349, 28.73617430169802134, 5.000000000000000000 ) ) ;
#63086 = LINE ( 'NONE', #107259, #84401 ) ;
#63087 = DIRECTION ( 'NONE',  ( -0.7071067811865486830, -0.7071067811865464625, -0.000000000000000000 ) ) ;
#63088 = LINE ( 'NONE', #107262, #73690 ) ;
#63089 = CONICAL_SURFACE ( 'NONE', #120893, 2.055000000000001048, 0.9599310885968758145 ) ;
#63090 = VECTOR ( 'NONE', #23506, 1000.000000000000227 ) ;
#63091 = CONICAL_SURFACE ( 'NONE', #65374, 2.500000000000000888, 0.9599310885968822538 ) ;
#63092 = CARTESIAN_POINT ( 'NONE',  ( -34.49999999999975842, 14.14708470758588099, -0.5283514160165768692 ) ) ;
#63093 = VECTOR ( 'NONE', #75755, 1000.000000000000000 ) ;
#63094 = VECTOR ( 'NONE', #26837, 1000.000000000000000 ) ;
#63095 = FACE_OUTER_BOUND ( 'NONE', #100966, .T. ) ;
#63096 = CARTESIAN_POINT ( 'NONE',  ( -1.734723475976807094E-15, 19.93112307739198386, 4.000000000000000000 ) ) ;
#63097 = DIRECTION ( 'NONE',  ( 0.7071067811865486830, -0.7071067811865464625, -0.000000000000000000 ) ) ;
#63098 = VERTEX_POINT ( 'NONE', #75674 ) ;
#63099 = EDGE_LOOP ( 'NONE', ( #96415, #71214, #82523, #26275 ) ) ;
#63100 = AXIS2_PLACEMENT_3D ( 'NONE', #124143, #1612, #100953 ) ;
#63101 = ORIENTED_EDGE ( 'NONE', *, *, #46556, .F. ) ;
#63102 = CIRCLE ( 'NONE', #56188, 2.500000000000000444 ) ;
#63103 = ORIENTED_EDGE ( 'NONE', *, *, #56423, .F. ) ;
#63104 = COLOUR_RGB ( '', 0.08235294, 0.09019608, 0.10196078) ;
#63105 = CARTESIAN_POINT ( 'NONE',  ( 11.15159235450332176, 9.902892378096218942E-16, 0.000000000000000000 ) ) ;
#63106 = EDGE_LOOP ( 'NONE', ( #49300, #64700, #74529, #115635 ) ) ;
#63107 = EDGE_LOOP ( 'NONE', ( #127532, #111341, #56392, #118889 ) ) ;
#63108 = PLANE ( 'NONE',  #472 ) ;
#63109 =( NAMED_UNIT ( * ) PLANE_ANGLE_UNIT ( ) SI_UNIT ( $, .RADIAN. ) );
#63110 = DIRECTION ( 'NONE',  ( 0.000000000000000000, -0.000000000000000000, -1.000000000000000000 ) ) ;
#63111 = ORIENTED_EDGE ( 'NONE', *, *, #81166, .F. ) ;
#63112 = CARTESIAN_POINT ( 'NONE',  ( 14.99999999999988809, -10.77435723561694125, -9.972017380717266732 ) ) ;
#63113 = ORIENTED_EDGE ( 'NONE', *, *, #78695, .F. ) ;
#63114 = DIRECTION ( 'NONE',  ( -1.000000000000000000, -0.000000000000000000, 0.000000000000000000 ) ) ;
#63115 = DIRECTION ( 'NONE',  ( -1.000000000000000000, -1.224606353822377258E-16, -0.000000000000000000 ) ) ;
#63116 = CARTESIAN_POINT ( 'NONE',  ( 11.00456980810188590, 6.871911579029510442, -3.967499999999998916 ) ) ;
#63117 = ORIENTED_EDGE ( 'NONE', *, *, #78037, .T. ) ;
#63118 = CARTESIAN_POINT ( 'NONE',  ( 91.49543019189812298, 5.291415217122917625, 3.055000000000002380 ) ) ;
#63119 = SURFACE_STYLE_USAGE ( .BOTH. , #18110 ) ;
#63120 = LINE ( 'NONE', #61688, #88348 ) ;
#63121 = LINE ( 'NONE', #97863, #67440 ) ;
#63122 = VERTEX_POINT ( 'NONE', #130788 ) ;
#63123 = ORIENTED_EDGE ( 'NONE', *, *, #127022, .F. ) ;
#63124 = CARTESIAN_POINT ( 'NONE',  ( 22.07159235450331991, 9.902892378096218942E-16, 0.000000000000000000 ) ) ;
#63125 = VERTEX_POINT ( 'NONE', #130053 ) ;
#63126 = LINE ( 'NONE', #68144, #111063 ) ;
#63127 = CARTESIAN_POINT ( 'NONE',  ( 21.08314806772918004, 21.75929247661549581, 7.311836541448100135 ) ) ;
#63128 = CARTESIAN_POINT ( 'NONE',  ( -18.47512612785034491, 14.25929247661557575, 9.797011795316594274 ) ) ;
#63129 = DIRECTION ( 'NONE',  ( -0.3543493200069162685, -0.000000000000000000, -0.9351131265310288487 ) ) ;
#63130 = VERTEX_POINT ( 'NONE', #44501 ) ;
#63131 =( GEOMETRIC_REPRESENTATION_CONTEXT ( 3 ) GLOBAL_UNCERTAINTY_ASSIGNED_CONTEXT ( ( #103937 ) ) GLOBAL_UNIT_ASSIGNED_CONTEXT ( ( #48620, #47250, #26158 ) ) REPRESENTATION_CONTEXT ( 'NONE', 'WORKASPACE' ) );
#63132 = FACE_OUTER_BOUND ( 'NONE', #69333, .T. ) ;
#63133 = VECTOR ( 'NONE', #28137, 1000.000000000000227 ) ;
#63134 = DIRECTION ( 'NONE',  ( -1.000000000000000000, 0.000000000000000000, -1.224646799147353207E-16 ) ) ;
#63135 = DIRECTION ( 'NONE',  ( 0.6830127018922181881, 0.6830127018922202975, -0.2588190451025214056 ) ) ;
#63136 = EDGE_CURVE ( 'NONE', #38538, #66120, #42347, .T. ) ;
#63137 = ORIENTED_EDGE ( 'NONE', *, *, #604, .T. ) ;
#63138 = DIRECTION ( 'NONE',  ( -0.7071067811865486830, -0.7071067811865464625, 0.000000000000000000 ) ) ;
#63139 = AXIS2_PLACEMENT_3D ( 'NONE', #93829, #49651, #106833 ) ;
#63140 = VECTOR ( 'NONE', #100080, 999.9999999999998863 ) ;
#63141 = CARTESIAN_POINT ( 'NONE',  ( 31.17183060077626067, 21.75929247661550647, 4.000000000000000000 ) ) ;
#63142 = ORIENTED_EDGE ( 'NONE', *, *, #10112, .T. ) ;
#63144 = EDGE_LOOP ( 'NONE', ( #25261, #43092, #54029, #84819 ) ) ;
#63143 = CARTESIAN_POINT ( 'NONE',  ( -30.18398860626900060, 28.73617430169808173, 5.000000000000000000 ) ) ;
#63145 = ORIENTED_EDGE ( 'NONE', *, *, #40458, .F. ) ;
#63146 = EDGE_CURVE ( 'NONE', #142010, #76898, #20542, .T. ) ;
#63147 = EDGE_CURVE ( 'NONE', #89949, #70280, #19838, .T. ) ;
#63148 = FACE_OUTER_BOUND ( 'NONE', #76064, .T. ) ;
#63149 = DIRECTION ( 'NONE',  ( -0.7071067811865486830, -0.7071067811865464625, 0.000000000000000000 ) ) ;
#63150 = ORIENTED_EDGE ( 'NONE', *, *, #62528, .F. ) ;
#63151 = DIRECTION ( 'NONE',  ( -0.3543493200069162685, -0.000000000000000000, -0.9351131265310288487 ) ) ;
#63152 = EDGE_CURVE ( 'NONE', #112531, #113476, #64801, .T. ) ;
#63153 = EDGE_CURVE ( 'NONE', #86059, #123098, #61614, .T. ) ;
#63154 = CARTESIAN_POINT ( 'NONE',  ( 12.71159235450332048, 9.902892378096218942E-16, 0.000000000000000000 ) ) ;
#63155 = EDGE_CURVE ( 'NONE', #14007, #139229, #78526, .T. ) ;
#63156 = PLANE ( 'NONE',  #80933 ) ;
#63157 = LINE ( 'NONE', #8683, #113715 ) ;
#63158 = EDGE_CURVE ( 'NONE', #104460, #64781, #94814, .T. ) ;
#63159 = CARTESIAN_POINT ( 'NONE',  ( -3.299744871391591339, -27.71228299555208352, 4.000000000000000000 ) ) ;
#63160 = AXIS2_PLACEMENT_3D ( 'NONE', #1801, #47554, #113450 ) ;
#63161 = DIRECTION ( 'NONE',  ( 0.3543493200069162685, -0.000000000000000000, -0.9351131265310288487 ) ) ;
#63162 = CARTESIAN_POINT ( 'NONE',  ( -17.81601139373099940, 28.73617430169775133, 5.000000000000000000 ) ) ;
#63163 = CARTESIAN_POINT ( 'NONE',  ( 8.287690060339658160, -21.73547319004781642, 4.999917730833664642 ) ) ;
#63164 = PLANE ( 'NONE',  #134693 ) ;
#63165 = VECTOR ( 'NONE', #30148, 1000.000000000000000 ) ;
#63166 = DIRECTION ( 'NONE',  ( -0.7071067811865487940, 0.7071067811865463515, -0.000000000000000000 ) ) ;
#63167 = ADVANCED_FACE ( 'NONE', ( #91547 ), #13235, .F. ) ;
#63168 = CARTESIAN_POINT ( 'NONE',  ( -6.792893218813404133, -2.240707523384255939, 5.000000000000000000 ) ) ;
#63169 = CARTESIAN_POINT ( 'NONE',  ( -12.18398860626900060, 28.73617430169795739, 5.000000000000000000 ) ) ;
#63170 = VERTEX_POINT ( 'NONE', #28246 ) ;
#63171 =( BOUNDED_CURVE ( )  B_SPLINE_CURVE ( 2, ( #134526, #46841, #78001, #67867, #46097, #113447, #14137, #133799, #58429, #35938, #135249, #35223, #102608 ),
 .UNSPECIFIED., .F., .F. ) 
 B_SPLINE_CURVE_WITH_KNOTS ( ( 3, 2, 2, 2, 2, 2, 3 ),
 ( 0.6833333333333334592, 0.6861111111111112271, 0.6888888888888889950, 0.6916666666666667629, 0.6944444444444445308, 0.6972222222222222987, 0.7000000000000000666 ),
 .UNSPECIFIED. ) 
 CURVE ( )  GEOMETRIC_REPRESENTATION_ITEM ( )  RATIONAL_B_SPLINE_CURVE ( ( 0.9999999999999986677, 0.9659258262890696445, 1.000000000000000000, 0.9659258262890683122, 1.000000000000000000, 0.9659258262890683122, 1.000000000000000000, 0.9659258262890683122, 1.000000000000000000, 0.9659258262890683122, 1.000000000000000000, 0.9659258262890669799, 1.000000000000001332 ) ) 
 REPRESENTATION_ITEM ( '' )  );
#63172 = VERTEX_POINT ( 'NONE', #45218 ) ;
#63173 = EDGE_LOOP ( 'NONE', ( #115435, #8968, #8755, #16734 ) ) ;
#63175 = EDGE_CURVE ( 'NONE', #30612, #84615, #133625, .T. ) ;
#63174 = CARTESIAN_POINT ( 'NONE',  ( 111.9791666666666714, -7.950000000000001066, 2.130196079827424427 ) ) ;
#63176 = VERTEX_POINT ( 'NONE', #57505 ) ;
#63177 = ORIENTED_EDGE ( 'NONE', *, *, #95956, .T. ) ;
#63178 = ORIENTED_EDGE ( 'NONE', *, *, #94224, .F. ) ;
#63179 = CARTESIAN_POINT ( 'NONE',  ( -16.49999999999988276, -5.947814304570758104, 5.000000000000000000 ) ) ;
#63180 = CARTESIAN_POINT ( 'NONE',  ( 11.29289321881338282, -15.74070752338412049, 5.000000000000000000 ) ) ;
#63181 = AXIS2_PLACEMENT_3D ( 'NONE', #70883, #41080, #82458 ) ;
#63182 = VERTEX_POINT ( 'NONE', #67684 ) ;
#63183 =( BOUNDED_CURVE ( )  B_SPLINE_CURVE ( 2, ( #8870, #108936, #53137, #31414, #9625, #21240, #33580, #100936, #45179, #56777, #123450, #98782, #124125 ),
 .UNSPECIFIED., .F., .T. ) 
 B_SPLINE_CURVE_WITH_KNOTS ( ( 3, 2, 2, 2, 2, 2, 3 ),
 ( 0.4500000000000001221, 0.4527777777777778900, 0.4555555555555556024, 0.4583333333333333703, 0.4611111111111111938, 0.4638888888888889062, 0.4666666666666666741 ),
 .UNSPECIFIED. ) 
 CURVE ( )  GEOMETRIC_REPRESENTATION_ITEM ( )  RATIONAL_B_SPLINE_CURVE ( ( 0.9999999999999986677, 0.9659258262890696445, 1.000000000000000000, 0.9659258262890683122, 1.000000000000000000, 0.9659258262890683122, 1.000000000000000000, 0.9659258262890683122, 1.000000000000000000, 0.9659258262890683122, 1.000000000000000000, 0.9659258262890683122, 1.000000000000000000 ) ) 
 REPRESENTATION_ITEM ( '' )  );
#63184 = PLANE ( 'NONE',  #83307 ) ;
#63185 = EDGE_CURVE ( 'NONE', #49545, #63026, #135080, .T. ) ;
#63186 = DIRECTION ( 'NONE',  ( 0.6830127018922180770, -0.6830127018922204085, -0.2588190451025213501 ) ) ;
#63187 = DIRECTION ( 'NONE',  ( 0.6830127018922180770, -0.6830127018922204085, -0.2588190451025213501 ) ) ;
#63188 = PLANE ( 'NONE',  #9515 ) ;
#63189 = CARTESIAN_POINT ( 'NONE',  ( 101.3545968585647614, -1.637169565754161615, 6.110000000000000320 ) ) ;
#63190 = ORIENTED_EDGE ( 'NONE', *, *, #31901, .T. ) ;
#63191 = CARTESIAN_POINT ( 'NONE',  ( 0.4414447833044549130, 12.59086548424452090, -26.73346183226842498 ) ) ;
#63192 = CARTESIAN_POINT ( 'NONE',  ( -16.49999999999988276, -9.462702396501025959, -9.474982329943475889 ) ) ;
#63194 = VECTOR ( 'NONE', #130396, 1000.000000000000000 ) ;
#63193 = CARTESIAN_POINT ( 'NONE',  ( -23.95341186370441378, 14.25929247661557042, 18.84478104361333450 ) ) ;
#63195 = EDGE_CURVE ( 'NONE', #93386, #51714, #35772, .T. ) ;
#63196 = DIRECTION ( 'NONE',  ( 1.000000000000000000, 3.115803279706882722E-16, -0.000000000000000000 ) ) ;
#63197 = DIRECTION ( 'NONE',  ( -0.6830127018922181881, 0.6830127018922202975, -0.2588190451025214056 ) ) ;
#63198 = CARTESIAN_POINT ( 'NONE',  ( 20.99451991528748707, 28.92564299267952777, 4.000000000000000000 ) ) ;
#63199 = CARTESIAN_POINT ( 'NONE',  ( 29.82919371712955581, -3.975000000000001865, 6.884901960086284411 ) ) ;
#63200 = CARTESIAN_POINT ( 'NONE',  ( 42.18398860626899705, 28.73617430169816700, 5.000000000000000000 ) ) ;
#63201 = ORIENTED_EDGE ( 'NONE', *, *, #104302, .F. ) ;
#63202 = ORIENTED_EDGE ( 'NONE', *, *, #72131, .F. ) ;
#63203 = CARTESIAN_POINT ( 'NONE',  ( 28.70833333333332149, -3.974999999999999201, -6.884901960086287964 ) ) ;
#63204 = ORIENTED_EDGE ( 'NONE', *, *, #9594, .T. ) ;
#63205 = CARTESIAN_POINT ( 'NONE',  ( 11.25346039003969523, 2.055000000000001048, 0.000000000000000000 ) ) ;
#63206 = DIRECTION ( 'NONE',  ( -0.7071067811865486830, 0.7071067811865464625, 0.000000000000000000 ) ) ;
#63207 = VECTOR ( 'NONE', #37065, 1000.000000000000227 ) ;
#63208 = DIRECTION ( 'NONE',  ( 0.000000000000000000, -1.000000000000000000, 0.000000000000000000 ) ) ;
#63209 = LINE ( 'NONE', #8730, #39921 ) ;
#63210 = AXIS2_PLACEMENT_3D ( 'NONE', #86465, #83623, #74890 ) ;
#63211 = LINE ( 'NONE', #41409, #104521 ) ;
#63213 = CONICAL_SURFACE ( 'NONE', #33103, 2.055000000000001048, 0.9599310885968758145 ) ;
#63212 = CARTESIAN_POINT ( 'NONE',  ( -20.99999999999984368, -6.412538124160692909, 4.000000000000000000 ) ) ;
#63214 = ADVANCED_FACE ( 'NONE', ( #79990 ), #124879, .F. ) ;
#63215 = CARTESIAN_POINT ( 'NONE',  ( 126.3495968585647944, 6.109999999999996767, 1.637169565754163836 ) ) ;
#63216 = ORIENTED_EDGE ( 'NONE', *, *, #77063, .F. ) ;
#63217 = EDGE_CURVE ( 'NONE', #65963, #142366, #39121, .T. ) ;
#63218 = DIRECTION ( 'NONE',  ( 0.6830127018922180770, -0.6830127018922204085, -0.2588190451025213501 ) ) ;
#63219 = EDGE_LOOP ( 'NONE', ( #111378, #14610, #65148, #8027 ) ) ;
#63220 = AXIS2_PLACEMENT_3D ( 'NONE', #93400, #139791, #7791 ) ;
#63221 = VECTOR ( 'NONE', #129473, 1000.000000000000227 ) ;
#63222 = CARTESIAN_POINT ( 'NONE',  ( 17.54840764549667398, 3.061616997868385113E-16, -2.500000000000001332 ) ) ;
#63223 = LINE ( 'NONE', #64608, #52435 ) ;
#63225 = EDGE_CURVE ( 'NONE', #88378, #19029, #60917, .T. ) ;
#63224 = CARTESIAN_POINT ( 'NONE',  ( -33.51665438641022376, 22.22500000000000142, 4.500000000000000888 ) ) ;
#63226 = EDGE_CURVE ( 'NONE', #106843, #83227, #72507, .T. ) ;
#63227 = DIRECTION ( 'NONE',  ( 0.6830127018922180770, -0.6830127018922204085, -0.2588190451025213501 ) ) ;
#63228 = EDGE_LOOP ( 'NONE', ( #39962, #53089, #66025, #69473, #12479 ) ) ;
#63229 = CARTESIAN_POINT ( 'NONE',  ( 48.85459685856476142, -1.637169565754161615, 6.110000000000000320 ) ) ;
#63230 = ORIENTED_EDGE ( 'NONE', *, *, #92485, .T. ) ;
#63231 = CARTESIAN_POINT ( 'NONE',  ( -45.29974487139158867, -27.71228299555237840, 4.000000000000000000 ) ) ;
#63232 = LINE ( 'NONE', #63914, #20776 ) ;
#63233 = CARTESIAN_POINT ( 'NONE',  ( 1.499999999999990896, -2.947814304570802513, 5.000000000000000000 ) ) ;
#63234 = DIRECTION ( 'NONE',  ( 0.000000000000000000, 0.000000000000000000, 1.000000000000000000 ) ) ;
#63235 = VECTOR ( 'NONE', #73637, 1000.000000000000000 ) ;
#63236 = CARTESIAN_POINT ( 'NONE',  ( 37.82876352523144448, 0.000000000000000000, -6.109999999999998543 ) ) ;
#63237 = EDGE_LOOP ( 'NONE', ( #21640, #30018, #73786, #15154, #29723 ) ) ;
#63238 = EDGE_CURVE ( 'NONE', #33598, #103136, #105078, .T. ) ;
#63239 = CARTESIAN_POINT ( 'NONE',  ( -7.499999999999949374, 16.77039438581778796, 0.4657186855307913764 ) ) ;
#63240 = VERTEX_POINT ( 'NONE', #116668 ) ;
#63241 = ORIENTED_EDGE ( 'NONE', *, *, #52322, .T. ) ;
#63242 = EDGE_LOOP ( 'NONE', ( #23251, #52727, #86871, #45378 ) ) ;
#63243 = AXIS2_PLACEMENT_3D ( 'NONE', #46345, #47086, #15082 ) ;
#63244 = CARTESIAN_POINT ( 'NONE',  ( 0.000000000000000000, 0.000000000000000000, 5.000000000000000000 ) ) ;
#63245 = PRODUCT_DEFINITION_SHAPE ( 'NONE', 'NONE',  #143561 ) ;
#63246 = CARTESIAN_POINT ( 'NONE',  ( 79.99586038379621300, -3.974999999999998312, -6.884901960086286188 ) ) ;
#63247 = PRODUCT_DEFINITION_CONTEXT ( 'detailed design', #92057, 'design' ) ;
#63248 = EDGE_CURVE ( 'NONE', #87783, #100682, #102440, .T. ) ;
#63249 = VERTEX_POINT ( 'NONE', #68394 ) ;
#63250 = VECTOR ( 'NONE', #65638, 1000.000000000000000 ) ;
#63251 = CARTESIAN_POINT ( 'NONE',  ( 17.92867102513379862, 9.037728232668255757, 5.000000000000000000 ) ) ;
#63252 = DIRECTION ( 'NONE',  ( -0.000000000000000000, 0.000000000000000000, 1.000000000000000000 ) ) ;
#63253 = CARTESIAN_POINT ( 'NONE',  ( 13.20450575203696886, 4.382956123802139281, 4.000000000000000000 ) ) ;
#63254 = EDGE_CURVE ( 'NONE', #35625, #30995, #43948, .T. ) ;
#63255 = FACE_BOUND ( 'NONE', #19311, .T. ) ;
#63256 = ORIENTED_EDGE ( 'NONE', *, *, #15469, .F. ) ;
#63257 = FILL_AREA_STYLE ('',( #20393 ) ) ;
#63258 = CARTESIAN_POINT ( 'NONE',  ( 3.487905803711476072, -49.11927476322658492, 40.22110306067541075 ) ) ;
#63259 = VERTEX_POINT ( 'NONE', #5740 ) ;
#63260 = DIRECTION ( 'NONE',  ( 0.7071067811865487940, 0.7071067811865463515, 0.000000000000000000 ) ) ;
#63261 = ORIENTED_EDGE ( 'NONE', *, *, #38299, .T. ) ;
#63262 = ORIENTED_EDGE ( 'NONE', *, *, #59661, .T. ) ;
#63263 = FACE_OUTER_BOUND ( 'NONE', #40270, .T. ) ;
#63264 = VERTEX_POINT ( 'NONE', #94190 ) ;
#63265 = AXIS2_PLACEMENT_3D ( 'NONE', #91316, #74378, #91992 ) ;
#63266 = CARTESIAN_POINT ( 'NONE',  ( 55.32876352523144448, 0.000000000000000000, -6.109999999999998543 ) ) ;
#63267 = ORIENTED_EDGE ( 'NONE', *, *, #86450, .T. ) ;
#63268 = CARTESIAN_POINT ( 'NONE',  ( 21.29974487139158512, -27.71228299555221142, 4.000000000000000000 ) ) ;
#63269 = LINE ( 'NONE', #40776, #75096 ) ;
#63270 = AXIS2_PLACEMENT_3D ( 'NONE', #57516, #943, #103135 ) ;
#63271 = ORIENTED_EDGE ( 'NONE', *, *, #135363, .F. ) ;
#63272 = CARTESIAN_POINT ( 'NONE',  ( 60.18398860626900415, 28.73617430169829490, 5.000000000000000000 ) ) ;
#63273 = AXIS2_PLACEMENT_3D ( 'NONE', #52441, #96629, #40190 ) ;
#63274 = EDGE_CURVE ( 'NONE', #1311, #94958, #62491, .T. ) ;
#63275 = EDGE_CURVE ( 'NONE', #141681, #1315, #23409, .T. ) ;
#63276 = CARTESIAN_POINT ( 'NONE',  ( 33.48921356237309510, -27.52281430457078670, 5.000000000000000000 ) ) ;
#63277 = SURFACE_STYLE_FILL_AREA ( #32031 ) ;
#63278 = CARTESIAN_POINT ( 'NONE',  ( -5.292893218813412126, 11.25929247661560240, 5.000000000000000000 ) ) ;
#63279 = DIRECTION ( 'NONE',  ( -0.7071067811865487940, 0.7071067811865463515, 0.000000000000000000 ) ) ;
#63280 = FACE_OUTER_BOUND ( 'NONE', #143346, .T. ) ;
#63281 = EDGE_LOOP ( 'NONE', ( #15902, #6204, #11036, #54792 ) ) ;
#63282 = VECTOR ( 'NONE', #91780, 1000.000000000000000 ) ;
#63283 = VERTEX_POINT ( 'NONE', #134342 ) ;
#63284 = CARTESIAN_POINT ( 'NONE',  ( 12.51280225271498736, 0.000000000000000000, 2.500000000000000444 ) ) ;
#63285 = LINE ( 'NONE', #8115, #130025 ) ;
#63286 = ORIENTED_EDGE ( 'NONE', *, *, #58465, .T. ) ;
#63287 = ORIENTED_EDGE ( 'NONE', *, *, #93603, .T. ) ;
#63288 = ORIENTED_EDGE ( 'NONE', *, *, #138786, .F. ) ;
#63289 = CARTESIAN_POINT ( 'NONE',  ( 33.48921356237309510, -27.52281430457078670, 5.000000000000000000 ) ) ;
#63290 = CARTESIAN_POINT ( 'NONE',  ( 55.78752705046288440, 0.000000000000000000, -7.949999999999998401 ) ) ;
#63291 = ADVANCED_FACE ( 'NONE', ( #28955 ), #107900, .F. ) ;
#63292 = DIRECTION ( 'NONE',  ( -0.7071067811865486830, -0.7071067811865464625, 0.000000000000000000 ) ) ;
#63293 = VECTOR ( 'NONE', #99893, 1000.000000000000000 ) ;
#63294 = VERTEX_POINT ( 'NONE', #130422 ) ;
#63295 = CARTESIAN_POINT ( 'NONE',  ( 39.29974487139159578, -27.71228299555233576, 4.000000000000000000 ) ) ;
#63296 = CARTESIAN_POINT ( 'NONE',  ( -34.92500000000001137, -22.22500000000000142, 4.000000000000000000 ) ) ;
#63297 = CARTESIAN_POINT ( 'NONE',  ( 22.52540314143522338, 2.126176841940962348, 7.934999999999989839 ) ) ;
#63298 = CARTESIAN_POINT ( 'NONE',  ( -5.816011393731002066, 28.73617430169783304, 5.000000000000000000 ) ) ;
#63299 = VERTEX_POINT ( 'NONE', #118805 ) ;
#63300 = CARTESIAN_POINT ( 'NONE',  ( 117.1620968585647802, -5.291415217122919401, 3.054999999999998384 ) ) ;
#63301 = DIRECTION ( 'NONE',  ( 0.7071067811865487940, 0.7071067811865463515, 0.000000000000000000 ) ) ;
#63302 = CARTESIAN_POINT ( 'NONE',  ( 14.29289321881336150, -0.7407075233842770334, 5.000000000000000000 ) ) ;
#63303 = AXIS2_PLACEMENT_3D ( 'NONE', #1384, #45671, #13688 ) ;
#63305 = ORIENTED_EDGE ( 'NONE', *, *, #45748, .T. ) ;
#63304 = LINE ( 'NONE', #119059, #40254 ) ;
#63306 = CARTESIAN_POINT ( 'NONE',  ( -11.99451991528749417, 28.92564299267946382, 4.000000000000000000 ) ) ;
#63307 = ORIENTED_EDGE ( 'NONE', *, *, #70036, .F. ) ;
#63308 = FACE_OUTER_BOUND ( 'NONE', #84481, .T. ) ;
#63309 = CARTESIAN_POINT ( 'NONE',  ( -10.49999999999992539, -14.56887692260766087, 4.000000000000000000 ) ) ;
#63310 = DIRECTION ( 'NONE',  ( -0.7071067811865487940, 0.7071067811865463515, 0.000000000000000000 ) ) ;
#63312 = ORIENTED_EDGE ( 'NONE', *, *, #112598, .T. ) ;
#63311 = AXIS2_PLACEMENT_3D ( 'NONE', #77696, #68278, #58112 ) ;
#63313 = DIRECTION ( 'NONE',  ( 0.6830127018922181881, 0.6830127018922202975, -0.2588190451025214056 ) ) ;
#63314 = CARTESIAN_POINT ( 'NONE',  ( 44.99451991528749772, 28.92564299267969474, 4.000000000000000000 ) ) ;
#63315 = CARTESIAN_POINT ( 'NONE',  ( -34.45011844616454511, 21.00230414159373638, 5.000000000000000888 ) ) ;
#63316 = VECTOR ( 'NONE', #131297, 999.9999999999998863 ) ;
#63317 = VERTEX_POINT ( 'NONE', #63743 ) ;
#63318 = DIRECTION ( 'NONE',  ( -0.000000000000000000, 0.3543493200069153248, 0.9351131265310292928 ) ) ;
#63319 = DIRECTION ( 'NONE',  ( -0.6830127018922180770, -0.6830127018922204085, -0.2588190451025213501 ) ) ;
#63320 = CARTESIAN_POINT ( 'NONE',  ( 4.520833333333333037, -6.094999999999989981, -1.633150327867689322 ) ) ;
#63321 = CARTESIAN_POINT ( 'NONE',  ( 47.99451991528749062, 28.92564299267971251, 4.000000000000000000 ) ) ;
#63322 = VERTEX_POINT ( 'NONE', #6423 ) ;
#63323 = EDGE_CURVE ( 'NONE', #84062, #95284, #60097, .T. ) ;
#63324 = VERTEX_POINT ( 'NONE', #128972 ) ;
#63325 = DIRECTION ( 'NONE',  ( 0.3543493200069162685, -0.000000000000000000, -0.9351131265310288487 ) ) ;
#63326 = CARTESIAN_POINT ( 'NONE',  ( 11.15971793293161340, -22.22500000000000142, 22.46322236200905209 ) ) ;
#63327 = CARTESIAN_POINT ( 'NONE',  ( 13.10373647476855297, 5.808823158059036373, 5.808823158059032821 ) ) ;
#63328 = DIRECTION ( 'NONE',  ( 0.7071067811865487940, 0.7071067811865463515, 0.000000000000000000 ) ) ;
#63329 = ADVANCED_FACE ( 'NONE', ( #117357 ), #18768, .F. ) ;
#63330 = VECTOR ( 'NONE', #140669, 1000.000000000000227 ) ;
#63331 = PLANE ( 'NONE',  #64544 ) ;
#63332 = LINE ( 'NONE', #139466, #93074 ) ;
#63333 = EDGE_CURVE ( 'NONE', #14760, #70281, #63041, .T. ) ;
#63334 = ORIENTED_EDGE ( 'NONE', *, *, #40412, .T. ) ;
#63335 = EDGE_CURVE ( 'NONE', #5782, #104397, #84760, .T. ) ;
#63336 = PLANE ( 'NONE',  #51347 ) ;
#63337 = LINE ( 'NONE', #108908, #35493 ) ;
#63338 = EDGE_CURVE ( 'NONE', #41423, #54775, #52814, .T. ) ;
#63339 = CARTESIAN_POINT ( 'NONE',  ( 34.91209685856478018, 5.291415217122922066, -3.054999999999995275 ) ) ;
#63340 = AXIS2_PLACEMENT_3D ( 'NONE', #121370, #131550, #63472 ) ;
#63341 = CARTESIAN_POINT ( 'NONE',  ( -6.932893218813454439, -40.13710678118653874, -40.00000000000000000 ) ) ;
#63342 = ORIENTED_EDGE ( 'NONE', *, *, #18485, .F. ) ;
#63343 = FACE_OUTER_BOUND ( 'NONE', #122808, .T. ) ;
#63344 = VECTOR ( 'NONE', #60188, 1000.000000000000227 ) ;
#63345 = ORIENTED_EDGE ( 'NONE', *, *, #54856, .F. ) ;
#63346 = EDGE_CURVE ( 'NONE', #36068, #10862, #41984, .T. ) ;
#63347 = ORIENTED_EDGE ( 'NONE', *, *, #93914, .F. ) ;
#63348 = DIRECTION ( 'NONE',  ( 0.3543493200069162685, -0.000000000000000000, -0.9351131265310288487 ) ) ;
#63349 = DIRECTION ( 'NONE',  ( -0.000000000000000000, -1.000000000000000000, -0.000000000000000000 ) ) ;
#63350 = ORIENTED_EDGE ( 'NONE', *, *, #78572, .T. ) ;
#63351 = DIRECTION ( 'NONE',  ( 0.7071067811865487940, -0.7071067811865463515, 0.000000000000000000 ) ) ;
#63353 = VECTOR ( 'NONE', #18479, 1000.000000000000000 ) ;
#63352 = CARTESIAN_POINT ( 'NONE',  ( -31.49999999999977973, -4.533600742197687161, 5.000000000000000000 ) ) ;
#63354 = ADVANCED_FACE ( 'NONE', ( #108608 ), #96307, .F. ) ;
#63355 = CARTESIAN_POINT ( 'NONE',  ( 57.18398860626899705, 28.73617430169827358, 5.000000000000000000 ) ) ;
#63356 = EDGE_CURVE ( 'NONE', #10452, #93773, #30375, .T. ) ;
#63357 = CARTESIAN_POINT ( 'NONE',  ( 82.37500000000000000, 7.950000000000000178, 1.460391307983218535E-15 ) ) ;
#63358 = CARTESIAN_POINT ( 'NONE',  ( -3.183988606268992161, 28.73617430169789699, 5.000000000000000000 ) ) ;
#63359 = ORIENTED_EDGE ( 'NONE', *, *, #69348, .F. ) ;
#63360 = CARTESIAN_POINT ( 'NONE',  ( -3.469446951953614189E-15, 4.965500833774328271, -4.007596771432656801 ) ) ;
#63361 = DIRECTION ( 'NONE',  ( 0.000000000000000000, 1.000000000000000000, -5.782411586589357244E-15 ) ) ;
#63362 = DIRECTION ( 'NONE',  ( -0.000000000000000000, 0.3543493200069153248, 0.9351131265310292928 ) ) ;
#63363 = CARTESIAN_POINT ( 'NONE',  ( -5.588385094051650626, 22.22500000000000142, 4.777194822843815913 ) ) ;
#63364 = EDGE_CURVE ( 'NONE', #129025, #4192, #75328, .T. ) ;
#63365 = CARTESIAN_POINT ( 'NONE',  ( 104.2041937171295700, -6.884901960086285300, -3.975000000000000089 ) ) ;
#63366 = AXIS2_PLACEMENT_3D ( 'NONE', #52683, #30967, #109212 ) ;
#63367 = CARTESIAN_POINT ( 'NONE',  ( 58.70419371712954870, -6.884901960086285300, -3.975000000000000089 ) ) ;
#63368 = CONICAL_SURFACE ( 'NONE', #5350, 2.500000000000000888, 0.9599310885968822538 ) ;
#63369 = DIRECTION ( 'NONE',  ( 0.7071067811865487940, 0.7071067811865463515, 0.000000000000000000 ) ) ;
#63370 = EDGE_LOOP ( 'NONE', ( #122628, #29307, #20630, #53708 ) ) ;
#63371 = EDGE_LOOP ( 'NONE', ( #11090, #89233 ) ) ;
#63372 = CARTESIAN_POINT ( 'NONE',  ( 51.45833333333332860, 3.974999999999997424, 6.884901960086288852 ) ) ;
#63373 = DIRECTION ( 'NONE',  ( 0.000000000000000000, -1.000000000000000000, 0.000000000000000000 ) ) ;
#63374 = DIRECTION ( 'NONE',  ( 0.7071067811865487940, 0.7071067811865463515, 0.000000000000000000 ) ) ;
#63375 =( GEOMETRIC_REPRESENTATION_CONTEXT ( 3 ) GLOBAL_UNCERTAINTY_ASSIGNED_CONTEXT ( ( #127485 ) ) GLOBAL_UNIT_ASSIGNED_CONTEXT ( ( #31779, #141991, #140521 ) ) REPRESENTATION_CONTEXT ( 'NONE', 'WORKASPACE' ) );
#63376 = SURFACE_STYLE_USAGE ( .BOTH. , #114318 ) ;
#63377 = ORIENTED_EDGE ( 'NONE', *, *, #114002, .F. ) ;
#63378 = LINE ( 'NONE', #120534, #14438 ) ;
#63379 = CARTESIAN_POINT ( 'NONE',  ( 50.45876352523143282, 0.000000000000000000, -6.110000000000001208 ) ) ;
#63380 = ORIENTED_EDGE ( 'NONE', *, *, #115404, .T. ) ;
#63381 = ADVANCED_FACE ( 'NONE', ( #119494 ), #40557, .T. ) ;
#63382 = CARTESIAN_POINT ( 'NONE',  ( 4.911592354503321545, 9.902892378096218942E-16, 0.000000000000000000 ) ) ;
#63383 = EDGE_LOOP ( 'NONE', ( #46728, #65220, #13769, #135220 ) ) ;
#63384 = ORIENTED_EDGE ( 'NONE', *, *, #74624, .T. ) ;
#63385 = CIRCLE ( 'NONE', #100405, 2.500000000000000444 ) ;
#63386 = DIRECTION ( 'NONE',  ( -1.000000000000000000, -1.224606353822377258E-16, -0.000000000000000000 ) ) ;
#63387 = SURFACE_STYLE_FILL_AREA ( #128607 ) ;
#63388 = CYLINDRICAL_SURFACE ( 'NONE', #48931, 0.5000000000000004441 ) ;
#63389 =( NAMED_UNIT ( * ) SI_UNIT ( $, .STERADIAN. ) SOLID_ANGLE_UNIT ( ) );
#63390 = ORIENTED_EDGE ( 'NONE', *, *, #13335, .T. ) ;
#63391 = DIRECTION ( 'NONE',  ( -0.3543493200069163240, 0.000000000000000000, 0.9351131265310288487 ) ) ;
#63393 = ORIENTED_EDGE ( 'NONE', *, *, #12875, .F. ) ;
#63392 = CARTESIAN_POINT ( 'NONE',  ( -16.96322138488664066, -0.7337853718385520807, -35.15696433214895933 ) ) ;
#63394 = CARTESIAN_POINT ( 'NONE',  ( 0.000000000000000000, 0.000000000000000000, 10.00000000000000000 ) ) ;
#63395 = CARTESIAN_POINT ( 'NONE',  ( -2.816011393730999401, 28.73617430169785436, 5.000000000000000000 ) ) ;
#63396 = CIRCLE ( 'NONE', #17000, 2.999999999999998224 ) ;
#63397 = CARTESIAN_POINT ( 'NONE',  ( -57.18398860626899705, 28.73617430169827358, 5.000000000000000000 ) ) ;
#63398 = DIRECTION ( 'NONE',  ( 0.7071067811865487940, 0.7071067811865463515, 0.000000000000000000 ) ) ;
#63399 = EDGE_CURVE ( 'NONE', #107560, #132680, #73194, .T. ) ;
#63400 = ORIENTED_EDGE ( 'NONE', *, *, #84852, .T. ) ;
#63401 = ORIENTED_EDGE ( 'NONE', *, *, #26593, .F. ) ;
#63402 = CIRCLE ( 'NONE', #121501, 2.055000000000000604 ) ;
#63403 = DIRECTION ( 'NONE',  ( 0.7071067811865486830, -0.7071067811865464625, -0.000000000000000000 ) ) ;
#63404 = CARTESIAN_POINT ( 'NONE',  ( 65.53709685856478018, -3.054999999999998828, -5.291415217122919401 ) ) ;
#63405 = CARTESIAN_POINT ( 'NONE',  ( -27.32816939922334143, -6.740707523384214639, 4.000000000000000000 ) ) ;
#63406 = EDGE_CURVE ( 'NONE', #49442, #129167, #18030, .T. ) ;
#63407 = CARTESIAN_POINT ( 'NONE',  ( 8.671830600776416986, -9.740707523384180888, 4.000000000000000000 ) ) ;
#63408 = FACE_OUTER_BOUND ( 'NONE', #70356, .T. ) ;
#63409 = ORIENTED_EDGE ( 'NONE', *, *, #82838, .T. ) ;
#63410 = ORIENTED_EDGE ( 'NONE', *, *, #67932, .F. ) ;
#63411 = LINE ( 'NONE', #87978, #44755 ) ;
#63412 = DIRECTION ( 'NONE',  ( 0.7071067811865486830, -0.7071067811865464625, -0.000000000000000000 ) ) ;
#63413 = ORIENTED_EDGE ( 'NONE', *, *, #95698, .T. ) ;
#63414 = VECTOR ( 'NONE', #44905, 1000.000000000000000 ) ;
#63415 = VERTEX_POINT ( 'NONE', #95626 ) ;
#63416 = EDGE_CURVE ( 'NONE', #89630, #137664, #139880, .T. ) ;
#63417 = DIRECTION ( 'NONE',  ( -0.7071067811865487940, 0.7071067811865463515, 0.000000000000000000 ) ) ;
#63418 = VERTEX_POINT ( 'NONE', #99433 ) ;
#63419 = CARTESIAN_POINT ( 'NONE',  ( 17.66989781452724984, 17.25929247661554555, 19.83885114516067105 ) ) ;
#63420 = CARTESIAN_POINT ( 'NONE',  ( 0.1429064800270019031, 0.5999999999999986455, 3.726828488909569081 ) ) ;
#63421 = CARTESIAN_POINT ( 'NONE',  ( -34.92500000000001137, -17.24070752338410628, 4.255531930566259113 ) ) ;
#63422 = ADVANCED_FACE ( 'NONE', ( #77026 ), #119061, .T. ) ;
#63423 = FACE_BOUND ( 'NONE', #118210, .T. ) ;
#63424 = DIRECTION ( 'NONE',  ( 0.3543493200069162685, -0.000000000000000000, -0.9351131265310288487 ) ) ;
#63425 = DIRECTION ( 'NONE',  ( -1.000000000000000000, -0.000000000000000000, -0.000000000000000000 ) ) ;
#63426 = CARTESIAN_POINT ( 'NONE',  ( -15.70710678118643422, 8.259292476615641476, 5.000000000000000000 ) ) ;
#63428 = ORIENTED_EDGE ( 'NONE', *, *, #8250, .F. ) ;
#63427 = LINE ( 'NONE', #75007, #108268 ) ;
#63429 = VECTOR ( 'NONE', #124908, 1000.000000000000000 ) ;
#63430 = CARTESIAN_POINT ( 'NONE',  ( -14.99999999999989164, -15.03360074219758857, 5.000000000000000000 ) ) ;
#63431 = CONTEXT_DEPENDENT_SHAPE_REPRESENTATION ( #114292, #40059 ) ;
#63432 = ORIENTED_EDGE ( 'NONE', *, *, #70184, .F. ) ;
#63433 = AXIS2_PLACEMENT_3D ( 'NONE', #60862, #84708, #8520 ) ;
#63434 = VERTEX_POINT ( 'NONE', #121199 ) ;
#63435 = CARTESIAN_POINT ( 'NONE',  ( 87.55793019189812298, 6.110000000000000320, -1.637169565754156064 ) ) ;
#63436 = ORIENTED_EDGE ( 'NONE', *, *, #34819, .F. ) ;
#63437 = FACE_OUTER_BOUND ( 'NONE', #112700, .T. ) ;
#63438 = DIRECTION ( 'NONE',  ( 0.000000000000000000, 0.000000000000000000, 1.000000000000000000 ) ) ;
#63439 = AXIS2_PLACEMENT_3D ( 'NONE', #10292, #132107, #98727 ) ;
#63440 = PLANE ( 'NONE',  #65649 ) ;
#63441 = DIRECTION ( 'NONE',  ( 0.7071067811865487940, 0.7071067811865463515, -0.000000000000000000 ) ) ;
#63442 = EDGE_CURVE ( 'NONE', #33782, #942, #77331, .T. ) ;
#63443 = DIRECTION ( 'NONE',  ( 0.9843059135695010342, 0.000000000000000000, 0.1764705882352919641 ) ) ;
#63444 = VECTOR ( 'NONE', #20284, 1000.000000000000227 ) ;
#63445 = LINE ( 'NONE', #107612, #78292 ) ;
#63446 = CARTESIAN_POINT ( 'NONE',  ( -69.29974487139159578, -27.71228299555254537, 4.000000000000000000 ) ) ;
#63447 = CARTESIAN_POINT ( 'NONE',  ( 6.066782984417857350, 4.584330080086930965E-16, 0.000000000000000000 ) ) ;
#63448 = ORIENTED_EDGE ( 'NONE', *, *, #31909, .F. ) ;
#63449 = DIRECTION ( 'NONE',  ( -1.000000000000000000, -0.000000000000000000, -0.000000000000000000 ) ) ;
#63450 = ORIENTED_EDGE ( 'NONE', *, *, #120717, .F. ) ;
#63451 = CARTESIAN_POINT ( 'NONE',  ( -17.95341186370444930, 14.25929247661557753, 18.84478104361332385 ) ) ;
#63452 = CARTESIAN_POINT ( 'NONE',  ( -14.99999999999988987, -9.033600742197641864, 5.000000000000000000 ) ) ;
#63453 = VECTOR ( 'NONE', #104637, 1000.000000000000227 ) ;
#63454 = ORIENTED_EDGE ( 'NONE', *, *, #41107, .F. ) ;
#63455 = VERTEX_POINT ( 'NONE', #8821 ) ;
#63456 = AXIS2_PLACEMENT_3D ( 'NONE', #93585, #127645, #37051 ) ;
#63457 = EDGE_CURVE ( 'NONE', #105369, #25809, #20450, .T. ) ;
#63458 = EDGE_LOOP ( 'NONE', ( #90001, #66810, #133680, #113218 ) ) ;
#63459 = CARTESIAN_POINT ( 'NONE',  ( 38.35459685856476852, -1.637169565754161615, 6.110000000000000320 ) ) ;
#63460 = EDGE_LOOP ( 'NONE', ( #573, #54322, #96042, #61179, #90686, #77563 ) ) ;
#63462 = VECTOR ( 'NONE', #50753, 1000.000000000000000 ) ;
#63461 = PRODUCT_RELATED_PRODUCT_CATEGORY ( 'part', '', ( #142759 ) ) ;
#63463 = VECTOR ( 'NONE', #136172, 1000.000000000000000 ) ;
#63464 = CARTESIAN_POINT ( 'NONE',  ( 25.27497294953710849, 4.461849672132300881, 4.461849672132299105 ) ) ;
#63465 = CARTESIAN_POINT ( 'NONE',  ( -3.244551382801596606, 12.29205737877197713, -27.00337393511194151 ) ) ;
#63466 = VERTEX_POINT ( 'NONE', #19042 ) ;
#63467 = CARTESIAN_POINT ( 'NONE',  ( 0.000000000000000000, 0.000000000000000000, 5.000000000000000000 ) ) ;
#63468 = ORIENTED_EDGE ( 'NONE', *, *, #77784, .T. ) ;
#63469 = CARTESIAN_POINT ( 'NONE',  ( 34.42499999999998295, 21.72500000000000142, 0.5000000000000000000 ) ) ;
#63470 = VECTOR ( 'NONE', #51917, 1000.000000000000227 ) ;
#63471 = FACE_OUTER_BOUND ( 'NONE', #125278, .T. ) ;
#63473 = ORIENTED_EDGE ( 'NONE', *, *, #14016, .F. ) ;
#63472 = DIRECTION ( 'NONE',  ( -0.7071067811865486830, 0.7071067811865464625, 0.000000000000000000 ) ) ;
#63474 = VERTEX_POINT ( 'NONE', #41500 ) ;
#63475 = EDGE_CURVE ( 'NONE', #32751, #105463, #54553, .T. ) ;
#63476 = CARTESIAN_POINT ( 'NONE',  ( -60.48921356237309510, -27.52281430457097500, 5.000000000000000000 ) ) ;
#63477 = LINE ( 'NONE', #107643, #42539 ) ;
#63478 = ORIENTED_EDGE ( 'NONE', *, *, #30496, .T. ) ;
#63479 = AXIS2_PLACEMENT_3D ( 'NONE', #982, #101018, #45266 ) ;
#63480 = CARTESIAN_POINT ( 'NONE',  ( 108.8708603837962272, 6.884901960086289741, -3.974999999999993427 ) ) ;
#63481 = VERTEX_POINT ( 'NONE', #74887 ) ;
#63482 = VERTEX_POINT ( 'NONE', #10294 ) ;
#63483 = ORIENTED_EDGE ( 'NONE', *, *, #45362, .F. ) ;
#63484 = PLANE ( 'NONE',  #118902 ) ;
#63485 = VECTOR ( 'NONE', #82537, 1000.000000000000000 ) ;
#63486 = DIRECTION ( 'NONE',  ( -1.000000000000000000, -1.224606353822377258E-16, -0.000000000000000000 ) ) ;
#63487 = CARTESIAN_POINT ( 'NONE',  ( -28.49999999999978684, 19.08746187583905041, 4.000000000000000000 ) ) ;
#63488 = CARTESIAN_POINT ( 'NONE',  ( -25.82816939922334853, -20.24070752338407431, 4.000000000000000000 ) ) ;
#63489 = DIRECTION ( 'NONE',  ( 0.000000000000000000, 1.000000000000000000, 0.000000000000000000 ) ) ;
#63490 = VERTEX_POINT ( 'NONE', #55253 ) ;
#63491 = CARTESIAN_POINT ( 'NONE',  ( 10.49999999999992895, 12.43112307739206024, 4.000000000000000000 ) ) ;
#63492 = ORIENTED_EDGE ( 'NONE', *, *, #11671, .T. ) ;
#63493 = LINE ( 'NONE', #96752, #125842 ) ;
#63494 = CARTESIAN_POINT ( 'NONE',  ( 29.72873647476855297, 5.808823158059031044, -5.808823158059038150 ) ) ;
#63495 = EDGE_CURVE ( 'NONE', #136020, #32222, #109615, .T. ) ;
#63497 = ORIENTED_EDGE ( 'NONE', *, *, #3068, .T. ) ;
#63496 = VECTOR ( 'NONE', #61853, 1000.000000000000000 ) ;
#63498 = CARTESIAN_POINT ( 'NONE',  ( 45.18398860626900415, 28.73617430169818832, 5.000000000000000000 ) ) ;
#63499 = CARTESIAN_POINT ( 'NONE',  ( 15.70710678118643955, 17.25929247661554200, 5.000000000000000000 ) ) ;
#63500 = ORIENTED_EDGE ( 'NONE', *, *, #57338, .F. ) ;
#63501 = ADVANCED_FACE ( 'NONE', ( #52378 ), #132109, .T. ) ;
#63502 = ORIENTED_EDGE ( 'NONE', *, *, #116771, .T. ) ;
#63503 = CARTESIAN_POINT ( 'NONE',  ( 9.489213562373095101, -27.52281430457062328, 5.000000000000000000 ) ) ;
#63504 = DIRECTION ( 'NONE',  ( -1.000000000000000000, -0.000000000000000000, -0.000000000000000000 ) ) ;
#63505 = ADVANCED_FACE ( 'NONE', ( #64701 ), #87158, .F. ) ;
#63506 = LINE ( 'NONE', #74360, #53911 ) ;
#63507 = CARTESIAN_POINT ( 'NONE',  ( 16.98012225071442316, -17.24070752338409918, 20.23474786156473115 ) ) ;
#63508 = CARTESIAN_POINT ( 'NONE',  ( 22.11017322888194769, -22.22500000000000142, 4.785647885939353863 ) ) ;
#63509 = ADVANCED_FACE ( 'NONE', ( #131383 ), #96564, .F. ) ;
#63511 = ADVANCED_FACE ( 'NONE', ( #19752 ), #129955, .T. ) ;
#63510 = CARTESIAN_POINT ( 'NONE',  ( 61.74543019189811588, -5.291415217122919401, -3.055000000000000604 ) ) ;
#63512 = CARTESIAN_POINT ( 'NONE',  ( 73.43336038379621300, 2.130196079827431532, -7.949999999999996625 ) ) ;
#63513 = SURFACE_STYLE_USAGE ( .BOTH. , #9796 ) ;
#63514 = CARTESIAN_POINT ( 'NONE',  ( -18.18398860626898994, 28.73617430169800002, 5.000000000000000000 ) ) ;
#63515 = CARTESIAN_POINT ( 'NONE',  ( -33.79289321881321939, 6.759292476615654799, 5.000000000000000000 ) ) ;
#63516 = ORIENTED_EDGE ( 'NONE', *, *, #78201, .F. ) ;
#63517 = DIRECTION ( 'NONE',  ( -0.7071067811865486830, -0.7071067811865464625, -0.000000000000000000 ) ) ;
#63518 = EDGE_LOOP ( 'NONE', ( #53547, #123093, #130983, #139775 ) ) ;
#63519 = DIRECTION ( 'NONE',  ( -0.000000000000000000, -0.3543493200069152693, 0.9351131265310292928 ) ) ;
#63520 = CARTESIAN_POINT ( 'NONE',  ( -34.49999999999975842, 0.4497235411627144019, -5.599840258123620629 ) ) ;
#63521 = EDGE_LOOP ( 'NONE', ( #35183, #96771, #98348, #14568 ) ) ;
#63522 = DIRECTION ( 'NONE',  ( 0.000000000000000000, 0.000000000000000000, -1.000000000000000000 ) ) ;
#63524 = EDGE_LOOP ( 'NONE', ( #72982, #124734, #1751, #141102, #44881, #18490 ) ) ;
#63523 = CARTESIAN_POINT ( 'NONE',  ( -45.18398860626900415, 28.73617430169818832, 5.000000000000000000 ) ) ;
#63525 = EDGE_CURVE ( 'NONE', #128612, #16746, #53839, .T. ) ;
#63526 = CARTESIAN_POINT ( 'NONE',  ( 0.000000000000000000, 0.000000000000000000, 5.000000000000000000 ) ) ;
#63527 = EDGE_CURVE ( 'NONE', #7366, #19220, #42961, .T. ) ;
#63528 = CARTESIAN_POINT ( 'NONE',  ( -34.92500000000001137, -9.183345613589475320, 4.500000000000000888 ) ) ;
#63529 = DIRECTION ( 'NONE',  ( 0.6830127018922180770, -0.6830127018922204085, -0.2588190451025213501 ) ) ;
#63530 = EDGE_LOOP ( 'NONE', ( #112128, #8697, #14491, #118101 ) ) ;
#63531 = ORIENTED_EDGE ( 'NONE', *, *, #99183, .T. ) ;
#63532 = FACE_OUTER_BOUND ( 'NONE', #50021, .T. ) ;
#63533 = UNCERTAINTY_MEASURE_WITH_UNIT (LENGTH_MEASURE( 1.000000000000000082E-05 ), #98576, 'distance_accuracy_value', 'NONE');
#63534 = VECTOR ( 'NONE', #45434, 1000.000000000000000 ) ;
#63535 = CARTESIAN_POINT ( 'NONE',  ( 21.70710678118638981, -3.740707523384241728, 5.000000000000000000 ) ) ;
#63536 = EDGE_CURVE ( 'NONE', #128596, #60521, #2989, .T. ) ;
#63537 = CARTESIAN_POINT ( 'NONE',  ( 84.22502705046287019, 5.819803920172573086, -5.819803920172572198 ) ) ;
#63538 = DIRECTION ( 'NONE',  ( -0.000000000000000000, 0.3543493200069153248, 0.9351131265310292928 ) ) ;
#63539 = AXIS2_PLACEMENT_3D ( 'NONE', #46233, #123056, #15663 ) ;
#63540 = DIRECTION ( 'NONE',  ( 0.3543493200069163240, 0.000000000000000000, 0.9351131265310288487 ) ) ;
#63541 = EDGE_LOOP ( 'NONE', ( #117771, #92450, #91719, #78921 ) ) ;
#63542 = DIRECTION ( 'NONE',  ( -0.7071067811865487940, 0.7071067811865463515, -0.000000000000000000 ) ) ;
#63543 = AXIS2_PLACEMENT_3D ( 'NONE', #118581, #72985, #117141 ) ;
#63544 = DIRECTION ( 'NONE',  ( 1.000000000000000000, 0.000000000000000000, 0.000000000000000000 ) ) ;
#63545 = FACE_OUTER_BOUND ( 'NONE', #127036, .T. ) ;
#63546 = ADVANCED_FACE ( 'NONE', ( #111773 ), #14593, .T. ) ;
#63547 = ORIENTED_EDGE ( 'NONE', *, *, #89910, .T. ) ;
#63548 = DIRECTION ( 'NONE',  ( -1.000000000000000000, -0.000000000000000000, -0.000000000000000000 ) ) ;
#63549 = EDGE_LOOP ( 'NONE', ( #133610, #102562, #119437, #8603 ) ) ;
#63550 = VECTOR ( 'NONE', #101428, 1000.000000000000000 ) ;
#63551 = CARTESIAN_POINT ( 'NONE',  ( 76.27126352523144703, 4.472830434245839371, 4.472830434245842035 ) ) ;
#63552 = DIRECTION ( 'NONE',  ( 0.3543493200069162685, -0.000000000000000000, -0.9351131265310288487 ) ) ;
#63553 = EDGE_CURVE ( 'NONE', #1294, #97836, #55544, .T. ) ;
#63554 = DIRECTION ( 'NONE',  ( -1.000000000000000000, -1.224606353822377258E-16, -0.000000000000000000 ) ) ;
#63555 = ORIENTED_EDGE ( 'NONE', *, *, #27513, .F. ) ;
#63556 = LINE ( 'NONE', #66387, #69685 ) ;
#63557 = CARTESIAN_POINT ( 'NONE',  ( 14.99999999999989697, 16.93112307739200872, 4.000000000000000000 ) ) ;
#63558 = VECTOR ( 'NONE', #40641, 999.9999999999998863 ) ;
#63559 = FACE_OUTER_BOUND ( 'NONE', #22572, .T. ) ;
#63560 = LINE ( 'NONE', #11244, #113389 ) ;
#63562 = VERTEX_POINT ( 'NONE', #13848 ) ;
#63561 = DIRECTION ( 'NONE',  ( -0.000000000000000000, -0.000000000000000000, 1.000000000000000000 ) ) ;
#63563 = CARTESIAN_POINT ( 'NONE',  ( 128.9683591370938416, -49.14999999999998437, -41.64500000000001023 ) ) ;
#63564 = CARTESIAN_POINT ( 'NONE',  ( -1.786780966966399209, 12.75929247661558996, 10.29404684609034781 ) ) ;
#63565 = LINE ( 'NONE', #88148, #23944 ) ;
#63566 = CARTESIAN_POINT ( 'NONE',  ( -72.29974487139158157, -27.71228299555256669, 4.000000000000000000 ) ) ;
#63567 = VECTOR ( 'NONE', #82022, 999.9999999999998863 ) ;
#63568 = ORIENTED_EDGE ( 'NONE', *, *, #25823, .F. ) ;
#63569 = EDGE_CURVE ( 'NONE', #79010, #130681, #122629, .T. ) ;
#63570 = ORIENTED_EDGE ( 'NONE', *, *, #32152, .T. ) ;
#63571 = CARTESIAN_POINT ( 'NONE',  ( 75.10459685856474721, 1.637169565754164946, -6.109999999999999432 ) ) ;
#63572 = VECTOR ( 'NONE', #63988, 1000.000000000000000 ) ;
#63573 = VECTOR ( 'NONE', #59388, 1000.000000000000227 ) ;
#63574 = VERTEX_POINT ( 'NONE', #90750 ) ;
#63575 = LINE ( 'NONE', #9857, #112445 ) ;
#63576 = DIRECTION ( 'NONE',  ( 0.7071067811865486830, -0.7071067811865464625, -0.000000000000000000 ) ) ;
#63577 = DIRECTION ( 'NONE',  ( -0.7071067811865487940, 0.7071067811865463515, 0.000000000000000000 ) ) ;
#63578 = DIRECTION ( 'NONE',  ( -0.3543493200069162685, -0.000000000000000000, -0.9351131265310288487 ) ) ;
#63579 = EDGE_LOOP ( 'NONE', ( #72370, #25613, #13566, #63643, #55989, #77099 ) ) ;
#63580 = CARTESIAN_POINT ( 'NONE',  ( 57.18398860626899705, 28.73617430169827358, 5.000000000000000000 ) ) ;
#63582 =( BOUNDED_CURVE ( )  B_SPLINE_CURVE ( 3, ( #75345, #119505, #111518, #97787 ),
 .UNSPECIFIED., .F., .F. ) 
 B_SPLINE_CURVE_WITH_KNOTS ( ( 4, 4 ),
 ( 4.987589563512864643, 5.034563671340741564 ),
 .UNSPECIFIED. ) 
 CURVE ( )  GEOMETRIC_REPRESENTATION_ITEM ( )  RATIONAL_B_SPLINE_CURVE ( ( 1.000000000000000000, 0.9998161278856747547, 0.9998161278856747547, 1.000000000000000000 ) ) 
 REPRESENTATION_ITEM ( '' )  );
#63581 = FACE_OUTER_BOUND ( 'NONE', #22277, .T. ) ;
#63583 = AXIS2_PLACEMENT_3D ( 'NONE', #138118, #38806, #6833 ) ;
#63584 = ORIENTED_EDGE ( 'NONE', *, *, #123462, .F. ) ;
#63585 = ADVANCED_FACE ( 'NONE', ( #46562 ), #56721, .T. ) ;
#63586 = CARTESIAN_POINT ( 'NONE',  ( 0.6679544216110644417, -1.152520817846947043, 3.947122439933573812 ) ) ;
#63587 = CARTESIAN_POINT ( 'NONE',  ( 2.700255128608413990, -27.71228299555204089, 4.000000000000000000 ) ) ;
#63588 = DIRECTION ( 'NONE',  ( 0.7071067811865486830, -0.7071067811865464625, -0.000000000000000000 ) ) ;
#63589 = ORIENTED_EDGE ( 'NONE', *, *, #63060, .F. ) ;
#63590 = VERTEX_POINT ( 'NONE', #44401 ) ;
#63591 = EDGE_CURVE ( 'NONE', #111361, #130559, #108672, .T. ) ;
#63592 = LINE ( 'NONE', #108439, #100942 ) ;
#63593 = CARTESIAN_POINT ( 'NONE',  ( 1.499999999999989120, -20.53675388469230256, 2.352720554255897323 ) ) ;
#63594 = CARTESIAN_POINT ( 'NONE',  ( 127.1386022459138019, -7.776507174585692163E-16, 6.349999999999999645 ) ) ;
#63595 = LINE ( 'NONE', #51981, #141634 ) ;
#63596 =( NAMED_UNIT ( * ) PLANE_ANGLE_UNIT ( ) SI_UNIT ( $, .RADIAN. ) );
#63597 = CARTESIAN_POINT ( 'NONE',  ( 0.000000000000000000, 0.000000000000000000, 5.000000000000000000 ) ) ;
#63598 = FILL_AREA_STYLE_COLOUR ( '', #40136 ) ;
#63599 = VERTEX_POINT ( 'NONE', #113902 ) ;
#63600 = VERTEX_POINT ( 'NONE', #57407 ) ;
#63601 = ORIENTED_EDGE ( 'NONE', *, *, #113989, .T. ) ;
#63602 = ORIENTED_EDGE ( 'NONE', *, *, #42750, .T. ) ;
#63603 =( NAMED_UNIT ( * ) PLANE_ANGLE_UNIT ( ) SI_UNIT ( $, .RADIAN. ) );
#63604 = AXIS2_PLACEMENT_3D ( 'NONE', #52171, #49361, #18819 ) ;
#63605 = DIRECTION ( 'NONE',  ( 1.000000000000000000, 0.000000000000000000, 0.000000000000000000 ) ) ;
#63606 = PLANE ( 'NONE',  #63366 ) ;
#63607 = EDGE_LOOP ( 'NONE', ( #34455, #7042, #10794, #73318 ) ) ;
#63608 = FACE_OUTER_BOUND ( 'NONE', #126039, .T. ) ;
#63609 = LINE ( 'NONE', #97613, #10168 ) ;
#63610 = ADVANCED_FACE ( 'NONE', ( #66841 ), #55988, .T. ) ;
#63611 = DIRECTION ( 'NONE',  ( 0.000000000000000000, -0.2631995976047492580, -0.9647414015272165466 ) ) ;
#63612 = CARTESIAN_POINT ( 'NONE',  ( -4.171830600776436526, 0.7592924766157138627, 4.000000000000000000 ) ) ;
#63613 = CARTESIAN_POINT ( 'NONE',  ( 19.89359858452208130, 2.055000000000001048, 2.516649172247811554E-16 ) ) ;
#63614 = ORIENTED_EDGE ( 'NONE', *, *, #106320, .F. ) ;
#63615 = DIRECTION ( 'NONE',  ( 0.7071067811865487940, 0.7071067811865463515, 0.000000000000000000 ) ) ;
#63616 = CARTESIAN_POINT ( 'NONE',  ( 51.60416666666665009, 2.130196079827498146, 7.949999999999958433 ) ) ;
#63617 = ORIENTED_EDGE ( 'NONE', *, *, #41052, .T. ) ;
#63618 = EDGE_CURVE ( 'NONE', #112333, #122150, #132837, .T. ) ;
#63619 = DIRECTION ( 'NONE',  ( 2.110369192185896011E-16, -1.000000000000000000, 0.000000000000000000 ) ) ;
#63620 = EDGE_LOOP ( 'NONE', ( #23859, #122785, #65580, #78257 ) ) ;
#63621 = EDGE_CURVE ( 'NONE', #72549, #11328, #101588, .T. ) ;
#63622 = ORIENTED_EDGE ( 'NONE', *, *, #34693, .F. ) ;
#63623 = CARTESIAN_POINT ( 'NONE',  ( 66.93793019189810423, -6.110000000000001208, 1.637169565754158951 ) ) ;
#63624 = AXIS2_PLACEMENT_3D ( 'NONE', #30635, #73418, #74864 ) ;
#63625 = EDGE_LOOP ( 'NONE', ( #70839, #68816, #1234, #103446 ) ) ;
#63626 = ORIENTED_EDGE ( 'NONE', *, *, #26766, .F. ) ;
#63627 = LINE ( 'NONE', #19373, #58194 ) ;
#63628 = VECTOR ( 'NONE', #112377, 999.9999999999998863 ) ;
#63629 = CARTESIAN_POINT ( 'NONE',  ( -0.2458603837962275163, 3.047499999999993214, -5.278424836066146320 ) ) ;
#63630 = CARTESIAN_POINT ( 'NONE',  ( 99.45876352523144703, 0.000000000000000000, -6.110000000000001208 ) ) ;
#63631 = DIRECTION ( 'NONE',  ( -0.7071067811865486830, 0.7071067811865464625, 0.000000000000000000 ) ) ;
#63632 = EDGE_CURVE ( 'NONE', #75329, #6181, #134978, .T. ) ;
#63633 = CIRCLE ( 'NONE', #5620, 2.500000000000000444 ) ;
#63634 = CARTESIAN_POINT ( 'NONE',  ( 56.99999999999999289, 0.000000000000000000, -7.950000000000000178 ) ) ;
#63635 = CARTESIAN_POINT ( 'NONE',  ( 5.999999999999956479, -2.904428200921311376, -6.989807076074958658 ) ) ;
#63636 = DIRECTION ( 'NONE',  ( 1.000000000000000000, 0.000000000000000000, 0.000000000000000000 ) ) ;
#63637 = EDGE_CURVE ( 'NONE', #26091, #101520, #45819, .T. ) ;
#63638 = LINE ( 'NONE', #73767, #16692 ) ;
#63639 = CYLINDRICAL_SURFACE ( 'NONE', #1104, 1.249999999999970690 ) ;
#63640 = ORIENTED_EDGE ( 'NONE', *, *, #40724, .T. ) ;
#63641 = PLANE ( 'NONE',  #80499 ) ;
#63642 = ORIENTED_EDGE ( 'NONE', *, *, #9571, .T. ) ;
#63643 = ORIENTED_EDGE ( 'NONE', *, *, #30784, .F. ) ;
#63644 = ORIENTED_EDGE ( 'NONE', *, *, #138169, .F. ) ;
#63645 = VERTEX_POINT ( 'NONE', #102341 ) ;
#63646 = LINE ( 'NONE', #51326, #130282 ) ;
#63647 = DIRECTION ( 'NONE',  ( 0.7071067811865487940, -0.7071067811865463515, 0.000000000000000000 ) ) ;
#63648 = CARTESIAN_POINT ( 'NONE',  ( 24.56840764549667355, 9.139736423841732040E-16, 0.000000000000000000 ) ) ;
#63649 = ORIENTED_EDGE ( 'NONE', *, *, #71392, .T. ) ;
#63650 = CARTESIAN_POINT ( 'NONE',  ( 3.221442824812094763, -48.88296141031990061, 39.14553452061911543 ) ) ;
#63651 = VERTEX_POINT ( 'NONE', #111020 ) ;
#63652 = AXIS2_PLACEMENT_3D ( 'NONE', #38830, #26523, #139602 ) ;
#63653 = CARTESIAN_POINT ( 'NONE',  ( 8.437069808101885116, 2.126176841940952134, -7.934999999999993392 ) ) ;
#63654 = LINE ( 'NONE', #20098, #4437 ) ;
#63655 = EDGE_CURVE ( 'NONE', #42001, #103370, #91455, .T. ) ;
#63656 = CARTESIAN_POINT ( 'NONE',  ( -13.01987774928539032, -17.24070752338409918, 20.23474786156466010 ) ) ;
#63657 = AXIS2_PLACEMENT_3D ( 'NONE', #64291, #98355, #107766 ) ;
#63658 = CARTESIAN_POINT ( 'NONE',  ( 22.49999999999984368, 9.431123077392088661, 4.000000000000000000 ) ) ;
#63659 = ORIENTED_EDGE ( 'NONE', *, *, #18605, .F. ) ;
#63660 = ADVANCED_FACE ( 'NONE', ( #113173 ), #133527, .F. ) ;
#63661 = EDGE_LOOP ( 'NONE', ( #54877, #11093, #45083, #22574 ) ) ;
#63662 = EDGE_LOOP ( 'NONE', ( #138564, #23991, #96097, #91239 ) ) ;
#63663 = DIRECTION ( 'NONE',  ( -1.000000000000000000, 0.000000000000000000, -0.000000000000000000 ) ) ;
#63664 = LINE ( 'NONE', #107824, #48812 ) ;
#63665 = CARTESIAN_POINT ( 'NONE',  ( -14.20666063542142687, 21.75929247661549937, 4.998822639870708073 ) ) ;
#63666 = CARTESIAN_POINT ( 'NONE',  ( -25.39999999999996305, 0.000000000000000000, 0.000000000000000000 ) ) ;
#63667 = EDGE_CURVE ( 'NONE', #137445, #133889, #134244, .T. ) ;
#63668 = ADVANCED_FACE ( 'NONE', ( #34937 ), #836, .F. ) ;
#63669 = DIRECTION ( 'NONE',  ( -1.000000000000000000, 0.000000000000000000, 0.000000000000000000 ) ) ;
#63670 = CARTESIAN_POINT ( 'NONE',  ( 0.000000000000000000, 0.000000000000000000, 0.000000000000000000 ) ) ;
#63671 = CARTESIAN_POINT ( 'NONE',  ( 25.37543019189810067, -5.291415217122920289, -3.055000000000001492 ) ) ;
#63672 = CARTESIAN_POINT ( 'NONE',  ( 8.536408254699722420, -22.22500000000000142, 21.46915226046162672 ) ) ;
#63673 = LINE ( 'NONE', #107832, #58228 ) ;
#63674 = ORIENTED_EDGE ( 'NONE', *, *, #5307, .T. ) ;
#63675 = CARTESIAN_POINT ( 'NONE',  ( 15.29974487139158867, -27.71228299555216879, 4.000000000000000000 ) ) ;
#63676 = CARTESIAN_POINT ( 'NONE',  ( -17.99999999999987566, 14.87792677143806941, -11.06722581663444060 ) ) ;
#63677 = EDGE_LOOP ( 'NONE', ( #12412, #70061, #5024, #641, #51113, #61732 ) ) ;
#63678 = DIRECTION ( 'NONE',  ( 0.7071067811865486830, -0.7071067811865464625, -0.000000000000000000 ) ) ;
#63680 = VERTEX_POINT ( 'NONE', #13137 ) ;
#63679 = CARTESIAN_POINT ( 'NONE',  ( 55.29044309249841405, -47.26730531257518919, -36.54674188582485783 ) ) ;
#63681 = EDGE_CURVE ( 'NONE', #102321, #63466, #2250, .T. ) ;
#63682 = EDGE_CURVE ( 'NONE', #70988, #7787, #73277, .T. ) ;
#63683 = CARTESIAN_POINT ( 'NONE',  ( 3.489213562373097322, -27.52281430457057709, 5.000000000000000000 ) ) ;
#63684 = VERTEX_POINT ( 'NONE', #70456 ) ;
#63685 = SURFACE_SIDE_STYLE ('',( #31745 ) ) ;
#63686 = ORIENTED_EDGE ( 'NONE', *, *, #57629, .F. ) ;
#63687 = DIRECTION ( 'NONE',  ( -0.3543493200069163240, 0.000000000000000000, 0.9351131265310288487 ) ) ;
#63688 = EDGE_LOOP ( 'NONE', ( #136608, #101725, #41311, #45208, #28007 ) ) ;
#63689 = SURFACE_STYLE_USAGE ( .BOTH. , #106404 ) ;
#63690 = CARTESIAN_POINT ( 'NONE',  ( 118.0583603837962130, -7.949999999999997513, -2.130196079827425759 ) ) ;
#63691 = FACE_OUTER_BOUND ( 'NONE', #8635, .T. ) ;
#63692 = ADVANCED_FACE ( 'NONE', ( #50794 ), #103034, .F. ) ;
#63693 = FACE_OUTER_BOUND ( 'NONE', #33031, .T. ) ;
#63694 = FILL_AREA_STYLE_COLOUR ( '', #100453 ) ;
#63695 = CARTESIAN_POINT ( 'NONE',  ( -32.48334561358932149, 22.22500000000000142, 4.500000000000000888 ) ) ;
#63696 = CARTESIAN_POINT ( 'NONE',  ( 5.395833333333334814, 1.633150327867687324, -6.094999999999991758 ) ) ;
#63697 = CARTESIAN_POINT ( 'NONE',  ( 19.95790314143522437, 6.871911579029515771, 3.967499999999989146 ) ) ;
#63698 = EDGE_CURVE ( 'NONE', #35574, #18121, #3674, .T. ) ;
#63699 = DIRECTION ( 'NONE',  ( -0.6830127018922180770, -0.6830127018922204085, -0.2588190451025213501 ) ) ;
#63700 = CARTESIAN_POINT ( 'NONE',  ( 13.35824297541131322, 15.75929247661555088, 19.34181609438696370 ) ) ;
#63701 = VERTEX_POINT ( 'NONE', #61694 ) ;
#63702 = ORIENTED_EDGE ( 'NONE', *, *, #73931, .T. ) ;
#63703 = LINE ( 'NONE', #116630, #28095 ) ;
#63704 = VERTEX_POINT ( 'NONE', #26193 ) ;
#63705 = LINE ( 'NONE', #41942, #133643 ) ;
#63706 = DIRECTION ( 'NONE',  ( -0.000000000000000000, 0.000000000000000000, 1.000000000000000000 ) ) ;
#63707 = CARTESIAN_POINT ( 'NONE',  ( -48.48921356237309510, -27.52281430457089328, 5.000000000000000000 ) ) ;
#63708 = EDGE_CURVE ( 'NONE', #132084, #47759, #15974, .T. ) ;
#63709 = ORIENTED_EDGE ( 'NONE', *, *, #128289, .T. ) ;
#63710 = CARTESIAN_POINT ( 'NONE',  ( 10.82816939922345156, -11.24070752338417201, 4.000000000000000000 ) ) ;
#63711 = DIRECTION ( 'NONE',  ( 0.7071067811865487940, -0.7071067811865463515, 0.000000000000000000 ) ) ;
#63712 = CARTESIAN_POINT ( 'NONE',  ( -3.299744871391591339, -27.71228299555208352, 4.000000000000000000 ) ) ;
#63713 = DIRECTION ( 'NONE',  ( 0.000000000000000000, 0.000000000000000000, 1.000000000000000000 ) ) ;
#63715 = ORIENTED_EDGE ( 'NONE', *, *, #75503, .F. ) ;
#63714 = CARTESIAN_POINT ( 'NONE',  ( -63.48921356237309510, -27.52281430457099631, 5.000000000000000000 ) ) ;
#63716 = CARTESIAN_POINT ( 'NONE',  ( -51.18398860626899705, 28.73617430169823095, 5.000000000000000000 ) ) ;
#63717 = ADVANCED_FACE ( 'NONE', ( #61006 ), #103709, .F. ) ;
#63718 = CARTESIAN_POINT ( 'NONE',  ( 69.68750000000000000, -5.819803920172573974, 5.819803920172573086 ) ) ;
#63719 = DIRECTION ( 'NONE',  ( -0.7071067811865487940, 0.7071067811865463515, -0.000000000000000000 ) ) ;
#63720 = CARTESIAN_POINT ( 'NONE',  ( 45.18398860626900415, 28.73617430169818832, 5.000000000000000000 ) ) ;
#63721 = DIRECTION ( 'NONE',  ( 0.3543493200069162685, -0.000000000000000000, -0.9351131265310288487 ) ) ;
#63722 = ORIENTED_EDGE ( 'NONE', *, *, #90073, .T. ) ;
#63723 = ADVANCED_FACE ( 'NONE', ( #84169 ), #88022, .T. ) ;
#63724 = VECTOR ( 'NONE', #73167, 1000.000000000000000 ) ;
#63725 = ORIENTED_EDGE ( 'NONE', *, *, #70898, .T. ) ;
#63726 = ORIENTED_EDGE ( 'NONE', *, *, #135209, .F. ) ;
#63727 = CARTESIAN_POINT ( 'NONE',  ( 103.9795968585647756, 6.109999999999999432, 1.637169565754164280 ) ) ;
#63728 =( BOUNDED_CURVE ( )  B_SPLINE_CURVE ( 3, ( #112803, #91085, #55596, #112116 ),
 .UNSPECIFIED., .F., .T. ) 
 B_SPLINE_CURVE_WITH_KNOTS ( ( 4, 4 ),
 ( 1.208578181583236821, 1.359146454359400957 ),
 .UNSPECIFIED. ) 
 CURVE ( )  GEOMETRIC_REPRESENTATION_ITEM ( )  RATIONAL_B_SPLINE_CURVE ( ( 1.000000000000000000, 0.9981116584018963067, 0.9981116584018963067, 1.000000000000000000 ) ) 
 REPRESENTATION_ITEM ( '' )  );
#63729 = ORIENTED_EDGE ( 'NONE', *, *, #19130, .T. ) ;
#63730 = VECTOR ( 'NONE', #127357, 1000.000000000000000 ) ;
#63731 = CARTESIAN_POINT ( 'NONE',  ( 124.0768256643112011, -45.23984008851422800, 35.04755940937925374 ) ) ;
#63732 = DIRECTION ( 'NONE',  ( 0.7071067811865486830, -0.7071067811865464625, -0.000000000000000000 ) ) ;
#63733 = ORIENTED_EDGE ( 'NONE', *, *, #32704, .F. ) ;
#63734 = EDGE_CURVE ( 'NONE', #29768, #119001, #141191, .T. ) ;
#63735 = FACE_OUTER_BOUND ( 'NONE', #47589, .T. ) ;
#63736 = CARTESIAN_POINT ( 'NONE',  ( 49.12500000000000000, -7.950000000000000178, -4.867971026610729436E-16 ) ) ;
#63737 = CARTESIAN_POINT ( 'NONE',  ( 91.78709685856478018, 3.054999999999997495, 5.291415217122919401 ) ) ;
#63738 = VECTOR ( 'NONE', #67428, 1000.000000000000000 ) ;
#63739 = ORIENTED_EDGE ( 'NONE', *, *, #3223, .T. ) ;
#63740 = CARTESIAN_POINT ( 'NONE',  ( 54.18398860626899705, 28.73617430169825226, 5.000000000000000000 ) ) ;
#63741 = CARTESIAN_POINT ( 'NONE',  ( -33.48921356237309510, -27.52281430457078670, 5.000000000000000000 ) ) ;
#63742 = CARTESIAN_POINT ( 'NONE',  ( 2.488313940715670913, 6.759292476615645917, 16.35960578974468760 ) ) ;
#63743 = CARTESIAN_POINT ( 'NONE',  ( 8.292893218813404133, 14.25929247661557753, 5.000000000000000000 ) ) ;
#63744 = VERTEX_POINT ( 'NONE', #139967 ) ;
#63745 = ORIENTED_EDGE ( 'NONE', *, *, #10334, .T. ) ;
#63746 = ORIENTED_EDGE ( 'NONE', *, *, #11344, .T. ) ;
#63747 = LINE ( 'NONE', #107218, #19075 ) ;
#63748 = CARTESIAN_POINT ( 'NONE',  ( 6.489213562373093325, -27.52281430457059841, 5.000000000000000000 ) ) ;
#63749 = LINE ( 'NONE', #8576, #135940 ) ;
#63750 = AXIS2_PLACEMENT_3D ( 'NONE', #118778, #2704, #113613 ) ;
#63751 = CARTESIAN_POINT ( 'NONE',  ( 12.71159235450332048, -5.777789833161707559E-31, 2.500000000000001332 ) ) ;
#63752 = VECTOR ( 'NONE', #125852, 1000.000000000000000 ) ;
#63753 = VECTOR ( 'NONE', #18007, 1000.000000000000000 ) ;
#63754 = ORIENTED_EDGE ( 'NONE', *, *, #78212, .F. ) ;
#63755 = ORIENTED_EDGE ( 'NONE', *, *, #86620, .T. ) ;
#63756 = LINE ( 'NONE', #97029, #129010 ) ;
#63758 = EDGE_CURVE ( 'NONE', #120820, #11462, #8660, .T. ) ;
#63757 = EDGE_LOOP ( 'NONE', ( #96513, #132186, #85429, #2075 ) ) ;
#63759 = ADVANCED_FACE ( 'NONE', ( #75410 ), #129771, .F. ) ;
#63760 = EDGE_LOOP ( 'NONE', ( #56059, #17555, #32575, #87002 ) ) ;
#63761 = CARTESIAN_POINT ( 'NONE',  ( 0.000000000000000000, 0.000000000000000000, 5.000000000000000000 ) ) ;
#63762 = CARTESIAN_POINT ( 'NONE',  ( -14.99999999999989164, 19.55218569542897100, 5.000000000000000000 ) ) ;
#63763 = ORIENTED_EDGE ( 'NONE', *, *, #64654, .T. ) ;
#63764 = LINE ( 'NONE', #54333, #129296 ) ;
#63765 =( LENGTH_UNIT ( ) NAMED_UNIT ( * ) SI_UNIT ( .MILLI., .METRE. ) );
#63766 = CARTESIAN_POINT ( 'NONE',  ( -34.42500000000001137, 0.000000000000000000, 4.500000000000000888 ) ) ;
#63767 = CARTESIAN_POINT ( 'NONE',  ( -12.20000000000000284, -35.14999999999999147, 17.49210858042621908 ) ) ;
#63768 = CARTESIAN_POINT ( 'NONE',  ( 28.49999999999980460, -10.53360074219763121, 5.000000000000000000 ) ) ;
#63769 = VERTEX_POINT ( 'NONE', #10132 ) ;
#63770 = FILL_AREA_STYLE_COLOUR ( '', #55736 ) ;
#63771 = CARTESIAN_POINT ( 'NONE',  ( 37.31250000000000000, 5.819803920172571310, 5.819803920172576639 ) ) ;
#63772 = ORIENTED_EDGE ( 'NONE', *, *, #50333, .F. ) ;
#63773 = CARTESIAN_POINT ( 'NONE',  ( -17.99451991528748351, 28.92564299267950645, 4.000000000000000000 ) ) ;
#63774 = EDGE_CURVE ( 'NONE', #93762, #97422, #142108, .T. ) ;
#63775 = CARTESIAN_POINT ( 'NONE',  ( 19.91089914266474281, -3.052838087030619096, -34.75743929853354786 ) ) ;
#63776 = ORIENTED_EDGE ( 'NONE', *, *, #90851, .F. ) ;
#63777 = CARTESIAN_POINT ( 'NONE',  ( 9.748407645496676821, 2.500000000000000888, 3.061616997868383141E-16 ) ) ;
#63778 = VERTEX_POINT ( 'NONE', #107989 ) ;
#63780 = ADVANCED_FACE ( 'NONE', ( #108697 ), #106499, .T. ) ;
#63779 = LINE ( 'NONE', #107937, #110658 ) ;
#63781 = VERTEX_POINT ( 'NONE', #118154 ) ;
#63782 = ORIENTED_EDGE ( 'NONE', *, *, #123667, .F. ) ;
#63783 = ORIENTED_EDGE ( 'NONE', *, *, #100311, .T. ) ;
#63784 = EDGE_CURVE ( 'NONE', #113425, #34606, #42794, .T. ) ;
#63785 = CARTESIAN_POINT ( 'NONE',  ( 31.70376352523145158, 6.109999999999998543, 1.122388791418548911E-15 ) ) ;
#63786 = PRESENTATION_STYLE_ASSIGNMENT (( #30430 ) ) ;
#63787 = CARTESIAN_POINT ( 'NONE',  ( 27.18398860626900060, 28.73617430169806042, 5.000000000000000000 ) ) ;
#63788 =( NAMED_UNIT ( * ) SI_UNIT ( $, .STERADIAN. ) SOLID_ANGLE_UNIT ( ) );
#63789 = CARTESIAN_POINT ( 'NONE',  ( 51.48921356237309510, -27.52281430457091460, 5.000000000000000000 ) ) ;
#63790 = ADVANCED_FACE ( 'NONE', ( #131935 ), #32627, .F. ) ;
#63791 = CARTESIAN_POINT ( 'NONE',  ( 24.48921356237309510, -27.52281430457072631, 5.000000000000000000 ) ) ;
#63792 = CARTESIAN_POINT ( 'NONE',  ( -59.99451991528749772, 28.92564299267980132, 4.000000000000000000 ) ) ;
#63793 = PLANE ( 'NONE',  #16735 ) ;
#63794 = ADVANCED_FACE ( 'NONE', ( #74712 ), #104129, .T. ) ;
#63795 = DIRECTION ( 'NONE',  ( 0.7071067811865487940, 0.7071067811865463515, 0.000000000000000000 ) ) ;
#63796 = CARTESIAN_POINT ( 'NONE',  ( -54.29974487139159578, -27.71228299555243879, 4.000000000000000000 ) ) ;
#63797 = CARTESIAN_POINT ( 'NONE',  ( -30.31657961132771462, -6.740707523384216415, 11.88629033278131253 ) ) ;
#63798 = ORIENTED_EDGE ( 'NONE', *, *, #74692, .F. ) ;
#63799 = VERTEX_POINT ( 'NONE', #40643 ) ;
#63800 = ORIENTED_EDGE ( 'NONE', *, *, #143347, .F. ) ;
#63801 = ORIENTED_EDGE ( 'NONE', *, *, #11960, .T. ) ;
#63802 = CARTESIAN_POINT ( 'NONE',  ( 35.99451991528749772, 28.92564299267963079, 4.000000000000000000 ) ) ;
#63803 = EDGE_CURVE ( 'NONE', #55828, #10662, #54394, .T. ) ;
#63804 = VERTEX_POINT ( 'NONE', #76117 ) ;
#63805 = ORIENTED_EDGE ( 'NONE', *, *, #59669, .F. ) ;
#63806 = CARTESIAN_POINT ( 'NONE',  ( 26.40000000000000568, -17.48000000000005016, -33.92499999999998295 ) ) ;
#63807 = PLANE ( 'NONE',  #17974 ) ;
#63808 = LINE ( 'NONE', #118875, #127336 ) ;
#63809 = VERTEX_POINT ( 'NONE', #76858 ) ;
#63810 = DIRECTION ( 'NONE',  ( 0.7071067811865487940, 0.7071067811865463515, 0.000000000000000000 ) ) ;
#63811 = EDGE_CURVE ( 'NONE', #29477, #17037, #71806, .T. ) ;
#63812 = VERTEX_POINT ( 'NONE', #130514 ) ;
#63813 = AXIS2_PLACEMENT_3D ( 'NONE', #128611, #29286, #83714 ) ;
#63814 = CARTESIAN_POINT ( 'NONE',  ( 27.29974487139158512, -27.71228299555225405, 4.000000000000000000 ) ) ;
#63815 = CARTESIAN_POINT ( 'NONE',  ( 12.60873647476855197, -5.808823158059033709, 5.808823158059035485 ) ) ;
#63816 = ORIENTED_EDGE ( 'NONE', *, *, #1520, .T. ) ;
#63817 = CARTESIAN_POINT ( 'NONE',  ( 90.03709685856478018, -3.054999999999999272, -5.291415217122919401 ) ) ;
#63818 =( GEOMETRIC_REPRESENTATION_CONTEXT ( 3 ) GLOBAL_UNCERTAINTY_ASSIGNED_CONTEXT ( ( #111257 ) ) GLOBAL_UNIT_ASSIGNED_CONTEXT ( ( #93309, #4814, #49115 ) ) REPRESENTATION_CONTEXT ( 'NONE', 'WORKASPACE' ) );
#63819 = CARTESIAN_POINT ( 'NONE',  ( -41.99451991528749062, 28.92564299267967343, 4.000000000000000000 ) ) ;
#63820 = CARTESIAN_POINT ( 'NONE',  ( -48.48921356237309510, -27.52281430457089328, 5.000000000000000000 ) ) ;
#63821 = VERTEX_POINT ( 'NONE', #142795 ) ;
#63822 = EDGE_CURVE ( 'NONE', #74472, #104351, #31193, .T. ) ;
#63823 = ORIENTED_EDGE ( 'NONE', *, *, #12871, .T. ) ;
#63824 = DIRECTION ( 'NONE',  ( -0.6830127018922181881, 0.6830127018922202975, -0.2588190451025214056 ) ) ;
#63825 = ORIENTED_EDGE ( 'NONE', *, *, #66618, .T. ) ;
#63826 = DIRECTION ( 'NONE',  ( 0.6830127018922181881, 0.6830127018922202975, -0.2588190451025214056 ) ) ;
#63827 = CARTESIAN_POINT ( 'NONE',  ( 15.96626304157554266, 4.202752102959690472E-16, 0.000000000000000000 ) ) ;
#63828 = PLANE ( 'NONE',  #58573 ) ;
#63829 = CARTESIAN_POINT ( 'NONE',  ( -34.92500000000001137, 22.22500000000000142, 4.000000000000000000 ) ) ;
#63830 = ORIENTED_EDGE ( 'NONE', *, *, #121619, .F. ) ;
#63831 = EDGE_CURVE ( 'NONE', #133340, #109375, #41324, .T. ) ;
#63832 = EDGE_CURVE ( 'NONE', #132213, #115620, #21003, .T. ) ;
#63833 = CARTESIAN_POINT ( 'NONE',  ( 5.380000000000000782, 9.521314400968980422E-16, 0.000000000000000000 ) ) ;
#63834 = CONICAL_SURFACE ( 'NONE', #132974, 2.500000000000000444, 0.9599310885968830309 ) ;
#63835 = CARTESIAN_POINT ( 'NONE',  ( -8.999999999999944933, 14.58746187583910903, 4.000000000000000000 ) ) ;
#63836 = DIRECTION ( 'NONE',  ( 0.7071067811865486830, -0.7071067811865464625, -0.000000000000000000 ) ) ;
#63837 = VERTEX_POINT ( 'NONE', #52213 ) ;
#63838 = DIRECTION ( 'NONE',  ( 0.7071067811865486830, -0.7071067811865464625, -0.000000000000000000 ) ) ;
#63840 = ADVANCED_FACE ( 'NONE', ( #129053 ), #109449, .F. ) ;
#63839 = PLANE ( 'NONE',  #121106 ) ;
#63841 = ORIENTED_EDGE ( 'NONE', *, *, #93484, .T. ) ;
#63843 = ORIENTED_EDGE ( 'NONE', *, *, #32136, .T. ) ;
#63842 = CARTESIAN_POINT ( 'NONE',  ( -1.499999999999986677, -16.53360074219757792, 5.000000000000000000 ) ) ;
#63845 = ORIENTED_EDGE ( 'NONE', *, *, #11005, .F. ) ;
#63844 = EDGE_CURVE ( 'NONE', #100802, #55039, #63126, .T. ) ;
#63846 = CARTESIAN_POINT ( 'NONE',  ( -8.999999999999925393, -22.06887692260758982, 4.000000000000000000 ) ) ;
#63847 = CARTESIAN_POINT ( 'NONE',  ( 153.4000000000000057, 26.96999999999993847, 34.92499999999998295 ) ) ;
#63848 = ORIENTED_EDGE ( 'NONE', *, *, #86125, .F. ) ;
#63849 = DIRECTION ( 'NONE',  ( 0.7071067811865487940, 0.7071067811865463515, -0.000000000000000000 ) ) ;
#63850 = UNCERTAINTY_MEASURE_WITH_UNIT (LENGTH_MEASURE( 1.000000000000000082E-05 ), #46762, 'distance_accuracy_value', 'NONE');
#63851 = CIRCLE ( 'NONE', #121758, 2.500000000000000888 ) ;
#63852 = CARTESIAN_POINT ( 'NONE',  ( 0.000000000000000000, 4.999999999999997335, -7.627214432543508948 ) ) ;
#63853 = VECTOR ( 'NONE', #26279, 1000.000000000000114 ) ;
#63854 = DIRECTION ( 'NONE',  ( 0.000000000000000000, 0.000000000000000000, 1.000000000000000000 ) ) ;
#63855 = VECTOR ( 'NONE', #101579, 1000.000000000000000 ) ;
#63856 = ADVANCED_FACE ( 'NONE', ( #47113 ), #80418, .F. ) ;
#63857 = CARTESIAN_POINT ( 'NONE',  ( 34.92499999999998295, 22.22500000000000142, 4.000000000000000000 ) ) ;
#63858 = CARTESIAN_POINT ( 'NONE',  ( 0.1600000000000008915, -3.866712830111943333, -6.953158445676763222 ) ) ;
#63859 = DIRECTION ( 'NONE',  ( -0.7071067811865486830, -0.7071067811865464625, 0.000000000000000000 ) ) ;
#63860 = DIRECTION ( 'NONE',  ( 0.7071067811865487940, 0.7071067811865463515, -0.000000000000000000 ) ) ;
#63861 = CARTESIAN_POINT ( 'NONE',  ( 1.500000000000001332, 10.46639925780216274, 5.000000000000000000 ) ) ;
#63862 = CARTESIAN_POINT ( 'NONE',  ( 17.51078643762690845, -27.52281430457043143, 5.000000000000000000 ) ) ;
#63863 = DIRECTION ( 'NONE',  ( -0.6830127018922180770, -0.6830127018922204085, -0.2588190451025213501 ) ) ;
#63864 = AXIS2_PLACEMENT_3D ( 'NONE', #139653, #40332, #70813 ) ;
#63865 = EDGE_CURVE ( 'NONE', #39389, #106040, #135505, .T. ) ;
#63866 = CARTESIAN_POINT ( 'NONE',  ( 1.629999999999999893, 0.4000000000000001887, -2.500000000000000000 ) ) ;
#63867 = CARTESIAN_POINT ( 'NONE',  ( 25.97159235450331849, 9.902892378096218942E-16, 0.000000000000000000 ) ) ;
#63868 = ORIENTED_EDGE ( 'NONE', *, *, #39113, .T. ) ;
#63869 = ORIENTED_EDGE ( 'NONE', *, *, #105018, .T. ) ;
#63870 = ORIENTED_EDGE ( 'NONE', *, *, #23922, .F. ) ;
#63871 = CARTESIAN_POINT ( 'NONE',  ( 107.6041666666666572, 2.130196079827422206, 7.950000000000001954 ) ) ;
#63872 = ORIENTED_EDGE ( 'NONE', *, *, #141699, .F. ) ;
#63873 = ORIENTED_EDGE ( 'NONE', *, *, #4009, .F. ) ;
#63874 = ORIENTED_EDGE ( 'NONE', *, *, #96654, .F. ) ;
#63875 = DIRECTION ( 'NONE',  ( 0.6830127018922180770, -0.6830127018922204085, -0.2588190451025213501 ) ) ;
#63876 = LINE ( 'NONE', #31244, #129626 ) ;
#63877 = EDGE_LOOP ( 'NONE', ( #76794, #35866, #86838, #93543 ) ) ;
#63878 = DIRECTION ( 'NONE',  ( -1.000000000000000000, -1.224606353822377258E-16, -0.000000000000000000 ) ) ;
#63879 = PLANE ( 'NONE',  #4598 ) ;
#63880 = DIRECTION ( 'NONE',  ( -0.000000000000000000, 0.000000000000000000, 1.000000000000000000 ) ) ;
#63881 = CARTESIAN_POINT ( 'NONE',  ( 9.591592354503321260, 9.902892378096218942E-16, 0.000000000000000000 ) ) ;
#63882 = CARTESIAN_POINT ( 'NONE',  ( 102.9587635252314470, 0.000000000000000000, -6.110000000000001208 ) ) ;
#63883 = ORIENTED_EDGE ( 'NONE', *, *, #50517, .F. ) ;
#63884 = PLANE ( 'NONE',  #106652 ) ;
#63885 = CARTESIAN_POINT ( 'NONE',  ( 51.48921356237309510, -27.52281430457091460, 5.000000000000000000 ) ) ;
#63886 = DIRECTION ( 'NONE',  ( 1.000000000000000000, 0.000000000000000000, 0.000000000000000000 ) ) ;
#63887 = CARTESIAN_POINT ( 'NONE',  ( -31.49999999999977973, 15.05218569542901186, 5.000000000000000000 ) ) ;
#63888 = DIRECTION ( 'NONE',  ( -0.7071067811865486830, -0.7071067811865464625, 0.000000000000000000 ) ) ;
#63889 = LINE ( 'NONE', #108051, #73182 ) ;
#63890 = CARTESIAN_POINT ( 'NONE',  ( 32.45419371712955581, 6.884901960086283523, 3.975000000000002753 ) ) ;
#63891 = CARTESIAN_POINT ( 'NONE',  ( -4.499999999999962697, -19.53360074219753884, 5.000000000000000000 ) ) ;
#63892 = ORIENTED_EDGE ( 'NONE', *, *, #117157, .T. ) ;
#63893 = ORIENTED_EDGE ( 'NONE', *, *, #120601, .F. ) ;
#63894 = CARTESIAN_POINT ( 'NONE',  ( 30.89583333333332860, -2.130196079827427091, 7.949999999999999289 ) ) ;
#63895 = VERTEX_POINT ( 'NONE', #36189 ) ;
#63896 = FACE_OUTER_BOUND ( 'NONE', #1853, .T. ) ;
#63897 = PLANE ( 'NONE',  #114947 ) ;
#63898 = FACE_OUTER_BOUND ( 'NONE', #24915, .T. ) ;
#63899 = CARTESIAN_POINT ( 'NONE',  ( 10.49999999999993250, 13.46639925780212366, 5.000000000000000000 ) ) ;
#63900 = DIRECTION ( 'NONE',  ( 0.7071067811865487940, 0.7071067811865463515, -0.000000000000000000 ) ) ;
#63901 = CARTESIAN_POINT ( 'NONE',  ( 2.999999999999975131, -16.02097659208071079, -11.96015758381209082 ) ) ;
#63902 = CARTESIAN_POINT ( 'NONE',  ( 126.2037635252314658, 6.109999999999998543, 1.122388791418548911E-15 ) ) ;
#63903 = ORIENTED_EDGE ( 'NONE', *, *, #10075, .F. ) ;
#63904 = FACE_OUTER_BOUND ( 'NONE', #125372, .T. ) ;
#63905 = ORIENTED_EDGE ( 'NONE', *, *, #55768, .T. ) ;
#63906 = FACE_OUTER_BOUND ( 'NONE', #94280, .T. ) ;
#63907 = DIRECTION ( 'NONE',  ( 1.000000000000000000, 0.000000000000000000, 0.000000000000000000 ) ) ;
#63908 = DIRECTION ( 'NONE',  ( 0.000000000000000000, -1.000000000000000000, 0.000000000000000000 ) ) ;
#63909 = CARTESIAN_POINT ( 'NONE',  ( 17.99999999999987210, 15.45873954670186734, -0.03131636524298340996 ) ) ;
#63910 = VERTEX_POINT ( 'NONE', #55811 ) ;
#63911 = CARTESIAN_POINT ( 'NONE',  ( 48.12543019189810423, 5.291415217122919401, 3.055000000000002824 ) ) ;
#63912 = ORIENTED_EDGE ( 'NONE', *, *, #100029, .F. ) ;
#63913 = CARTESIAN_POINT ( 'NONE',  ( -18.69326993309588403, -3.740707523384244837, 12.88036043432871836 ) ) ;
#63914 = CARTESIAN_POINT ( 'NONE',  ( 32.35681257248241849, -20.24070752338406720, 21.22881796311220270 ) ) ;
#63915 = DIRECTION ( 'NONE',  ( -0.6830127018922181881, 0.6830127018922202975, -0.2588190451025214056 ) ) ;
#63916 = VECTOR ( 'NONE', #5008, 1000.000000000000000 ) ;
#63917 = CARTESIAN_POINT ( 'NONE',  ( 40.89126352523144448, -4.472830434245839371, -4.472830434245839371 ) ) ;
#63918 = ORIENTED_EDGE ( 'NONE', *, *, #130762, .T. ) ;
#63919 = VECTOR ( 'NONE', #7163, 1000.000000000000000 ) ;
#63920 = CARTESIAN_POINT ( 'NONE',  ( 0.000000000000000000, -21.76999999999999247, -0.5000000000000000000 ) ) ;
#63921 = EDGE_LOOP ( 'NONE', ( #64878, #101212, #23979, #104177 ) ) ;
#63922 = VERTEX_POINT ( 'NONE', #132676 ) ;
#63923 = VERTEX_POINT ( 'NONE', #21735 ) ;
#63924 = ADVANCED_FACE ( 'NONE', ( #102163 ), #100012, .F. ) ;
#63925 = CARTESIAN_POINT ( 'NONE',  ( 23.32000000000000028, 9.521314400968980422E-16, 0.000000000000000000 ) ) ;
#63926 = DIRECTION ( 'NONE',  ( 0.7071067811865487940, 0.7071067811865463515, 0.000000000000000000 ) ) ;
#63927 = ORIENTED_EDGE ( 'NONE', *, *, #22321, .T. ) ;
#63928 = CARTESIAN_POINT ( 'NONE',  ( 29.29289321881325847, -3.740707523384241728, 5.000000000000000000 ) ) ;
#63929 = CIRCLE ( 'NONE', #50062, 5.999999999999998224 ) ;
#63930 = CARTESIAN_POINT ( 'NONE',  ( 17.99999999999987566, 16.55218569542899587, 5.000000000000000000 ) ) ;
#63931 = CARTESIAN_POINT ( 'NONE',  ( 48.48921356237309510, -27.52281430457089328, 5.000000000000000000 ) ) ;
#63932 = ADVANCED_FACE ( 'NONE', ( #113005 ), #11530, .T. ) ;
#63933 = FACE_BOUND ( 'NONE', #123471, .T. ) ;
#63934 = ORIENTED_EDGE ( 'NONE', *, *, #51160, .T. ) ;
#63935 = EDGE_CURVE ( 'NONE', #137150, #122980, #22412, .T. ) ;
#63936 = EDGE_CURVE ( 'NONE', #28467, #7925, #89143, .T. ) ;
#63937 = LINE ( 'NONE', #31308, #53774 ) ;
#63938 = CARTESIAN_POINT ( 'NONE',  ( -50.99451991528749062, 28.92564299267973738, 4.000000000000000000 ) ) ;
#63939 = ORIENTED_EDGE ( 'NONE', *, *, #42904, .F. ) ;
#63940 = ORIENTED_EDGE ( 'NONE', *, *, #76754, .F. ) ;
#63941 = ORIENTED_EDGE ( 'NONE', *, *, #99841, .F. ) ;
#63942 = DIRECTION ( 'NONE',  ( 0.000000000000000000, -1.000000000000000000, 0.000000000000000000 ) ) ;
#63943 = VECTOR ( 'NONE', #127001, 1000.000000000000227 ) ;
#63944 = VERTEX_POINT ( 'NONE', #121734 ) ;
#63945 = ADVANCED_FACE ( 'NONE', ( #133364 ), #100726, .F. ) ;
#63946 = EDGE_CURVE ( 'NONE', #21831, #121565, #97192, .T. ) ;
#63947 = VECTOR ( 'NONE', #9661, 1000.000000000000227 ) ;
#63948 = CARTESIAN_POINT ( 'NONE',  ( 56.64126352523144448, 4.472830434245835818, 4.472830434245840259 ) ) ;
#63949 = VERTEX_POINT ( 'NONE', #44966 ) ;
#63950 = DIRECTION ( 'NONE',  ( -0.000000000000000000, 0.000000000000000000, 1.000000000000000000 ) ) ;
#63951 = DIRECTION ( 'NONE',  ( 0.7071067811865487940, 0.7071067811865463515, 0.000000000000000000 ) ) ;
#63952 = EDGE_CURVE ( 'NONE', #139559, #86675, #12271, .T. ) ;
#63953 = VERTEX_POINT ( 'NONE', #55085 ) ;
#63954 = SURFACE_STYLE_USAGE ( .BOTH. , #19712 ) ;
#63955 = LINE ( 'NONE', #131343, #20372 ) ;
#63956 = AXIS2_PLACEMENT_3D ( 'NONE', #63867, #128401, #8011 ) ;
#63957 = EDGE_CURVE ( 'NONE', #114197, #108193, #99256, .T. ) ;
#63958 = CARTESIAN_POINT ( 'NONE',  ( 1.180000000000001270, -9.043340090917736163, 6.750000000000000888 ) ) ;
#63959 = CARTESIAN_POINT ( 'NONE',  ( -72.18398860626899705, 28.73617430169837661, 5.000000000000000000 ) ) ;
#63960 = CARTESIAN_POINT ( 'NONE',  ( 22.49999999999985434, 22.08746187583901843, 4.000000000000000000 ) ) ;
#63961 = CARTESIAN_POINT ( 'NONE',  ( -81.18398860626899705, 28.73617430169844056, 5.000000000000000000 ) ) ;
#63962 = DIRECTION ( 'NONE',  ( -0.000000000000000000, 0.000000000000000000, 1.000000000000000000 ) ) ;
#63963 = ORIENTED_EDGE ( 'NONE', *, *, #131077, .T. ) ;
#63964 = EDGE_CURVE ( 'NONE', #50789, #140166, #44220, .T. ) ;
#63965 = ORIENTED_EDGE ( 'NONE', *, *, #71408, .F. ) ;
#63966 = PLANE ( 'NONE',  #79143 ) ;
#63967 = EDGE_LOOP ( 'NONE', ( #71136, #80870, #82059, #35051 ) ) ;
#63968 = ORIENTED_EDGE ( 'NONE', *, *, #19393, .T. ) ;
#63969 = ORIENTED_EDGE ( 'NONE', *, *, #28694, .F. ) ;
#63970 = CARTESIAN_POINT ( 'NONE',  ( 5.010880286539447503, -22.02621442084248926, 4.990779571109220214 ) ) ;
#63971 = CARTESIAN_POINT ( 'NONE',  ( -2.999999999999975131, 9.631307414974321190, -9.079085613539549016 ) ) ;
#63972 = PLANE ( 'NONE',  #9111 ) ;
#63973 = EDGE_LOOP ( 'NONE', ( #30423, #460, #29367 ) ) ;
#63974 = DIRECTION ( 'NONE',  ( -0.000000000000000000, 1.000000000000000000, 1.091707662666338270E-16 ) ) ;
#63975 = ADVANCED_FACE ( 'NONE', ( #143500 ), #45658, .F. ) ;
#63976 = DIRECTION ( 'NONE',  ( 0.7071067811865487940, 0.7071067811865463515, 0.000000000000000000 ) ) ;
#63977 = CARTESIAN_POINT ( 'NONE',  ( 20.48373647476854842, -5.808823158059035485, -5.808823158059033709 ) ) ;
#63978 = ORIENTED_EDGE ( 'NONE', *, *, #97203, .F. ) ;
#63979 = CARTESIAN_POINT ( 'NONE',  ( 122.4120968585647802, 5.291415217122922066, -3.054999999999995275 ) ) ;
#63980 = CARTESIAN_POINT ( 'NONE',  ( -5.700255128608413102, -27.71228299555201957, 4.000000000000000000 ) ) ;
#63981 = EDGE_CURVE ( 'NONE', #99111, #79754, #101882, .T. ) ;
#63982 = DIRECTION ( 'NONE',  ( 0.6830127018922180770, -0.6830127018922204085, -0.2588190451025213501 ) ) ;
#63984 = VERTEX_POINT ( 'NONE', #134072 ) ;
#63983 = DIRECTION ( 'NONE',  ( 0.7071067811865487940, 0.7071067811865463515, 0.000000000000000000 ) ) ;
#63985 = VECTOR ( 'NONE', #53340, 1000.000000000000000 ) ;
#63986 = CARTESIAN_POINT ( 'NONE',  ( 67.30836038379622721, 7.949999999999996625, 2.130196079827431088 ) ) ;
#63987 = ORIENTED_EDGE ( 'NONE', *, *, #34863, .T. ) ;
#63988 = DIRECTION ( 'NONE',  ( 0.7071067811865486830, -0.7071067811865464625, -0.000000000000000000 ) ) ;
#63989 = DIRECTION ( 'NONE',  ( -1.000000000000000000, 0.000000000000000000, -0.000000000000000000 ) ) ;
#63990 = CARTESIAN_POINT ( 'NONE',  ( 43.00000000000000000, 0.000000000000000000, -7.950000000000000178 ) ) ;
#63991 = ORIENTED_EDGE ( 'NONE', *, *, #131385, .F. ) ;
#63992 = EDGE_CURVE ( 'NONE', #31310, #119557, #46385, .T. ) ;
#63993 = ADVANCED_FACE ( 'NONE', ( #110839 ), #123206, .F. ) ;
#63994 = DIRECTION ( 'NONE',  ( 0.7071067811865487940, 0.7071067811865463515, 0.000000000000000000 ) ) ;
#63995 = FACE_OUTER_BOUND ( 'NONE', #1781, .T. ) ;
#63996 = AXIS2_PLACEMENT_3D ( 'NONE', #38014, #51736, #39438 ) ;
#63997 = ORIENTED_EDGE ( 'NONE', *, *, #54093, .T. ) ;
#63998 = DIRECTION ( 'NONE',  ( -0.000000000000000000, -0.3543493200069152693, 0.9351131265310292928 ) ) ;
#63999 =( BOUNDED_CURVE ( )  B_SPLINE_CURVE ( 3, ( #122773, #101015, #132979, #90892 ),
 .UNSPECIFIED., .F., .T. ) 
 B_SPLINE_CURVE_WITH_KNOTS ( ( 4, 4 ),
 ( 1.864375635226923400, 1.933014472006560958 ),
 .UNSPECIFIED. ) 
 CURVE ( )  GEOMETRIC_REPRESENTATION_ITEM ( )  RATIONAL_B_SPLINE_CURVE ( ( 1.000000000000000000, 0.9996074310407762065, 0.9996074310407762065, 1.000000000000000000 ) ) 
 REPRESENTATION_ITEM ( '' )  );
#64001 = EDGE_CURVE ( 'NONE', #58035, #45698, #91974, .T. ) ;
#64000 = FACE_OUTER_BOUND ( 'NONE', #125416, .T. ) ;
#64002 = ORIENTED_EDGE ( 'NONE', *, *, #91353, .T. ) ;
#64003 = CARTESIAN_POINT ( 'NONE',  ( -34.42500000000001137, 8.977185695429334089, 5.000000000000000000 ) ) ;
#64004 = DIRECTION ( 'NONE',  ( -1.000000000000000000, 0.000000000000000000, 0.000000000000000000 ) ) ;
#64005 = ORIENTED_EDGE ( 'NONE', *, *, #71864, .F. ) ;
#64006 = ORIENTED_EDGE ( 'NONE', *, *, #20255, .T. ) ;
#64007 = DIRECTION ( 'NONE',  ( 1.248002500702736137E-15, 1.000000000000000000, 0.000000000000000000 ) ) ;
#64008 = CARTESIAN_POINT ( 'NONE',  ( -10.82816939922345156, 21.75929247661549937, 4.000000000000000000 ) ) ;
#64009 = EDGE_CURVE ( 'NONE', #136985, #98372, #108885, .T. ) ;
#64010 = CARTESIAN_POINT ( 'NONE',  ( 15.14540314143522082, -2.126176841940958351, -7.934999999999989839 ) ) ;
#64011 = VECTOR ( 'NONE', #133144, 1000.000000000000227 ) ;
#64012 = CARTESIAN_POINT ( 'NONE',  ( 184.1500000000000057, -43.14999999999999147, 31.92499999999998295 ) ) ;
#64013 = DIRECTION ( 'NONE',  ( -0.7071067811865486830, -0.7071067811865464625, -0.000000000000000000 ) ) ;
#64014 = LINE ( 'NONE', #29227, #9747 ) ;
#64015 = AXIS2_PLACEMENT_3D ( 'NONE', #96155, #142560, #76605 ) ;
#64016 = ORIENTED_EDGE ( 'NONE', *, *, #118453, .T. ) ;
#64017 = EDGE_CURVE ( 'NONE', #112008, #56955, #113733, .T. ) ;
#64018 = DIRECTION ( 'NONE',  ( 1.000000000000000000, 0.000000000000000000, 0.000000000000000000 ) ) ;
#64019 = DIRECTION ( 'NONE',  ( 0.6830127018922181881, 0.6830127018922202975, -0.2588190451025214056 ) ) ;
#64020 = CARTESIAN_POINT ( 'NONE',  ( 33.18398860626899705, 28.73617430169810305, 5.000000000000000000 ) ) ;
#64021 = LINE ( 'NONE', #53112, #18197 ) ;
#64022 = CARTESIAN_POINT ( 'NONE',  ( 41.91209685856478728, 5.291415217122922066, -3.054999999999995275 ) ) ;
#64023 = CARTESIAN_POINT ( 'NONE',  ( 32.29298673570672662, -21.74070752338405654, 4.999753212805222446 ) ) ;
#64024 = ORIENTED_EDGE ( 'NONE', *, *, #129111, .F. ) ;
#64025 = CARTESIAN_POINT ( 'NONE',  ( -30.32816939922331656, -15.74070752338412760, 4.000000000000000000 ) ) ;
#64026 = EDGE_LOOP ( 'NONE', ( #139510, #138511, #31746, #45888 ) ) ;
#64027 = VECTOR ( 'NONE', #24346, 1000.000000000000000 ) ;
#64028 = VERTEX_POINT ( 'NONE', #103543 ) ;
#64029 = LINE ( 'NONE', #108197, #31702 ) ;
#64030 = LINE ( 'NONE', #11028, #34760 ) ;
#64031 = ORIENTED_EDGE ( 'NONE', *, *, #73436, .T. ) ;
#64032 = CARTESIAN_POINT ( 'NONE',  ( 11.71247294953710671, 0.000000000000000000, 6.094999999999989981 ) ) ;
#64033 = CARTESIAN_POINT ( 'NONE',  ( -24.18398860626899705, 28.73617430169804265, 5.000000000000000000 ) ) ;
#64034 = DIRECTION ( 'NONE',  ( 0.000000000000000000, 1.000000000000000000, 0.000000000000000000 ) ) ;
#64035 = EDGE_CURVE ( 'NONE', #49314, #39393, #26017, .T. ) ;
#64036 = VECTOR ( 'NONE', #70711, 1000.000000000000000 ) ;
#64037 = CARTESIAN_POINT ( 'NONE',  ( 17.53719725875415847, 2.055000000000001048, 0.000000000000000000 ) ) ;
#64038 = CARTESIAN_POINT ( 'NONE',  ( -30.29974487139158867, -27.71228299555227537, 4.000000000000000000 ) ) ;
#64039 = ORIENTED_EDGE ( 'NONE', *, *, #50510, .T. ) ;
#64040 = DIRECTION ( 'NONE',  ( -0.000000000000000000, -0.3543493200069152693, 0.9351131265310292928 ) ) ;
#64041 = DIRECTION ( 'NONE',  ( 0.7071067811865487940, 0.7071067811865463515, 0.000000000000000000 ) ) ;
#64042 = LINE ( 'NONE', #140857, #107463 ) ;
#64043 = FACE_OUTER_BOUND ( 'NONE', #2919, .T. ) ;
#64044 = CARTESIAN_POINT ( 'NONE',  ( 29.27718569542920335, -21.72500000000000142, 5.000000000000000000 ) ) ;
#64045 = AXIS2_PLACEMENT_3D ( 'NONE', #62135, #138982, #128110 ) ;
#64046 = CIRCLE ( 'NONE', #8414, 4.749999999999997335 ) ;
#64047 = CARTESIAN_POINT ( 'NONE',  ( 52.87086038379622011, 6.884901960086289741, -3.974999999999993427 ) ) ;
#64048 = VECTOR ( 'NONE', #142879, 1000.000000000000000 ) ;
#64049 = FACE_OUTER_BOUND ( 'NONE', #7387, .T. ) ;
#64050 = ORIENTED_EDGE ( 'NONE', *, *, #45248, .T. ) ;
#64051 = ORIENTED_EDGE ( 'NONE', *, *, #43557, .F. ) ;
#64052 = CARTESIAN_POINT ( 'NONE',  ( 50.29166666666666430, 3.975000000000003642, -6.884901960086285300 ) ) ;
#64053 = DIRECTION ( 'NONE',  ( 0.7071067811865486830, -0.7071067811865464625, -0.000000000000000000 ) ) ;
#64054 = CARTESIAN_POINT ( 'NONE',  ( 6.183988606268994381, 28.73617430169791476, 5.000000000000000000 ) ) ;
#64056 = LINE ( 'NONE', #61934, #11319 ) ;
#64055 = VECTOR ( 'NONE', #51383, 1000.000000000000000 ) ;
#64057 = VERTEX_POINT ( 'NONE', #92673 ) ;
#64058 = DIRECTION ( 'NONE',  ( -0.000000000000000000, -0.000000000000000000, 1.000000000000000000 ) ) ;
#64059 = EDGE_CURVE ( 'NONE', #125931, #66092, #49216, .T. ) ;
#64060 = CARTESIAN_POINT ( 'NONE',  ( 51.47959685856477563, 6.109999999999999432, 1.637169565754164280 ) ) ;
#64061 = ORIENTED_EDGE ( 'NONE', *, *, #42924, .F. ) ;
#64062 = CARTESIAN_POINT ( 'NONE',  ( 34.49999999999975842, -10.53574439159940113, 4.994342998332163219 ) ) ;
#64063 = VERTEX_POINT ( 'NONE', #102872 ) ;
#64064 = EDGE_LOOP ( 'NONE', ( #63825, #99845, #16428, #51301 ) ) ;
#64065 = DIRECTION ( 'NONE',  ( 0.000000000000000000, -1.000000000000000000, 0.000000000000000000 ) ) ;
#64066 = CARTESIAN_POINT ( 'NONE',  ( 81.30836038379622721, 7.949999999999996625, 2.130196079827431088 ) ) ;
#64067 = DIRECTION ( 'NONE',  ( -0.7071067811865486830, -0.7071067811865464625, 0.000000000000000000 ) ) ;
#64068 = FILL_AREA_STYLE_COLOUR ( '', #30083 ) ;
#64069 = ORIENTED_EDGE ( 'NONE', *, *, #131227, .F. ) ;
#64070 = EDGE_CURVE ( 'NONE', #35249, #127932, #104987, .T. ) ;
#64071 = PLANE ( 'NONE',  #113703 ) ;
#64073 = ORIENTED_EDGE ( 'NONE', *, *, #65647, .F. ) ;
#64072 = LINE ( 'NONE', #32900, #119341 ) ;
#64074 = CARTESIAN_POINT ( 'NONE',  ( 87.06293019189809002, 1.637169565754157174, 6.110000000000002984 ) ) ;
#64075 = CARTESIAN_POINT ( 'NONE',  ( 14.58333333333333570, -5.278424836066144543, 3.047499999999995879 ) ) ;
#64076 = FACE_OUTER_BOUND ( 'NONE', #62304, .T. ) ;
#64077 = DIRECTION ( 'NONE',  ( -0.000000000000000000, -0.000000000000000000, 1.000000000000000000 ) ) ;
#64078 = VERTEX_POINT ( 'NONE', #27413 ) ;
#64079 = VECTOR ( 'NONE', #99991, 999.9999999999998863 ) ;
#64080 = FACE_OUTER_BOUND ( 'NONE', #82834, .T. ) ;
#64081 = CARTESIAN_POINT ( 'NONE',  ( 64.51626352523143737, -4.472830434245839371, 4.472830434245839371 ) ) ;
#64082 = FACE_OUTER_BOUND ( 'NONE', #44192, .T. ) ;
#64083 = LINE ( 'NONE', #51074, #87117 ) ;
#64084 = LINE ( 'NONE', #8234, #131183 ) ;
#64085 = ORIENTED_EDGE ( 'NONE', *, *, #17529, .F. ) ;
#64086 = ORIENTED_EDGE ( 'NONE', *, *, #60920, .T. ) ;
#64087 = AXIS2_PLACEMENT_3D ( 'NONE', #17509, #95065, #59630 ) ;
#64088 = CARTESIAN_POINT ( 'NONE',  ( -60.18398860626900415, 28.73617430169829490, 5.000000000000000000 ) ) ;
#64089 =( NAMED_UNIT ( * ) SI_UNIT ( $, .STERADIAN. ) SOLID_ANGLE_UNIT ( ) );
#64090 = VERTEX_POINT ( 'NONE', #115118 ) ;
#64091 = ORIENTED_EDGE ( 'NONE', *, *, #14885, .T. ) ;
#64092 = DIRECTION ( 'NONE',  ( -1.000000000000000000, -0.000000000000000000, -0.000000000000000000 ) ) ;
#64093 = EDGE_LOOP ( 'NONE', ( #26042, #132738, #3220 ) ) ;
#64094 = CARTESIAN_POINT ( 'NONE',  ( 174.7500000000000000, 7.919999999999947526, -18.97500000000001918 ) ) ;
#64095 = FACE_OUTER_BOUND ( 'NONE', #131322, .T. ) ;
#64096 = VECTOR ( 'NONE', #74192, 999.9999999999998863 ) ;
#64097 = CARTESIAN_POINT ( 'NONE',  ( -6.489213562373093325, -27.52281430457059841, 5.000000000000000000 ) ) ;
#64098 = VECTOR ( 'NONE', #77509, 1000.000000000000000 ) ;
#64099 = FACE_BOUND ( 'NONE', #52129, .T. ) ;
#64100 = CARTESIAN_POINT ( 'NONE',  ( 45.48921356237309510, -27.52281430457087197, 5.000000000000000000 ) ) ;
#64101 = EDGE_CURVE ( 'NONE', #31365, #53394, #25601, .T. ) ;
#64102 = LINE ( 'NONE', #97415, #123112 ) ;
#64103 = LINE ( 'NONE', #53970, #98886 ) ;
#64105 = VERTEX_POINT ( 'NONE', #61533 ) ;
#64104 = DIRECTION ( 'NONE',  ( -0.000000000000000000, -0.3543493200069152693, 0.9351131265310292928 ) ) ;
#64106 = DIRECTION ( 'NONE',  ( 0.3543493200069162685, -0.000000000000000000, -0.9351131265310288487 ) ) ;
#64107 = CONTEXT_DEPENDENT_SHAPE_REPRESENTATION ( #117041, #94391 ) ;
#64109 = VERTEX_POINT ( 'NONE', #49925 ) ;
#64108 = VECTOR ( 'NONE', #105301, 1000.000000000000114 ) ;
#64110 = EDGE_CURVE ( 'NONE', #13100, #29497, #15789, .T. ) ;
#64111 = EDGE_CURVE ( 'NONE', #42005, #14007, #81126, .T. ) ;
#64112 = ORIENTED_EDGE ( 'NONE', *, *, #101411, .F. ) ;
#64113 = CARTESIAN_POINT ( 'NONE',  ( 88.14126352523143737, 4.472830434245835818, 4.472830434245840259 ) ) ;
#64114 = ORIENTED_EDGE ( 'NONE', *, *, #138997, .T. ) ;
#64115 = CARTESIAN_POINT ( 'NONE',  ( -8.510786437626906675, -27.52281430457049183, 5.000000000000000000 ) ) ;
#64116 = ADVANCED_FACE ( 'NONE', ( #60084 ), #50619, .T. ) ;
#64117 = AXIS2_PLACEMENT_3D ( 'NONE', #44528, #24163, #66963 ) ;
#64118 = CARTESIAN_POINT ( 'NONE',  ( -28.49999999999979750, 3.431123077392151277, 4.000000000000000000 ) ) ;
#64119 = EDGE_CURVE ( 'NONE', #121969, #64882, #30267, .T. ) ;
#64120 = ORIENTED_EDGE ( 'NONE', *, *, #21636, .F. ) ;
#64121 = FACE_OUTER_BOUND ( 'NONE', #2384, .T. ) ;
#64122 = ADVANCED_FACE ( 'NONE', ( #58703 ), #39026, .T. ) ;
#64123 = DIRECTION ( 'NONE',  ( 1.000000000000000000, 0.000000000000000000, 0.000000000000000000 ) ) ;
#64124 = PLANE ( 'NONE',  #48387 ) ;
#64125 = EDGE_CURVE ( 'NONE', #70281, #94584, #105680, .T. ) ;
#64126 = LINE ( 'NONE', #10432, #87180 ) ;
#64127 = DIRECTION ( 'NONE',  ( 0.7071067811865486830, -0.7071067811865464625, -0.000000000000000000 ) ) ;
#64128 = FACE_OUTER_BOUND ( 'NONE', #8781, .T. ) ;
#64129 = DIRECTION ( 'NONE',  ( -0.7071067811865486830, -0.7071067811865464625, 0.000000000000000000 ) ) ;
#64130 = CARTESIAN_POINT ( 'NONE',  ( 13.49999999999990763, -11.94781430457070748, 5.000000000000000000 ) ) ;
#64131 = ORIENTED_EDGE ( 'NONE', *, *, #41550, .F. ) ;
#64132 =( NAMED_UNIT ( * ) SI_UNIT ( $, .STERADIAN. ) SOLID_ANGLE_UNIT ( ) );
#64133 = ORIENTED_EDGE ( 'NONE', *, *, #88385, .T. ) ;
#64134 = CARTESIAN_POINT ( 'NONE',  ( 21.32816939922336985, -6.740707523384216415, 4.000000000000000000 ) ) ;
#64135 = DIRECTION ( 'NONE',  ( -0.6830127018922181881, 0.6830127018922202975, -0.2588190451025214056 ) ) ;
#64136 = EDGE_CURVE ( 'NONE', #37795, #141564, #4919, .T. ) ;
#64137 = EDGE_LOOP ( 'NONE', ( #33872, #127779, #54126, #139516 ) ) ;
#64139 = ORIENTED_EDGE ( 'NONE', *, *, #94042, .T. ) ;
#64138 = AXIS2_PLACEMENT_3D ( 'NONE', #100291, #122007, #66943 ) ;
#64140 = PLANE ( 'NONE',  #126243 ) ;
#64141 = ORIENTED_EDGE ( 'NONE', *, *, #75018, .F. ) ;
#64142 = CARTESIAN_POINT ( 'NONE',  ( 33.10459685856476852, 1.637169565754164946, -6.109999999999999432 ) ) ;
#64143 = ORIENTED_EDGE ( 'NONE', *, *, #106454, .F. ) ;
#64144 = LINE ( 'NONE', #106912, #110707 ) ;
#64145 = EDGE_CURVE ( 'NONE', #37768, #8478, #115833, .T. ) ;
#64146 = VECTOR ( 'NONE', #12553, 1000.000000000000227 ) ;
#64148 = VECTOR ( 'NONE', #134305, 1000.000000000000227 ) ;
#64147 = VECTOR ( 'NONE', #63055, 1000.000000000000000 ) ;
#64149 = COLOUR_RGB ( '', 0.09019608, 0.27058824, 0.51372549) ;
#64150 = CARTESIAN_POINT ( 'NONE',  ( 21.92080628287044064, 3.047499999999997655, 5.278424836066143655 ) ) ;
#64151 = CARTESIAN_POINT ( 'NONE',  ( 0.9490416316764018756, 12.57141199504220808, -25.28239494629447037 ) ) ;
#64152 = EDGE_LOOP ( 'NONE', ( #50970, #74703, #18362, #16109 ) ) ;
#64153 = DIRECTION ( 'NONE',  ( 1.000000000000000000, -0.000000000000000000, -0.000000000000000000 ) ) ;
#64154 = AXIS2_PLACEMENT_3D ( 'NONE', #31088, #107879, #52793 ) ;
#64155 = ORIENTED_EDGE ( 'NONE', *, *, #91294, .T. ) ;
#64156 = LINE ( 'NONE', #122804, #136746 ) ;
#64157 = VECTOR ( 'NONE', #117000, 1000.000000000000000 ) ;
#64158 = PLANE ( 'NONE',  #75339 ) ;
#64160 = EDGE_LOOP ( 'NONE', ( #63056, #21230, #27147, #103465 ) ) ;
#64159 = LINE ( 'NONE', #32983, #3070 ) ;
#64161 = EDGE_LOOP ( 'NONE', ( #4063, #112246, #12337, #114326 ) ) ;
#64162 = CARTESIAN_POINT ( 'NONE',  ( 12.32816939922343913, -9.740707523384184441, 4.000000000000000000 ) ) ;
#64163 = CARTESIAN_POINT ( 'NONE',  ( 33.79333936457825160, 21.75929247661550647, 4.998822639870711626 ) ) ;
#64164 = ORIENTED_EDGE ( 'NONE', *, *, #132612, .F. ) ;
#64165 = CARTESIAN_POINT ( 'NONE',  ( 110.0375270504628986, -9.735942053221456900E-16, 7.949999999999998401 ) ) ;
#64166 = VERTEX_POINT ( 'NONE', #127457 ) ;
#64167 = ORIENTED_EDGE ( 'NONE', *, *, #136235, .F. ) ;
#64168 = ORIENTED_EDGE ( 'NONE', *, *, #69363, .T. ) ;
#64169 = ADVANCED_FACE ( 'NONE', ( #28157 ), #39769, .F. ) ;
#64170 = CARTESIAN_POINT ( 'NONE',  ( 1.499999999999987566, -17.91344420646042579, 1.358650452708467737 ) ) ;
#64171 = CARTESIAN_POINT ( 'NONE',  ( -36.48921356237310221, -27.52281430457080802, 5.000000000000000000 ) ) ;
#64172 = CARTESIAN_POINT ( 'NONE',  ( -12.70000000000000462, -22.26999999999999247, -39.50000000000000000 ) ) ;
#64173 = ADVANCED_FACE ( 'NONE', ( #108521 ), #86107, .F. ) ;
#64174 = DIRECTION ( 'NONE',  ( 1.000000000000000000, 0.000000000000000000, 0.000000000000000000 ) ) ;
#64175 = DIRECTION ( 'NONE',  ( 0.7071067811865487940, 0.7071067811865463515, -0.000000000000000000 ) ) ;
#64176 = DIRECTION ( 'NONE',  ( -1.000000000000000000, -0.000000000000000000, -0.000000000000000000 ) ) ;
#64177 = ORIENTED_EDGE ( 'NONE', *, *, #55093, .F. ) ;
#64178 = CARTESIAN_POINT ( 'NONE',  ( 96.03752705046289861, -9.735942053221456900E-16, 7.949999999999998401 ) ) ;
#64179 = ORIENTED_EDGE ( 'NONE', *, *, #343, .F. ) ;
#64180 = AXIS2_PLACEMENT_3D ( 'NONE', #134591, #81643, #125108 ) ;
#64181 = CARTESIAN_POINT ( 'NONE',  ( -34.47516574401890921, -19.50948238788419076, 4.998110765256836174 ) ) ;
#64183 = ADVANCED_FACE ( 'NONE', ( #117969 ), #128880, .T. ) ;
#64182 =( BOUNDED_CURVE ( )  B_SPLINE_CURVE ( 3, ( #91544, #124876, #12531, #35039 ),
 .UNSPECIFIED., .F., .T. ) 
 B_SPLINE_CURVE_WITH_KNOTS ( ( 4, 4 ),
 ( 5.106027341939272546, 6.645403452391245303 ),
 .UNSPECIFIED. ) 
 CURVE ( )  GEOMETRIC_REPRESENTATION_ITEM ( )  RATIONAL_B_SPLINE_CURVE ( ( 1.000000000000000000, 0.8120851936182260644, 0.8120851936182260644, 1.000000000000000000 ) ) 
 REPRESENTATION_ITEM ( '' )  );
#64184 = DIRECTION ( 'NONE',  ( 1.000000000000000000, -0.000000000000000000, -0.000000000000000000 ) ) ;
#64185 = VERTEX_POINT ( 'NONE', #75252 ) ;
#64186 = DIRECTION ( 'NONE',  ( 0.000000000000000000, -1.000000000000000000, 0.000000000000000000 ) ) ;
#64187 = CARTESIAN_POINT ( 'NONE',  ( 10.82816939922345512, -2.240707523384264377, 4.000000000000000000 ) ) ;
#64188 = VERTEX_POINT ( 'NONE', #62949 ) ;
#64189 = ORIENTED_EDGE ( 'NONE', *, *, #85641, .F. ) ;
#64190 = ADVANCED_FACE ( 'NONE', ( #107123 ), #74268, .T. ) ;
#64191 = CARTESIAN_POINT ( 'NONE',  ( -13.75179860200718984, 5.925774409307371648, 4.669108085256721274 ) ) ;
#64192 = CARTESIAN_POINT ( 'NONE',  ( 0.000000000000000000, 0.000000000000000000, 5.000000000000000000 ) ) ;
#64193 = AXIS2_PLACEMENT_3D ( 'NONE', #41069, #10557, #96835 ) ;
#64194 = DIRECTION ( 'NONE',  ( 0.000000000000000000, -1.000000000000000000, 0.000000000000000000 ) ) ;
#64195 = CARTESIAN_POINT ( 'NONE',  ( 22.96641869250914070, 7.680402717527123890, 4.333886692633072357 ) ) ;
#64196 = CARTESIAN_POINT ( 'NONE',  ( 64.95376352523145158, -6.109999999999999432, -3.741295971395163529E-16 ) ) ;
#64197 = CARTESIAN_POINT ( 'NONE',  ( -24.79289321881327623, 18.75929247661552068, 5.000000000000000000 ) ) ;
#64198 = DIRECTION ( 'NONE',  ( 0.7071067811865486830, -0.7071067811865464625, -0.000000000000000000 ) ) ;
#64199 = CARTESIAN_POINT ( 'NONE',  ( -7.122370700763609008, -39.92999999999999261, 19.06900128115122328 ) ) ;
#64200 = DIRECTION ( 'NONE',  ( -1.000000000000000000, -1.224606353822377258E-16, -0.000000000000000000 ) ) ;
#64201 = EDGE_LOOP ( 'NONE', ( #23484, #114058, #98503, #13066 ) ) ;
#64202 = CARTESIAN_POINT ( 'NONE',  ( 0.000000000000000000, 0.000000000000000000, 5.000000000000000000 ) ) ;
#64203 = AXIS2_PLACEMENT_3D ( 'NONE', #111460, #33241, #77448 ) ;
#64204 = VERTEX_POINT ( 'NONE', #52052 ) ;
#64205 = DIRECTION ( 'NONE',  ( 0.7071067811865487940, -0.7071067811865463515, 0.000000000000000000 ) ) ;
#64206 = LINE ( 'NONE', #85216, #19851 ) ;
#64207 = ORIENTED_EDGE ( 'NONE', *, *, #113401, .F. ) ;
#64208 = LINE ( 'NONE', #9046, #83196 ) ;
#64210 = ORIENTED_EDGE ( 'NONE', *, *, #82180, .T. ) ;
#64209 = CARTESIAN_POINT ( 'NONE',  ( 16.49999999999989342, 13.46639925780212010, 5.000000000000000000 ) ) ;
#64211 = LINE ( 'NONE', #105012, #50831 ) ;
#64212 = AXIS2_PLACEMENT_3D ( 'NONE', #33985, #102814, #69482 ) ;
#64213 = EDGE_CURVE ( 'NONE', #13173, #53146, #140469, .T. ) ;
#64214 = CARTESIAN_POINT ( 'NONE',  ( 34.92499999999998295, -21.28150956279551664, 4.759050581649326261 ) ) ;
#64215 = LINE ( 'NONE', #87396, #12510 ) ;
#64216 = ORIENTED_EDGE ( 'NONE', *, *, #114038, .F. ) ;
#64217 = ORIENTED_EDGE ( 'NONE', *, *, #1571, .F. ) ;
#64218 = DIRECTION ( 'NONE',  ( -0.6830127018922180770, -0.6830127018922204085, -0.2588190451025213501 ) ) ;
#64219 = PLANE ( 'NONE',  #23644 ) ;
#64220 = DIRECTION ( 'NONE',  ( -0.000000000000000000, -0.3543493200069152693, 0.9351131265310292928 ) ) ;
#64221 = CARTESIAN_POINT ( 'NONE',  ( 80.28752705046289861, 0.000000000000000000, -7.949999999999998401 ) ) ;
#64222 = DIRECTION ( 'NONE',  ( 0.7071067811865486830, -0.7071067811865464625, -0.000000000000000000 ) ) ;
#64223 = CARTESIAN_POINT ( 'NONE',  ( 15.08314806772921557, 21.75929247661549937, 7.311836541448085036 ) ) ;
#64224 = ORIENTED_EDGE ( 'NONE', *, *, #19102, .F. ) ;
#64225 = CARTESIAN_POINT ( 'NONE',  ( 8.500000000000000000, 2.055000000000001492, 2.516649172247811554E-16 ) ) ;
#64226 = CARTESIAN_POINT ( 'NONE',  ( -34.92500000000001137, 22.22500000000000142, 4.500000000000000888 ) ) ;
#64227 = CARTESIAN_POINT ( 'NONE',  ( 29.45833333333333570, -3.047499999999997211, -5.278424836066143655 ) ) ;
#64228 = ORIENTED_EDGE ( 'NONE', *, *, #39936, .F. ) ;
#64229 = CARTESIAN_POINT ( 'NONE',  ( -25.39999999999996305, 0.000000000000000000, 0.000000000000000000 ) ) ;
#64230 = ORIENTED_EDGE ( 'NONE', *, *, #34657, .F. ) ;
#64231 = VECTOR ( 'NONE', #109852, 1000.000000000000000 ) ;
#64232 = EDGE_CURVE ( 'NONE', #119557, #96580, #7064, .T. ) ;
#64233 = CARTESIAN_POINT ( 'NONE',  ( 73.79209685856477563, -5.291415217122921177, 3.054999999999999272 ) ) ;
#64234 = DIRECTION ( 'NONE',  ( -0.6830127018922180770, -0.6830127018922204085, -0.2588190451025214056 ) ) ;
#64235 = CARTESIAN_POINT ( 'NONE',  ( 17.54840764549667398, 9.139736423841732040E-16, 0.000000000000000000 ) ) ;
#64236 = ORIENTED_EDGE ( 'NONE', *, *, #15073, .T. ) ;
#64237 = DIRECTION ( 'NONE',  ( 0.7071067811865487940, -0.7071067811865463515, 0.000000000000000000 ) ) ;
#64238 = CARTESIAN_POINT ( 'NONE',  ( -26.99451991528749417, 28.92564299267956685, 4.000000000000000000 ) ) ;
#64239 = VECTOR ( 'NONE', #70729, 1000.000000000000000 ) ;
#64240 = CARTESIAN_POINT ( 'NONE',  ( -30.32816939922331301, 8.259292476615636147, 4.000000000000000000 ) ) ;
#64241 = EDGE_CURVE ( 'NONE', #63949, #17180, #51345, .T. ) ;
#64242 = LINE ( 'NONE', #98302, #62513 ) ;
#64244 = ORIENTED_EDGE ( 'NONE', *, *, #24543, .F. ) ;
#64243 = CARTESIAN_POINT ( 'NONE',  ( 34.47516574401891631, -2.971932658884160361, 4.998110765256834398 ) ) ;
#64245 = PLANE ( 'NONE',  #138678 ) ;
#64246 = CARTESIAN_POINT ( 'NONE',  ( 21.46453280170069888, 4.202752102959690472E-16, 0.000000000000000000 ) ) ;
#64247 = CARTESIAN_POINT ( 'NONE',  ( 23.42830866441052962, 7.233000843196646379, 4.333645886165172101 ) ) ;
#64248 = VECTOR ( 'NONE', #57197, 1000.000000000000000 ) ;
#64249 = CARTESIAN_POINT ( 'NONE',  ( 2.999999999999995559, -16.44781430457066662, 5.000000000000000000 ) ) ;
#64250 = VECTOR ( 'NONE', #76422, 1000.000000000000227 ) ;
#64251 = ORIENTED_EDGE ( 'NONE', *, *, #50171, .F. ) ;
#64252 = EDGE_LOOP ( 'NONE', ( #69665, #2963, #112195, #127056 ) ) ;
#64253 = VECTOR ( 'NONE', #23958, 999.9999999999998863 ) ;
#64254 = CARTESIAN_POINT ( 'NONE',  ( 68.68793019189809002, 6.110000000000002984, -1.637169565754156730 ) ) ;
#64255 = ORIENTED_EDGE ( 'NONE', *, *, #5017, .F. ) ;
#64256 = DIRECTION ( 'NONE',  ( 0.7071067811865487940, 0.7071067811865463515, 0.000000000000000000 ) ) ;
#64257 = DIRECTION ( 'NONE',  ( 0.000000000000000000, -1.000000000000000000, 0.000000000000000000 ) ) ;
#64259 = AXIS2_PLACEMENT_3D ( 'NONE', #56458, #100633, #78170 ) ;
#64258 = DIRECTION ( 'NONE',  ( 1.000000000000000000, 1.224606353822377258E-16, 0.000000000000000000 ) ) ;
#64260 = DIRECTION ( 'NONE',  ( 0.000000000000000000, 0.000000000000000000, 1.000000000000000000 ) ) ;
#64261 = ORIENTED_EDGE ( 'NONE', *, *, #40253, .F. ) ;
#64262 = DIRECTION ( 'NONE',  ( -0.7071067811865487940, 0.7071067811865463515, -0.000000000000000000 ) ) ;
#64263 = LINE ( 'NONE', #30933, #14334 ) ;
#64264 = EDGE_LOOP ( 'NONE', ( #59016, #106978, #47874, #9977 ) ) ;
#64265 = CARTESIAN_POINT ( 'NONE',  ( 24.18398860626899705, 28.73617430169804265, 5.000000000000000000 ) ) ;
#64266 = EDGE_CURVE ( 'NONE', #18293, #44324, #96932, .T. ) ;
#64267 = CARTESIAN_POINT ( 'NONE',  ( 13.49999999999991473, 13.46639925780212366, 5.000000000000000000 ) ) ;
#64268 = CARTESIAN_POINT ( 'NONE',  ( -13.11547925347946908, 3.815643823912585386, 4.000000000000000000 ) ) ;
#64269 = ORIENTED_EDGE ( 'NONE', *, *, #34872, .F. ) ;
#64270 = ORIENTED_EDGE ( 'NONE', *, *, #55411, .F. ) ;
#64271 = FACE_BOUND ( 'NONE', #102829, .T. ) ;
#64272 = LINE ( 'NONE', #9118, #119539 ) ;
#64273 = CARTESIAN_POINT ( 'NONE',  ( 128.7427689125804591, -1.701477371937628824, -6.349999999999999645 ) ) ;
#64274 = FACE_OUTER_BOUND ( 'NONE', #39187, .T. ) ;
#64275 = VECTOR ( 'NONE', #1694, 1000.000000000000000 ) ;
#64276 = PLANE ( 'NONE',  #11001 ) ;
#64277 = PLANE ( 'NONE',  #69795 ) ;
#64278 = VERTEX_POINT ( 'NONE', #19410 ) ;
#64279 = EDGE_CURVE ( 'NONE', #96885, #114780, #130335, .T. ) ;
#64280 = AXIS2_PLACEMENT_3D ( 'NONE', #62229, #41896, #106383 ) ;
#64281 = ORIENTED_EDGE ( 'NONE', *, *, #89951, .F. ) ;
#64282 = CARTESIAN_POINT ( 'NONE',  ( 116.4329301918981088, 1.637169565754156508, 6.110000000000000320 ) ) ;
#64283 = VERTEX_POINT ( 'NONE', #75941 ) ;
#64284 = EDGE_CURVE ( 'NONE', #29435, #96265, #63664, .T. ) ;
#64285 = ADVANCED_FACE ( 'NONE', ( #9198 ), #73110, .F. ) ;
#64286 = EDGE_LOOP ( 'NONE', ( #59571, #33268, #23955, #102381 ) ) ;
#64287 = EDGE_CURVE ( 'NONE', #26316, #113825, #83995, .T. ) ;
#64288 = CARTESIAN_POINT ( 'NONE',  ( -15.98911971346040062, -22.02621442084248571, 4.990779571109219326 ) ) ;
#64289 = ADVANCED_FACE ( 'NONE', ( #42627 ), #115810, .T. ) ;
#64290 = CARTESIAN_POINT ( 'NONE',  ( 15.52400138585438683, 22.03583458319438648, 4.979811245910089390 ) ) ;
#64291 = CARTESIAN_POINT ( 'NONE',  ( 0.000000000000000000, 0.000000000000000000, 5.000000000000000000 ) ) ;
#64292 = VERTEX_POINT ( 'NONE', #119411 ) ;
#64293 = CARTESIAN_POINT ( 'NONE',  ( -28.49999999999981171, 22.22500000000000853, 4.362957392718823435 ) ) ;
#64294 = CARTESIAN_POINT ( 'NONE',  ( -2.999999999999978240, 20.96639925780204550, 5.000000000000000000 ) ) ;
#64295 = ADVANCED_FACE ( 'NONE', ( #54917 ), #67964, .F. ) ;
#64296 = CARTESIAN_POINT ( 'NONE',  ( 16.61159235450331906, -2.500000000000000444, 3.061616997868384620E-16 ) ) ;
#64297 = DIRECTION ( 'NONE',  ( -0.6830127018922181881, 0.6830127018922202975, -0.2588190451025214056 ) ) ;
#64298 = DIRECTION ( 'NONE',  ( 0.7071067811865486830, -0.7071067811865464625, -0.000000000000000000 ) ) ;
#64299 = ORIENTED_EDGE ( 'NONE', *, *, #140716, .F. ) ;
#64300 = CARTESIAN_POINT ( 'NONE',  ( 4.171830600776446296, 21.75929247661550292, 4.000000000000000000 ) ) ;
#64301 = CARTESIAN_POINT ( 'NONE',  ( -5.999999999999967137, 4.931123077392134846, 4.000000000000000000 ) ) ;
#64302 = ADVANCED_FACE ( 'NONE', ( #88978 ), #55626, .F. ) ;
#64304 = ORIENTED_EDGE ( 'NONE', *, *, #95469, .T. ) ;
#64303 = AXIS2_PLACEMENT_3D ( 'NONE', #107771, #108459, #88929 ) ;
#64305 = LINE ( 'NONE', #97629, #27367 ) ;
#64306 = ORIENTED_EDGE ( 'NONE', *, *, #53646, .F. ) ;
#64307 = ORIENTED_EDGE ( 'NONE', *, *, #7084, .T. ) ;
#64308 = EDGE_CURVE ( 'NONE', #10128, #2613, #92089, .T. ) ;
#64309 = ORIENTED_EDGE ( 'NONE', *, *, #8897, .F. ) ;
#64310 = CARTESIAN_POINT ( 'NONE',  ( 67.95876352523144703, 0.000000000000000000, -6.110000000000001208 ) ) ;
#64311 = ORIENTED_EDGE ( 'NONE', *, *, #135802, .T. ) ;
#64312 = ORIENTED_EDGE ( 'NONE', *, *, #22962, .F. ) ;
#64313 = ADVANCED_FACE ( 'NONE', ( #111405 ), #78805, .F. ) ;
#64314 = LINE ( 'NONE', #54186, #115957 ) ;
#64315 = AXIS2_PLACEMENT_3D ( 'NONE', #26499, #37379, #17728 ) ;
#64316 = CARTESIAN_POINT ( 'NONE',  ( 99.02126352523143282, -4.472830434245838482, -4.472830434245840259 ) ) ;
#64317 = DIRECTION ( 'NONE',  ( -0.3543493200069162685, -0.000000000000000000, -0.9351131265310288487 ) ) ;
#64318 = DIRECTION ( 'NONE',  ( 1.000000000000000000, 0.000000000000000000, 0.000000000000000000 ) ) ;
#64319 = VERTEX_POINT ( 'NONE', #76681 ) ;
#64320 = DIRECTION ( 'NONE',  ( -0.000000000000000000, 0.3543493200069153248, 0.9351131265310292928 ) ) ;
#64321 = ADVANCED_FACE ( 'NONE', ( #112839 ), #88253, .F. ) ;
#64322 = CARTESIAN_POINT ( 'NONE',  ( -4.171830600776443632, 6.759292476615649470, 4.000000000000000000 ) ) ;
#64323 = CARTESIAN_POINT ( 'NONE',  ( 91.56249999999998579, -5.819803920172573086, -5.819803920172573974 ) ) ;
#64324 = CARTESIAN_POINT ( 'NONE',  ( -6.349999999999999645, 0.000000000000000000, 0.000000000000000000 ) ) ;
#64325 = ORIENTED_EDGE ( 'NONE', *, *, #135623, .T. ) ;
#64326 = AXIS2_PLACEMENT_3D ( 'NONE', #69790, #68365, #91515 ) ;
#64327 = CARTESIAN_POINT ( 'NONE',  ( 109.5000000000000000, 0.000000000000000000, -7.950000000000000178 ) ) ;
#64328 = ORIENTED_EDGE ( 'NONE', *, *, #94999, .F. ) ;
#64329 = VERTEX_POINT ( 'NONE', #1204 ) ;
#64330 = EDGE_LOOP ( 'NONE', ( #105370, #107759, #125618, #75881 ) ) ;
#64331 = ADVANCED_FACE ( 'NONE', ( #22239, #133891, #11350 ), #56375, .F. ) ;
#64332 = CARTESIAN_POINT ( 'NONE',  ( 119.6412635252314516, 4.472830434245835818, 4.472830434245840259 ) ) ;
#64333 = ORIENTED_EDGE ( 'NONE', *, *, #46004, .F. ) ;
#64334 = VECTOR ( 'NONE', #49013, 1000.000000000000000 ) ;
#64335 = DIRECTION ( 'NONE',  ( -0.7071067811865487940, 0.7071067811865463515, -0.000000000000000000 ) ) ;
#64336 = PLANE ( 'NONE',  #108118 ) ;
#64337 = CIRCLE ( 'NONE', #8707, 4.750000000000000000 ) ;
#64338 = CARTESIAN_POINT ( 'NONE',  ( 25.17183060077629619, -8.240707523384198652, 4.000000000000000000 ) ) ;
#64339 = ORIENTED_EDGE ( 'NONE', *, *, #94822, .T. ) ;
#64340 = ORIENTED_EDGE ( 'NONE', *, *, #3303, .T. ) ;
#64341 = VECTOR ( 'NONE', #80729, 1000.000000000000000 ) ;
#64342 = VECTOR ( 'NONE', #95837, 1000.000000000000000 ) ;
#64343 = EDGE_CURVE ( 'NONE', #98816, #50789, #78094, .T. ) ;
#64344 = CARTESIAN_POINT ( 'NONE',  ( 4.062069808101884227, -7.934999999999991616, -2.126176841940955242 ) ) ;
#64345 = FACE_OUTER_BOUND ( 'NONE', #130695, .T. ) ;
#64346 = CARTESIAN_POINT ( 'NONE',  ( 37.89583333333332149, -2.130196079827351596, 7.950000000000043698 ) ) ;
#64347 = ORIENTED_EDGE ( 'NONE', *, *, #132035, .T. ) ;
#64348 = VERTEX_POINT ( 'NONE', #23697 ) ;
#64349 = EDGE_CURVE ( 'NONE', #143112, #13174, #66505, .T. ) ;
#64350 = VERTEX_POINT ( 'NONE', #12802 ) ;
#64351 = CARTESIAN_POINT ( 'NONE',  ( 0.000000000000000000, 4.999999999999997335, -7.627214432543508948 ) ) ;
#64352 = SURFACE_SIDE_STYLE ('',( #53477 ) ) ;
#64353 = CARTESIAN_POINT ( 'NONE',  ( 26.99451991528749417, 28.92564299267956685, 4.000000000000000000 ) ) ;
#64354 = FACE_OUTER_BOUND ( 'NONE', #17655, .T. ) ;
#64355 = DIRECTION ( 'NONE',  ( 1.000000000000000000, 0.000000000000000000, 0.000000000000000000 ) ) ;
#64356 = DIRECTION ( 'NONE',  ( -0.7071067811865486830, -0.7071067811865464625, 0.000000000000000000 ) ) ;
#64357 = CARTESIAN_POINT ( 'NONE',  ( 33.97959685856477563, 6.109999999999999432, 1.637169565754164280 ) ) ;
#64358 = EDGE_CURVE ( 'NONE', #332, #101734, #99086, .T. ) ;
#64359 = DIRECTION ( 'NONE',  ( 0.3543493200069163240, -0.000000000000000000, -0.9351131265310288487 ) ) ;
#64360 = CARTESIAN_POINT ( 'NONE',  ( 14.70025512860841133, -27.71228299555195917, 4.000000000000000000 ) ) ;
#64361 = VERTEX_POINT ( 'NONE', #134626 ) ;
#64362 = PLANE ( 'NONE',  #92784 ) ;
#64363 = VERTEX_POINT ( 'NONE', #132504 ) ;
#64364 = CARTESIAN_POINT ( 'NONE',  ( 1.199999999999999956, 0.000000000000000000, 0.000000000000000000 ) ) ;
#64365 = VERTEX_POINT ( 'NONE', #33189 ) ;
#64366 = VECTOR ( 'NONE', #100178, 1000.000000000000000 ) ;
#64367 = DIRECTION ( 'NONE',  ( -0.7071067811865486830, -0.7071067811865464625, 0.000000000000000000 ) ) ;
#64369 = EDGE_LOOP ( 'NONE', ( #8527, #37867, #109069, #142712 ) ) ;
#64368 = PLANE ( 'NONE',  #51091 ) ;
#64370 = ADVANCED_FACE ( 'NONE', ( #77403 ), #48303, .F. ) ;
#64371 = CARTESIAN_POINT ( 'NONE',  ( 17.54840764549667398, 2.500000000000003553, 3.061616997868386099E-16 ) ) ;
#64372 = ORIENTED_EDGE ( 'NONE', *, *, #85086, .F. ) ;
#64373 = CARTESIAN_POINT ( 'NONE',  ( 18.79653912142945060, 3.821174125832445049E-16, 0.000000000000000000 ) ) ;
#64374 = ORIENTED_EDGE ( 'NONE', *, *, #10890, .F. ) ;
#64375 = CARTESIAN_POINT ( 'NONE',  ( -53.99451991528749062, 28.92564299267975869, 4.000000000000000000 ) ) ;
#64376 = ORIENTED_EDGE ( 'NONE', *, *, #74463, .F. ) ;
#64377 = CARTESIAN_POINT ( 'NONE',  ( -15.48921356237309510, -27.52281430457066236, 5.000000000000000000 ) ) ;
#64378 = CARTESIAN_POINT ( 'NONE',  ( 112.6625270504628986, 7.949999999999998401, 1.460391307983218338E-15 ) ) ;
#64379 = FACE_OUTER_BOUND ( 'NONE', #71055, .T. ) ;
#64380 = DIRECTION ( 'NONE',  ( -0.7071067811865487940, 0.7071067811865463515, 0.000000000000000000 ) ) ;
#64381 = FACE_OUTER_BOUND ( 'NONE', #140195, .T. ) ;
#64382 = DIRECTION ( 'NONE',  ( 0.000000000000000000, -1.000000000000000000, 0.000000000000000000 ) ) ;
#64383 = PLANE ( 'NONE',  #39232 ) ;
#64384 = CARTESIAN_POINT ( 'NONE',  ( 0.7291666666666667407, -6.094999999999989093, 1.633150327867691765 ) ) ;
#64385 = CARTESIAN_POINT ( 'NONE',  ( 13.24956980810188689, 3.967499999999998916, 6.871911579029510442 ) ) ;
#64386 = DIRECTION ( 'NONE',  ( -0.7071067811865486830, -0.7071067811865464625, 0.000000000000000000 ) ) ;
#64387 = FACE_OUTER_BOUND ( 'NONE', #41156, .T. ) ;
#64388 = ORIENTED_EDGE ( 'NONE', *, *, #117008, .F. ) ;
#64389 = SHAPE_REPRESENTATION ( 'slotted set screw dog point_iso_ISO 7435 - M5 x 25-S', ( #127880 ), #97842 ) ;
#64390 = ORIENTED_EDGE ( 'NONE', *, *, #120189, .T. ) ;
#64391 = LINE ( 'NONE', #45529, #58268 ) ;
#64392 = ORIENTED_EDGE ( 'NONE', *, *, #4938, .T. ) ;
#64393 = EDGE_CURVE ( 'NONE', #81745, #35625, #122784, .T. ) ;
#64394 = CARTESIAN_POINT ( 'NONE',  ( 92.53752705046289861, -9.735942053221456900E-16, 7.949999999999998401 ) ) ;
#64395 = CARTESIAN_POINT ( 'NONE',  ( 29.99999999999978328, -13.39766691384881092, -10.96608748226472763 ) ) ;
#64396 = CARTESIAN_POINT ( 'NONE',  ( 129.9042113015468942, -47.96374157527412763, -37.32649486623387958 ) ) ;
#64397 = VERTEX_POINT ( 'NONE', #2639 ) ;
#64398 = CARTESIAN_POINT ( 'NONE',  ( -12.69999999999998153, 0.000000000000000000, 0.000000000000000000 ) ) ;
#64399 = DIRECTION ( 'NONE',  ( 0.6830127018922181881, 0.6830127018922202975, -0.2588190451025214056 ) ) ;
#64400 = CARTESIAN_POINT ( 'NONE',  ( 93.60416666666665719, 2.130196079827422206, 7.950000000000001954 ) ) ;
#64401 = ADVANCED_FACE ( 'NONE', ( #47636 ), #127283, .F. ) ;
#64402 = ADVANCED_FACE ( 'NONE', ( #15624 ), #135343, .T. ) ;
#64403 = CARTESIAN_POINT ( 'NONE',  ( 3.000000000000000000, -4.600000000000012079, -20.40202195861968093 ) ) ;
#64405 = VERTEX_POINT ( 'NONE', #49768 ) ;
#64404 = PLANE ( 'NONE',  #139993 ) ;
#64406 = CARTESIAN_POINT ( 'NONE',  ( 69.25000000000000000, -9.735942053221458872E-16, 7.950000000000000178 ) ) ;
#64407 = DIRECTION ( 'NONE',  ( 1.000000000000000000, -1.248002500702738504E-15, 3.404785525682858480E-16 ) ) ;
#64408 = DIRECTION ( 'NONE',  ( -0.7071067811865486830, 0.7071067811865464625, 0.000000000000000000 ) ) ;
#64409 = FACE_OUTER_BOUND ( 'NONE', #94697, .T. ) ;
#64410 = ORIENTED_EDGE ( 'NONE', *, *, #124420, .F. ) ;
#64411 = ORIENTED_EDGE ( 'NONE', *, *, #118284, .T. ) ;
#64412 = EDGE_LOOP ( 'NONE', ( #21707, #2259, #109548, #120066 ) ) ;
#64413 = CARTESIAN_POINT ( 'NONE',  ( 99.75043019189810423, 3.055000000000002824, -5.291415217122919401 ) ) ;
#64414 = AXIS2_PLACEMENT_3D ( 'NONE', #46712, #122775, #69135 ) ;
#64415 = EDGE_LOOP ( 'NONE', ( #70861, #101947, #41836, #134019 ) ) ;
#64416 = CARTESIAN_POINT ( 'NONE',  ( 126.2468580783130960, -45.52550609312172725, 35.40428284070863896 ) ) ;
#64417 = PLANE ( 'NONE',  #75849 ) ;
#64418 = VERTEX_POINT ( 'NONE', #27983 ) ;
#64419 = ADVANCED_FACE ( 'NONE', ( #46937 ), #80250, .F. ) ;
#64420 = CARTESIAN_POINT ( 'NONE',  ( 183.6042742895559741, -52.10338527932238151, 40.45859298138253735 ) ) ;
#64421 = DIRECTION ( 'NONE',  ( -0.7071067811865486830, -0.7071067811865464625, 0.000000000000000000 ) ) ;
#64422 = CARTESIAN_POINT ( 'NONE',  ( 94.12043019189810877, 3.055000000000001936, -5.291415217122916737 ) ) ;
#64423 = ORIENTED_EDGE ( 'NONE', *, *, #127480, .F. ) ;
#64424 = VECTOR ( 'NONE', #115289, 1000.000000000000000 ) ;
#64425 = CARTESIAN_POINT ( 'NONE',  ( 0.000000000000000000, 0.5999999999999987566, -3.054668707061621191 ) ) ;
#64426 = LINE ( 'NONE', #30370, #73133 ) ;
#64427 = LINE ( 'NONE', #55003, #100199 ) ;
#64428 = VECTOR ( 'NONE', #4176, 1000.000000000000000 ) ;
#64429 = CARTESIAN_POINT ( 'NONE',  ( 0.000000000000000000, 0.000000000000000000, 5.000000000000000000 ) ) ;
#64430 = ORIENTED_EDGE ( 'NONE', *, *, #129141, .F. ) ;
#64431 = ORIENTED_EDGE ( 'NONE', *, *, #134066, .F. ) ;
#64432 = VECTOR ( 'NONE', #14876, 999.9999999999998863 ) ;
#64433 = ORIENTED_EDGE ( 'NONE', *, *, #36778, .F. ) ;
#64434 = CARTESIAN_POINT ( 'NONE',  ( -12.69999999999998153, 3.061616997868383634E-16, -2.500000000000000444 ) ) ;
#64435 = DIRECTION ( 'NONE',  ( 0.000000000000000000, 0.000000000000000000, 1.000000000000000000 ) ) ;
#64436 = CARTESIAN_POINT ( 'NONE',  ( 15.37956980810188767, 3.967499999999998916, 6.871911579029510442 ) ) ;
#64437 = VECTOR ( 'NONE', #143464, 1000.000000000000114 ) ;
#64438 = VECTOR ( 'NONE', #125281, 1000.000000000000000 ) ;
#64439 = DIRECTION ( 'NONE',  ( -0.3543493200069162685, -0.000000000000000000, -0.9351131265310288487 ) ) ;
#64440 = CARTESIAN_POINT ( 'NONE',  ( -11.18753812416045257, -22.22500000000000142, 4.000000000000000000 ) ) ;
#64441 =( LENGTH_UNIT ( ) NAMED_UNIT ( * ) SI_UNIT ( .MILLI., .METRE. ) );
#64442 = EDGE_CURVE ( 'NONE', #36267, #124621, #132122, .T. ) ;
#64443 = ORIENTED_EDGE ( 'NONE', *, *, #13608, .T. ) ;
#64444 = ORIENTED_EDGE ( 'NONE', *, *, #88518, .T. ) ;
#64445 = EDGE_CURVE ( 'NONE', #121029, #22536, #82380, .T. ) ;
#64446 = CARTESIAN_POINT ( 'NONE',  ( -17.29298673570684386, -21.74070752338406720, 4.999753212805220670 ) ) ;
#64447 = ORIENTED_EDGE ( 'NONE', *, *, #52929, .T. ) ;
#64448 = ORIENTED_EDGE ( 'NONE', *, *, #50327, .T. ) ;
#64449 = EDGE_CURVE ( 'NONE', #52608, #15705, #4023, .T. ) ;
#64450 = EDGE_CURVE ( 'NONE', #67554, #122496, #115660, .T. ) ;
#64451 = VECTOR ( 'NONE', #25869, 1000.000000000000000 ) ;
#64452 = CARTESIAN_POINT ( 'NONE',  ( 18.81250000000000355, -4.461849672132299993, -4.461849672132299105 ) ) ;
#64453 = CARTESIAN_POINT ( 'NONE',  ( 36.29974487139159578, -27.71228299555231445, 4.000000000000000000 ) ) ;
#64454 = ORIENTED_EDGE ( 'NONE', *, *, #14510, .T. ) ;
#64455 = CARTESIAN_POINT ( 'NONE',  ( 56.56250000000000000, -5.819803920172573086, -5.819803920172573974 ) ) ;
#64456 = DIRECTION ( 'NONE',  ( -0.7071067811865486830, -0.7071067811865464625, 0.000000000000000000 ) ) ;
#64457 = DIRECTION ( 'NONE',  ( -0.6830127018922181881, 0.6830127018922202975, -0.2588190451025214056 ) ) ;
#64458 = DIRECTION ( 'NONE',  ( -0.7071067811865487940, 0.7071067811865463515, 0.000000000000000000 ) ) ;
#64459 = VECTOR ( 'NONE', #47844, 1000.000000000000000 ) ;
#64460 = DIRECTION ( 'NONE',  ( -0.000000000000000000, 0.000000000000000000, 1.000000000000000000 ) ) ;
#64461 = ORIENTED_EDGE ( 'NONE', *, *, #69177, .T. ) ;
#64462 = CIRCLE ( 'NONE', #136174, 2.500000000000000444 ) ;
#64463 = CARTESIAN_POINT ( 'NONE',  ( 71.99451991528749772, 28.92564299267988304, 4.000000000000000000 ) ) ;
#64464 = PRESENTATION_LAYER_ASSIGNMENT (  '', '', ( #126957 ) ) ;
#64465 = EDGE_CURVE ( 'NONE', #17205, #130681, #58529, .T. ) ;
#64466 = ORIENTED_EDGE ( 'NONE', *, *, #18622, .T. ) ;
#64467 = DIRECTION ( 'NONE',  ( 0.6830127018922181881, 0.6830127018922202975, -0.2588190451025214056 ) ) ;
#64468 = FACE_OUTER_BOUND ( 'NONE', #10174, .T. ) ;
#64469 = ORIENTED_EDGE ( 'NONE', *, *, #1223, .F. ) ;
#64470 = CARTESIAN_POINT ( 'NONE',  ( -20.99451991528748707, 28.92564299267952777, 4.000000000000000000 ) ) ;
#64471 = EDGE_CURVE ( 'NONE', #80773, #43157, #116423, .T. ) ;
#64472 = ORIENTED_EDGE ( 'NONE', *, *, #112885, .F. ) ;
#64473 = LINE ( 'NONE', #5777, #38985 ) ;
#64474 = EDGE_LOOP ( 'NONE', ( #83928, #73604, #26716, #53185 ) ) ;
#64475 = VERTEX_POINT ( 'NONE', #103373 ) ;
#64476 = ORIENTED_EDGE ( 'NONE', *, *, #95541, .F. ) ;
#64477 = EDGE_CURVE ( 'NONE', #28064, #74252, #38862, .T. ) ;
#64478 = CARTESIAN_POINT ( 'NONE',  ( 29.22459685856478373, -1.637169565754160949, 6.109999999999997655 ) ) ;
#64479 = DIRECTION ( 'NONE',  ( -0.000000000000000000, 0.000000000000000000, 1.000000000000000000 ) ) ;
#64480 = FACE_OUTER_BOUND ( 'NONE', #28832, .T. ) ;
#64481 = DIRECTION ( 'NONE',  ( 0.000000000000000000, -1.000000000000000000, 0.000000000000000000 ) ) ;
#64482 = FACE_OUTER_BOUND ( 'NONE', #5741, .T. ) ;
#64483 = FACE_OUTER_BOUND ( 'NONE', #22032, .T. ) ;
#64484 = EDGE_CURVE ( 'NONE', #129447, #5674, #71496, .T. ) ;
#64485 = AXIS2_PLACEMENT_3D ( 'NONE', #31859, #43449, #42761 ) ;
#64486 = LINE ( 'NONE', #11491, #28448 ) ;
#64487 = AXIS2_PLACEMENT_3D ( 'NONE', #138733, #39426, #83659 ) ;
#64488 = CARTESIAN_POINT ( 'NONE',  ( -3.299744871391591339, -27.71228299555208352, 4.000000000000000000 ) ) ;
#64489 = CARTESIAN_POINT ( 'NONE',  ( 23.99999999999981881, -16.02097659208070368, -11.96015758381214766 ) ) ;
#64490 = DIRECTION ( 'NONE',  ( 0.7071067811865487940, 0.7071067811865463515, 0.000000000000000000 ) ) ;
#64491 = ORIENTED_EDGE ( 'NONE', *, *, #127229, .T. ) ;
#64492 = VERTEX_POINT ( 'NONE', #125884 ) ;
#64494 = EDGE_LOOP ( 'NONE', ( #64374, #32965, #107410, #80354 ) ) ;
#64493 = EDGE_CURVE ( 'NONE', #129366, #37814, #121721, .T. ) ;
#64495 = EDGE_LOOP ( 'NONE', ( #78598, #96335, #55391 ) ) ;
#64496 = CARTESIAN_POINT ( 'NONE',  ( 0.4892135623730947680, -27.52281430457055578, 5.000000000000000000 ) ) ;
#64497 = ORIENTED_EDGE ( 'NONE', *, *, #14074, .T. ) ;
#64498 = ORIENTED_EDGE ( 'NONE', *, *, #98642, .F. ) ;
#64499 = DIRECTION ( 'NONE',  ( -1.000000000000000000, -1.224606353822377258E-16, -0.000000000000000000 ) ) ;
#64500 = CARTESIAN_POINT ( 'NONE',  ( 184.1500000000000057, 0.000000000000000000, 0.000000000000000000 ) ) ;
#64501 = CARTESIAN_POINT ( 'NONE',  ( -5.207106781186503497, 0.7592924766157104211, 5.000000000000000000 ) ) ;
#64502 = EDGE_CURVE ( 'NONE', #123534, #96735, #130891, .T. ) ;
#64503 = EDGE_LOOP ( 'NONE', ( #7747, #63755, #12925, #114641 ) ) ;
#64504 = ADVANCED_FACE ( 'NONE', ( #39595 ), #140314, .F. ) ;
#64505 = DIRECTION ( 'NONE',  ( -0.3543493200069162685, -0.000000000000000000, -0.9351131265310288487 ) ) ;
#64506 = ORIENTED_EDGE ( 'NONE', *, *, #142315, .T. ) ;
#64507 = SURFACE_SIDE_STYLE ('',( #121723 ) ) ;
#64508 = EDGE_CURVE ( 'NONE', #56146, #134058, #22633, .T. ) ;
#64509 = CARTESIAN_POINT ( 'NONE',  ( 69.18398860626899705, 28.73617430169835529, 5.000000000000000000 ) ) ;
#64510 = CARTESIAN_POINT ( 'NONE',  ( 6.192069808101887674, -7.934999999999991616, -2.126176841940955242 ) ) ;
#64511 = ORIENTED_EDGE ( 'NONE', *, *, #10016, .F. ) ;
#64512 = CARTESIAN_POINT ( 'NONE',  ( 93.97459685856478018, 1.637169565754164280, -6.109999999999997655 ) ) ;
#64513 = CARTESIAN_POINT ( 'NONE',  ( -25.82816939922334143, 3.759292476615685441, 4.000000000000000000 ) ) ;
#64514 = CARTESIAN_POINT ( 'NONE',  ( 0.000000000000000000, 0.000000000000000000, 5.000000000000000000 ) ) ;
#64515 = DIRECTION ( 'NONE',  ( 0.7071067811865486830, -0.7071067811865464625, -0.000000000000000000 ) ) ;
#64516 = ORIENTED_EDGE ( 'NONE', *, *, #106579, .T. ) ;
#64517 = VERTEX_POINT ( 'NONE', #105522 ) ;
#64518 = CARTESIAN_POINT ( 'NONE',  ( 3.005480084712505828, 28.92564299267936079, 4.000000000000000000 ) ) ;
#64519 = ORIENTED_EDGE ( 'NONE', *, *, #6966, .T. ) ;
#64520 = DIRECTION ( 'NONE',  ( -1.000000000000000000, -1.224606353822377258E-16, -0.000000000000000000 ) ) ;
#64521 = LINE ( 'NONE', #19583, #108978 ) ;
#64522 = PLANE ( 'NONE',  #70610 ) ;
#64523 = LINE ( 'NONE', #96404, #56524 ) ;
#64524 = ORIENTED_EDGE ( 'NONE', *, *, #1175, .F. ) ;
#64525 = DIRECTION ( 'NONE',  ( -0.000000000000000000, 0.000000000000000000, 1.000000000000000000 ) ) ;
#64526 = DIRECTION ( 'NONE',  ( -0.7071067811865486830, -0.7071067811865464625, 0.000000000000000000 ) ) ;
#64527 = PLANE ( 'NONE',  #129885 ) ;
#64528 = ORIENTED_EDGE ( 'NONE', *, *, #65492, .T. ) ;
#64529 = CARTESIAN_POINT ( 'NONE',  ( -30.48921356237309510, -27.52281430457076894, 5.000000000000000000 ) ) ;
#64530 = AXIS2_PLACEMENT_3D ( 'NONE', #10064, #124550, #89085 ) ;
#64531 = VECTOR ( 'NONE', #1883, 1000.000000000000227 ) ;
#64532 = AXIS2_PLACEMENT_3D ( 'NONE', #45068, #26126, #89241 ) ;
#64533 = DIRECTION ( 'NONE',  ( -1.000000000000000000, 0.000000000000000000, 0.000000000000000000 ) ) ;
#64534 = VERTEX_POINT ( 'NONE', #30862 ) ;
#64535 = VECTOR ( 'NONE', #5766, 1000.000000000000227 ) ;
#64537 = ORIENTED_EDGE ( 'NONE', *, *, #133337, .T. ) ;
#64536 = CARTESIAN_POINT ( 'NONE',  ( 7.637717201596474048, 2.500000000000000444, 0.000000000000000000 ) ) ;
#64538 = ORIENTED_EDGE ( 'NONE', *, *, #26619, .T. ) ;
#64539 = CARTESIAN_POINT ( 'NONE',  ( -84.18398860626899705, 28.73617430169846187, 5.000000000000000000 ) ) ;
#64540 = DIRECTION ( 'NONE',  ( -0.000000000000000000, 0.000000000000000000, 1.000000000000000000 ) ) ;
#64541 = VECTOR ( 'NONE', #117240, 999.9999999999998863 ) ;
#64542 = ORIENTED_EDGE ( 'NONE', *, *, #4380, .T. ) ;
#64543 = PLANE ( 'NONE',  #74377 ) ;
#64544 = AXIS2_PLACEMENT_3D ( 'NONE', #105355, #128554, #107503 ) ;
#64545 = CARTESIAN_POINT ( 'NONE',  ( 0.000000000000000000, 0.000000000000000000, 5.000000000000000000 ) ) ;
#64546 = CARTESIAN_POINT ( 'NONE',  ( -25.49999999999982592, -17.56887692260762535, 4.000000000000000000 ) ) ;
#64547 =( BOUNDED_CURVE ( )  B_SPLINE_CURVE ( 3, ( #121311, #21993, #108256, #97393 ),
 .UNSPECIFIED., .F., .T. ) 
 B_SPLINE_CURVE_WITH_KNOTS ( ( 4, 4 ),
 ( 5.143245962375970315, 6.645403452391246191 ),
 .UNSPECIFIED. ) 
 CURVE ( )  GEOMETRIC_REPRESENTATION_ITEM ( )  RATIONAL_B_SPLINE_CURVE ( ( 1.000000000000000000, 0.8206354192515253887, 0.8206354192515253887, 1.000000000000000000 ) ) 
 REPRESENTATION_ITEM ( '' )  );
#64548 = LINE ( 'NONE', #53694, #32295 ) ;
#64549 = CARTESIAN_POINT ( 'NONE',  ( 0.1600000000000008360, -6.382865826061452807, -4.762547549401616287 ) ) ;
#64550 = CYLINDRICAL_SURFACE ( 'NONE', #79111, 2.500000000000000444 ) ;
#64551 = LINE ( 'NONE', #119612, #137396 ) ;
#64552 = CYLINDRICAL_SURFACE ( 'NONE', #143229, 1.000000000000000000 ) ;
#64553 = DIRECTION ( 'NONE',  ( 0.000000000000000000, -1.000000000000000000, 0.000000000000000000 ) ) ;
#64555 = VECTOR ( 'NONE', #63149, 1000.000000000000000 ) ;
#64554 = LINE ( 'NONE', #10164, #86130 ) ;
#64556 = CARTESIAN_POINT ( 'NONE',  ( -29.99451991528749417, 28.92564299267958816, 4.000000000000000000 ) ) ;
#64557 = LINE ( 'NONE', #50833, #85872 ) ;
#64558 = DIRECTION ( 'NONE',  ( -0.000000000000000000, -0.3543493200069153248, -0.9351131265310291818 ) ) ;
#64559 = ORIENTED_EDGE ( 'NONE', *, *, #14480, .F. ) ;
#64560 = VERTEX_POINT ( 'NONE', #106958 ) ;
#64561 = EDGE_LOOP ( 'NONE', ( #93207, #27496, #50695, #105748 ) ) ;
#64562 = CARTESIAN_POINT ( 'NONE',  ( 99.14583333333331439, 2.130196079827431976, -7.949999999999999289 ) ) ;
#64563 = CIRCLE ( 'NONE', #6656, 3.000000000000002220 ) ;
#64564 = ORIENTED_EDGE ( 'NONE', *, *, #20578, .F. ) ;
#64565 = EDGE_LOOP ( 'NONE', ( #56870, #83095, #95121, #129348 ) ) ;
#64566 = VERTEX_POINT ( 'NONE', #108350 ) ;
#64567 = FACE_OUTER_BOUND ( 'NONE', #52257, .T. ) ;
#64568 = VECTOR ( 'NONE', #131242, 1000.000000000000000 ) ;
#64569 = ORIENTED_EDGE ( 'NONE', *, *, #46463, .F. ) ;
#64570 = VECTOR ( 'NONE', #127170, 1000.000000000000000 ) ;
#64571 = CARTESIAN_POINT ( 'NONE',  ( 3.183988606268992161, 28.73617430169789699, 5.000000000000000000 ) ) ;
#64572 = AXIS2_PLACEMENT_3D ( 'NONE', #115851, #105002, #48490 ) ;
#64573 = CARTESIAN_POINT ( 'NONE',  ( 34.92499999999998295, -8.240707523384182664, 4.255531930566164078 ) ) ;
#64574 = PRESENTATION_LAYER_ASSIGNMENT (  '', '', ( #127064 ) ) ;
#64575 = LINE ( 'NONE', #76913, #92662 ) ;
#64576 = PLANE ( 'NONE',  #62761 ) ;
#64577 = CARTESIAN_POINT ( 'NONE',  ( 108.0629301918980900, 1.637169565754157174, 6.110000000000002984 ) ) ;
#64578 = EDGE_CURVE ( 'NONE', #30943, #91794, #141010, .T. ) ;
#64579 = ORIENTED_EDGE ( 'NONE', *, *, #112900, .F. ) ;
#64580 = CARTESIAN_POINT ( 'NONE',  ( 54.48921356237310221, -27.52281430457093236, 5.000000000000000000 ) ) ;
#64581 = ADVANCED_FACE ( 'NONE', ( #62773 ), #139639, .F. ) ;
#64582 = CARTESIAN_POINT ( 'NONE',  ( -24.72281430457042717, -21.72500000000000142, 5.000000000000000000 ) ) ;
#64583 = VECTOR ( 'NONE', #102194, 1000.000000000000000 ) ;
#64584 = CARTESIAN_POINT ( 'NONE',  ( 22.53999999999999915, 9.521314400968980422E-16, 0.000000000000000000 ) ) ;
#64585 = DIRECTION ( 'NONE',  ( -0.7071067811865486830, 0.7071067811865464625, 0.000000000000000000 ) ) ;
#64586 = FACE_OUTER_BOUND ( 'NONE', #98682, .T. ) ;
#64587 = AXIS2_PLACEMENT_3D ( 'NONE', #46338, #134768, #47078 ) ;
#64588 = CARTESIAN_POINT ( 'NONE',  ( 32.89169371712954870, 2.130196079827421762, 7.950000000000001066 ) ) ;
#64589 = LINE ( 'NONE', #63200, #81663 ) ;
#64590 = ORIENTED_EDGE ( 'NONE', *, *, #139148, .T. ) ;
#64591 = ORIENTED_EDGE ( 'NONE', *, *, #126923, .T. ) ;
#64592 = CARTESIAN_POINT ( 'NONE',  ( 31.33333333333332504, -6.884901960086287964, 3.974999999999998312 ) ) ;
#64593 = ORIENTED_EDGE ( 'NONE', *, *, #13181, .F. ) ;
#64594 = EDGE_CURVE ( 'NONE', #21679, #45954, #31561, .T. ) ;
#64595 = CARTESIAN_POINT ( 'NONE',  ( 19.73159235450332005, 9.902892378096218942E-16, 0.000000000000000000 ) ) ;
#64596 = LINE ( 'NONE', #108061, #101119 ) ;
#64597 = AXIS2_PLACEMENT_3D ( 'NONE', #30095, #66326, #43850 ) ;
#64598 = CARTESIAN_POINT ( 'NONE',  ( 12.19999999999999574, 12.19802518668052649, 4.711086268963014412 ) ) ;
#64599 =( NAMED_UNIT ( * ) SI_UNIT ( $, .STERADIAN. ) SOLID_ANGLE_UNIT ( ) );
#64600 = EDGE_CURVE ( 'NONE', #76199, #71344, #9025, .T. ) ;
#64601 = DIRECTION ( 'NONE',  ( 0.7071067811865486830, -0.7071067811865464625, -0.000000000000000000 ) ) ;
#64602 = DIRECTION ( 'NONE',  ( -0.6830127018922181881, 0.6830127018922202975, -0.2588190451025214056 ) ) ;
#64603 = CARTESIAN_POINT ( 'NONE',  ( 119.0579301918981230, 6.110000000000000320, -1.637169565754156064 ) ) ;
#64604 = EDGE_LOOP ( 'NONE', ( #40657, #51612, #73713, #99848, #107312 ) ) ;
#64605 = ORIENTED_EDGE ( 'NONE', *, *, #59432, .T. ) ;
#64606 = LINE ( 'NONE', #20358, #2131 ) ;
#64607 = EDGE_CURVE ( 'NONE', #101265, #115184, #138904, .T. ) ;
#64608 = CARTESIAN_POINT ( 'NONE',  ( -60.18398860626900415, 28.73617430169829490, 5.000000000000000000 ) ) ;
#64609 = CARTESIAN_POINT ( 'NONE',  ( -14.54487008052910824, -0.7407075233842735917, 4.335043535661659675 ) ) ;
#64610 = ORIENTED_EDGE ( 'NONE', *, *, #49779, .T. ) ;
#64611 = CARTESIAN_POINT ( 'NONE',  ( 44.62543019189810423, 5.291415217122919401, 3.055000000000002824 ) ) ;
#64612 = ORIENTED_EDGE ( 'NONE', *, *, #74448, .F. ) ;
#64613 = PLANE ( 'NONE',  #47093 ) ;
#64614 = LINE ( 'NONE', #129874, #13727 ) ;
#64615 = DIRECTION ( 'NONE',  ( -0.6830127018922181881, 0.6830127018922202975, -0.2588190451025214056 ) ) ;
#64616 = CARTESIAN_POINT ( 'NONE',  ( 35.34959685856478728, 6.109999999999996767, 1.637169565754163836 ) ) ;
#64617 = ORIENTED_EDGE ( 'NONE', *, *, #46372, .F. ) ;
#64618 = ADVANCED_FACE ( 'NONE', ( #83828 ), #128036, .T. ) ;
#64619 = CARTESIAN_POINT ( 'NONE',  ( -28.99806943317882002, -22.22500000000000142, 4.500000000000000888 ) ) ;
#64620 = ORIENTED_EDGE ( 'NONE', *, *, #954, .T. ) ;
#64621 = ORIENTED_EDGE ( 'NONE', *, *, #96748, .F. ) ;
#64622 = VERTEX_POINT ( 'NONE', #19946 ) ;
#64623 = EDGE_CURVE ( 'NONE', #130094, #84395, #42463, .T. ) ;
#64624 = EDGE_CURVE ( 'NONE', #13935, #86438, #85203, .T. ) ;
#64626 = DIRECTION ( 'NONE',  ( -0.000000000000000000, -0.3543493200069152693, 0.9351131265310292928 ) ) ;
#64625 = VECTOR ( 'NONE', #131942, 999.9999999999998863 ) ;
#64627 = CARTESIAN_POINT ( 'NONE',  ( 79.26669371712955581, -7.949999999999998401, 2.130196079827423983 ) ) ;
#64628 = EDGE_LOOP ( 'NONE', ( #66762, #49650, #134513, #116021 ) ) ;
#64629 = PLANE ( 'NONE',  #6630 ) ;
#64630 = COLOUR_RGB ( '', 0.72549020, 0.75294118, 0.79215686) ;
#64631 = LINE ( 'NONE', #41439, #76027 ) ;
#64632 = AXIS2_PLACEMENT_3D ( 'NONE', #25770, #136669, #135966 ) ;
#64633 = VECTOR ( 'NONE', #72797, 1000.000000000000114 ) ;
#64634 = VECTOR ( 'NONE', #71389, 1000.000000000000000 ) ;
#64635 = EDGE_CURVE ( 'NONE', #66768, #137573, #85835, .T. ) ;
#64636 = CARTESIAN_POINT ( 'NONE',  ( -36.18398860626899705, 28.73617430169812437, 5.000000000000000000 ) ) ;
#64637 = VECTOR ( 'NONE', #34520, 1000.000000000000000 ) ;
#64638 = FACE_BOUND ( 'NONE', #126880, .T. ) ;
#64639 = EDGE_CURVE ( 'NONE', #91199, #8776, #118548, .T. ) ;
#64640 = ORIENTED_EDGE ( 'NONE', *, *, #21262, .T. ) ;
#64641 = CARTESIAN_POINT ( 'NONE',  ( 24.48921356237309510, -27.52281430457072631, 5.000000000000000000 ) ) ;
#64642 = CARTESIAN_POINT ( 'NONE',  ( 51.29974487139158867, -27.71228299555242103, 4.000000000000000000 ) ) ;
#64643 = CARTESIAN_POINT ( 'NONE',  ( 27.79289321881326558, 9.759292476615625489, 5.000000000000000000 ) ) ;
#64644 = EDGE_CURVE ( 'NONE', #59942, #55364, #107672, .T. ) ;
#64645 = ORIENTED_EDGE ( 'NONE', *, *, #27425, .T. ) ;
#64646 = FILL_AREA_STYLE ('',( #128486 ) ) ;
#64647 = VERTEX_POINT ( 'NONE', #41716 ) ;
#64648 = ORIENTED_EDGE ( 'NONE', *, *, #50531, .F. ) ;
#64649 = AXIS2_PLACEMENT_3D ( 'NONE', #119779, #120480, #141577 ) ;
#64650 = DIRECTION ( 'NONE',  ( -0.3543493200069162685, -0.000000000000000000, -0.9351131265310288487 ) ) ;
#64651 = ORIENTED_EDGE ( 'NONE', *, *, #72275, .T. ) ;
#64652 = CARTESIAN_POINT ( 'NONE',  ( 53.28709685856478018, 3.054999999999997495, 5.291415217122919401 ) ) ;
#64653 = ORIENTED_EDGE ( 'NONE', *, *, #28708, .F. ) ;
#64654 = EDGE_CURVE ( 'NONE', #40909, #10224, #96721, .T. ) ;
#64655 = DIRECTION ( 'NONE',  ( -0.3543493200069162685, -0.000000000000000000, -0.9351131265310288487 ) ) ;
#64656 = EDGE_LOOP ( 'NONE', ( #119922, #129868, #29515, #138412 ) ) ;
#64657 = FACE_OUTER_BOUND ( 'NONE', #22938, .T. ) ;
#64658 = ORIENTED_EDGE ( 'NONE', *, *, #131848, .F. ) ;
#64659 = LINE ( 'NONE', #51655, #56345 ) ;
#64660 = DIRECTION ( 'NONE',  ( -0.7071067811865486830, -0.7071067811865464625, 0.000000000000000000 ) ) ;
#64661 = COLOUR_RGB ( '', 0.08235294, 0.09019608, 0.10196078) ;
#64662 = VECTOR ( 'NONE', #54034, 1000.000000000000000 ) ;
#64663 = EDGE_CURVE ( 'NONE', #82847, #93164, #86624, .T. ) ;
#64664 = MECHANICAL_DESIGN_GEOMETRIC_PRESENTATION_REPRESENTATION (  '', ( #131834 ), #101705 ) ;
#64665 = CARTESIAN_POINT ( 'NONE',  ( -16.82816939922341248, -11.24070752338416845, 4.000000000000000000 ) ) ;
#64666 = CARTESIAN_POINT ( 'NONE',  ( 28.49999999999980460, -10.91253812416064406, 4.000000000000000000 ) ) ;
#64667 = PLANE ( 'NONE',  #106111 ) ;
#64668 = CARTESIAN_POINT ( 'NONE',  ( 33.70612307739173730, 22.22500000000000142, 4.000000000000000000 ) ) ;
#64669 = CARTESIAN_POINT ( 'NONE',  ( 1.171830600776464504, 15.75929247661555976, 4.000000000000000000 ) ) ;
#64670 = ORIENTED_EDGE ( 'NONE', *, *, #41889, .T. ) ;
#64671 = ORIENTED_EDGE ( 'NONE', *, *, #17579, .F. ) ;
#64672 = ORIENTED_EDGE ( 'NONE', *, *, #87360, .T. ) ;
#64673 = CONICAL_SURFACE ( 'NONE', #71609, 2.055000000000001048, 0.9599310885968758145 ) ;
#64674 = DIRECTION ( 'NONE',  ( 0.7071067811865486830, -0.7071067811865464625, -0.000000000000000000 ) ) ;
#64675 = DIRECTION ( 'NONE',  ( 0.3543493200069162685, -0.000000000000000000, -0.9351131265310288487 ) ) ;
#64676 = ORIENTED_EDGE ( 'NONE', *, *, #114485, .F. ) ;
#64677 = VECTOR ( 'NONE', #83100, 1000.000000000000227 ) ;
#64678 = AXIS2_PLACEMENT_3D ( 'NONE', #27624, #17464, #129798 ) ;
#64679 = ORIENTED_EDGE ( 'NONE', *, *, #129468, .T. ) ;
#64680 = LINE ( 'NONE', #8804, #81453 ) ;
#64681 = FACE_OUTER_BOUND ( 'NONE', #80047, .T. ) ;
#64682 = AXIS2_PLACEMENT_3D ( 'NONE', #52994, #85622, #141457 ) ;
#64683 = CARTESIAN_POINT ( 'NONE',  ( -22.82816939922336630, -5.240707523384225297, 4.000000000000000000 ) ) ;
#64684 = ORIENTED_EDGE ( 'NONE', *, *, #133262, .T. ) ;
#64685 = AXIS2_PLACEMENT_3D ( 'NONE', #22978, #133235, #25874 ) ;
#64686 = EDGE_CURVE ( 'NONE', #96071, #130556, #54059, .T. ) ;
#64687 = DIRECTION ( 'NONE',  ( -0.000000000000000000, 0.3543493200069153248, 0.9351131265310292928 ) ) ;
#64688 = VECTOR ( 'NONE', #142462, 999.9999999999998863 ) ;
#64689 = EDGE_CURVE ( 'NONE', #130625, #114963, #100392, .T. ) ;
#64690 = LINE ( 'NONE', #87, #104558 ) ;
#64691 = EDGE_CURVE ( 'NONE', #142234, #40966, #44271, .T. ) ;
#64692 = CARTESIAN_POINT ( 'NONE',  ( 14.65040314143522338, 7.934999999999989839, -2.126176841940961904 ) ) ;
#64693 = CARTESIAN_POINT ( 'NONE',  ( 8.999999999999937828, -16.06887692260764666, 4.000000000000000000 ) ) ;
#64694 = ORIENTED_EDGE ( 'NONE', *, *, #91498, .T. ) ;
#64695 = CARTESIAN_POINT ( 'NONE',  ( 118.6204301918981230, 3.055000000000002380, -5.291415217122917625 ) ) ;
#64696 = DIRECTION ( 'NONE',  ( 0.6830127018922180770, -0.6830127018922204085, -0.2588190451025213501 ) ) ;
#64697 = CARTESIAN_POINT ( 'NONE',  ( 29.99999999999978684, -7.068876922607743474, 4.000000000000000000 ) ) ;
#64698 = STYLED_ITEM ( 'NONE', ( #31135 ), #21254 ) ;
#64700 = ORIENTED_EDGE ( 'NONE', *, *, #140677, .T. ) ;
#64699 = CARTESIAN_POINT ( 'NONE',  ( -33.18398860626899705, 28.73617430169810305, 5.000000000000000000 ) ) ;
#64701 = FACE_OUTER_BOUND ( 'NONE', #6076, .T. ) ;
#64702 = ORIENTED_EDGE ( 'NONE', *, *, #13663, .T. ) ;
#64703 = CARTESIAN_POINT ( 'NONE',  ( -23.55512991947090029, -0.7407075233842665973, 4.307968247156982677 ) ) ;
#64704 = DIRECTION ( 'NONE',  ( 1.000000000000000000, 0.000000000000000000, 0.000000000000000000 ) ) ;
#64705 = LINE ( 'NONE', #43655, #98079 ) ;
#64706 = VERTEX_POINT ( 'NONE', #65661 ) ;
#64707 = CARTESIAN_POINT ( 'NONE',  ( -45.18398860626900415, 28.73617430169818832, 5.000000000000000000 ) ) ;
#64708 = LINE ( 'NONE', #129226, #141698 ) ;
#64709 = VERTEX_POINT ( 'NONE', #98247 ) ;
#64710 = DIRECTION ( 'NONE',  ( -0.7071067811865486830, -0.7071067811865464625, 0.000000000000000000 ) ) ;
#64711 = DIRECTION ( 'NONE',  ( 0.7071067811865486830, -0.7071067811865464625, -0.000000000000000000 ) ) ;
#64712 = ORIENTED_EDGE ( 'NONE', *, *, #90091, .F. ) ;
#64713 = DIRECTION ( 'NONE',  ( -0.7071067811865486830, -0.7071067811865464625, -0.000000000000000000 ) ) ;
#64714 = CARTESIAN_POINT ( 'NONE',  ( 5.510786437626906675, -27.52281430457051314, 5.000000000000000000 ) ) ;
#64715 = EDGE_LOOP ( 'NONE', ( #123269, #113043, #35395 ) ) ;
#64716 = ORIENTED_EDGE ( 'NONE', *, *, #69354, .T. ) ;
#64717 = CARTESIAN_POINT ( 'NONE',  ( 2.510786437626908008, -27.52281430457053446, 5.000000000000000000 ) ) ;
#64718 = FILL_AREA_STYLE_COLOUR ( '', #66840 ) ;
#64719 = PLANE ( 'NONE',  #31976 ) ;
#64720 = CARTESIAN_POINT ( 'NONE',  ( -12.69999999999998153, 0.000000000000000000, 2.500000000000000444 ) ) ;
#64721 = LINE ( 'NONE', #75607, #137052 ) ;
#64722 = ORIENTED_EDGE ( 'NONE', *, *, #117390, .F. ) ;
#64723 = FACE_OUTER_BOUND ( 'NONE', #74202, .T. ) ;
#64724 = CARTESIAN_POINT ( 'NONE',  ( 72.29974487139158157, -27.71228299555256669, 4.000000000000000000 ) ) ;
#64725 = CARTESIAN_POINT ( 'NONE',  ( -4.499999999999966249, -1.533600742197721134, 5.000000000000000000 ) ) ;
#64726 = DIRECTION ( 'NONE',  ( -0.000000000000000000, -0.3543493200069152693, 0.9351131265310292928 ) ) ;
#64727 = CARTESIAN_POINT ( 'NONE',  ( 38.70376352523144448, 6.109999999999999432, 1.122388791418549108E-15 ) ) ;
#64728 = CARTESIAN_POINT ( 'NONE',  ( 3.000000000000000000, -49.85820393249935734, -34.92499999999996874 ) ) ;
#64729 = VERTEX_POINT ( 'NONE', #10493 ) ;
#64730 = ORIENTED_EDGE ( 'NONE', *, *, #20518, .T. ) ;
#64731 = DIRECTION ( 'NONE',  ( -0.6830127018922180770, -0.6830127018922204085, -0.2588190451025213501 ) ) ;
#64732 = EDGE_LOOP ( 'NONE', ( #110019, #50617, #104359, #90455 ) ) ;
#64733 = VERTEX_POINT ( 'NONE', #11921 ) ;
#64734 = VECTOR ( 'NONE', #117890, 1000.000000000000000 ) ;
#64735 = CARTESIAN_POINT ( 'NONE',  ( 24.18398860626899705, 28.73617430169804265, 5.000000000000000000 ) ) ;
#64736 = PLANE ( 'NONE',  #113282 ) ;
#64737 = VECTOR ( 'NONE', #91596, 1000.000000000000000 ) ;
#64738 = AXIS2_PLACEMENT_3D ( 'NONE', #23321, #133545, #21909 ) ;
#64739 = VECTOR ( 'NONE', #21182, 999.9999999999998863 ) ;
#64740 = VERTEX_POINT ( 'NONE', #89498 ) ;
#64741 = CARTESIAN_POINT ( 'NONE',  ( 0.1630955763144136539, 0.3999999999999995781, 2.152173649344992779 ) ) ;
#64742 = CARTESIAN_POINT ( 'NONE',  ( 69.48921356237309510, -27.52281430457103895, 5.000000000000000000 ) ) ;
#64744 = EDGE_CURVE ( 'NONE', #58453, #100009, #9788, .T. ) ;
#64743 = VECTOR ( 'NONE', #100330, 1000.000000000000000 ) ;
#64745 = DIRECTION ( 'NONE',  ( -0.7071067811865486830, -0.7071067811865464625, 0.000000000000000000 ) ) ;
#64746 = DIRECTION ( 'NONE',  ( -0.7071067811865486830, -0.7071067811865464625, 0.000000000000000000 ) ) ;
#64747 = CARTESIAN_POINT ( 'NONE',  ( 32.99451991528749062, 28.92564299267960948, 4.000000000000000000 ) ) ;
#64748 = ADVANCED_FACE ( 'NONE', ( #142471 ), #122846, .T. ) ;
#64749 = EDGE_CURVE ( 'NONE', #128517, #41026, #33019, .T. ) ;
#64750 = EDGE_LOOP ( 'NONE', ( #105488, #105506, #112514, #25729, #17249 ) ) ;
#64751 = CYLINDRICAL_SURFACE ( 'NONE', #108920, 2.500000000000000444 ) ;
#64752 = FACE_OUTER_BOUND ( 'NONE', #61509, .T. ) ;
#64753 = AXIS2_PLACEMENT_3D ( 'NONE', #94134, #105708, #94833 ) ;
#64754 = LINE ( 'NONE', #53139, #34015 ) ;
#64755 = CARTESIAN_POINT ( 'NONE',  ( -9.489213562373095101, -27.52281430457062328, 5.000000000000000000 ) ) ;
#64756 = CARTESIAN_POINT ( 'NONE',  ( 0.2569208697893815008, -0.3999999999999998002, -2.015694669338588429 ) ) ;
#64757 = LINE ( 'NONE', #98787, #57416 ) ;
#64758 = EDGE_CURVE ( 'NONE', #43661, #74078, #133733, .T. ) ;
#64760 = EDGE_CURVE ( 'NONE', #13171, #100977, #11180, .T. ) ;
#64759 = CARTESIAN_POINT ( 'NONE',  ( 60.30836038379622011, 7.949999999999997513, 2.130196079827431088 ) ) ;
#64761 = CARTESIAN_POINT ( 'NONE',  ( -66.18398860626901126, 28.73617430169833753, 5.000000000000000000 ) ) ;
#64762 = VECTOR ( 'NONE', #63998, 1000.000000000000000 ) ;
#64763 = ORIENTED_EDGE ( 'NONE', *, *, #10640, .T. ) ;
#64764 = ORIENTED_EDGE ( 'NONE', *, *, #102224, .T. ) ;
#64765 = CARTESIAN_POINT ( 'NONE',  ( 51.31249999999998579, 5.819803920172571310, 5.819803920172575751 ) ) ;
#64766 = CARTESIAN_POINT ( 'NONE',  ( 19.49999999999986500, -10.04351517176476172, -1.623559851933778830 ) ) ;
#64767 = EDGE_CURVE ( 'NONE', #112641, #77505, #55458, .T. ) ;
#64768 = LINE ( 'NONE', #85790, #117929 ) ;
#64769 = VECTOR ( 'NONE', #74760, 1000.000000000000227 ) ;
#64770 = AXIS2_PLACEMENT_3D ( 'NONE', #134193, #46, #66787 ) ;
#64771 = CARTESIAN_POINT ( 'NONE',  ( 33.70710678118631165, -15.74070752338412049, 5.000000000000000000 ) ) ;
#64772 = ORIENTED_EDGE ( 'NONE', *, *, #93579, .T. ) ;
#64773 = DIRECTION ( 'NONE',  ( 0.7071067811865487940, 0.7071067811865463515, 0.000000000000000000 ) ) ;
#64774 = PLANE ( 'NONE',  #104663 ) ;
#64775 = EDGE_CURVE ( 'NONE', #111906, #85516, #23524, .T. ) ;
#64776 = CIRCLE ( 'NONE', #87943, 2.247899999999996901 ) ;
#64777 = CARTESIAN_POINT ( 'NONE',  ( 50.16709685856476852, -3.055000000000000160, -5.291415217122921177 ) ) ;
#64778 = EDGE_LOOP ( 'NONE', ( #110020, #140392, #55752, #120956 ) ) ;
#64779 = CARTESIAN_POINT ( 'NONE',  ( -34.92500000000001137, 22.22500000000000142, 4.000000000000000000 ) ) ;
#64780 = VERTEX_POINT ( 'NONE', #99646 ) ;
#64781 = VERTEX_POINT ( 'NONE', #98931 ) ;
#64782 = PLANE ( 'NONE',  #100471 ) ;
#64783 = AXIS2_PLACEMENT_3D ( 'NONE', #134338, #89389, #23404 ) ;
#64784 = EDGE_CURVE ( 'NONE', #142812, #59733, #317, .T. ) ;
#64785 = AXIS2_PLACEMENT_3D ( 'NONE', #62612, #84380, #128568 ) ;
#64786 = LINE ( 'NONE', #42333, #33842 ) ;
#64787 = CARTESIAN_POINT ( 'NONE',  ( 15.32816939922342847, -9.740707523384177335, 4.000000000000000000 ) ) ;
#64788 =( GEOMETRIC_REPRESENTATION_CONTEXT ( 3 ) GLOBAL_UNCERTAINTY_ASSIGNED_CONTEXT ( ( #59085 ) ) GLOBAL_UNIT_ASSIGNED_CONTEXT ( ( #8518, #36739, #524 ) ) REPRESENTATION_CONTEXT ( 'NONE', 'WORKASPACE' ) );
#64789 = ORIENTED_EDGE ( 'NONE', *, *, #20213, .T. ) ;
#64790 = CARTESIAN_POINT ( 'NONE',  ( 51.48921356237309510, -27.52281430457091460, 5.000000000000000000 ) ) ;
#64792 = VERTEX_POINT ( 'NONE', #88083 ) ;
#64791 = CARTESIAN_POINT ( 'NONE',  ( 8.212472949537106715, 0.000000000000000000, 6.094999999999989981 ) ) ;
#64793 = VECTOR ( 'NONE', #15798, 1000.000000000000227 ) ;
#64794 = CARTESIAN_POINT ( 'NONE',  ( 81.66709685856477563, -3.055000000000000160, -5.291415217122921177 ) ) ;
#64795 = CARTESIAN_POINT ( 'NONE',  ( 14.00000000000000178, 0.000000000000000000, 6.094999999999989981 ) ) ;
#64796 = LINE ( 'NONE', #140897, #117197 ) ;
#64797 = CARTESIAN_POINT ( 'NONE',  ( 8.999999999999941380, -3.485240976185067563, -4.108735105802378662 ) ) ;
#64798 = VECTOR ( 'NONE', #19110, 1000.000000000000114 ) ;
#64799 = ADVANCED_FACE ( 'NONE', ( #132327 ), #44619, .F. ) ;
#64800 = LINE ( 'NONE', #87967, #13891 ) ;
#64801 = LINE ( 'NONE', #98140, #71681 ) ;
#64802 = ORIENTED_EDGE ( 'NONE', *, *, #67709, .T. ) ;
#64803 = CARTESIAN_POINT ( 'NONE',  ( 0.000000000000000000, 0.000000000000000000, 5.000000000000000000 ) ) ;
#64804 = CARTESIAN_POINT ( 'NONE',  ( 66.41209685856478018, 5.291415217122921177, -3.054999999999994831 ) ) ;
#64805 = DIRECTION ( 'NONE',  ( 0.000000000000000000, 0.000000000000000000, 1.000000000000000000 ) ) ;
#64806 = EDGE_CURVE ( 'NONE', #103866, #135194, #122114, .T. ) ;
#64807 = DIRECTION ( 'NONE',  ( 0.000000000000000000, 1.000000000000000000, 0.000000000000000000 ) ) ;
#64808 = CARTESIAN_POINT ( 'NONE',  ( 10.52840764549667618, 2.500000000000000888, 3.061616997868383141E-16 ) ) ;
#64809 = EDGE_LOOP ( 'NONE', ( #113669, #21115, #135578, #58889 ) ) ;
#64810 = VERTEX_POINT ( 'NONE', #1731 ) ;
#64811 = AXIS2_PLACEMENT_3D ( 'NONE', #26047, #36216, #69577 ) ;
#64812 = FACE_OUTER_BOUND ( 'NONE', #1001, .T. ) ;
#64813 = CARTESIAN_POINT ( 'NONE',  ( 39.29974487139159578, -27.71228299555233576, 4.000000000000000000 ) ) ;
#64814 = VERTEX_POINT ( 'NONE', #106584 ) ;
#64815 = EDGE_CURVE ( 'NONE', #66768, #86570, #26915, .T. ) ;
#64816 = ORIENTED_EDGE ( 'NONE', *, *, #38651, .T. ) ;
#64817 = DIRECTION ( 'NONE',  ( 0.5735764363510451602, 0.8191520442889924647, 0.000000000000000000 ) ) ;
#64819 = EDGE_CURVE ( 'NONE', #86117, #19554, #58160, .T. ) ;
#64818 = EDGE_LOOP ( 'NONE', ( #77769, #49103, #126220, #17155 ) ) ;
#64820 = DIRECTION ( 'NONE',  ( -0.7071067811865487940, 0.7071067811865463515, 0.000000000000000000 ) ) ;
#64821 = DIRECTION ( 'NONE',  ( -0.7071067811865486830, 0.7071067811865464625, 0.000000000000000000 ) ) ;
#64822 = VECTOR ( 'NONE', #49557, 1000.000000000000227 ) ;
#64823 = EDGE_CURVE ( 'NONE', #126389, #89318, #128386, .T. ) ;
#64824 = CARTESIAN_POINT ( 'NONE',  ( 17.99451991528748351, 28.92564299267950645, 4.000000000000000000 ) ) ;
#64825 = FACE_BOUND ( 'NONE', #129397, .T. ) ;
#64826 = DIRECTION ( 'NONE',  ( -0.000000000000000000, 0.000000000000000000, 1.000000000000000000 ) ) ;
#64827 = DIRECTION ( 'NONE',  ( -1.000000000000000000, -1.224606353822377258E-16, -0.000000000000000000 ) ) ;
#64828 = CARTESIAN_POINT ( 'NONE',  ( -27.29974487139158512, -27.71228299555225405, 4.000000000000000000 ) ) ;
#64830 = ORIENTED_EDGE ( 'NONE', *, *, #46400, .T. ) ;
#64829 = CARTESIAN_POINT ( 'NONE',  ( 1.500000000000000000, 0.000000000000000000, 0.000000000000000000 ) ) ;
#64831 = LINE ( 'NONE', #9706, #78766 ) ;
#64832 = VERTEX_POINT ( 'NONE', #103735 ) ;
#64833 = VERTEX_POINT ( 'NONE', #16752 ) ;
#64834 = CARTESIAN_POINT ( 'NONE',  ( 80.70376352523145158, 6.109999999999998543, 1.122388791418548911E-15 ) ) ;
#64835 = ORIENTED_EDGE ( 'NONE', *, *, #114431, .F. ) ;
#64836 = EDGE_CURVE ( 'NONE', #97655, #75539, #82054, .T. ) ;
#64837 = LINE ( 'NONE', #124201, #360 ) ;
#64838 = ORIENTED_EDGE ( 'NONE', *, *, #14501, .T. ) ;
#64839 = DIRECTION ( 'NONE',  ( -0.000000000000000000, -0.3543493200069152693, 0.9351131265310292928 ) ) ;
#64840 = EDGE_CURVE ( 'NONE', #15605, #45425, #5844, .T. ) ;
#64841 = LINE ( 'NONE', #53986, #121264 ) ;
#64842 = DIRECTION ( 'NONE',  ( -0.000000000000000000, 0.3543493200069153248, 0.9351131265310292928 ) ) ;
#64843 = VECTOR ( 'NONE', #35307, 1000.000000000000000 ) ;
#64844 = CARTESIAN_POINT ( 'NONE',  ( 21.66240673564756491, 0.000000000000000000, 0.000000000000000000 ) ) ;
#64845 = CARTESIAN_POINT ( 'NONE',  ( 10.49999999999992539, -6.839392718269124316, -8.480912228396110919 ) ) ;
#64846 = CARTESIAN_POINT ( 'NONE',  ( 24.29974487139158867, -27.71228299555223273, 4.000000000000000000 ) ) ;
#64847 = CARTESIAN_POINT ( 'NONE',  ( 20.19999999999999929, 9.521314400968980422E-16, 0.000000000000000000 ) ) ;
#64848 = DIRECTION ( 'NONE',  ( -0.6830127018922181881, 0.6830127018922202975, -0.2588190451025214056 ) ) ;
#64850 = ORIENTED_EDGE ( 'NONE', *, *, #19594, .F. ) ;
#64849 = AXIS2_PLACEMENT_3D ( 'NONE', #111115, #110404, #34302 ) ;
#64851 = VECTOR ( 'NONE', #47951, 1000.000000000000227 ) ;
#64852 = CONICAL_SURFACE ( 'NONE', #18545, 2.500000000000000888, 0.9599310885968822538 ) ;
#64853 = CARTESIAN_POINT ( 'NONE',  ( 25.39999999999999858, 0.000000000000000000, 0.000000000000000000 ) ) ;
#64854 = AXIS2_PLACEMENT_3D ( 'NONE', #22573, #23299, #11700 ) ;
#64855 = ORIENTED_EDGE ( 'NONE', *, *, #79569, .T. ) ;
#64856 = CARTESIAN_POINT ( 'NONE',  ( -18.18398860626898994, 28.73617430169800002, 5.000000000000000000 ) ) ;
#64857 = LINE ( 'NONE', #62012, #65167 ) ;
#64858 = CIRCLE ( 'NONE', #46363, 2.500000000000000444 ) ;
#64859 = ORIENTED_EDGE ( 'NONE', *, *, #35920, .F. ) ;
#64860 = VERTEX_POINT ( 'NONE', #29062 ) ;
#64861 = ORIENTED_EDGE ( 'NONE', *, *, #3415, .T. ) ;
#64862 = EDGE_CURVE ( 'NONE', #53913, #42124, #49423, .T. ) ;
#64863 = CARTESIAN_POINT ( 'NONE',  ( 39.66709685856477563, -3.055000000000000160, -5.291415217122921177 ) ) ;
#64864 = ORIENTED_EDGE ( 'NONE', *, *, #93477, .T. ) ;
#64865 = VECTOR ( 'NONE', #2668, 1000.000000000000000 ) ;
#64866 = LINE ( 'NONE', #54006, #38935 ) ;
#64867 = ADVANCED_FACE ( 'NONE', ( #18141 ), #15289, .F. ) ;
#64868 = CARTESIAN_POINT ( 'NONE',  ( 20.99065804761471199, 0.000000000000000000, 2.500000000000000444 ) ) ;
#64869 = CARTESIAN_POINT ( 'NONE',  ( 27.02497294953710494, -4.461849672132299993, -4.461849672132299105 ) ) ;
#64870 = CARTESIAN_POINT ( 'NONE',  ( -5.035040864892940782, 11.85438914953258305, -27.38739306153288311 ) ) ;
#64871 = ORIENTED_EDGE ( 'NONE', *, *, #78263, .T. ) ;
#64872 = DIRECTION ( 'NONE',  ( -0.6830127018922181881, 0.6830127018922202975, -0.2588190451025214056 ) ) ;
#64873 = ORIENTED_EDGE ( 'NONE', *, *, #72980, .F. ) ;
#64874 = AXIS2_PLACEMENT_3D ( 'NONE', #109994, #143341, #19422 ) ;
#64875 = DIRECTION ( 'NONE',  ( -0.7071067811865486830, -0.7071067811865464625, -0.000000000000000000 ) ) ;
#64877 = ORIENTED_EDGE ( 'NONE', *, *, #56875, .F. ) ;
#64876 = CARTESIAN_POINT ( 'NONE',  ( 34.49999999999976552, 18.05432934483075513, 4.994342998332162331 ) ) ;
#64878 = ORIENTED_EDGE ( 'NONE', *, *, #88313, .F. ) ;
#64879 = CARTESIAN_POINT ( 'NONE',  ( 41.99451991528749062, 28.92564299267967343, 4.000000000000000000 ) ) ;
#64880 = CARTESIAN_POINT ( 'NONE',  ( 5.691592354503320905, -2.500000000000000000, 3.061616997868384127E-16 ) ) ;
#64881 = DIRECTION ( 'NONE',  ( -0.6830127018922180770, -0.6830127018922204085, -0.2588190451025213501 ) ) ;
#64882 = VERTEX_POINT ( 'NONE', #137839 ) ;
#64883 = VECTOR ( 'NONE', #122159, 999.9999999999998863 ) ;
#64884 = ADVANCED_FACE ( 'NONE', ( #105875 ), #40662, .F. ) ;
#64885 = CARTESIAN_POINT ( 'NONE',  ( 27.18398860626900060, 28.73617430169806042, 5.000000000000000000 ) ) ;
#64886 = ORIENTED_EDGE ( 'NONE', *, *, #84488, .F. ) ;
#64887 = ORIENTED_EDGE ( 'NONE', *, *, #4566, .T. ) ;
#64888 = VERTEX_POINT ( 'NONE', #51546 ) ;
#64890 = CARTESIAN_POINT ( 'NONE',  ( -27.48921356237309155, -27.52281430457074762, 5.000000000000000000 ) ) ;
#64889 = VECTOR ( 'NONE', #119976, 1000.000000000000000 ) ;
#64891 = DIRECTION ( 'NONE',  ( -0.3543493200069162685, -0.000000000000000000, -0.9351131265310288487 ) ) ;
#64892 = DIRECTION ( 'NONE',  ( -0.3543493200069163240, -0.000000000000000000, -0.9351131265310288487 ) ) ;
#64893 = VECTOR ( 'NONE', #8705, 1000.000000000000000 ) ;
#64894 = SURFACE_SIDE_STYLE ('',( #110491 ) ) ;
#64895 = DIRECTION ( 'NONE',  ( -0.7071067811865487940, 0.7071067811865463515, -0.000000000000000000 ) ) ;
#64896 = CARTESIAN_POINT ( 'NONE',  ( -13.26506670282042499, 12.75929247661558996, 18.34774599283959517 ) ) ;
#64897 = FACE_OUTER_BOUND ( 'NONE', #106619, .T. ) ;
#64898 = ADVANCED_FACE ( 'NONE', ( #59576 ), #115306, .F. ) ;
#64899 = ORIENTED_EDGE ( 'NONE', *, *, #42293, .T. ) ;
#64900 = CARTESIAN_POINT ( 'NONE',  ( -29.67183060077627843, -18.74070752338409918, 4.000000000000000000 ) ) ;
#64901 = ORIENTED_EDGE ( 'NONE', *, *, #45178, .F. ) ;
#64902 = LINE ( 'NONE', #10480, #54050 ) ;
#64903 = CARTESIAN_POINT ( 'NONE',  ( 34.92499999999999005, 21.66246187583879390, 4.000000000000000000 ) ) ;
#64904 = VERTEX_POINT ( 'NONE', #71882 ) ;
#64905 = TOROIDAL_SURFACE ( 'NONE', #118042, 2.000000000000000000, 1.000000000000000000 ) ;
#64906 = CARTESIAN_POINT ( 'NONE',  ( -9.489213562373095101, -27.52281430457062328, 5.000000000000000000 ) ) ;
#64907 = FACE_OUTER_BOUND ( 'NONE', #11865, .T. ) ;
#64908 = ORIENTED_EDGE ( 'NONE', *, *, #18942, .F. ) ;
#64909 = ORIENTED_EDGE ( 'NONE', *, *, #20444, .F. ) ;
#64910 = CARTESIAN_POINT ( 'NONE',  ( 0.000000000000000000, 0.000000000000000000, 5.000000000000000000 ) ) ;
#64911 = CARTESIAN_POINT ( 'NONE',  ( 111.9791666666666714, -7.950000000000000178, 2.130196079827424427 ) ) ;
#64912 = VECTOR ( 'NONE', #37286, 1000.000000000000227 ) ;
#64913 = FACE_OUTER_BOUND ( 'NONE', #34188, .T. ) ;
#64914 = DIRECTION ( 'NONE',  ( 0.7071067811865486830, -0.7071067811865464625, -0.000000000000000000 ) ) ;
#64915 = CARTESIAN_POINT ( 'NONE',  ( 69.03709685856478018, -3.054999999999999272, -5.291415217122919401 ) ) ;
#64916 = CARTESIAN_POINT ( 'NONE',  ( -39.18398860626899705, 28.73617430169814568, 5.000000000000000000 ) ) ;
#64917 = CARTESIAN_POINT ( 'NONE',  ( 184.1500000000000057, -17.48000000000005016, -12.70000000000045404 ) ) ;
#64918 = CARTESIAN_POINT ( 'NONE',  ( 84.41666666666667140, -6.884901960086287076, -3.975000000000000977 ) ) ;
#64919 = ORIENTED_EDGE ( 'NONE', *, *, #12188, .T. ) ;
#64920 = DIRECTION ( 'NONE',  ( -0.000000000000000000, -0.3543493200069152693, 0.9351131265310292928 ) ) ;
#64921 = EDGE_CURVE ( 'NONE', #137344, #104855, #60288, .T. ) ;
#64922 = ORIENTED_EDGE ( 'NONE', *, *, #5022, .T. ) ;
#64923 = VECTOR ( 'NONE', #64505, 1000.000000000000227 ) ;
#64924 = FACE_OUTER_BOUND ( 'NONE', #101959, .T. ) ;
#64925 = ORIENTED_EDGE ( 'NONE', *, *, #68566, .F. ) ;
#64926 = LINE ( 'NONE', #87388, #117827 ) ;
#64928 = ORIENTED_EDGE ( 'NONE', *, *, #136460, .T. ) ;
#64927 = PLANE ( 'NONE',  #116041 ) ;
#64929 = FACE_OUTER_BOUND ( 'NONE', #8305, .T. ) ;
#64930 = CARTESIAN_POINT ( 'NONE',  ( -20.99999999999985434, -13.97847968911261951, -0.1324546996127294596 ) ) ;
#64931 = CARTESIAN_POINT ( 'NONE',  ( 19.56687199751245032, -21.74070752338406720, 6.915939825044026712 ) ) ;
#64932 = EDGE_CURVE ( 'NONE', #38574, #90775, #116054, .T. ) ;
#64933 = ADVANCED_FACE ( 'NONE', ( #50823 ), #105184, .F. ) ;
#64934 = ORIENTED_EDGE ( 'NONE', *, *, #57775, .T. ) ;
#64935 = ORIENTED_EDGE ( 'NONE', *, *, #42660, .F. ) ;
#64936 = DIRECTION ( 'NONE',  ( 0.000000000000000000, -1.000000000000000000, 0.000000000000000000 ) ) ;
#64937 = DIRECTION ( 'NONE',  ( 0.3543493200069162685, -0.000000000000000000, -0.9351131265310288487 ) ) ;
#64938 = VECTOR ( 'NONE', #32299, 1000.000000000000000 ) ;
#64939 = DIRECTION ( 'NONE',  ( -0.7071067811865487940, 0.7071067811865463515, 0.000000000000000000 ) ) ;
#64940 = CARTESIAN_POINT ( 'NONE',  ( -0.7123099396602794453, -21.73547319004781642, 4.999917730833664642 ) ) ;
#64941 = EDGE_CURVE ( 'NONE', #142188, #51446, #138545, .T. ) ;
#64943 = EDGE_CURVE ( 'NONE', #44540, #128760, #139281, .T. ) ;
#64942 = CARTESIAN_POINT ( 'NONE',  ( 85.68336038379624142, -2.130196079827426203, 7.949999999999997513 ) ) ;
#64944 = DIRECTION ( 'NONE',  ( -0.6830127018922181881, 0.6830127018922202975, -0.2588190451025214056 ) ) ;
#64945 = DIRECTION ( 'NONE',  ( -0.000000000000000000, -0.3543493200069152693, 0.9351131265310292928 ) ) ;
#64947 = EDGE_CURVE ( 'NONE', #41180, #78032, #132235, .T. ) ;
#64946 = ORIENTED_EDGE ( 'NONE', *, *, #47383, .T. ) ;
#64948 = CARTESIAN_POINT ( 'NONE',  ( 83.24999999999998579, -9.735942053221458872E-16, 7.950000000000000178 ) ) ;
#64949 = DIRECTION ( 'NONE',  ( -0.7071067811865486830, -0.7071067811865464625, 0.000000000000000000 ) ) ;
#64950 = EDGE_CURVE ( 'NONE', #73748, #109110, #84191, .T. ) ;
#64951 = LINE ( 'NONE', #64226, #134136 ) ;
#64952 = LINE ( 'NONE', #106996, #35929 ) ;
#64953 = EDGE_CURVE ( 'NONE', #76469, #65412, #92883, .T. ) ;
#64954 = ORIENTED_EDGE ( 'NONE', *, *, #103897, .F. ) ;
#64955 = VECTOR ( 'NONE', #54760, 1000.000000000000000 ) ;
#64956 = LINE ( 'NONE', #87415, #51395 ) ;
#64957 = CIRCLE ( 'NONE', #101977, 2.055000000000000604 ) ;
#64959 = VERTEX_POINT ( 'NONE', #10843 ) ;
#64958 = ADVANCED_FACE ( 'NONE', ( #129793 ), #109002, .F. ) ;
#64960 = VECTOR ( 'NONE', #136459, 1000.000000000000000 ) ;
#64961 = CARTESIAN_POINT ( 'NONE',  ( 76.56293019189810423, 1.637169565754157174, 6.110000000000002984 ) ) ;
#64962 = LINE ( 'NONE', #40365, #70935 ) ;
#64963 = DIRECTION ( 'NONE',  ( 0.000000000000000000, -1.000000000000000000, 0.000000000000000000 ) ) ;
#64964 = ORIENTED_EDGE ( 'NONE', *, *, #70482, .F. ) ;
#64965 = AXIS2_PLACEMENT_3D ( 'NONE', #54377, #131186, #111572 ) ;
#64966 = VECTOR ( 'NONE', #51196, 1000.000000000000227 ) ;
#64967 = AXIS2_PLACEMENT_3D ( 'NONE', #72416, #124608, #141937 ) ;
#64968 = CARTESIAN_POINT ( 'NONE',  ( 8.500000000000000000, 9.521314400968980422E-16, 0.000000000000000000 ) ) ;
#64969 = AXIS2_PLACEMENT_3D ( 'NONE', #53812, #42934, #76265 ) ;
#64970 = ADVANCED_FACE ( 'NONE', ( #108011 ), #9404, .F. ) ;
#64971 = CARTESIAN_POINT ( 'NONE',  ( -10.49999999999992539, 10.46639925780214853, 5.000000000000000000 ) ) ;
#64972 = DIRECTION ( 'NONE',  ( 0.7071067811865487940, 0.7071067811865463515, 0.000000000000000000 ) ) ;
#64973 = DIRECTION ( 'NONE',  ( 0.000000000000000000, 0.06845965770171358322, -0.9976538855070752332 ) ) ;
#64975 = VERTEX_POINT ( 'NONE', #42816 ) ;
#64974 = LINE ( 'NONE', #99709, #3534 ) ;
#64976 = LINE ( 'NONE', #19307, #113185 ) ;
#64977 = DIRECTION ( 'NONE',  ( 0.3543493200069162685, -0.000000000000000000, -0.9351131265310288487 ) ) ;
#64978 = CARTESIAN_POINT ( 'NONE',  ( -30.13499573751603933, 3.759292476615678336, 15.36553568819732796 ) ) ;
#64979 = CIRCLE ( 'NONE', #2414, 3.000000000000002220 ) ;
#64980 = EDGE_CURVE ( 'NONE', #48229, #107272, #110167, .T. ) ;
#64981 = DIRECTION ( 'NONE',  ( 0.7071067811865486830, -0.7071067811865464625, -0.000000000000000000 ) ) ;
#64982 = ORIENTED_EDGE ( 'NONE', *, *, #100451, .F. ) ;
#64983 = ORIENTED_EDGE ( 'NONE', *, *, #34196, .T. ) ;
#64984 = CARTESIAN_POINT ( 'NONE',  ( 61.39626352523143993, 4.472830434245840259, -4.472830434245839371 ) ) ;
#64985 = ORIENTED_EDGE ( 'NONE', *, *, #58671, .T. ) ;
#64986 = DIRECTION ( 'NONE',  ( -0.7071067811865487940, 0.7071067811865463515, -0.000000000000000000 ) ) ;
#64987 = FACE_OUTER_BOUND ( 'NONE', #9054, .T. ) ;
#64988 = AXIS2_PLACEMENT_3D ( 'NONE', #43330, #129597, #21575 ) ;
#64989 = CARTESIAN_POINT ( 'NONE',  ( -57.29974487139158157, -27.71228299555246011, 4.000000000000000000 ) ) ;
#64990 = CARTESIAN_POINT ( 'NONE',  ( -12.18398860626900060, 28.73617430169795739, 5.000000000000000000 ) ) ;
#64991 = ORIENTED_EDGE ( 'NONE', *, *, #56498, .T. ) ;
#64992 = CARTESIAN_POINT ( 'NONE',  ( -38.99451991528749062, 28.92564299267965211, 4.000000000000000000 ) ) ;
#64993 = AXIS2_PLACEMENT_3D ( 'NONE', #41420, #63227, #140724 ) ;
#64994 = EDGE_CURVE ( 'NONE', #73333, #98820, #142130, .T. ) ;
#64995 = VERTEX_POINT ( 'NONE', #120309 ) ;
#64996 = AXIS2_PLACEMENT_3D ( 'NONE', #13985, #102473, #12571 ) ;
#64997 = LINE ( 'NONE', #86743, #44518 ) ;
#64998 = EDGE_CURVE ( 'NONE', #67140, #28687, #99283, .T. ) ;
#64999 = VECTOR ( 'NONE', #84224, 1000.000000000000000 ) ;
#65000 = PLANE ( 'NONE',  #70991 ) ;
#65001 = PLANE ( 'NONE',  #21540 ) ;
#65002 = VECTOR ( 'NONE', #46775, 1000.000000000000227 ) ;
#65003 = ADVANCED_FACE ( 'NONE', ( #42104 ), #19605, .F. ) ;
#65004 = EDGE_LOOP ( 'NONE', ( #89678, #22338, #70664, #140286, #46198, #4963, #142427, #136057, #38425, #71402 ) ) ;
#65005 = ORIENTED_EDGE ( 'NONE', *, *, #56682, .T. ) ;
#65006 = LINE ( 'NONE', #9117, #17532 ) ;
#65007 =( GEOMETRIC_REPRESENTATION_CONTEXT ( 3 ) GLOBAL_UNCERTAINTY_ASSIGNED_CONTEXT ( ( #122867 ) ) GLOBAL_UNIT_ASSIGNED_CONTEXT ( ( #52406, #42278, #20477 ) ) REPRESENTATION_CONTEXT ( 'NONE', 'WORKASPACE' ) );
#65008 = DIRECTION ( 'NONE',  ( 0.6830127018922181881, 0.6830127018922202975, -0.2588190451025214056 ) ) ;
#65009 = LINE ( 'NONE', #141855, #9529 ) ;
#65010 = FACE_OUTER_BOUND ( 'NONE', #132769, .T. ) ;
#65011 = CARTESIAN_POINT ( 'NONE',  ( 18.29974487139159223, -27.71228299555219010, 4.000000000000000000 ) ) ;
#65012 = LINE ( 'NONE', #20756, #95192 ) ;
#65013 = ORIENTED_EDGE ( 'NONE', *, *, #79328, .T. ) ;
#65014 = VECTOR ( 'NONE', #98078, 999.9999999999998863 ) ;
#65015 = VERTEX_POINT ( 'NONE', #97891 ) ;
#65016 = CARTESIAN_POINT ( 'NONE',  ( 110.1620968585647944, -5.291415217122919401, 3.054999999999997939 ) ) ;
#65017 = ORIENTED_EDGE ( 'NONE', *, *, #94829, .T. ) ;
#65018 = EDGE_CURVE ( 'NONE', #109272, #43579, #107326, .T. ) ;
#65019 = ORIENTED_EDGE ( 'NONE', *, *, #138766, .F. ) ;
#65020 = AXIS2_PLACEMENT_3D ( 'NONE', #20329, #97922, #65321 ) ;
#65021 = CARTESIAN_POINT ( 'NONE',  ( 25.08376352523143638, -6.110000000000001208, -3.741295971395164515E-16 ) ) ;
#65022 = CARTESIAN_POINT ( 'NONE',  ( 34.92499999999998295, 22.22500000000000142, 4.000000000000000000 ) ) ;
#65023 = ORIENTED_EDGE ( 'NONE', *, *, #85655, .T. ) ;
#65024 = FACE_OUTER_BOUND ( 'NONE', #142707, .T. ) ;
#65025 = CARTESIAN_POINT ( 'NONE',  ( 2.301729841053981485, 3.821174125832445049E-16, 0.000000000000000000 ) ) ;
#65026 = EDGE_CURVE ( 'NONE', #56703, #99523, #30501, .T. ) ;
#65027 = CARTESIAN_POINT ( 'NONE',  ( 58.85002705046289151, -5.819803920172573086, -5.819803920172573086 ) ) ;
#65028 = CARTESIAN_POINT ( 'NONE',  ( 2.670806282870439308, -3.047499999999997211, -5.278424836066143655 ) ) ;
#65029 = VECTOR ( 'NONE', #22229, 1000.000000000000227 ) ;
#65030 = DIRECTION ( 'NONE',  ( 0.6830127018922180770, -0.6830127018922204085, -0.2588190451025213501 ) ) ;
#65031 = ORIENTED_EDGE ( 'NONE', *, *, #30145, .F. ) ;
#65032 = CARTESIAN_POINT ( 'NONE',  ( 0.000000000000000000, 0.000000000000000000, 5.000000000000000000 ) ) ;
#65033 = CARTESIAN_POINT ( 'NONE',  ( 50.43749999999999289, 5.819803920172574863, -5.819803920172573086 ) ) ;
#65034 = ORIENTED_EDGE ( 'NONE', *, *, #35835, .T. ) ;
#65035 = EDGE_CURVE ( 'NONE', #117767, #141737, #131229, .T. ) ;
#65036 = ORIENTED_EDGE ( 'NONE', *, *, #126582, .T. ) ;
#65037 = ORIENTED_EDGE ( 'NONE', *, *, #68056, .F. ) ;
#65038 = CARTESIAN_POINT ( 'NONE',  ( 66.50043019189810423, -3.055000000000002380, 5.291415217122920289 ) ) ;
#65039 = CIRCLE ( 'NONE', #127523, 2.500000000000000888 ) ;
#65040 = ORIENTED_EDGE ( 'NONE', *, *, #17658, .F. ) ;
#65041 = VECTOR ( 'NONE', #86987, 999.9999999999998863 ) ;
#65042 = DIRECTION ( 'NONE',  ( -0.7071067811865486830, -0.7071067811865464625, -0.000000000000000000 ) ) ;
#65043 = EDGE_CURVE ( 'NONE', #64534, #2906, #98589, .T. ) ;
#65044 =( LENGTH_UNIT ( ) NAMED_UNIT ( * ) SI_UNIT ( .MILLI., .METRE. ) );
#65045 = CARTESIAN_POINT ( 'NONE',  ( 96.54209685856477563, 5.291415217122923842, -3.054999999999996163 ) ) ;
#65046 = CARTESIAN_POINT ( 'NONE',  ( 18.48921356237309510, -27.52281430457068367, 5.000000000000000000 ) ) ;
#65048 = DIRECTION ( 'NONE',  ( -0.5735764363510503783, -0.8191520442889886899, 0.000000000000000000 ) ) ;
#65047 = CARTESIAN_POINT ( 'NONE',  ( 0.03865102804815071652, 0.4000000000000001332, -2.083945628037807030 ) ) ;
#65049 = ORIENTED_EDGE ( 'NONE', *, *, #44256, .F. ) ;
#65050 = DIRECTION ( 'NONE',  ( 0.000000000000000000, -1.000000000000000000, 0.000000000000000000 ) ) ;
#65051 = AXIS2_PLACEMENT_3D ( 'NONE', #86981, #107297, #131203 ) ;
#65052 = CARTESIAN_POINT ( 'NONE',  ( 2.510786437626908008, -27.52281430457053446, 5.000000000000000000 ) ) ;
#65053 = ADVANCED_FACE ( 'NONE', ( #97126 ), #64543, .T. ) ;
#65054 = CARTESIAN_POINT ( 'NONE',  ( -10.17183060077639745, 3.759292476615674783, 4.000000000000000000 ) ) ;
#65056 = DIRECTION ( 'NONE',  ( -0.000000000000000000, 0.000000000000000000, 1.000000000000000000 ) ) ;
#65055 = AXIS2_PLACEMENT_3D ( 'NONE', #92619, #5603, #16480 ) ;
#65058 = ORIENTED_EDGE ( 'NONE', *, *, #85371, .T. ) ;
#65057 = VECTOR ( 'NONE', #82464, 1000.000000000000000 ) ;
#65059 = EDGE_CURVE ( 'NONE', #128930, #14912, #54414, .T. ) ;
#65060 = FACE_OUTER_BOUND ( 'NONE', #75366, .T. ) ;
#65061 = ORIENTED_EDGE ( 'NONE', *, *, #130157, .F. ) ;
#65062 = VERTEX_POINT ( 'NONE', #41348 ) ;
#65063 = ORIENTED_EDGE ( 'NONE', *, *, #17637, .F. ) ;
#65064 = CARTESIAN_POINT ( 'NONE',  ( 118.7662635252314516, 4.472830434245838482, -4.472830434245837594 ) ) ;
#65065 = CONICAL_SURFACE ( 'NONE', #32672, 2.055000000000001048, 0.9599310885968758145 ) ;
#65066 = VECTOR ( 'NONE', #77255, 1000.000000000000000 ) ;
#65067 = EDGE_LOOP ( 'NONE', ( #71920, #81021, #70135, #69146 ) ) ;
#65068 = VECTOR ( 'NONE', #128722, 1000.000000000000000 ) ;
#65069 = STYLED_ITEM ( 'NONE', ( #129136 ), #142469 ) ;
#65070 = DIRECTION ( 'NONE',  ( -0.7071067811865486830, -0.7071067811865464625, 0.000000000000000000 ) ) ;
#65071 = FACE_OUTER_BOUND ( 'NONE', #103179, .T. ) ;
#65072 = EDGE_CURVE ( 'NONE', #98060, #43787, #118914, .T. ) ;
#65073 = ORIENTED_EDGE ( 'NONE', *, *, #128356, .T. ) ;
#65074 = FACE_OUTER_BOUND ( 'NONE', #35099, .T. ) ;
#65076 = ORIENTED_EDGE ( 'NONE', *, *, #33616, .F. ) ;
#65075 = VECTOR ( 'NONE', #41774, 999.9999999999998863 ) ;
#65077 = CARTESIAN_POINT ( 'NONE',  ( 10.18706980810188689, -2.126176841940956130, 7.934999999999991616 ) ) ;
#65078 =( LENGTH_UNIT ( ) NAMED_UNIT ( * ) SI_UNIT ( .MILLI., .METRE. ) );
#65079 = DIRECTION ( 'NONE',  ( -0.7071067811865487940, 0.7071067811865463515, -0.000000000000000000 ) ) ;
#65080 = AXIS2_PLACEMENT_3D ( 'NONE', #66951, #136471, #69837 ) ;
#65081 = DIRECTION ( 'NONE',  ( -0.7071067811865487940, 0.7071067811865463515, 0.000000000000000000 ) ) ;
#65082 = VERTEX_POINT ( 'NONE', #52925 ) ;
#65083 = ORIENTED_EDGE ( 'NONE', *, *, #81192, .F. ) ;
#65084 = VERTEX_POINT ( 'NONE', #86314 ) ;
#65086 = AXIS2_PLACEMENT_3D ( 'NONE', #22097, #68507, #57623 ) ;
#65085 = FILL_AREA_STYLE_COLOUR ( '', #90329 ) ;
#65087 =( LENGTH_UNIT ( ) NAMED_UNIT ( * ) SI_UNIT ( .MILLI., .METRE. ) );
#65088 = CARTESIAN_POINT ( 'NONE',  ( -31.63753812416075206, 22.22499999999999432, 4.000000000000000000 ) ) ;
#65089 = PLANE ( 'NONE',  #122365 ) ;
#65090 = FACE_OUTER_BOUND ( 'NONE', #119165, .T. ) ;
#65091 = VECTOR ( 'NONE', #63391, 1000.000000000000227 ) ;
#65092 = PLANE ( 'NONE',  #136379 ) ;
#65093 = CARTESIAN_POINT ( 'NONE',  ( 26.25043019189810067, 3.055000000000002824, -5.291415217122919401 ) ) ;
#65094 = DIRECTION ( 'NONE',  ( -0.000000000000000000, 0.000000000000000000, 1.000000000000000000 ) ) ;
#65095 = PLANE ( 'NONE',  #111452 ) ;
#65096 = AXIS2_PLACEMENT_3D ( 'NONE', #39902, #105808, #74663 ) ;
#65097 = ORIENTED_EDGE ( 'NONE', *, *, #96182, .F. ) ;
#65098 = CARTESIAN_POINT ( 'NONE',  ( 28.49999999999980105, -11.94781430457070392, 5.000000000000000000 ) ) ;
#65099 = EDGE_CURVE ( 'NONE', #116519, #43439, #31918, .T. ) ;
#65100 = VERTEX_POINT ( 'NONE', #108725 ) ;
#65102 = VECTOR ( 'NONE', #47318, 1000.000000000000000 ) ;
#65101 = CARTESIAN_POINT ( 'NONE',  ( -21.62762920772360786, 8.558752285115851066, 4.000000000000000000 ) ) ;
#65103 = ORIENTED_EDGE ( 'NONE', *, *, #143188, .F. ) ;
#65104 = CARTESIAN_POINT ( 'NONE',  ( -17.99451991528748351, 28.92564299267950645, 4.000000000000000000 ) ) ;
#65106 = ORIENTED_EDGE ( 'NONE', *, *, #72494, .T. ) ;
#65105 = DIRECTION ( 'NONE',  ( -0.000000000000000000, 0.000000000000000000, 1.000000000000000000 ) ) ;
#65107 = VECTOR ( 'NONE', #8167, 1000.000000000000000 ) ;
#65108 = FACE_OUTER_BOUND ( 'NONE', #63921, .T. ) ;
#65109 = ORIENTED_EDGE ( 'NONE', *, *, #33126, .T. ) ;
#65110 = FACE_OUTER_BOUND ( 'NONE', #113655, .T. ) ;
#65111 = ORIENTED_EDGE ( 'NONE', *, *, #125455, .T. ) ;
#65112 = DIRECTION ( 'NONE',  ( -0.000000000000000000, -0.000000000000000000, 1.000000000000000000 ) ) ;
#65113 = UNCERTAINTY_MEASURE_WITH_UNIT (LENGTH_MEASURE( 1.000000000000000082E-05 ), #87432, 'distance_accuracy_value', 'NONE');
#65114 = ORIENTED_EDGE ( 'NONE', *, *, #42860, .F. ) ;
#65116 = ADVANCED_FACE ( 'NONE', ( #10152 ), #142819, .F. ) ;
#65115 = CARTESIAN_POINT ( 'NONE',  ( 114.2666937171295700, -7.949999999999999289, 2.130196079827424427 ) ) ;
#65117 = CARTESIAN_POINT ( 'NONE',  ( 49.07919371712955581, 3.975000000000002753, -6.884901960086283523 ) ) ;
#65118 = AXIS2_PLACEMENT_3D ( 'NONE', #40403, #84612, #30211 ) ;
#65119 = DIRECTION ( 'NONE',  ( -1.000000000000000000, -0.000000000000000000, -0.000000000000000000 ) ) ;
#65120 = EDGE_CURVE ( 'NONE', #69350, #59049, #110866, .T. ) ;
#65121 = LINE ( 'NONE', #62983, #118591 ) ;
#65122 = LINE ( 'NONE', #32478, #137599 ) ;
#65123 = EDGE_CURVE ( 'NONE', #111265, #117852, #80439, .T. ) ;
#65124 = CARTESIAN_POINT ( 'NONE',  ( -25.49999999999981526, -11.56887692260769995, 4.000000000000000000 ) ) ;
#65126 = VECTOR ( 'NONE', #126609, 1000.000000000000000 ) ;
#65125 = CARTESIAN_POINT ( 'NONE',  ( 4.520833333333333037, -6.094999999999989981, -1.633150327867689100 ) ) ;
#65127 = CARTESIAN_POINT ( 'NONE',  ( 13.68706980810188512, -2.126176841940956130, 7.934999999999990727 ) ) ;
#65128 = DIRECTION ( 'NONE',  ( -1.000000000000000000, -0.000000000000000000, -0.000000000000000000 ) ) ;
#65130 = ADVANCED_FACE ( 'NONE', ( #56578 ), #133387, .F. ) ;
#65129 = FACE_OUTER_BOUND ( 'NONE', #132962, .T. ) ;
#65131 = VERTEX_POINT ( 'NONE', #34076 ) ;
#65132 = EDGE_LOOP ( 'NONE', ( #49935, #55062, #33832, #120960 ) ) ;
#65133 = CARTESIAN_POINT ( 'NONE',  ( -5.999999999999963585, 11.58746187583913390, 4.000000000000000000 ) ) ;
#65134 = ORIENTED_EDGE ( 'NONE', *, *, #138064, .F. ) ;
#65135 = EDGE_CURVE ( 'NONE', #110737, #84831, #78288, .T. ) ;
#65136 = DIRECTION ( 'NONE',  ( -0.3543493200069162685, -0.000000000000000000, -0.9351131265310288487 ) ) ;
#65137 = FACE_OUTER_BOUND ( 'NONE', #139908, .T. ) ;
#65138 = AXIS2_PLACEMENT_3D ( 'NONE', #1383, #132688, #65996 ) ;
#65139 = DIRECTION ( 'NONE',  ( 0.7071067811865487940, -0.7071067811865463515, 0.000000000000000000 ) ) ;
#65140 = VERTEX_POINT ( 'NONE', #135527 ) ;
#65141 = DIRECTION ( 'NONE',  ( -0.7071067811865487940, 0.7071067811865463515, -0.000000000000000000 ) ) ;
#65142 = CARTESIAN_POINT ( 'NONE',  ( 75.48921356237309510, -27.52281430457107803, 5.000000000000000000 ) ) ;
#65143 = EDGE_CURVE ( 'NONE', #108859, #59468, #22435, .T. ) ;
#65144 = ADVANCED_FACE ( 'NONE', ( #100041 ), #58725, .F. ) ;
#65145 = CARTESIAN_POINT ( 'NONE',  ( 10.49999999999993250, 6.052185695429105117, 5.000000000000000000 ) ) ;
#65146 = CARTESIAN_POINT ( 'NONE',  ( 0.3872656504350777129, -51.96230815476842224, 39.57541490114646621 ) ) ;
#65148 = ORIENTED_EDGE ( 'NONE', *, *, #70201, .T. ) ;
#65147 = CARTESIAN_POINT ( 'NONE',  ( 34.92499999999998295, -8.993876922607942248, 4.000000000000000000 ) ) ;
#65149 = CARTESIAN_POINT ( 'NONE',  ( 95.50000000000000000, 0.000000000000000000, -7.950000000000000178 ) ) ;
#65150 = CARTESIAN_POINT ( 'NONE',  ( 131.5423521607622774, -52.00875322212549179, -39.33676470588227403 ) ) ;
#65151 = VECTOR ( 'NONE', #94340, 1000.000000000000000 ) ;
#65152 = LINE ( 'NONE', #19474, #125776 ) ;
#65153 = CARTESIAN_POINT ( 'NONE',  ( 45.18398860626900415, 28.73617430169818832, 5.000000000000000000 ) ) ;
#65154 = EDGE_CURVE ( 'NONE', #28611, #23453, #102892, .T. ) ;
#65155 = CARTESIAN_POINT ( 'NONE',  ( 22.85159235450332105, 9.902892378096218942E-16, 0.000000000000000000 ) ) ;
#65156 = VERTEX_POINT ( 'NONE', #33387 ) ;
#65157 = EDGE_LOOP ( 'NONE', ( #134172, #116271, #125098, #90159, #137998 ) ) ;
#65158 = ORIENTED_EDGE ( 'NONE', *, *, #53861, .T. ) ;
#65159 = CARTESIAN_POINT ( 'NONE',  ( 93.18793019189809002, 6.110000000000002984, -1.637169565754156730 ) ) ;
#65160 = ORIENTED_EDGE ( 'NONE', *, *, #120338, .T. ) ;
#65161 = CARTESIAN_POINT ( 'NONE',  ( 21.41161490594815930, 22.22500000000000142, 4.777194822843818578 ) ) ;
#65162 = CARTESIAN_POINT ( 'NONE',  ( 85.53752705046288440, -9.735942053221456900E-16, 7.949999999999998401 ) ) ;
#65163 = ORIENTED_EDGE ( 'NONE', *, *, #49468, .F. ) ;
#65164 = AXIS2_PLACEMENT_3D ( 'NONE', #39021, #70279, #83245 ) ;
#65165 = CARTESIAN_POINT ( 'NONE',  ( 184.1499999999998067, -49.85820393249939286, 34.92500000000001847 ) ) ;
#65166 = DIRECTION ( 'NONE',  ( -0.3543493200069162685, -0.000000000000000000, -0.9351131265310288487 ) ) ;
#65167 = VECTOR ( 'NONE', #86614, 1000.000000000000000 ) ;
#65168 = AXIS2_PLACEMENT_3D ( 'NONE', #127201, #48224, #18412 ) ;
#65169 = CARTESIAN_POINT ( 'NONE',  ( 89.89126352523143737, -4.472830434245839371, -4.472830434245839371 ) ) ;
#65170 = VERTEX_POINT ( 'NONE', #77588 ) ;
#65171 = LINE ( 'NONE', #99165, #39741 ) ;
#65172 = EDGE_CURVE ( 'NONE', #113402, #141378, #111579, .T. ) ;
#65173 = VECTOR ( 'NONE', #123926, 999.9999999999998863 ) ;
#65174 = AXIS2_PLACEMENT_3D ( 'NONE', #105723, #85405, #138385 ) ;
#65175 = CARTESIAN_POINT ( 'NONE',  ( -34.49999999999975842, 12.05432934483081553, 4.994342998332167660 ) ) ;
#65176 = ORIENTED_EDGE ( 'NONE', *, *, #142876, .F. ) ;
#65177 = VERTEX_POINT ( 'NONE', #44988 ) ;
#65178 = EDGE_LOOP ( 'NONE', ( #52546, #77233, #4666, #136863 ) ) ;
#65179 = CARTESIAN_POINT ( 'NONE',  ( 7.499999999999944045, -2.568876922607782998, 4.000000000000000000 ) ) ;
#65180 = FACE_OUTER_BOUND ( 'NONE', #61277, .T. ) ;
#65181 = CARTESIAN_POINT ( 'NONE',  ( 18.15040314143521982, 7.934999999999988951, -2.126176841940961904 ) ) ;
#65182 = CARTESIAN_POINT ( 'NONE',  ( 17.20710678118642889, 12.75929247661558463, 5.000000000000000000 ) ) ;
#65183 = VECTOR ( 'NONE', #110394, 1000.000000000000227 ) ;
#65184 = CYLINDRICAL_SURFACE ( 'NONE', #22493, 7.950000000000000178 ) ;
#65185 = ADVANCED_FACE ( 'NONE', ( #112339 ), #41982, .T. ) ;
#65186 = DIRECTION ( 'NONE',  ( -0.000000000000000000, -0.3543493200069152693, 0.9351131265310292928 ) ) ;
#65187 = PRESENTATION_STYLE_ASSIGNMENT (( #86922 ) ) ;
#65188 = ORIENTED_EDGE ( 'NONE', *, *, #66583, .F. ) ;
#65189 = ORIENTED_EDGE ( 'NONE', *, *, #59560, .T. ) ;
#65190 = AXIS2_PLACEMENT_3D ( 'NONE', #15905, #6448, #60191 ) ;
#65191 = CARTESIAN_POINT ( 'NONE',  ( 12.69999999999999574, -22.26999999999999247, -0.5000000000000004441 ) ) ;
#65193 = ORIENTED_EDGE ( 'NONE', *, *, #97046, .F. ) ;
#65192 = EDGE_CURVE ( 'NONE', #105061, #31469, #89160, .T. ) ;
#65194 = EDGE_LOOP ( 'NONE', ( #22387, #104487, #68304, #15742 ) ) ;
#65195 = AXIS2_PLACEMENT_3D ( 'NONE', #132051, #135609, #112425 ) ;
#65196 = VECTOR ( 'NONE', #57874, 1000.000000000000000 ) ;
#65197 = PLANE ( 'NONE',  #84462 ) ;
#65198 = ORIENTED_EDGE ( 'NONE', *, *, #71617, .F. ) ;
#65199 = PLANE ( 'NONE',  #64530 ) ;
#65200 = DIRECTION ( 'NONE',  ( 0.3543493200069162685, -0.000000000000000000, -0.9351131265310288487 ) ) ;
#65201 = EDGE_CURVE ( 'NONE', #133459, #93212, #138366, .T. ) ;
#65202 = AXIS2_PLACEMENT_3D ( 'NONE', #21165, #75560, #74869 ) ;
#65203 = LINE ( 'NONE', #121672, #87282 ) ;
#65204 = LINE ( 'NONE', #55743, #69211 ) ;
#65205 = VECTOR ( 'NONE', #93452, 1000.000000000000000 ) ;
#65206 = CARTESIAN_POINT ( 'NONE',  ( 119.1250000000000142, -7.950000000000000178, -4.867971026610729436E-16 ) ) ;
#65207 = ORIENTED_EDGE ( 'NONE', *, *, #54934, .T. ) ;
#65208 = CARTESIAN_POINT ( 'NONE',  ( 25.49999999999982947, 0.05218569542917231296, 5.000000000000000000 ) ) ;
#65209 = EDGE_LOOP ( 'NONE', ( #16023, #102595, #15959, #77039 ) ) ;
#65211 = EDGE_CURVE ( 'NONE', #13983, #92723, #6364, .T. ) ;
#65210 = DIRECTION ( 'NONE',  ( -0.000000000000000000, 0.3543493200069153248, 0.9351131265310292928 ) ) ;
#65212 = EDGE_LOOP ( 'NONE', ( #120692, #53253, #8429, #62564 ) ) ;
#65213 =( GEOMETRIC_REPRESENTATION_CONTEXT ( 3 ) GLOBAL_UNCERTAINTY_ASSIGNED_CONTEXT ( ( #44647 ) ) GLOBAL_UNIT_ASSIGNED_CONTEXT ( ( #58733, #85227, #107697 ) ) REPRESENTATION_CONTEXT ( 'NONE', 'WORKASPACE' ) );
#65214 = FILL_AREA_STYLE ('',( #50744 ) ) ;
#65215 = ORIENTED_EDGE ( 'NONE', *, *, #103404, .T. ) ;
#65216 = APPLICATION_CONTEXT ( 'automotive_design' ) ;
#65217 = FACE_OUTER_BOUND ( 'NONE', #59485, .T. ) ;
#65218 = ORIENTED_EDGE ( 'NONE', *, *, #53646, .T. ) ;
#65219 = EDGE_LOOP ( 'NONE', ( #24782, #515, #50458, #142054 ) ) ;
#65220 = ORIENTED_EDGE ( 'NONE', *, *, #140747, .T. ) ;
#65221 = CARTESIAN_POINT ( 'NONE',  ( -2.816011393730999401, 28.73617430169785436, 5.000000000000000000 ) ) ;
#65222 = LINE ( 'NONE', #63084, #117732 ) ;
#65223 = LINE ( 'NONE', #10088, #65750 ) ;
#65224 = CARTESIAN_POINT ( 'NONE',  ( 125.5629301918981042, 1.637169565754157174, 6.110000000000002984 ) ) ;
#65225 = DIRECTION ( 'NONE',  ( 0.6830127018922181881, 0.6830127018922202975, -0.2588190451025214056 ) ) ;
#65226 = PRODUCT_DEFINITION_SHAPE ( 'NONE', 'NONE',  #117397 ) ;
#65227 = CARTESIAN_POINT ( 'NONE',  ( 51.18398860626899705, 28.73617430169823095, 5.000000000000000000 ) ) ;
#65228 = CARTESIAN_POINT ( 'NONE',  ( -30.48921356237309510, -27.52281430457076894, 5.000000000000000000 ) ) ;
#65229 = VECTOR ( 'NONE', #29760, 1000.000000000000000 ) ;
#65230 = DIRECTION ( 'NONE',  ( 0.000000000000000000, -1.000000000000000000, 0.000000000000000000 ) ) ;
#65231 = ADVANCED_FACE ( 'NONE', ( #73131 ), #49244, .F. ) ;
#65232 = DIRECTION ( 'NONE',  ( 0.3543493200069162685, -0.000000000000000000, -0.9351131265310288487 ) ) ;
#65233 = ADVANCED_FACE ( 'NONE', ( #49946 ), #116609, .F. ) ;
#65234 = DIRECTION ( 'NONE',  ( 0.000000000000000000, -1.000000000000000000, 0.000000000000000000 ) ) ;
#65235 = DIRECTION ( 'NONE',  ( -0.7071067811865486830, -0.7071067811865464625, 0.000000000000000000 ) ) ;
#65236 = AXIS2_PLACEMENT_3D ( 'NONE', #125293, #47769, #114407 ) ;
#65237 = VERTEX_POINT ( 'NONE', #61553 ) ;
#65238 = ORIENTED_EDGE ( 'NONE', *, *, #10366, .T. ) ;
#65239 = ORIENTED_EDGE ( 'NONE', *, *, #60800, .F. ) ;
#65240 = LINE ( 'NONE', #109425, #125948 ) ;
#65241 = EDGE_LOOP ( 'NONE', ( #1874, #119300, #119668, #108424 ) ) ;
#65242 = VERTEX_POINT ( 'NONE', #91996 ) ;
#65243 = LINE ( 'NONE', #109428, #49154 ) ;
#65244 = LINE ( 'NONE', #141341, #52472 ) ;
#65245 = ADVANCED_FACE ( 'NONE', ( #28181 ), #17289, .T. ) ;
#65246 = EDGE_CURVE ( 'NONE', #8597, #49412, #81884, .T. ) ;
#65247 = LINE ( 'NONE', #142776, #108883 ) ;
#65248 = ORIENTED_EDGE ( 'NONE', *, *, #19905, .F. ) ;
#65249 = DIRECTION ( 'NONE',  ( -0.7071067811865486830, 0.7071067811865464625, 0.000000000000000000 ) ) ;
#65250 = VECTOR ( 'NONE', #74746, 999.9999999999998863 ) ;
#65251 = VERTEX_POINT ( 'NONE', #105701 ) ;
#65252 = DIRECTION ( 'NONE',  ( -0.7071067811865487940, 0.7071067811865463515, 0.000000000000000000 ) ) ;
#65253 = CARTESIAN_POINT ( 'NONE',  ( 27.70710678118635784, -18.74070752338408852, 5.000000000000000000 ) ) ;
#65254 = CARTESIAN_POINT ( 'NONE',  ( 22.52540314143522338, 2.126176841940962348, 7.934999999999989839 ) ) ;
#65255 = ORIENTED_EDGE ( 'NONE', *, *, #62906, .T. ) ;
#65256 = CARTESIAN_POINT ( 'NONE',  ( 91.64126352523143737, 4.472830434245837594, 4.472830434245841147 ) ) ;
#65257 = LINE ( 'NONE', #99249, #20426 ) ;
#65258 = CARTESIAN_POINT ( 'NONE',  ( -27.81246187583927920, -22.22500000000000142, 4.000000000000000000 ) ) ;
#65259 = CARTESIAN_POINT ( 'NONE',  ( -27.72281430457040940, -21.72500000000000142, 5.000000000000000000 ) ) ;
#65260 = VERTEX_POINT ( 'NONE', #39049 ) ;
#65261 = ORIENTED_EDGE ( 'NONE', *, *, #29552, .F. ) ;
#65262 = ORIENTED_EDGE ( 'NONE', *, *, #118769, .T. ) ;
#65263 = DIRECTION ( 'NONE',  ( 0.6830127018922181881, 0.6830127018922202975, -0.2588190451025214056 ) ) ;
#65264 = VECTOR ( 'NONE', #123015, 1000.000000000000227 ) ;
#65266 = CARTESIAN_POINT ( 'NONE',  ( -21.18398860626899349, 28.73617430169802134, 5.000000000000000000 ) ) ;
#65265 = STYLED_ITEM ( 'NONE', ( #54381 ), #131675 ) ;
#65267 = CARTESIAN_POINT ( 'NONE',  ( -26.95341186370439601, 14.25929247661557042, 18.84478104361334161 ) ) ;
#65268 = EDGE_CURVE ( 'NONE', #103666, #42327, #50639, .T. ) ;
#65270 = ORIENTED_EDGE ( 'NONE', *, *, #118073, .T. ) ;
#65269 =( BOUNDED_CURVE ( )  B_SPLINE_CURVE ( 3, ( #21771, #44258, #99299, #88471 ),
 .UNSPECIFIED., .F., .F. ) 
 B_SPLINE_CURVE_WITH_KNOTS ( ( 4, 4 ),
 ( 4.628641526727098388, 4.642507259593577018 ),
 .UNSPECIFIED. ) 
 CURVE ( )  GEOMETRIC_REPRESENTATION_ITEM ( )  RATIONAL_B_SPLINE_CURVE ( ( 1.000000000000000000, 0.9999839785185119512, 0.9999839785185119512, 1.000000000000000000 ) ) 
 REPRESENTATION_ITEM ( '' )  );
#65271 = AXIS2_PLACEMENT_3D ( 'NONE', #75913, #131017, #117943 ) ;
#65272 = DIRECTION ( 'NONE',  ( 0.000000000000000000, -1.000000000000000000, 0.000000000000000000 ) ) ;
#65273 = VECTOR ( 'NONE', #27723, 999.9999999999998863 ) ;
#65274 = DIRECTION ( 'NONE',  ( 0.7071067811865487940, -0.7071067811865463515, 0.000000000000000000 ) ) ;
#65275 = ORIENTED_EDGE ( 'NONE', *, *, #36949, .F. ) ;
#65276 = DIRECTION ( 'NONE',  ( 0.3543493200069162685, -0.000000000000000000, -0.9351131265310288487 ) ) ;
#65277 = AXIS2_PLACEMENT_3D ( 'NONE', #30902, #119299, #19984 ) ;
#65278 = VECTOR ( 'NONE', #18524, 1000.000000000000000 ) ;
#65279 = AXIS2_PLACEMENT_3D ( 'NONE', #119327, #75168, #96841 ) ;
#65280 = CARTESIAN_POINT ( 'NONE',  ( -9.183988606268997046, 28.73617430169793607, 5.000000000000000000 ) ) ;
#65281 = ORIENTED_EDGE ( 'NONE', *, *, #81633, .F. ) ;
#65283 = ORIENTED_EDGE ( 'NONE', *, *, #126761, .F. ) ;
#65282 = CARTESIAN_POINT ( 'NONE',  ( 16.73493329717938494, 12.75929247661558996, 18.34774599283952412 ) ) ;
#65284 = ORIENTED_EDGE ( 'NONE', *, *, #67451, .T. ) ;
#65285 = DIRECTION ( 'NONE',  ( -0.000000000000000000, 0.000000000000000000, 1.000000000000000000 ) ) ;
#65286 = AXIS2_PLACEMENT_3D ( 'NONE', #140048, #51610, #63908 ) ;
#65287 = CARTESIAN_POINT ( 'NONE',  ( 69.18398860626899705, 28.73617430169835529, 5.000000000000000000 ) ) ;
#65288 = ORIENTED_EDGE ( 'NONE', *, *, #55111, .F. ) ;
#65289 = CARTESIAN_POINT ( 'NONE',  ( 39.18398860626899705, 28.73617430169814568, 5.000000000000000000 ) ) ;
#65290 = DIRECTION ( 'NONE',  ( -0.7071067811865486830, -0.7071067811865464625, 0.000000000000000000 ) ) ;
#65291 = EDGE_CURVE ( 'NONE', #47857, #71793, #115861, .T. ) ;
#65292 =( NAMED_UNIT ( * ) SI_UNIT ( $, .STERADIAN. ) SOLID_ANGLE_UNIT ( ) );
#65293 = CARTESIAN_POINT ( 'NONE',  ( -32.99999999999976552, 8.587461875839160541, 4.000000000000000000 ) ) ;
#65294 = ADVANCED_FACE ( 'NONE', ( #16562 ), #60853, .F. ) ;
#65295 = CARTESIAN_POINT ( 'NONE',  ( 0.1600000000000025013, -7.946673527226693956, -0.3850431644948629772 ) ) ;
#65296 = CARTESIAN_POINT ( 'NONE',  ( 28.49999999999980815, 9.052185695429077583, 5.000000000000000000 ) ) ;
#65297 = CARTESIAN_POINT ( 'NONE',  ( 48.48921356237309510, -27.52281430457089328, 5.000000000000000000 ) ) ;
#65298 = DIRECTION ( 'NONE',  ( -0.7071067811865486830, -0.7071067811865464625, -0.000000000000000000 ) ) ;
#65299 = DIRECTION ( 'NONE',  ( 0.7071067811865487940, 0.7071067811865463515, 0.000000000000000000 ) ) ;
#65300 = DIRECTION ( 'NONE',  ( 0.6830127018922181881, 0.6830127018922202975, -0.2588190451025214056 ) ) ;
#65301 = LINE ( 'NONE', #64556, #27498 ) ;
#65302 = CARTESIAN_POINT ( 'NONE',  ( -1.998069433179001653, -22.22500000000000142, 4.500000000000000888 ) ) ;
#65304 = EDGE_CURVE ( 'NONE', #57105, #66501, #94826, .T. ) ;
#65303 = CARTESIAN_POINT ( 'NONE',  ( -45.18398860626900415, 28.73617430169818832, 5.000000000000000000 ) ) ;
#65306 = EDGE_CURVE ( 'NONE', #37520, #126076, #92702, .T. ) ;
#65305 = EDGE_LOOP ( 'NONE', ( #67285, #90050, #37074, #45509 ) ) ;
#65307 = VECTOR ( 'NONE', #78046, 1000.000000000000000 ) ;
#65308 = VERTEX_POINT ( 'NONE', #37646 ) ;
#65309 = ORIENTED_EDGE ( 'NONE', *, *, #23737, .T. ) ;
#65310 = CARTESIAN_POINT ( 'NONE',  ( 105.2708333333333286, -7.949999999999999289, -2.130196079827426203 ) ) ;
#65311 = VECTOR ( 'NONE', #113454, 999.9999999999998863 ) ;
#65312 = ORIENTED_EDGE ( 'NONE', *, *, #102066, .F. ) ;
#65313 = ORIENTED_EDGE ( 'NONE', *, *, #69348, .T. ) ;
#65314 = AXIS2_PLACEMENT_3D ( 'NONE', #85513, #139232, #62381 ) ;
#65315 = ORIENTED_EDGE ( 'NONE', *, *, #53095, .F. ) ;
#65316 = DIRECTION ( 'NONE',  ( 0.3543493200069162685, -0.000000000000000000, -0.9351131265310288487 ) ) ;
#65317 = CARTESIAN_POINT ( 'NONE',  ( 89.52083333333332860, 7.949999999999998401, 2.130196079827431532 ) ) ;
#65318 = VECTOR ( 'NONE', #136425, 1000.000000000000000 ) ;
#65319 = ORIENTED_EDGE ( 'NONE', *, *, #102066, .T. ) ;
#65320 = CARTESIAN_POINT ( 'NONE',  ( 23.99999999999983302, 20.96639925780204550, 5.000000000000000000 ) ) ;
#65321 = DIRECTION ( 'NONE',  ( 0.000000000000000000, 0.000000000000000000, -1.000000000000000000 ) ) ;
#65322 = ADVANCED_FACE ( 'NONE', ( #26743 ), #139091, .T. ) ;
#65323 = LINE ( 'NONE', #98618, #30176 ) ;
#65324 = FACE_OUTER_BOUND ( 'NONE', #137110, .T. ) ;
#65325 = EDGE_LOOP ( 'NONE', ( #15308, #32469, #50044, #132250 ) ) ;
#65326 = ADVANCED_FACE ( 'NONE', ( #9223 ), #75966, .F. ) ;
#65327 = CARTESIAN_POINT ( 'NONE',  ( 2.335353848949925037, 12.43939446707911678, -26.87120046541300766 ) ) ;
#65328 = PLANE ( 'NONE',  #33512 ) ;
#65329 = DIRECTION ( 'NONE',  ( -0.7071067811865486830, -0.7071067811865464625, -0.000000000000000000 ) ) ;
#65331 = VECTOR ( 'NONE', #110444, 1000.000000000000000 ) ;
#65330 = LINE ( 'NONE', #42142, #49884 ) ;
#65332 = CARTESIAN_POINT ( 'NONE',  ( 22.89583333333333570, 1.633150327867706864, -6.094999999999981100 ) ) ;
#65333 = DIRECTION ( 'NONE',  ( -0.7071067811865486830, -0.7071067811865464625, -0.000000000000000000 ) ) ;
#65334 = CARTESIAN_POINT ( 'NONE',  ( 29.68336038379622366, -2.130196079827426203, 7.949999999999997513 ) ) ;
#65335 = EDGE_CURVE ( 'NONE', #32425, #131572, #131060, .T. ) ;
#65336 = LINE ( 'NONE', #89896, #63140 ) ;
#65337 = VERTEX_POINT ( 'NONE', #120139 ) ;
#65338 = ORIENTED_EDGE ( 'NONE', *, *, #100318, .F. ) ;
#65339 = CARTESIAN_POINT ( 'NONE',  ( 121.3337635252314328, 6.110000000000001208, 1.122388791418549305E-15 ) ) ;
#65340 = ORIENTED_EDGE ( 'NONE', *, *, #107225, .T. ) ;
#65341 = DIRECTION ( 'NONE',  ( 0.7071067811865487940, -0.7071067811865463515, 0.000000000000000000 ) ) ;
#65342 = AXIS2_PLACEMENT_3D ( 'NONE', #13049, #82614, #49301 ) ;
#65343 = CARTESIAN_POINT ( 'NONE',  ( -21.32816939922338406, -9.740707523384182664, 4.000000000000000000 ) ) ;
#65344 = EDGE_CURVE ( 'NONE', #40790, #143444, #53503, .T. ) ;
#65345 = AXIS2_PLACEMENT_3D ( 'NONE', #52768, #118002, #20140 ) ;
#65346 = CARTESIAN_POINT ( 'NONE',  ( 3.046588136295422355, 14.25929247661557042, 18.84478104361327055 ) ) ;
#65347 = DIRECTION ( 'NONE',  ( 0.000000000000000000, -1.000000000000000000, 0.000000000000000000 ) ) ;
#65348 = FACE_OUTER_BOUND ( 'NONE', #5722, .T. ) ;
#65349 = CARTESIAN_POINT ( 'NONE',  ( -10.00193056682090997, -22.22500000000000142, 4.500000000000000888 ) ) ;
#65350 = CARTESIAN_POINT ( 'NONE',  ( 124.0162635252314658, -4.472830434245839371, 4.472830434245839371 ) ) ;
#65351 = ORIENTED_EDGE ( 'NONE', *, *, #82209, .F. ) ;
#65352 = VERTEX_POINT ( 'NONE', #31747 ) ;
#65353 = EDGE_CURVE ( 'NONE', #6537, #72772, #51370, .T. ) ;
#65354 = VECTOR ( 'NONE', #54402, 1000.000000000000000 ) ;
#65355 = LINE ( 'NONE', #21814, #50817 ) ;
#65356 = CARTESIAN_POINT ( 'NONE',  ( 24.70710678118637560, -15.74070752338411339, 5.000000000000000000 ) ) ;
#65357 = ORIENTED_EDGE ( 'NONE', *, *, #14184, .T. ) ;
#65358 = CARTESIAN_POINT ( 'NONE',  ( 42.43793019189809712, -6.110000000000001208, 1.637169565754158951 ) ) ;
#65359 = ORIENTED_EDGE ( 'NONE', *, *, #18454, .F. ) ;
#65360 = CARTESIAN_POINT ( 'NONE',  ( 0.000000000000000000, 0.000000000000000000, 5.000000000000000000 ) ) ;
#65361 = CARTESIAN_POINT ( 'NONE',  ( 34.92499999999998295, 3.207916084809844914, -2.206283991393068966 ) ) ;
#65362 = EDGE_CURVE ( 'NONE', #124820, #6035, #99918, .T. ) ;
#65363 = CARTESIAN_POINT ( 'NONE',  ( 7.637538124160930586, 22.22500000000000142, 4.000000000000000000 ) ) ;
#65364 = VECTOR ( 'NONE', #75639, 999.9999999999998863 ) ;
#65365 = EDGE_CURVE ( 'NONE', #70306, #126386, #141205, .T. ) ;
#65366 = CARTESIAN_POINT ( 'NONE',  ( 37.39126352523143737, -4.472830434245839371, -4.472830434245839371 ) ) ;
#65367 = VERTEX_POINT ( 'NONE', #52073 ) ;
#65368 = LINE ( 'NONE', #109547, #78020 ) ;
#65369 = ORIENTED_EDGE ( 'NONE', *, *, #47815, .F. ) ;
#65370 = VERTEX_POINT ( 'NONE', #52762 ) ;
#65371 = AXIS2_PLACEMENT_3D ( 'NONE', #44616, #111227, #11919 ) ;
#65372 = AXIS2_PLACEMENT_3D ( 'NONE', #96745, #70952, #40986 ) ;
#65373 = ORIENTED_EDGE ( 'NONE', *, *, #80644, .F. ) ;
#65374 = AXIS2_PLACEMENT_3D ( 'NONE', #36276, #89228, #122545 ) ;
#65375 = CIRCLE ( 'NONE', #2823, 4.999999999999998224 ) ;
#65376 = DIRECTION ( 'NONE',  ( -0.6830127018922181881, 0.6830127018922202975, -0.2588190451025214056 ) ) ;
#65377 = ORIENTED_EDGE ( 'NONE', *, *, #121256, .F. ) ;
#65378 = DIRECTION ( 'NONE',  ( 0.000000000000000000, -1.000000000000000000, 0.000000000000000000 ) ) ;
#65379 = EDGE_CURVE ( 'NONE', #143546, #3467, #19436, .T. ) ;
#65380 = AXIS2_PLACEMENT_3D ( 'NONE', #122706, #103110, #12513 ) ;
#65381 = VECTOR ( 'NONE', #108934, 1000.000000000000000 ) ;
#65382 = MECHANICAL_DESIGN_GEOMETRIC_PRESENTATION_REPRESENTATION (  '', ( #134819 ), #95456 ) ;
#65383 = DIRECTION ( 'NONE',  ( 0.3543493200069162685, -0.000000000000000000, -0.9351131265310288487 ) ) ;
#65384 = CARTESIAN_POINT ( 'NONE',  ( -20.99999999999984723, -6.033600742197678279, 5.000000000000000000 ) ) ;
#65385 = FACE_BOUND ( 'NONE', #46581, .T. ) ;
#65386 = ORIENTED_EDGE ( 'NONE', *, *, #63364, .T. ) ;
#65387 = DIRECTION ( 'NONE',  ( -0.7071067811865486830, -0.7071067811865464625, 0.000000000000000000 ) ) ;
#65388 = EDGE_CURVE ( 'NONE', #87654, #9178, #96952, .T. ) ;
#65389 = CARTESIAN_POINT ( 'NONE',  ( 3.062159117892259808, -48.47815212813054586, 38.14157743968410585 ) ) ;
#65390 = DIRECTION ( 'NONE',  ( 0.7071067811865487940, 0.7071067811865463515, 0.000000000000000000 ) ) ;
#65391 = ORIENTED_EDGE ( 'NONE', *, *, #59709, .T. ) ;
#65392 = CARTESIAN_POINT ( 'NONE',  ( 20.18753812416037974, -22.22500000000000142, 4.000000000000000000 ) ) ;
#65393 = ORIENTED_EDGE ( 'NONE', *, *, #22680, .T. ) ;
#65394 = ORIENTED_EDGE ( 'NONE', *, *, #10204, .F. ) ;
#65395 = DIRECTION ( 'NONE',  ( 0.000000000000000000, -1.000000000000000000, 0.000000000000000000 ) ) ;
#65396 = ORIENTED_EDGE ( 'NONE', *, *, #133515, .T. ) ;
#65397 = CARTESIAN_POINT ( 'NONE',  ( 44.82876352523145158, 0.000000000000000000, -6.109999999999998543 ) ) ;
#65398 = ORIENTED_EDGE ( 'NONE', *, *, #33594, .F. ) ;
#65399 = FACE_OUTER_BOUND ( 'NONE', #79740, .T. ) ;
#65400 = LINE ( 'NONE', #59, #54299 ) ;
#65401 = DIRECTION ( 'NONE',  ( 0.000000000000000000, -1.000000000000000000, 0.000000000000000000 ) ) ;
#65402 = EDGE_LOOP ( 'NONE', ( #112806, #5652, #139182, #54243 ) ) ;
#65403 = CARTESIAN_POINT ( 'NONE',  ( 34.75611968250419892, -4.294349301475905101, 4.955485411084876723 ) ) ;
#65404 = CIRCLE ( 'NONE', #137210, 6.349999999999997868 ) ;
#65405 = DIRECTION ( 'NONE',  ( 0.7071067811865486830, -0.7071067811865464625, -0.000000000000000000 ) ) ;
#65406 = DIRECTION ( 'NONE',  ( 0.000000000000000000, 0.000000000000000000, -1.000000000000000000 ) ) ;
#65407 = ADVANCED_FACE ( 'NONE', ( #18697 ), #141202, .F. ) ;
#65408 = LINE ( 'NONE', #99397, #87621 ) ;
#65409 = VECTOR ( 'NONE', #13482, 1000.000000000000000 ) ;
#65410 = LINE ( 'NONE', #142935, #142041 ) ;
#65411 = FACE_OUTER_BOUND ( 'NONE', #33654, .T. ) ;
#65412 = VERTEX_POINT ( 'NONE', #73822 ) ;
#65413 = ORIENTED_EDGE ( 'NONE', *, *, #53739, .T. ) ;
#65414 = ORIENTED_EDGE ( 'NONE', *, *, #140438, .F. ) ;
#65415 = STYLED_ITEM ( 'NONE', ( #105059 ), #62206 ) ;
#65416 = DIRECTION ( 'NONE',  ( 0.7071067811865487940, -0.7071067811865463515, 0.000000000000000000 ) ) ;
#65417 = FACE_OUTER_BOUND ( 'NONE', #88326, .T. ) ;
#65418 = ORIENTED_EDGE ( 'NONE', *, *, #16223, .T. ) ;
#65419 = VERTEX_POINT ( 'NONE', #130360 ) ;
#65420 = CARTESIAN_POINT ( 'NONE',  ( 0.000000000000000000, 0.000000000000000000, 0.000000000000000000 ) ) ;
#65421 = LINE ( 'NONE', #108857, #119700 ) ;
#65422 = ADVANCED_FACE ( 'NONE', ( #117994 ), #95563, .F. ) ;
#65423 = ADVANCED_FACE ( 'NONE', ( #9982 ), #54250, .F. ) ;
#65424 = CARTESIAN_POINT ( 'NONE',  ( 15.32816939922342847, -3.740707523384238176, 4.000000000000000000 ) ) ;
#65425 = ORIENTED_EDGE ( 'NONE', *, *, #42528, .F. ) ;
#65426 = CARTESIAN_POINT ( 'NONE',  ( 13.64840764549667540, 9.139736423841732040E-16, 0.000000000000000000 ) ) ;
#65427 = CARTESIAN_POINT ( 'NONE',  ( -3.838293875473783423, -6.740707523384212863, 16.75550250614866599 ) ) ;
#65428 = CARTESIAN_POINT ( 'NONE',  ( 20.92123647476855197, -9.717572351234235426E-16, -7.934999999999990727 ) ) ;
#65429 = LINE ( 'NONE', #42953, #78561 ) ;
#65430 = ORIENTED_EDGE ( 'NONE', *, *, #97066, .T. ) ;
#65431 = CARTESIAN_POINT ( 'NONE',  ( 118.3287635252314658, 0.000000000000000000, -6.109999999999999432 ) ) ;
#65432 =( BOUNDED_CURVE ( )  B_SPLINE_CURVE ( 3, ( #111662, #55874, #135565, #1433 ),
 .UNSPECIFIED., .F., .T. ) 
 B_SPLINE_CURVE_WITH_KNOTS ( ( 4, 4 ),
 ( 5.920967161967927161, 7.341195215986585865 ),
 .UNSPECIFIED. ) 
 CURVE ( )  GEOMETRIC_REPRESENTATION_ITEM ( )  RATIONAL_B_SPLINE_CURVE ( ( 1.000000000000000000, 0.8388583629366725969, 0.8388583629366725969, 1.000000000000000000 ) ) 
 REPRESENTATION_ITEM ( '' )  );
#65433 = EDGE_CURVE ( 'NONE', #111218, #79059, #86132, .T. ) ;
#65434 = LINE ( 'NONE', #92, #14115 ) ;
#65435 = VECTOR ( 'NONE', #33793, 1000.000000000000000 ) ;
#65436 = CARTESIAN_POINT ( 'NONE',  ( 18.18398860626898994, 28.73617430169800002, 5.000000000000000000 ) ) ;
#65438 = ORIENTED_EDGE ( 'NONE', *, *, #77651, .F. ) ;
#65437 = LINE ( 'NONE', #141545, #102740 ) ;
#65440 = AXIS2_PLACEMENT_3D ( 'NONE', #26591, #81717, #82410 ) ;
#65439 = DIRECTION ( 'NONE',  ( 0.7071067811865486830, -0.7071067811865464625, -0.000000000000000000 ) ) ;
#65441 = EDGE_LOOP ( 'NONE', ( #85850, #65061, #107955 ) ) ;
#65442 = DIRECTION ( 'NONE',  ( 0.7071067811865486830, -0.7071067811865464625, -0.000000000000000000 ) ) ;
#65443 = DIRECTION ( 'NONE',  ( -0.3543493200069162685, -0.000000000000000000, -0.9351131265310288487 ) ) ;
#65444 = DIRECTION ( 'NONE',  ( -0.7071067811865486830, 0.7071067811865464625, 0.000000000000000000 ) ) ;
#65445 = EDGE_CURVE ( 'NONE', #55968, #91497, #140490, .T. ) ;
#65446 = ORIENTED_EDGE ( 'NONE', *, *, #107199, .F. ) ;
#65447 = CARTESIAN_POINT ( 'NONE',  ( 77.99451991528749772, 28.92564299267992567, 4.000000000000000000 ) ) ;
#65448 = CARTESIAN_POINT ( 'NONE',  ( 0.2997448713915885632, -27.71228299555206220, 4.000000000000000000 ) ) ;
#65449 = EDGE_LOOP ( 'NONE', ( #141520, #45862, #106020, #107986 ) ) ;
#65450 = ADVANCED_FACE ( 'NONE', ( #119436 ), #74554, .F. ) ;
#65451 = VECTOR ( 'NONE', #85103, 1000.000000000000000 ) ;
#65452 = CARTESIAN_POINT ( 'NONE',  ( 14.70692117890024697, -2.500000000000000444, 3.061616997868384127E-16 ) ) ;
#65453 = DIRECTION ( 'NONE',  ( -0.000000000000000000, 0.3543493200069153248, 0.9351131265310292928 ) ) ;
#65454 = VERTEX_POINT ( 'NONE', #30315 ) ;
#65456 = ORIENTED_EDGE ( 'NONE', *, *, #106284, .T. ) ;
#65455 = CARTESIAN_POINT ( 'NONE',  ( 0.000000000000000000, 0.000000000000000000, 5.000000000000000000 ) ) ;
#65457 = EDGE_LOOP ( 'NONE', ( #141082, #10356, #12865, #97638, #25694 ) ) ;
#65458 = VECTOR ( 'NONE', #103606, 1000.000000000000227 ) ;
#65459 = DIRECTION ( 'NONE',  ( -1.000000000000000000, -0.000000000000000000, -0.000000000000000000 ) ) ;
#65460 = CARTESIAN_POINT ( 'NONE',  ( 29.99999999999979394, -3.485240976185050243, -4.108735105802328036 ) ) ;
#65461 =( BOUNDED_CURVE ( )  B_SPLINE_CURVE ( 3, ( #77209, #31538, #98224, #61516 ),
 .UNSPECIFIED., .F., .F. ) 
 B_SPLINE_CURVE_WITH_KNOTS ( ( 4, 4 ),
 ( 5.920967161967927161, 7.341195215986588529 ),
 .UNSPECIFIED. ) 
 CURVE ( )  GEOMETRIC_REPRESENTATION_ITEM ( )  RATIONAL_B_SPLINE_CURVE ( ( 1.000000000000000000, 0.8388583629366720418, 0.8388583629366720418, 1.000000000000000000 ) ) 
 REPRESENTATION_ITEM ( '' )  );
#65462 = VERTEX_POINT ( 'NONE', #108545 ) ;
#65463 = LINE ( 'NONE', #21917, #45973 ) ;
#65464 = DIRECTION ( 'NONE',  ( -0.7071067811865486830, 0.7071067811865464625, 0.000000000000000000 ) ) ;
#65465 = CARTESIAN_POINT ( 'NONE',  ( 7.499999999999948486, 15.43112307739203182, 4.000000000000000000 ) ) ;
#65466 = ORIENTED_EDGE ( 'NONE', *, *, #88190, .F. ) ;
#65467 = ADVANCED_FACE ( 'NONE', ( #35347 ), #54939, .F. ) ;
#65468 = DIRECTION ( 'NONE',  ( -1.000000000000000000, -0.000000000000000000, -0.000000000000000000 ) ) ;
#65469 = LINE ( 'NONE', #19779, #95305 ) ;
#65470 = LINE ( 'NONE', #54580, #91054 ) ;
#65471 = VECTOR ( 'NONE', #79192, 1000.000000000000000 ) ;
#65472 = PRESENTATION_STYLE_ASSIGNMENT (( #99463 ) ) ;
#65473 = CARTESIAN_POINT ( 'NONE',  ( 38.26626352523144448, 4.472830434245839371, -4.472830434245839371 ) ) ;
#65474 = CARTESIAN_POINT ( 'NONE',  ( 0.1839886062690032631, 28.73617430169787568, 5.000000000000000000 ) ) ;
#65475 = ADVANCED_FACE ( 'NONE', ( #44059 ), #25132, .F. ) ;
#65477 = EDGE_CURVE ( 'NONE', #47195, #22650, #33216, .T. ) ;
#65476 = VECTOR ( 'NONE', #107479, 1000.000000000000227 ) ;
#65478 = AXIS2_PLACEMENT_3D ( 'NONE', #61156, #105304, #5960 ) ;
#65479 = ORIENTED_EDGE ( 'NONE', *, *, #59713, .T. ) ;
#65480 = EDGE_LOOP ( 'NONE', ( #91143, #17442, #111815, #403 ) ) ;
#65481 = VERTEX_POINT ( 'NONE', #88280 ) ;
#65482 = ORIENTED_EDGE ( 'NONE', *, *, #141493, .F. ) ;
#65483 = MECHANICAL_DESIGN_GEOMETRIC_PRESENTATION_REPRESENTATION (  '', ( #130022 ), #26128 ) ;
#65484 = VECTOR ( 'NONE', #106266, 1000.000000000000227 ) ;
#65485 = DIRECTION ( 'NONE',  ( 0.3543493200069162685, -0.000000000000000000, -0.9351131265310288487 ) ) ;
#65486 =( GEOMETRIC_REPRESENTATION_CONTEXT ( 3 ) GLOBAL_UNCERTAINTY_ASSIGNED_CONTEXT ( ( #22770 ) ) GLOBAL_UNIT_ASSIGNED_CONTEXT ( ( #123847, #24501, #48398 ) ) REPRESENTATION_CONTEXT ( 'NONE', 'WORKASPACE' ) );
#65487 = PLANE ( 'NONE',  #122700 ) ;
#65488 = EDGE_CURVE ( 'NONE', #118275, #35117, #78838, .T. ) ;
#65489 = VERTEX_POINT ( 'NONE', #99110 ) ;
#65490 = FACE_OUTER_BOUND ( 'NONE', #142355, .T. ) ;
#65491 = CARTESIAN_POINT ( 'NONE',  ( 2.816011393730999401, 28.73617430169785436, 5.000000000000000000 ) ) ;
#65492 = EDGE_CURVE ( 'NONE', #36317, #53631, #80273, .T. ) ;
#65493 = CARTESIAN_POINT ( 'NONE',  ( 83.24999999999998579, -9.735942053221458872E-16, 7.950000000000000178 ) ) ;
#65494 = LINE ( 'NONE', #51021, #33822 ) ;
#65495 = ORIENTED_EDGE ( 'NONE', *, *, #105507, .F. ) ;
#65496 = EDGE_CURVE ( 'NONE', #52878, #106919, #335, .T. ) ;
#65497 = LINE ( 'NONE', #98095, #27922 ) ;
#65498 = DIRECTION ( 'NONE',  ( -0.7071067811865486830, -0.7071067811865464625, -0.000000000000000000 ) ) ;
#65499 = DIRECTION ( 'NONE',  ( -0.7071067811865486830, -0.7071067811865464625, 0.000000000000000000 ) ) ;
#65500 = CARTESIAN_POINT ( 'NONE',  ( 0.1600000000000011136, 3.289720434613005118, -7.220939306079887210 ) ) ;
#65501 = LINE ( 'NONE', #23371, #12674 ) ;
#65502 = CARTESIAN_POINT ( 'NONE',  ( 20.65000000000000213, 7.776507174585702024E-16, -6.350000000000008527 ) ) ;
#65503 = CARTESIAN_POINT ( 'NONE',  ( 7.326124847093153925, 2.055000000000001048, 2.516649172247811554E-16 ) ) ;
#65504 = CARTESIAN_POINT ( 'NONE',  ( 55.35002705046288440, -5.819803920172572198, -5.819803920172572198 ) ) ;
#65505 =( BOUNDED_CURVE ( )  B_SPLINE_CURVE ( 3, ( #50923, #48785, #92990, #136483 ),
 .UNSPECIFIED., .F., .T. ) 
 B_SPLINE_CURVE_WITH_KNOTS ( ( 4, 4 ),
 ( 4.350170835173029715, 4.500739107949259576 ),
 .UNSPECIFIED. ) 
 CURVE ( )  GEOMETRIC_REPRESENTATION_ITEM ( )  RATIONAL_B_SPLINE_CURVE ( ( 1.000000000000000000, 0.9981116584018945304, 0.9981116584018945304, 1.000000000000000000 ) ) 
 REPRESENTATION_ITEM ( '' )  );
#65506 = DIRECTION ( 'NONE',  ( -0.3543493200069162685, -0.000000000000000000, -0.9351131265310288487 ) ) ;
#65507 = EDGE_CURVE ( 'NONE', #38910, #18696, #132529, .T. ) ;
#65509 = CARTESIAN_POINT ( 'NONE',  ( 36.18398860626899705, 28.73617430169812437, 5.000000000000000000 ) ) ;
#65508 = AXIS2_PLACEMENT_3D ( 'NONE', #104650, #61217, #14793 ) ;
#65510 = ORIENTED_EDGE ( 'NONE', *, *, #1464, .T. ) ;
#65511 = ORIENTED_EDGE ( 'NONE', *, *, #30459, .F. ) ;
#65512 = CARTESIAN_POINT ( 'NONE',  ( 49.27083333333333570, -7.949999999999999289, -2.130196079827426203 ) ) ;
#65513 = EDGE_CURVE ( 'NONE', #13150, #119701, #46223, .T. ) ;
#65514 = LINE ( 'NONE', #119131, #67074 ) ;
#65515 = DIRECTION ( 'NONE',  ( -0.6830127018922181881, 0.6830127018922202975, -0.2588190451025214056 ) ) ;
#65516 = VERTEX_POINT ( 'NONE', #110005 ) ;
#65517 = EDGE_CURVE ( 'NONE', #123774, #118884, #112862, .T. ) ;
#65518 = PLANE ( 'NONE',  #105706 ) ;
#65519 = AXIS2_PLACEMENT_3D ( 'NONE', #59355, #135477, #102126 ) ;
#65520 = DIRECTION ( 'NONE',  ( 1.000000000000000000, 0.000000000000000000, 0.000000000000000000 ) ) ;
#65521 = CARTESIAN_POINT ( 'NONE',  ( 47.97959685856477563, 6.109999999999999432, 1.637169565754164280 ) ) ;
#65522 = VECTOR ( 'NONE', #49748, 1000.000000000000000 ) ;
#65523 = ORIENTED_EDGE ( 'NONE', *, *, #90688, .F. ) ;
#65524 = FILL_AREA_STYLE ('',( #76369 ) ) ;
#65525 = ORIENTED_EDGE ( 'NONE', *, *, #116602, .T. ) ;
#65526 = EDGE_LOOP ( 'NONE', ( #63288, #133285, #24226, #104301 ) ) ;
#65527 = EDGE_CURVE ( 'NONE', #59092, #24092, #22260, .T. ) ;
#65528 = VECTOR ( 'NONE', #57853, 1000.000000000000000 ) ;
#65529 = PLANE ( 'NONE',  #137215 ) ;
#65530 = CARTESIAN_POINT ( 'NONE',  ( 18.53421140649331633, 9.121673282332597665, 4.000000000000000000 ) ) ;
#65531 = CARTESIAN_POINT ( 'NONE',  ( 42.48921356237308800, -27.52281430457085065, 5.000000000000000000 ) ) ;
#65532 = CARTESIAN_POINT ( 'NONE',  ( 0.000000000000000000, 0.000000000000000000, 5.000000000000000000 ) ) ;
#65533 = VERTEX_POINT ( 'NONE', #102000 ) ;
#65534 = DIRECTION ( 'NONE',  ( -0.000000000000000000, 0.000000000000000000, 1.000000000000000000 ) ) ;
#65535 = LINE ( 'NONE', #121293, #106649 ) ;
#65537 = VERTEX_POINT ( 'NONE', #110694 ) ;
#65536 = CARTESIAN_POINT ( 'NONE',  ( 0.000000000000000000, 0.000000000000000000, 5.000000000000000000 ) ) ;
#65538 = CARTESIAN_POINT ( 'NONE',  ( 78.75043019189810423, 3.055000000000002824, -5.291415217122919401 ) ) ;
#65539 = DIRECTION ( 'NONE',  ( 0.7071067811865486830, -0.7071067811865464625, -0.000000000000000000 ) ) ;
#65540 = FACE_OUTER_BOUND ( 'NONE', #85053, .T. ) ;
#65541 = LINE ( 'NONE', #19836, #79661 ) ;
#65542 = EDGE_CURVE ( 'NONE', #70976, #97364, #124463, .T. ) ;
#65543 = CARTESIAN_POINT ( 'NONE',  ( 0.000000000000000000, 0.000000000000000000, 7.950000000000000178 ) ) ;
#65544 = CARTESIAN_POINT ( 'NONE',  ( 10.49999999999993250, -4.796895815301006394, -3.611700055028658429 ) ) ;
#65545 = CONICAL_SURFACE ( 'NONE', #88703, 2.500000000000000888, 0.9599310885968822538 ) ;
#65546 = EDGE_CURVE ( 'NONE', #108369, #108304, #122296, .T. ) ;
#65547 = ORIENTED_EDGE ( 'NONE', *, *, #82626, .F. ) ;
#65548 = CARTESIAN_POINT ( 'NONE',  ( 87.87086038379622721, 6.884901960086289741, -3.974999999999993427 ) ) ;
#65549 = CARTESIAN_POINT ( 'NONE',  ( 67.72459685856478018, -1.637169565754160949, 6.109999999999997655 ) ) ;
#65550 = DIRECTION ( 'NONE',  ( -1.000000000000000000, -1.224606353822377258E-16, -0.000000000000000000 ) ) ;
#65551 = TOROIDAL_SURFACE ( 'NONE', #132706, 2.500000000000000000, 0.5000000000000000000 ) ;
#65552 = CARTESIAN_POINT ( 'NONE',  ( -4.580140136459718292, -22.22500000000000142, 16.49880175272448568 ) ) ;
#65553 = PLANE ( 'NONE',  #24688 ) ;
#65554 = EDGE_LOOP ( 'NONE', ( #119885, #130054, #56928, #103911 ) ) ;
#65555 = ORIENTED_EDGE ( 'NONE', *, *, #124037, .F. ) ;
#65556 = CARTESIAN_POINT ( 'NONE',  ( 48.48921356237309510, -27.52281430457089328, 5.000000000000000000 ) ) ;
#65558 = ADVANCED_FACE ( 'NONE', ( #133225 ), #9656, .T. ) ;
#65557 = DIRECTION ( 'NONE',  ( -0.000000000000000000, -0.3543493200069152693, 0.9351131265310292928 ) ) ;
#65559 = VERTEX_POINT ( 'NONE', #55654 ) ;
#65560 = VERTEX_POINT ( 'NONE', #89688 ) ;
#65561 = CARTESIAN_POINT ( 'NONE',  ( -39.48921356237310221, -27.52281430457082934, 5.000000000000000000 ) ) ;
#65562 = ORIENTED_EDGE ( 'NONE', *, *, #50992, .T. ) ;
#65563 = DIRECTION ( 'NONE',  ( 0.7071067811865487940, -0.7071067811865463515, 0.000000000000000000 ) ) ;
#65564 = CARTESIAN_POINT ( 'NONE',  ( -20.67183060077633527, -9.740707523384180888, 4.000000000000000000 ) ) ;
#65565 = CARTESIAN_POINT ( 'NONE',  ( 42.18398860626899705, 28.73617430169816700, 5.000000000000000000 ) ) ;
#65566 = AXIS2_PLACEMENT_3D ( 'NONE', #134538, #36619, #2545 ) ;
#65567 = DIRECTION ( 'NONE',  ( 0.6830127018922180770, -0.6830127018922204085, -0.2588190451025213501 ) ) ;
#65568 = FACE_BOUND ( 'NONE', #142186, .T. ) ;
#65569 = CARTESIAN_POINT ( 'NONE',  ( -25.49999999999982592, -8.568876922607724822, 4.000000000000000000 ) ) ;
#65570 = CARTESIAN_POINT ( 'NONE',  ( 41.64169371712954870, -2.130196079827424871, -7.949999999999998401 ) ) ;
#65571 = AXIS2_PLACEMENT_3D ( 'NONE', #65881, #54981, #131100 ) ;
#65572 = CARTESIAN_POINT ( 'NONE',  ( 0.000000000000000000, 0.000000000000000000, 5.000000000000000000 ) ) ;
#65574 = ORIENTED_EDGE ( 'NONE', *, *, #2027, .F. ) ;
#65573 = CARTESIAN_POINT ( 'NONE',  ( 51.26669371712954870, -7.949999999999998401, 2.130196079827423983 ) ) ;
#65575 = CARTESIAN_POINT ( 'NONE',  ( 35.99451991528749772, 28.92564299267963079, 4.000000000000000000 ) ) ;
#65576 = ITEM_DEFINED_TRANSFORMATION ( 'NONE', 'NONE', #95648,  #127880 ) ;
#65577 = VERTEX_POINT ( 'NONE', #33901 ) ;
#65578 = ORIENTED_EDGE ( 'NONE', *, *, #6028, .F. ) ;
#65579 = CARTESIAN_POINT ( 'NONE',  ( 89.01626352523143737, -4.472830434245838482, 4.472830434245838482 ) ) ;
#65580 = ORIENTED_EDGE ( 'NONE', *, *, #69041, .F. ) ;
#65581 = PLANE ( 'NONE',  #1307 ) ;
#65582 = CARTESIAN_POINT ( 'NONE',  ( 34.42499999999998295, 22.22500000000000142, 5.000000000000000000 ) ) ;
#65583 = EDGE_CURVE ( 'NONE', #19566, #47325, #22969, .T. ) ;
#65584 = ORIENTED_EDGE ( 'NONE', *, *, #7092, .F. ) ;
#65585 = LINE ( 'NONE', #101012, #123160 ) ;
#65586 = VECTOR ( 'NONE', #129784, 1000.000000000000227 ) ;
#65587 = AXIS2_PLACEMENT_3D ( 'NONE', #63961, #74859, #107442 ) ;
#65588 = LINE ( 'NONE', #98180, #56448 ) ;
#65589 = PLANE ( 'NONE',  #71580 ) ;
#65590 = DIRECTION ( 'NONE',  ( 0.000000000000000000, 1.000000000000000000, 0.000000000000000000 ) ) ;
#65591 = LINE ( 'NONE', #64845, #113030 ) ;
#65592 = DIRECTION ( 'NONE',  ( -0.6830127018922180770, -0.6830127018922204085, -0.2588190451025213501 ) ) ;
#65593 = CARTESIAN_POINT ( 'NONE',  ( -24.78162688292477256, 21.74787736706806385, 4.999607392498049308 ) ) ;
#65594 = FACE_OUTER_BOUND ( 'NONE', #131932, .T. ) ;
#65595 = ORIENTED_EDGE ( 'NONE', *, *, #58628, .F. ) ;
#65596 = AXIS2_PLACEMENT_3D ( 'NONE', #27691, #50185, #105947 ) ;
#65597 = PRESENTATION_LAYER_ASSIGNMENT (  '', '', ( #7688 ) ) ;
#65598 = DIRECTION ( 'NONE',  ( -0.7071067811865486830, -0.7071067811865464625, 0.000000000000000000 ) ) ;
#65599 = ORIENTED_EDGE ( 'NONE', *, *, #97649, .T. ) ;
#65600 = DIRECTION ( 'NONE',  ( -0.6830127018922181881, 0.6830127018922202975, -0.2588190451025214056 ) ) ;
#65601 = FILL_AREA_STYLE ('',( #11130 ) ) ;
#65602 = EDGE_CURVE ( 'NONE', #71954, #80946, #12118, .T. ) ;
#65603 = ORIENTED_EDGE ( 'NONE', *, *, #67377, .T. ) ;
#65604 = ORIENTED_EDGE ( 'NONE', *, *, #112311, .T. ) ;
#65605 = ADVANCED_FACE ( 'NONE', ( #90404 ), #34605, .F. ) ;
#65606 = CARTESIAN_POINT ( 'NONE',  ( 32.95876352523143282, 0.000000000000000000, -6.110000000000001208 ) ) ;
#65607 = EDGE_LOOP ( 'NONE', ( #19485, #52501, #126822, #74045 ) ) ;
#65608 = CARTESIAN_POINT ( 'NONE',  ( 12.18398860626900060, 28.73617430169795739, 5.000000000000000000 ) ) ;
#65609 = EDGE_CURVE ( 'NONE', #80548, #37747, #135369, .T. ) ;
#65610 = EDGE_CURVE ( 'NONE', #53682, #71447, #12498, .T. ) ;
#65611 = DIRECTION ( 'NONE',  ( -0.7071067811865487940, 0.7071067811865463515, 0.000000000000000000 ) ) ;
#65612 = MECHANICAL_DESIGN_GEOMETRIC_PRESENTATION_REPRESENTATION (  '', ( #128099 ), #118852 ) ;
#65613 = CARTESIAN_POINT ( 'NONE',  ( 20.46247294953710849, -7.464222240803106570E-16, -6.094999999999989981 ) ) ;
#65614 = CARTESIAN_POINT ( 'NONE',  ( -0.9646429025310692129, 12.58792797458966284, -26.73614525879442994 ) ) ;
#65615 = ORIENTED_EDGE ( 'NONE', *, *, #99361, .T. ) ;
#65616 = EDGE_CURVE ( 'NONE', #37037, #132203, #14270, .T. ) ;
#65617 = CARTESIAN_POINT ( 'NONE',  ( 0.1600000000000011136, 3.289720434613005118, -7.220939306079887210 ) ) ;
#65618 = ORIENTED_EDGE ( 'NONE', *, *, #14210, .F. ) ;
#65619 = DIRECTION ( 'NONE',  ( 0.7071067811865486830, -0.7071067811865464625, -0.000000000000000000 ) ) ;
#65620 = DIRECTION ( 'NONE',  ( 0.6830127018922181881, 0.6830127018922202975, -0.2588190451025214056 ) ) ;
#65622 = VERTEX_POINT ( 'NONE', #138927 ) ;
#65621 = DIRECTION ( 'NONE',  ( -0.000000000000000000, -0.3543493200069152693, 0.9351131265310292928 ) ) ;
#65623 = ORIENTED_EDGE ( 'NONE', *, *, #26560, .T. ) ;
#65624 = CARTESIAN_POINT ( 'NONE',  ( 113.5375270504628986, -9.735942053221456900E-16, 7.949999999999998401 ) ) ;
#65625 = DIRECTION ( 'NONE',  ( -0.7071067811865486830, -0.7071067811865464625, -0.000000000000000000 ) ) ;
#65626 = AXIS2_PLACEMENT_3D ( 'NONE', #98897, #77198, #8298 ) ;
#65627 = CARTESIAN_POINT ( 'NONE',  ( -25.00193056682080339, -22.22500000000000142, 4.500000000000000888 ) ) ;
#65628 = EDGE_CURVE ( 'NONE', #51304, #129328, #28208, .T. ) ;
#65629 = ORIENTED_EDGE ( 'NONE', *, *, #141796, .F. ) ;
#65630 = FACE_OUTER_BOUND ( 'NONE', #95734, .T. ) ;
#65631 = ORIENTED_EDGE ( 'NONE', *, *, #15759, .F. ) ;
#65632 = AXIS2_PLACEMENT_3D ( 'NONE', #116224, #70623, #3839 ) ;
#65633 = ORIENTED_EDGE ( 'NONE', *, *, #92572, .F. ) ;
#65634 = CARTESIAN_POINT ( 'NONE',  ( 8.423184310185783730, 4.584330080086930965E-16, 0.000000000000000000 ) ) ;
#65635 = CARTESIAN_POINT ( 'NONE',  ( 128.6958184333952886, -52.10373894832327579, -40.45955814675561157 ) ) ;
#65636 = EDGE_CURVE ( 'NONE', #93893, #55894, #25862, .T. ) ;
#65637 = CARTESIAN_POINT ( 'NONE',  ( 48.48921356237309510, -27.52281430457089328, 5.000000000000000000 ) ) ;
#65638 = DIRECTION ( 'NONE',  ( -0.7071067811865486830, -0.7071067811865464625, -0.000000000000000000 ) ) ;
#65640 = CIRCLE ( 'NONE', #14684, 2.500000000000000444 ) ;
#65639 = LINE ( 'NONE', #132310, #63090 ) ;
#65641 = DIRECTION ( 'NONE',  ( -0.7071067811865487940, 0.7071067811865463515, -0.000000000000000000 ) ) ;
#65642 = LINE ( 'NONE', #118535, #6592 ) ;
#65643 = ORIENTED_EDGE ( 'NONE', *, *, #112928, .T. ) ;
#65644 = CARTESIAN_POINT ( 'NONE',  ( -8.700255128608413102, -27.71228299555199825, 4.000000000000000000 ) ) ;
#65645 = VERTEX_POINT ( 'NONE', #128061 ) ;
#65646 = EDGE_CURVE ( 'NONE', #54301, #58586, #105546, .T. ) ;
#65647 = EDGE_CURVE ( 'NONE', #52699, #116759, #48334, .T. ) ;
#65648 = CARTESIAN_POINT ( 'NONE',  ( -27.33010218547248726, 17.25929247661553845, 19.83885114516077408 ) ) ;
#65649 = AXIS2_PLACEMENT_3D ( 'NONE', #96018, #76436, #18428 ) ;
#65650 = LINE ( 'NONE', #109816, #65944 ) ;
#65651 = PLANE ( 'NONE',  #140816 ) ;
#65653 = ORIENTED_EDGE ( 'NONE', *, *, #143517, .F. ) ;
#65652 = AXIS2_PLACEMENT_3D ( 'NONE', #78795, #14935, #56365 ) ;
#65654 = FACE_OUTER_BOUND ( 'NONE', #41434, .T. ) ;
#65655 = CARTESIAN_POINT ( 'NONE',  ( 0.000000000000000000, 0.000000000000000000, 5.000000000000000000 ) ) ;
#65656 = LINE ( 'NONE', #90951, #69940 ) ;
#65657 = ORIENTED_EDGE ( 'NONE', *, *, #50286, .T. ) ;
#65658 = ORIENTED_EDGE ( 'NONE', *, *, #17629, .T. ) ;
#65659 = ADVANCED_FACE ( 'NONE', ( #114296 ), #16385, .T. ) ;
#65660 = CARTESIAN_POINT ( 'NONE',  ( 52.26932219902325727, -49.14999999999999147, 40.92499999999998295 ) ) ;
#65661 = CARTESIAN_POINT ( 'NONE',  ( 152.4000000000000057, -16.48000000000005016, -12.70000000000045404 ) ) ;
#65662 = DIRECTION ( 'NONE',  ( 0.000000000000000000, 0.000000000000000000, -1.000000000000000000 ) ) ;
#65663 = MECHANICAL_DESIGN_GEOMETRIC_PRESENTATION_REPRESENTATION (  '', ( #111990 ), #95716 ) ;
#65664 = CARTESIAN_POINT ( 'NONE',  ( 34.92499999999998295, 9.662461875838909364, 4.000000000000000000 ) ) ;
#65665 = CARTESIAN_POINT ( 'NONE',  ( -34.49999999999974420, -20.94567065516883275, 4.994342998332162331 ) ) ;
#65666 = CARTESIAN_POINT ( 'NONE',  ( 63.49543019189811588, 5.291415217122917625, 3.055000000000002380 ) ) ;
#65667 = CARTESIAN_POINT ( 'NONE',  ( 3.872664058232598627, -2.500000000000000444, 0.000000000000000000 ) ) ;
#65668 = EDGE_CURVE ( 'NONE', #110890, #136749, #58556, .T. ) ;
#65669 = EDGE_CURVE ( 'NONE', #31974, #10130, #93262, .T. ) ;
#65670 = CARTESIAN_POINT ( 'NONE',  ( -19.49999999999986500, 14.14708470758589165, -0.5283514160166116191 ) ) ;
#65671 = CARTESIAN_POINT ( 'NONE',  ( -14.57672154193637937, 11.25929247661560240, 17.85071094206588072 ) ) ;
#65672 = VERTEX_POINT ( 'NONE', #60686 ) ;
#65673 = CARTESIAN_POINT ( 'NONE',  ( -21.48921356237309155, -27.52281430457070499, 5.000000000000000000 ) ) ;
#65674 = EDGE_LOOP ( 'NONE', ( #124756, #75527, #76911, #389 ) ) ;
#65675 = AXIS2_PLACEMENT_3D ( 'NONE', #51153, #96055, #17090 ) ;
#65676 = DIRECTION ( 'NONE',  ( -0.7071067811865487940, 0.7071067811865463515, -0.000000000000000000 ) ) ;
#65677 = DIRECTION ( 'NONE',  ( 0.000000000000000000, 0.000000000000000000, -1.000000000000000000 ) ) ;
#65678 = ADVANCED_FACE ( 'NONE', ( #137495 ), #39628, .T. ) ;
#65679 = CARTESIAN_POINT ( 'NONE',  ( 156.1499999999997783, -49.14999999999999147, -34.92499999999975557 ) ) ;
#65680 = DIRECTION ( 'NONE',  ( 0.7071067811865487940, -0.7071067811865463515, 0.000000000000000000 ) ) ;
#65681 = SURFACE_STYLE_USAGE ( .BOTH. , #112694 ) ;
#65682 = ADVANCED_FACE ( 'NONE', ( #28742 ), #64219, .F. ) ;
#65683 = CARTESIAN_POINT ( 'NONE',  ( 156.1499999999997783, -52.14999999999999147, -62.92499999999978400 ) ) ;
#65684 = LINE ( 'NONE', #117833, #119456 ) ;
#65685 = ORIENTED_EDGE ( 'NONE', *, *, #36206, .T. ) ;
#65687 = VERTEX_POINT ( 'NONE', #30138 ) ;
#65686 = AXIS2_PLACEMENT_3D ( 'NONE', #6073, #103275, #72137 ) ;
#65688 = CARTESIAN_POINT ( 'NONE',  ( -30.48921356237309510, -27.52281430457076894, 5.000000000000000000 ) ) ;
#65689 = DIRECTION ( 'NONE',  ( -0.7071067811865486830, -0.7071067811865464625, 0.000000000000000000 ) ) ;
#65690 = CARTESIAN_POINT ( 'NONE',  ( 14.51078643762690490, -27.52281430457045275, 5.000000000000000000 ) ) ;
#65691 = CARTESIAN_POINT ( 'NONE',  ( 83.78752705046288440, 0.000000000000000000, -7.949999999999998401 ) ) ;
#65692 = DIRECTION ( 'NONE',  ( -0.7071067811865486830, -0.7071067811865464625, -0.000000000000000000 ) ) ;
#65693 = VECTOR ( 'NONE', #110637, 1000.000000000000000 ) ;
#65694 = DIRECTION ( 'NONE',  ( -0.3543493200069162685, -0.000000000000000000, -0.9351131265310288487 ) ) ;
#65695 = VERTEX_POINT ( 'NONE', #9818 ) ;
#65696 = CARTESIAN_POINT ( 'NONE',  ( 86.89583333333332860, -2.130196079827427091, 7.949999999999999289 ) ) ;
#65697 = EDGE_CURVE ( 'NONE', #137044, #69532, #95400, .T. ) ;
#65698 = DIRECTION ( 'NONE',  ( -1.000000000000000000, -0.000000000000000000, -0.000000000000000000 ) ) ;
#65699 = LINE ( 'NONE', #9071, #48432 ) ;
#65700 = DIRECTION ( 'NONE',  ( -0.6830127018922181881, 0.6830127018922202975, -0.2588190451025214056 ) ) ;
#65701 = ORIENTED_EDGE ( 'NONE', *, *, #60367, .F. ) ;
#65702 = EDGE_CURVE ( 'NONE', #71830, #48713, #52609, .T. ) ;
#65703 = AXIS2_PLACEMENT_3D ( 'NONE', #88405, #45627, #110814 ) ;
#65704 = LINE ( 'NONE', #53333, #106938 ) ;
#65705 = ORIENTED_EDGE ( 'NONE', *, *, #102626, .F. ) ;
#65706 = CARTESIAN_POINT ( 'NONE',  ( 75.68793019189811844, 6.110000000000002984, -1.637169565754156730 ) ) ;
#65707 = LINE ( 'NONE', #13925, #68655 ) ;
#65708 = DIRECTION ( 'NONE',  ( 0.7071067811865487940, 0.7071067811865463515, 0.000000000000000000 ) ) ;
#65709 = ORIENTED_EDGE ( 'NONE', *, *, #113123, .T. ) ;
#65710 = DIRECTION ( 'NONE',  ( -0.7071067811865487940, 0.7071067811865463515, 0.000000000000000000 ) ) ;
#65711 = LINE ( 'NONE', #54801, #40665 ) ;
#65712 = CARTESIAN_POINT ( 'NONE',  ( -0.8124618758394642759, -22.22500000000000142, 4.000000000000000000 ) ) ;
#65713 = DIRECTION ( 'NONE',  ( 0.000000000000000000, -1.000000000000000000, 0.000000000000000000 ) ) ;
#65714 = LINE ( 'NONE', #9087, #32390 ) ;
#65716 = VERTEX_POINT ( 'NONE', #72984 ) ;
#65715 = DIRECTION ( 'NONE',  ( -0.000000000000000000, 0.000000000000000000, 1.000000000000000000 ) ) ;
#65717 = LINE ( 'NONE', #119312, #9043 ) ;
#65718 = DIRECTION ( 'NONE',  ( 0.000000000000000000, -1.000000000000000000, 0.000000000000000000 ) ) ;
#65719 = DIRECTION ( 'NONE',  ( 1.000000000000000000, 0.000000000000000000, 0.000000000000000000 ) ) ;
#65720 = CIRCLE ( 'NONE', #56405, 2.500000000000000888 ) ;
#65721 = CARTESIAN_POINT ( 'NONE',  ( -19.93618820137057668, -6.270000000050818478, -36.99999999997771738 ) ) ;
#65722 = ORIENTED_EDGE ( 'NONE', *, *, #1137, .T. ) ;
#65723 = EDGE_CURVE ( 'NONE', #48454, #116545, #19972, .T. ) ;
#65724 = ORIENTED_EDGE ( 'NONE', *, *, #58442, .F. ) ;
#65725 = CARTESIAN_POINT ( 'NONE',  ( 65.33376352523143282, 6.110000000000001208, 1.122388791418549305E-15 ) ) ;
#65726 = VECTOR ( 'NONE', #89860, 1000.000000000000000 ) ;
#65727 = ORIENTED_EDGE ( 'NONE', *, *, #123549, .T. ) ;
#65728 = CARTESIAN_POINT ( 'NONE',  ( -11.20710678118646975, 12.75929247661559174, 5.000000000000000000 ) ) ;
#65729 = CARTESIAN_POINT ( 'NONE',  ( 17.53719725875415847, 4.202752102959690472E-16, 0.000000000000000000 ) ) ;
#65730 = CARTESIAN_POINT ( 'NONE',  ( 3.872664058232598183, 0.000000000000000000, 2.500000000000000444 ) ) ;
#65731 =( NAMED_UNIT ( * ) SI_UNIT ( $, .STERADIAN. ) SOLID_ANGLE_UNIT ( ) );
#65732 = EDGE_LOOP ( 'NONE', ( #21994, #126677, #57649, #23089 ) ) ;
#65733 = ORIENTED_EDGE ( 'NONE', *, *, #26901, .T. ) ;
#65734 = CARTESIAN_POINT ( 'NONE',  ( -24.32997752056147078, -22.22500000000000142, 0.9851499198022823922 ) ) ;
#65735 = DIRECTION ( 'NONE',  ( -1.000000000000000000, -1.224606353822377258E-16, -0.000000000000000000 ) ) ;
#65736 = VECTOR ( 'NONE', #72037, 1000.000000000000000 ) ;
#65737 = EDGE_LOOP ( 'NONE', ( #40397, #76809, #64590, #90327 ) ) ;
#65738 = AXIS2_PLACEMENT_3D ( 'NONE', #26197, #115287, #50096 ) ;
#65739 = LINE ( 'NONE', #97586, #88369 ) ;
#65740 = DIRECTION ( 'NONE',  ( -0.000000000000000000, 0.000000000000000000, 1.000000000000000000 ) ) ;
#65741 = CARTESIAN_POINT ( 'NONE',  ( -7.998069433178966570, -22.22500000000000142, 4.500000000000000888 ) ) ;
#65742 =( BOUNDED_CURVE ( )  B_SPLINE_CURVE ( 3, ( #129198, #63970, #19026, #86444 ),
 .UNSPECIFIED., .F., .T. ) 
 B_SPLINE_CURVE_WITH_KNOTS ( ( 4, 4 ),
 ( 5.106027341939291198, 6.645403452391242638 ),
 .UNSPECIFIED. ) 
 CURVE ( )  GEOMETRIC_REPRESENTATION_ITEM ( )  RATIONAL_B_SPLINE_CURVE ( ( 1.000000000000000000, 0.8120851936182310604, 0.8120851936182310604, 1.000000000000000000 ) ) 
 REPRESENTATION_ITEM ( '' )  );
#65743 = ORIENTED_EDGE ( 'NONE', *, *, #7751, .T. ) ;
#65744 = CIRCLE ( 'NONE', #33343, 0.5000000000000004441 ) ;
#65745 = DIRECTION ( 'NONE',  ( 0.6830127018922181881, 0.6830127018922202975, -0.2588190451025214056 ) ) ;
#65746 = DIRECTION ( 'NONE',  ( -0.7071067811865487940, 0.7071067811865463515, 0.000000000000000000 ) ) ;
#65747 = PLANE ( 'NONE',  #16584 ) ;
#65748 = LINE ( 'NONE', #141098, #71478 ) ;
#65749 = SURFACE_STYLE_FILL_AREA ( #109197 ) ;
#65750 = VECTOR ( 'NONE', #89106, 1000.000000000000000 ) ;
#65751 = CARTESIAN_POINT ( 'NONE',  ( -20.28242261357419451, -21.73023691814494285, 5.000000000000000888 ) ) ;
#65752 = ORIENTED_EDGE ( 'NONE', *, *, #62336, .F. ) ;
#65753 = CONICAL_SURFACE ( 'NONE', #111980, 2.500000000000000444, 0.9599310885968830309 ) ;
#65754 = ORIENTED_EDGE ( 'NONE', *, *, #62707, .F. ) ;
#65755 = CARTESIAN_POINT ( 'NONE',  ( 117.3079301918980946, -6.109999999999998543, 1.637169565754158507 ) ) ;
#65756 = ORIENTED_EDGE ( 'NONE', *, *, #27824, .T. ) ;
#65757 = ORIENTED_EDGE ( 'NONE', *, *, #140438, .T. ) ;
#65758 = VECTOR ( 'NONE', #49061, 1000.000000000000227 ) ;
#65759 = CARTESIAN_POINT ( 'NONE',  ( 184.1499999999998067, -50.22575108203859173, 35.38524182944927077 ) ) ;
#65760 = CARTESIAN_POINT ( 'NONE',  ( -1.828169399223519953, -11.24070752338416845, 4.000000000000000000 ) ) ;
#65761 = DIRECTION ( 'NONE',  ( -0.7071067811865486830, -0.7071067811865464625, -0.000000000000000000 ) ) ;
#65762 = ORIENTED_EDGE ( 'NONE', *, *, #95210, .F. ) ;
#65763 = DIRECTION ( 'NONE',  ( -1.000000000000000000, -1.224606353822377258E-16, -0.000000000000000000 ) ) ;
#65764 = LINE ( 'NONE', #129525, #17115 ) ;
#65767 = EDGE_CURVE ( 'NONE', #61191, #93479, #108378, .T. ) ;
#65766 = CARTESIAN_POINT ( 'NONE',  ( -20.88987624306225399, 8.854559187742358617, 4.414246686754470517 ) ) ;
#65765 = LINE ( 'NONE', #33824, #138364 ) ;
#65768 = LINE ( 'NONE', #109932, #92447 ) ;
#65769 = EDGE_CURVE ( 'NONE', #18049, #132699, #30889, .T. ) ;
#65770 = VECTOR ( 'NONE', #53264, 999.9999999999998863 ) ;
#65771 = PLANE ( 'NONE',  #79185 ) ;
#65772 = VERTEX_POINT ( 'NONE', #117837 ) ;
#65773 = DIRECTION ( 'NONE',  ( -0.6830127018922181881, 0.6830127018922202975, -0.2588190451025214056 ) ) ;
#65774 = DIRECTION ( 'NONE',  ( -0.6830127018922181881, 0.6830127018922202975, -0.2588190451025214056 ) ) ;
#65775 = EDGE_CURVE ( 'NONE', #108829, #566, #62806, .T. ) ;
#65776 = EDGE_CURVE ( 'NONE', #41224, #100224, #117139, .T. ) ;
#65777 = ORIENTED_EDGE ( 'NONE', *, *, #26827, .T. ) ;
#65778 = VERTEX_POINT ( 'NONE', #9057 ) ;
#65779 = EDGE_CURVE ( 'NONE', #53886, #70033, #128744, .T. ) ;
#65780 = EDGE_CURVE ( 'NONE', #93689, #129451, #31589, .T. ) ;
#65781 = ORIENTED_EDGE ( 'NONE', *, *, #59259, .F. ) ;
#65782 = CARTESIAN_POINT ( 'NONE',  ( 61.83376352523143993, 6.110000000000001208, 1.122388791418549305E-15 ) ) ;
#65783 = ORIENTED_EDGE ( 'NONE', *, *, #108426, .F. ) ;
#65784 = EDGE_CURVE ( 'NONE', #133821, #47983, #75812, .T. ) ;
#65785 = EDGE_CURVE ( 'NONE', #41872, #91199, #5078, .T. ) ;
#65786 = FACE_OUTER_BOUND ( 'NONE', #101862, .T. ) ;
#65787 = VECTOR ( 'NONE', #112989, 999.9999999999998863 ) ;
#65788 = CARTESIAN_POINT ( 'NONE',  ( 0.6291396162037723450, 5.278424836066147208, 3.047499999999990550 ) ) ;
#65789 = CARTESIAN_POINT ( 'NONE',  ( 99.60459685856476142, 1.637169565754164946, -6.109999999999999432 ) ) ;
#65790 = LINE ( 'NONE', #20069, #139758 ) ;
#65791 = EDGE_CURVE ( 'NONE', #109867, #58061, #73662, .T. ) ;
#65792 = VERTEX_POINT ( 'NONE', #42489 ) ;
#65793 = CARTESIAN_POINT ( 'NONE',  ( 2.816011393730999401, 28.73617430169785436, 5.000000000000000000 ) ) ;
#65794 = CARTESIAN_POINT ( 'NONE',  ( -0.1839886062690032631, 28.73617430169787568, 5.000000000000000000 ) ) ;
#65795 = AXIS2_PLACEMENT_3D ( 'NONE', #136495, #34516, #78041 ) ;
#65796 = FACE_OUTER_BOUND ( 'NONE', #106472, .T. ) ;
#65797 = CARTESIAN_POINT ( 'NONE',  ( -14.99999999999990230, 10.21212019023807649, -2.019456568337765212 ) ) ;
#65798 = EDGE_CURVE ( 'NONE', #68468, #122052, #51921, .T. ) ;
#65799 = EDGE_LOOP ( 'NONE', ( #79104, #6526, #30468, #33319 ) ) ;
#65800 = CARTESIAN_POINT ( 'NONE',  ( 22.42819999999999681, 3.174999999999997158, 5.000000000000000000 ) ) ;
#65801 = ORIENTED_EDGE ( 'NONE', *, *, #124735, .F. ) ;
#65802 = EDGE_LOOP ( 'NONE', ( #109170, #137622, #5514, #5456 ) ) ;
#65803 = ORIENTED_EDGE ( 'NONE', *, *, #136436, .F. ) ;
#65804 = CARTESIAN_POINT ( 'NONE',  ( 118.6204301918981230, 3.055000000000001936, -5.291415217122916737 ) ) ;
#65805 = ORIENTED_EDGE ( 'NONE', *, *, #141309, .T. ) ;
#65806 = PLANE ( 'NONE',  #81658 ) ;
#65807 = DIRECTION ( 'NONE',  ( -0.7071067811865486830, -0.7071067811865464625, 0.000000000000000000 ) ) ;
#65808 = ORIENTED_EDGE ( 'NONE', *, *, #130115, .F. ) ;
#65809 = DIRECTION ( 'NONE',  ( -0.7071067811865487940, 0.7071067811865463515, 0.000000000000000000 ) ) ;
#65810 = ORIENTED_EDGE ( 'NONE', *, *, #125818, .T. ) ;
#65812 = ADVANCED_FACE ( 'NONE', ( #63532 ), #130918, .F. ) ;
#65811 = VECTOR ( 'NONE', #51999, 1000.000000000000227 ) ;
#65813 = VECTOR ( 'NONE', #100595, 1000.000000000000000 ) ;
#65814 = CARTESIAN_POINT ( 'NONE',  ( 17.62456980810188867, -6.871911579029512218, 3.967499999999996252 ) ) ;
#65815 = LINE ( 'NONE', #109974, #11500 ) ;
#65816 = DIRECTION ( 'NONE',  ( 1.804112415015877406E-15, 0.000000000000000000, -1.000000000000000000 ) ) ;
#65817 = LINE ( 'NONE', #109979, #118411 ) ;
#65818 = ORIENTED_EDGE ( 'NONE', *, *, #34314, .T. ) ;
#65819 = ORIENTED_EDGE ( 'NONE', *, *, #134052, .T. ) ;
#65821 = VERTEX_POINT ( 'NONE', #41745 ) ;
#65820 = EDGE_CURVE ( 'NONE', #20392, #103852, #141040, .T. ) ;
#65822 = FILL_AREA_STYLE ('',( #65085 ) ) ;
#65823 = DIRECTION ( 'NONE',  ( 0.7071067811865487940, -0.7071067811865463515, 0.000000000000000000 ) ) ;
#65824 = FACE_OUTER_BOUND ( 'NONE', #9492, .T. ) ;
#65825 = DIRECTION ( 'NONE',  ( 0.7071067811865487940, -0.7071067811865463515, 0.000000000000000000 ) ) ;
#65826 = EDGE_CURVE ( 'NONE', #89630, #30859, #75115, .T. ) ;
#65827 = DIRECTION ( 'NONE',  ( 0.7071067811865486830, -0.7071067811865464625, -0.000000000000000000 ) ) ;
#65828 = AXIS2_PLACEMENT_3D ( 'NONE', #136914, #80421, #14427 ) ;
#65829 = CARTESIAN_POINT ( 'NONE',  ( 33.39626352523143993, 4.472830434245840259, -4.472830434245839371 ) ) ;
#65830 = PLANE ( 'NONE',  #122769 ) ;
#65831 = LINE ( 'NONE', #32451, #60478 ) ;
#65832 = EDGE_CURVE ( 'NONE', #139700, #49576, #27311, .T. ) ;
#65833 = ORIENTED_EDGE ( 'NONE', *, *, #76400, .T. ) ;
#65834 = FACE_OUTER_BOUND ( 'NONE', #708, .T. ) ;
#65835 = ORIENTED_EDGE ( 'NONE', *, *, #5937, .T. ) ;
#65836 = CARTESIAN_POINT ( 'NONE',  ( 0.000000000000000000, 0.000000000000000000, 0.000000000000000000 ) ) ;
#65837 = VERTEX_POINT ( 'NONE', #46797 ) ;
#65839 = ADVANCED_FACE ( 'NONE', ( #123618 ), #88837, .F. ) ;
#65838 = VECTOR ( 'NONE', #133549, 1000.000000000000000 ) ;
#65840 = DIRECTION ( 'NONE',  ( 1.000000000000000000, 0.000000000000000000, 0.000000000000000000 ) ) ;
#65842 = VERTEX_POINT ( 'NONE', #110537 ) ;
#65841 = DIRECTION ( 'NONE',  ( -0.6830127018922181881, 0.6830127018922202975, -0.2588190451025214056 ) ) ;
#65843 = VECTOR ( 'NONE', #51687, 1000.000000000000227 ) ;
#65844 = DIRECTION ( 'NONE',  ( 0.000000000000000000, -1.000000000000000000, 0.000000000000000000 ) ) ;
#65845 = ORIENTED_EDGE ( 'NONE', *, *, #72917, .T. ) ;
#65846 =( NAMED_UNIT ( * ) PLANE_ANGLE_UNIT ( ) SI_UNIT ( $, .RADIAN. ) );
#65847 = ORIENTED_EDGE ( 'NONE', *, *, #11562, .T. ) ;
#65848 = CARTESIAN_POINT ( 'NONE',  ( -29.20003122016818509, 8.259292476615634371, 16.85664084051848022 ) ) ;
#65849 = VERTEX_POINT ( 'NONE', #77949 ) ;
#65850 = ADVANCED_FACE ( 'NONE', ( #122136 ), #68519, .T. ) ;
#65851 = AXIS2_PLACEMENT_3D ( 'NONE', #74497, #83955, #128843 ) ;
#65852 = CARTESIAN_POINT ( 'NONE',  ( -8.999999999999932498, -10.44781430457072169, 5.000000000000000000 ) ) ;
#65853 = CARTESIAN_POINT ( 'NONE',  ( 107.9958603837962272, -3.974999999999998312, -6.884901960086286188 ) ) ;
#65855 = PRESENTATION_LAYER_ASSIGNMENT (  '', '', ( #95913 ) ) ;
#65854 = CARTESIAN_POINT ( 'NONE',  ( -23.99999999999984013, -2.904428200921339354, -6.989807076074889380 ) ) ;
#65856 = LINE ( 'NONE', #119443, #138885 ) ;
#65857 = ADVANCED_FACE ( 'NONE', ( #43895 ), #44646, .F. ) ;
#65858 = CARTESIAN_POINT ( 'NONE',  ( -11.99999999999992006, -4.068876922607777225, 4.000000000000000000 ) ) ;
#65859 = DIRECTION ( 'NONE',  ( -0.000000000000000000, -0.3543493200069152693, 0.9351131265310292928 ) ) ;
#65860 = CARTESIAN_POINT ( 'NONE',  ( 14.72916666666666607, -6.094999999999989093, 1.633150327867691765 ) ) ;
#65861 = CARTESIAN_POINT ( 'NONE',  ( 12.66623647476855297, 7.934999999999990727, -1.457635852685135314E-15 ) ) ;
#65862 = DIRECTION ( 'NONE',  ( 0.6830127018922181881, 0.6830127018922202975, -0.2588190451025214056 ) ) ;
#65863 = FACE_OUTER_BOUND ( 'NONE', #36460, .T. ) ;
#65864 = EDGE_LOOP ( 'NONE', ( #34045, #36439, #133484, #108882 ) ) ;
#65865 = EDGE_LOOP ( 'NONE', ( #34490, #97935, #60719 ) ) ;
#65866 = ORIENTED_EDGE ( 'NONE', *, *, #30885, .T. ) ;
#65867 = CARTESIAN_POINT ( 'NONE',  ( -0.6932699330959857242, -3.740707523384248390, 12.88036043432867750 ) ) ;
#65868 = CARTESIAN_POINT ( 'NONE',  ( -12.18398860626900060, 28.73617430169795739, 5.000000000000000000 ) ) ;
#65869 = LINE ( 'NONE', #63192, #53890 ) ;
#65870 = SURFACE_STYLE_FILL_AREA ( #32496 ) ;
#65871 = EDGE_LOOP ( 'NONE', ( #112634, #34189, #30147, #17924 ) ) ;
#65872 = DIRECTION ( 'NONE',  ( -0.7071067811865486830, 0.7071067811865464625, 0.000000000000000000 ) ) ;
#65873 = LINE ( 'NONE', #131091, #48823 ) ;
#65874 = ADVANCED_FACE ( 'NONE', ( #11208 ), #109848, .F. ) ;
#65875 = DIRECTION ( 'NONE',  ( -0.000000000000000000, 0.3543493200069153248, 0.9351131265310292928 ) ) ;
#65876 = DIRECTION ( 'NONE',  ( 0.7071067811865487940, 0.7071067811865463515, -0.000000000000000000 ) ) ;
#65878 = VERTEX_POINT ( 'NONE', #1753 ) ;
#65877 = DIRECTION ( 'NONE',  ( -0.6830127018922180770, -0.6830127018922204085, -0.2588190451025213501 ) ) ;
#65879 = DIRECTION ( 'NONE',  ( 0.000000000000000000, 0.000000000000000000, -1.000000000000000000 ) ) ;
#65880 = CARTESIAN_POINT ( 'NONE',  ( 69.97916666666665719, -7.950000000000000178, 2.130196079827424427 ) ) ;
#65881 = CARTESIAN_POINT ( 'NONE',  ( 0.000000000000000000, 8.616843969807042924, 0.000000000000000000 ) ) ;
#65882 = LINE ( 'NONE', #53542, #119676 ) ;
#65883 = CARTESIAN_POINT ( 'NONE',  ( -20.57672154193634384, 11.25929247661560240, 17.85071094206589137 ) ) ;
#65884 = ORIENTED_EDGE ( 'NONE', *, *, #111807, .F. ) ;
#65885 = VERTEX_POINT ( 'NONE', #112012 ) ;
#65886 = ORIENTED_EDGE ( 'NONE', *, *, #31045, .T. ) ;
#65887 = CARTESIAN_POINT ( 'NONE',  ( 89.10459685856477563, 1.637169565754164946, -6.109999999999999432 ) ) ;
#65888 = ORIENTED_EDGE ( 'NONE', *, *, #130808, .F. ) ;
#65889 = LINE ( 'NONE', #139868, #1641 ) ;
#65890 = DIRECTION ( 'NONE',  ( 0.7071067811865487940, 0.7071067811865463515, -0.000000000000000000 ) ) ;
#65891 = ORIENTED_EDGE ( 'NONE', *, *, #72187, .F. ) ;
#65892 = CARTESIAN_POINT ( 'NONE',  ( 0.000000000000000000, 0.000000000000000000, 5.000000000000000000 ) ) ;
#65895 = ADVANCED_FACE ( 'NONE', ( #350 ), #1060, .F. ) ;
#65894 = AXIS2_PLACEMENT_3D ( 'NONE', #32759, #31322, #53801 ) ;
#65893 = LINE ( 'NONE', #53557, #104455 ) ;
#65896 = CARTESIAN_POINT ( 'NONE',  ( 85.80793019189810877, -6.109999999999998543, 1.637169565754158063 ) ) ;
#65897 = ADVANCED_FACE ( 'NONE', ( #56931 ), #16593, .T. ) ;
#65898 = ORIENTED_EDGE ( 'NONE', *, *, #28833, .F. ) ;
#65899 = DIRECTION ( 'NONE',  ( -0.7071067811865486830, -0.7071067811865464625, -0.000000000000000000 ) ) ;
#65900 = ORIENTED_EDGE ( 'NONE', *, *, #103649, .F. ) ;
#65901 = VERTEX_POINT ( 'NONE', #45347 ) ;
#65902 = ORIENTED_EDGE ( 'NONE', *, *, #90436, .F. ) ;
#65903 = LINE ( 'NONE', #109365, #35257 ) ;
#65904 = ADVANCED_FACE ( 'NONE', ( #76535, #101104, #89524 ), #133753, .T. ) ;
#65905 = CARTESIAN_POINT ( 'NONE',  ( 39.18398860626899705, 28.73617430169814568, 5.000000000000000000 ) ) ;
#65906 = PLANE ( 'NONE',  #88224 ) ;
#65907 = AXIS2_PLACEMENT_3D ( 'NONE', #987, #98876, #23470 ) ;
#65908 = CARTESIAN_POINT ( 'NONE',  ( 3.600192512601737782, -49.14999999999999147, -40.57313449935462302 ) ) ;
#65909 =( BOUNDED_CURVE ( )  B_SPLINE_CURVE ( 3, ( #92259, #124195, #27732, #135111 ),
 .UNSPECIFIED., .F., .T. ) 
 B_SPLINE_CURVE_WITH_KNOTS ( ( 4, 4 ),
 ( 3.141592653589798889, 4.446051736530363563 ),
 .UNSPECIFIED. ) 
 CURVE ( )  GEOMETRIC_REPRESENTATION_ITEM ( )  RATIONAL_B_SPLINE_CURVE ( ( 1.000000000000000000, 0.8631550219135040170, 0.8631550219135040170, 1.000000000000000000 ) ) 
 REPRESENTATION_ITEM ( '' )  );
#65910 = CARTESIAN_POINT ( 'NONE',  ( 24.39999999999999858, -7.600000000000061817, 33.92499999999998295 ) ) ;
#65911 = MECHANICAL_DESIGN_GEOMETRIC_PRESENTATION_REPRESENTATION (  '', ( #107567 ), #49666 ) ;
#65912 = ORIENTED_EDGE ( 'NONE', *, *, #20473, .T. ) ;
#65913 = ORIENTED_EDGE ( 'NONE', *, *, #60517, .T. ) ;
#65914 = VECTOR ( 'NONE', #103939, 1000.000000000000000 ) ;
#65915 = LINE ( 'NONE', #53586, #45752 ) ;
#65916 = VERTEX_POINT ( 'NONE', #58385 ) ;
#65917 = ORIENTED_EDGE ( 'NONE', *, *, #83908, .F. ) ;
#65918 = CARTESIAN_POINT ( 'NONE',  ( -28.49999999999979039, 4.466399257802221356, 5.000000000000000000 ) ) ;
#65919 = ORIENTED_EDGE ( 'NONE', *, *, #40276, .F. ) ;
#65920 = STYLED_ITEM ( 'NONE', ( #109099 ), #88505 ) ;
#65921 = CARTESIAN_POINT ( 'NONE',  ( 56.70833333333333570, -3.974999999999999201, -6.884901960086287964 ) ) ;
#65922 = CARTESIAN_POINT ( 'NONE',  ( 10.49999999999993250, -1.533600742197719580, 5.000000000000000000 ) ) ;
#65923 = LINE ( 'NONE', #9312, #94194 ) ;
#65924 = PLANE ( 'NONE',  #15950 ) ;
#65925 = LINE ( 'NONE', #142739, #125413 ) ;
#65926 = EDGE_LOOP ( 'NONE', ( #37719, #65482, #101436, #48679 ) ) ;
#65927 = DIRECTION ( 'NONE',  ( -0.7071067811865487940, 0.7071067811865463515, -0.000000000000000000 ) ) ;
#65928 = ORIENTED_EDGE ( 'NONE', *, *, #55929, .T. ) ;
#65929 = DIRECTION ( 'NONE',  ( -0.3543493200069162685, -0.000000000000000000, -0.9351131265310288487 ) ) ;
#65930 = ORIENTED_EDGE ( 'NONE', *, *, #53365, .T. ) ;
#65931 = CARTESIAN_POINT ( 'NONE',  ( 116.8916937171295558, 2.130196079827421762, 7.950000000000000178 ) ) ;
#65933 = ORIENTED_EDGE ( 'NONE', *, *, #73931, .F. ) ;
#65932 = EDGE_CURVE ( 'NONE', #76747, #134004, #82940, .T. ) ;
#65934 = CARTESIAN_POINT ( 'NONE',  ( 5.999999999999956479, -5.527737879153189482, -7.983877177622385801 ) ) ;
#65935 = ORIENTED_EDGE ( 'NONE', *, *, #26965, .T. ) ;
#65936 = ORIENTED_EDGE ( 'NONE', *, *, #42057, .F. ) ;
#65937 = VERTEX_POINT ( 'NONE', #4585 ) ;
#65938 = VECTOR ( 'NONE', #65641, 999.9999999999998863 ) ;
#65939 = EDGE_CURVE ( 'NONE', #114073, #29586, #141846, .T. ) ;
#65940 = ADVANCED_FACE ( 'NONE', ( #38717 ), #90977, .F. ) ;
#65941 = FACE_OUTER_BOUND ( 'NONE', #46700, .T. ) ;
#65942 = FACE_OUTER_BOUND ( 'NONE', #64152, .T. ) ;
#65943 = AXIS2_PLACEMENT_3D ( 'NONE', #13606, #90487, #77493 ) ;
#65944 = VECTOR ( 'NONE', #143153, 1000.000000000000000 ) ;
#65945 = LINE ( 'NONE', #143454, #124805 ) ;
#65947 = EDGE_CURVE ( 'NONE', #6354, #15312, #6038, .T. ) ;
#65946 = LINE ( 'NONE', #75368, #7831 ) ;
#65948 = CARTESIAN_POINT ( 'NONE',  ( 126.4379301918981184, -6.110000000000001208, 1.637169565754158951 ) ) ;
#65949 = DIRECTION ( 'NONE',  ( -4.681814790819591790E-17, -0.3543493200069152693, 0.9351131265310292928 ) ) ;
#65950 = VECTOR ( 'NONE', #97035, 1000.000000000000227 ) ;
#65951 = EDGE_CURVE ( 'NONE', #68546, #73287, #16703, .T. ) ;
#65952 = LINE ( 'NONE', #86954, #25043 ) ;
#65953 = DIRECTION ( 'NONE',  ( -0.6830127018922181881, 0.6830127018922202975, -0.2588190451025214056 ) ) ;
#65954 = ADVANCED_FACE ( 'NONE', ( #103243 ), #3212, .F. ) ;
#65955 = CARTESIAN_POINT ( 'NONE',  ( 12.19999999999999574, -40.43000000000000682, 19.06900128115122683 ) ) ;
#65956 = EDGE_CURVE ( 'NONE', #86472, #73773, #82245, .T. ) ;
#65957 = LINE ( 'NONE', #8626, #117697 ) ;
#65958 = DIRECTION ( 'NONE',  ( 0.7071067811865487940, 0.7071067811865463515, 0.000000000000000000 ) ) ;
#65959 = VERTEX_POINT ( 'NONE', #91663 ) ;
#65960 = ORIENTED_EDGE ( 'NONE', *, *, #119759, .F. ) ;
#65961 = ORIENTED_EDGE ( 'NONE', *, *, #103126, .F. ) ;
#65962 = LINE ( 'NONE', #23856, #28675 ) ;
#65963 = VERTEX_POINT ( 'NONE', #60497 ) ;
#65964 = ORIENTED_EDGE ( 'NONE', *, *, #27572, .F. ) ;
#65965 = CARTESIAN_POINT ( 'NONE',  ( 23.67183060077630330, 8.259292476615630818, 4.000000000000000000 ) ) ;
#65966 = CARTESIAN_POINT ( 'NONE',  ( 13.60830628287043886, 1.633150327867687324, -6.094999999999991758 ) ) ;
#65967 = EDGE_CURVE ( 'NONE', #14576, #15770, #59084, .T. ) ;
#65968 = EDGE_CURVE ( 'NONE', #132252, #1839, #102566, .T. ) ;
#65969 = DIRECTION ( 'NONE',  ( -1.000000000000000000, -1.224606353822377258E-16, -0.000000000000000000 ) ) ;
#65970 = LINE ( 'NONE', #98550, #11611 ) ;
#65971 = ORIENTED_EDGE ( 'NONE', *, *, #69811, .T. ) ;
#65972 = CARTESIAN_POINT ( 'NONE',  ( 17.51078643762690845, -27.52281430457043143, 5.000000000000000000 ) ) ;
#65973 = EDGE_LOOP ( 'NONE', ( #6134, #26819, #134444, #41728 ) ) ;
#65974 = EDGE_CURVE ( 'NONE', #59163, #76525, #100125, .T. ) ;
#65975 = DIRECTION ( 'NONE',  ( -0.000000000000000000, 0.000000000000000000, 1.000000000000000000 ) ) ;
#65976 = CARTESIAN_POINT ( 'NONE',  ( 15.96290314143521805, -3.967499999999994476, 6.871911579029513106 ) ) ;
#65977 = EDGE_LOOP ( 'NONE', ( #70537, #117772, #119230, #47303 ) ) ;
#65978 = CARTESIAN_POINT ( 'NONE',  ( 83.32876352523143737, 0.000000000000000000, -6.109999999999999432 ) ) ;
#65979 = CARTESIAN_POINT ( 'NONE',  ( 6.092757112198636804, -9.434971466833395937, -1.145375144610985441 ) ) ;
#65980 = CARTESIAN_POINT ( 'NONE',  ( 52.51281677483321175, -49.11905619111353616, -40.21880474160295904 ) ) ;
#65981 = CARTESIAN_POINT ( 'NONE',  ( -16.49999999999988276, -19.91253812416055169, 4.000000000000000000 ) ) ;
#65982 = ORIENTED_EDGE ( 'NONE', *, *, #140608, .F. ) ;
#65983 = ORIENTED_EDGE ( 'NONE', *, *, #17294, .F. ) ;
#65984 = ORIENTED_EDGE ( 'NONE', *, *, #112028, .T. ) ;
#65985 = CARTESIAN_POINT ( 'NONE',  ( 48.48921356237309510, -27.52281430457089328, 5.000000000000000000 ) ) ;
#65986 = DIRECTION ( 'NONE',  ( 0.6830127018922181881, 0.6830127018922202975, -0.2588190451025214056 ) ) ;
#65987 = CARTESIAN_POINT ( 'NONE',  ( 10.49999999999993427, 0.05218569542917404769, 5.000000000000000000 ) ) ;
#65988 = DIRECTION ( 'NONE',  ( -0.000000000000000000, -0.3543493200069152693, 0.9351131265310292928 ) ) ;
#65989 = CARTESIAN_POINT ( 'NONE',  ( 69.29974487139159578, -27.71228299555254537, 4.000000000000000000 ) ) ;
#65991 = ORIENTED_EDGE ( 'NONE', *, *, #47365, .F. ) ;
#65990 = VECTOR ( 'NONE', #100847, 1000.000000000000000 ) ;
#65992 = LINE ( 'NONE', #142114, #22884 ) ;
#65993 = FACE_OUTER_BOUND ( 'NONE', #87552, .T. ) ;
#65994 = EDGE_CURVE ( 'NONE', #20842, #71467, #114129, .T. ) ;
#65995 = VERTEX_POINT ( 'NONE', #16964 ) ;
#65996 = DIRECTION ( 'NONE',  ( 1.000000000000000000, 0.000000000000000000, 0.000000000000000000 ) ) ;
#65997 = FACE_OUTER_BOUND ( 'NONE', #115974, .T. ) ;
#65998 = ORIENTED_EDGE ( 'NONE', *, *, #58667, .F. ) ;
#66000 = ORIENTED_EDGE ( 'NONE', *, *, #126909, .F. ) ;
#65999 = CARTESIAN_POINT ( 'NONE',  ( 1.827855086967997700, 4.202752102959690472E-16, 0.000000000000000000 ) ) ;
#66001 = EDGE_LOOP ( 'NONE', ( #43793, #120474, #20120, #5864 ) ) ;
#66002 = DIRECTION ( 'NONE',  ( 0.000000000000000000, 1.000000000000000000, 0.000000000000000000 ) ) ;
#66003 = CARTESIAN_POINT ( 'NONE',  ( 7.499999999999947597, -17.56887692260763245, 4.000000000000000000 ) ) ;
#66004 = ORIENTED_EDGE ( 'NONE', *, *, #117489, .T. ) ;
#66005 = DIRECTION ( 'NONE',  ( -0.000000000000000000, 0.000000000000000000, 1.000000000000000000 ) ) ;
#66006 = EDGE_CURVE ( 'NONE', #78277, #48269, #14815, .T. ) ;
#66007 = AXIS2_PLACEMENT_3D ( 'NONE', #74420, #6948, #85989 ) ;
#66008 = DIRECTION ( 'NONE',  ( 2.781805975412906507E-17, 0.3543493200069153248, 0.9351131265310292928 ) ) ;
#66009 = DIRECTION ( 'NONE',  ( 0.7071067811865487940, 0.7071067811865463515, -0.000000000000000000 ) ) ;
#66010 = CARTESIAN_POINT ( 'NONE',  ( -14.99999999999988987, -12.03360074219761522, 5.000000000000000000 ) ) ;
#66011 = EDGE_CURVE ( 'NONE', #6847, #7168, #124294, .T. ) ;
#66012 = CARTESIAN_POINT ( 'NONE',  ( 34.92499999999998295, -10.65190338184899410, -7.458287694568761950 ) ) ;
#66013 = DIRECTION ( 'NONE',  ( 0.7071067811865487940, 0.7071067811865463515, -0.000000000000000000 ) ) ;
#66014 = CARTESIAN_POINT ( 'NONE',  ( 36.48921356237310221, -27.52281430457080802, 5.000000000000000000 ) ) ;
#66015 = LINE ( 'NONE', #107337, #142890 ) ;
#66016 = LINE ( 'NONE', #109487, #120877 ) ;
#66017 = CARTESIAN_POINT ( 'NONE',  ( 30.29974487139158867, -27.71228299555227537, 4.000000000000000000 ) ) ;
#66018 = DIRECTION ( 'NONE',  ( 0.6830127018922180770, -0.6830127018922204085, -0.2588190451025214056 ) ) ;
#66019 = CARTESIAN_POINT ( 'NONE',  ( -34.42500000000001137, 21.72500000000000142, 0.5000000000000000000 ) ) ;
#66020 = VERTEX_POINT ( 'NONE', #70667 ) ;
#66021 = VERTEX_POINT ( 'NONE', #3890 ) ;
#66022 = CARTESIAN_POINT ( 'NONE',  ( 103.5208333333333428, 7.949999999999999289, 2.130196079827431532 ) ) ;
#66023 = ORIENTED_EDGE ( 'NONE', *, *, #122884, .T. ) ;
#66024 = VECTOR ( 'NONE', #56580, 1000.000000000000000 ) ;
#66025 = ORIENTED_EDGE ( 'NONE', *, *, #42537, .F. ) ;
#66026 = ADVANCED_FACE ( 'NONE', ( #125741 ), #114810, .F. ) ;
#66027 = VERTEX_POINT ( 'NONE', #48890 ) ;
#66028 = DIRECTION ( 'NONE',  ( -0.7071067811865486830, -0.7071067811865464625, -0.000000000000000000 ) ) ;
#66029 = CARTESIAN_POINT ( 'NONE',  ( 90.25000000000000000, -9.735942053221458872E-16, 7.950000000000000178 ) ) ;
#66030 = ORIENTED_EDGE ( 'NONE', *, *, #85208, .F. ) ;
#66031 = DIRECTION ( 'NONE',  ( 0.000000000000000000, 0.000000000000000000, 1.000000000000000000 ) ) ;
#66032 = CARTESIAN_POINT ( 'NONE',  ( 27.48921356237309155, -27.52281430457074762, 5.000000000000000000 ) ) ;
#66033 = CARTESIAN_POINT ( 'NONE',  ( -75.48921356237309510, -27.52281430457107803, 5.000000000000000000 ) ) ;
#66034 = LINE ( 'NONE', #77618, #127632 ) ;
#66035 = EDGE_CURVE ( 'NONE', #13073, #6949, #104676, .T. ) ;
#66036 = ORIENTED_EDGE ( 'NONE', *, *, #92222, .T. ) ;
#66037 = CARTESIAN_POINT ( 'NONE',  ( 29.29289321881326202, -18.74070752338408852, 5.000000000000000000 ) ) ;
#66038 = FACE_OUTER_BOUND ( 'NONE', #13264, .T. ) ;
#66039 = PLANE ( 'NONE',  #112278 ) ;
#66040 = PLANE ( 'NONE',  #42269 ) ;
#66041 = CARTESIAN_POINT ( 'NONE',  ( 0.02857727139928691387, -0.5999999999999994227, -3.398545894033870418 ) ) ;
#66042 = DIRECTION ( 'NONE',  ( -0.3543493200069163240, -0.000000000000000000, -0.9351131265310288487 ) ) ;
#66043 = AXIS2_PLACEMENT_3D ( 'NONE', #76183, #10187, #21062 ) ;
#66044 = LINE ( 'NONE', #89206, #2868 ) ;
#66045 = ORIENTED_EDGE ( 'NONE', *, *, #9311, .F. ) ;
#66046 = VERTEX_POINT ( 'NONE', #138032 ) ;
#66047 = AXIS2_PLACEMENT_3D ( 'NONE', #122246, #88953, #133862 ) ;
#66048 = CARTESIAN_POINT ( 'NONE',  ( 116.0837635252314470, -6.110000000000001208, -3.741295971395164515E-16 ) ) ;
#66049 = ORIENTED_EDGE ( 'NONE', *, *, #1984, .F. ) ;
#66050 = VECTOR ( 'NONE', #134044, 1000.000000000000000 ) ;
#66051 = LINE ( 'NONE', #110213, #99529 ) ;
#66052 = CARTESIAN_POINT ( 'NONE',  ( 13.49999999999990408, 21.43112307739196609, 4.000000000000000000 ) ) ;
#66053 = DIRECTION ( 'NONE',  ( -0.6830127018922180770, 0.6830127018922202975, -0.2588190451025213501 ) ) ;
#66054 = CARTESIAN_POINT ( 'NONE',  ( 21.99507522778792534, -5.240707523384225297, 12.38332538355491153 ) ) ;
#66056 = ADVANCED_FACE ( 'NONE', ( #128578 ), #72826, .T. ) ;
#66055 = SURFACE_STYLE_FILL_AREA ( #42875 ) ;
#66057 = CARTESIAN_POINT ( 'NONE',  ( 118.0370968585647802, -3.054999999999998828, -5.291415217122919401 ) ) ;
#66058 = EDGE_CURVE ( 'NONE', #53362, #63172, #85775, .T. ) ;
#66059 = EDGE_LOOP ( 'NONE', ( #59135, #20123, #47877, #30380 ) ) ;
#66060 = VERTEX_POINT ( 'NONE', #50314 ) ;
#66061 = CARTESIAN_POINT ( 'NONE',  ( -15.18398860626900237, 28.73617430169797871, 5.000000000000000000 ) ) ;
#66062 = CARTESIAN_POINT ( 'NONE',  ( -57.48921356237308800, -27.52281430457095368, 5.000000000000000000 ) ) ;
#66063 = ORIENTED_EDGE ( 'NONE', *, *, #34345, .F. ) ;
#66064 = ORIENTED_EDGE ( 'NONE', *, *, #59783, .F. ) ;
#66065 = CARTESIAN_POINT ( 'NONE',  ( 37.91709685856477563, 3.054999999999998828, 5.291415217122922066 ) ) ;
#66066 = ORIENTED_EDGE ( 'NONE', *, *, #7467, .T. ) ;
#66067 = DIRECTION ( 'NONE',  ( 1.000000000000000000, 0.000000000000000000, 0.000000000000000000 ) ) ;
#66068 = EDGE_CURVE ( 'NONE', #114249, #74087, #108207, .T. ) ;
#66069 = DIRECTION ( 'NONE',  ( 0.000000000000000000, -1.000000000000000000, 0.000000000000000000 ) ) ;
#66070 = CARTESIAN_POINT ( 'NONE',  ( -6.489213562373093325, -27.52281430457059841, 5.000000000000000000 ) ) ;
#66071 = CARTESIAN_POINT ( 'NONE',  ( 33.01626352523145158, -4.472830434245839371, 4.472830434245839371 ) ) ;
#66072 = ORIENTED_EDGE ( 'NONE', *, *, #131863, .F. ) ;
#66073 = CARTESIAN_POINT ( 'NONE',  ( -2.700255128608413990, -27.71228299555204089, 4.000000000000000000 ) ) ;
#66074 = EDGE_LOOP ( 'NONE', ( #139963, #20631, #132571, #15906 ) ) ;
#66075 = ORIENTED_EDGE ( 'NONE', *, *, #81494, .T. ) ;
#66076 = ORIENTED_EDGE ( 'NONE', *, *, #22875, .T. ) ;
#66077 = DIRECTION ( 'NONE',  ( -0.7071067811865486830, 0.7071067811865464625, 0.000000000000000000 ) ) ;
#66078 = CARTESIAN_POINT ( 'NONE',  ( 12.86840764549667604, 2.500000000000003553, 3.061616997868386099E-16 ) ) ;
#66079 = ORIENTED_EDGE ( 'NONE', *, *, #109956, .F. ) ;
#66080 = LINE ( 'NONE', #21838, #22785 ) ;
#66081 = CARTESIAN_POINT ( 'NONE',  ( -10.49999999999993250, 5.696342897626490931, -7.587980461218421624 ) ) ;
#66082 = DIRECTION ( 'NONE',  ( -1.000000000000000000, -0.000000000000000000, 0.000000000000000000 ) ) ;
#66083 = FACE_OUTER_BOUND ( 'NONE', #120172, .T. ) ;
#66084 = FACE_BOUND ( 'NONE', #30198, .T. ) ;
#66085 = ORIENTED_EDGE ( 'NONE', *, *, #19303, .F. ) ;
#66086 = CARTESIAN_POINT ( 'NONE',  ( -32.20710678118632586, 15.75929247661555443, 5.000000000000000000 ) ) ;
#66087 = LINE ( 'NONE', #134192, #120794 ) ;
#66088 = CARTESIAN_POINT ( 'NONE',  ( -15.29974487139158867, -27.71228299555216879, 4.000000000000000000 ) ) ;
#66089 = ORIENTED_EDGE ( 'NONE', *, *, #59410, .F. ) ;
#66090 = LINE ( 'NONE', #23252, #138444 ) ;
#66091 = ORIENTED_EDGE ( 'NONE', *, *, #76096, .F. ) ;
#66092 = VERTEX_POINT ( 'NONE', #94502 ) ;
#66093 = LINE ( 'NONE', #110262, #104977 ) ;
#66094 = ORIENTED_EDGE ( 'NONE', *, *, #132283, .F. ) ;
#66095 = CONICAL_SURFACE ( 'NONE', #70761, 2.055000000000000160, 1.047197551196600962 ) ;
#66096 = ADVANCED_FACE ( 'NONE', ( #64752 ), #90836, .T. ) ;
#66097 = CARTESIAN_POINT ( 'NONE',  ( 46.43293019189811588, 1.637169565754156508, 6.110000000000000320 ) ) ;
#66098 = ORIENTED_EDGE ( 'NONE', *, *, #107842, .F. ) ;
#66099 = CARTESIAN_POINT ( 'NONE',  ( 31.49999999999977973, 3.431123077392151277, 4.000000000000000000 ) ) ;
#66100 = EDGE_CURVE ( 'NONE', #1472, #105971, #119119, .T. ) ;
#66101 = FACE_OUTER_BOUND ( 'NONE', #38321, .T. ) ;
#66102 = LINE ( 'NONE', #120416, #37194 ) ;
#66103 = VERTEX_POINT ( 'NONE', #53135 ) ;
#66104 = EDGE_CURVE ( 'NONE', #71093, #24475, #63102, .T. ) ;
#66105 = CARTESIAN_POINT ( 'NONE',  ( 0.5166543864104510275, 22.22500000000000142, 4.500000000000000888 ) ) ;
#66106 = CARTESIAN_POINT ( 'NONE',  ( -27.18398860626900060, 28.73617430169806042, 5.000000000000000000 ) ) ;
#66107 = ADVANCED_FACE ( 'NONE', ( #52428 ), #19800, .F. ) ;
#66108 =( BOUNDED_CURVE ( )  B_SPLINE_CURVE ( 2, ( #127903, #62639, #60512, #18363, #72842, #16983, #82957, #48909, #103954, #74220, #93113, #71370, #105399 ),
 .UNSPECIFIED., .F., .F. ) 
 B_SPLINE_CURVE_WITH_KNOTS ( ( 3, 2, 2, 2, 2, 2, 3 ),
 ( 0.8833333333333334147, 0.8861111111111111827, 0.8888888888888889506, 0.8916666666666668295, 0.8944444444444445974, 0.8972222222222223653, 0.9000000000000001332 ),
 .UNSPECIFIED. ) 
 CURVE ( )  GEOMETRIC_REPRESENTATION_ITEM ( )  RATIONAL_B_SPLINE_CURVE ( ( 0.9999999999999986677, 0.9659258262890696445, 1.000000000000000000, 0.9659258262890683122, 1.000000000000000000, 0.9659258262890683122, 1.000000000000000000, 0.9659258262890683122, 1.000000000000000000, 0.9659258262890683122, 1.000000000000000000, 0.9659258262890669799, 1.000000000000001332 ) ) 
 REPRESENTATION_ITEM ( '' )  );
#66109 = FACE_OUTER_BOUND ( 'NONE', #98240, .T. ) ;
#66110 = VECTOR ( 'NONE', #112181, 1000.000000000000227 ) ;
#66111 = DIRECTION ( 'NONE',  ( 0.7071067811865486830, -0.7071067811865464625, -0.000000000000000000 ) ) ;
#66112 = CARTESIAN_POINT ( 'NONE',  ( 34.42500000000002558, -22.26999999999999247, 0.000000000000000000 ) ) ;
#66113 = LINE ( 'NONE', #87133, #74892 ) ;
#66114 = DIRECTION ( 'NONE',  ( 0.7071067811865487940, 0.7071067811865463515, 0.000000000000000000 ) ) ;
#66115 = ORIENTED_EDGE ( 'NONE', *, *, #62687, .T. ) ;
#66116 = ORIENTED_EDGE ( 'NONE', *, *, #124525, .F. ) ;
#66117 = ORIENTED_EDGE ( 'NONE', *, *, #42, .F. ) ;
#66118 = DIRECTION ( 'NONE',  ( -0.7071067811865486830, -0.7071067811865464625, 0.000000000000000000 ) ) ;
#66119 = CARTESIAN_POINT ( 'NONE',  ( -14.01844734635661283, 18.75929247661553134, 20.33588619593446367 ) ) ;
#66120 = VERTEX_POINT ( 'NONE', #117659 ) ;
#66121 = ORIENTED_EDGE ( 'NONE', *, *, #61115, .T. ) ;
#66122 = CARTESIAN_POINT ( 'NONE',  ( 2.510786437626908008, -27.52281430457053446, 5.000000000000000000 ) ) ;
#66124 = EDGE_CURVE ( 'NONE', #76368, #27605, #97340, .T. ) ;
#66123 = FACE_OUTER_BOUND ( 'NONE', #83563, .T. ) ;
#66125 = EDGE_CURVE ( 'NONE', #121862, #109240, #75634, .T. ) ;
#66126 = CARTESIAN_POINT ( 'NONE',  ( 4.499999999999974243, -1.533600742197722910, 5.000000000000000000 ) ) ;
#66127 = EDGE_LOOP ( 'NONE', ( #18018, #113455, #90011, #60073 ) ) ;
#66128 = LINE ( 'NONE', #32790, #67190 ) ;
#66129 = ADVANCED_FACE ( 'NONE', ( #40178 ), #138753, .F. ) ;
#66130 = VECTOR ( 'NONE', #47865, 1000.000000000000000 ) ;
#66131 = CARTESIAN_POINT ( 'NONE',  ( 12.69999999999999574, -27.68200100598810565, 15.59110741220538188 ) ) ;
#66132 = CARTESIAN_POINT ( 'NONE',  ( 29.81706980810189478, -2.126176841940956130, 7.934999999999991616 ) ) ;
#66133 = AXIS2_PLACEMENT_3D ( 'NONE', #49985, #25352, #16611 ) ;
#66134 = CARTESIAN_POINT ( 'NONE',  ( 5.510786437626906675, -27.52281430457051314, 5.000000000000000000 ) ) ;
#66135 = ORIENTED_EDGE ( 'NONE', *, *, #124140, .T. ) ;
#66136 = CARTESIAN_POINT ( 'NONE',  ( 124.3079301918981230, -6.109999999999999432, 1.637169565754158507 ) ) ;
#66137 = VECTOR ( 'NONE', #15756, 1000.000000000000227 ) ;
#66138 = LINE ( 'NONE', #131379, #116045 ) ;
#66139 = LINE ( 'NONE', #35673, #58924 ) ;
#66140 = EDGE_CURVE ( 'NONE', #28852, #111481, #39450, .T. ) ;
#66142 = VERTEX_POINT ( 'NONE', #141603 ) ;
#66141 = CARTESIAN_POINT ( 'NONE',  ( 24.39999999999999858, 1.399999999999987699, -20.40202195861970580 ) ) ;
#66143 = DIRECTION ( 'NONE',  ( 1.000000000000000000, 0.000000000000000000, 0.000000000000000000 ) ) ;
#66144 = ORIENTED_EDGE ( 'NONE', *, *, #34171, .T. ) ;
#66145 = CARTESIAN_POINT ( 'NONE',  ( -14.51078643762690490, -27.52281430457045275, 5.000000000000000000 ) ) ;
#66146 = CARTESIAN_POINT ( 'NONE',  ( -28.18992724054673360, -22.22500000000000142, 7.552170838797634289 ) ) ;
#66147 = LINE ( 'NONE', #123392, #61187 ) ;
#66148 = EDGE_LOOP ( 'NONE', ( #86093, #134114, #119362 ) ) ;
#66149 = CARTESIAN_POINT ( 'NONE',  ( -8.207106781186482181, -14.24070752338413826, 5.000000000000000000 ) ) ;
#66150 = CARTESIAN_POINT ( 'NONE',  ( 1.499999999999990896, -2.173586137069138946, -4.605770156576107333 ) ) ;
#66151 = ADVANCED_FACE ( 'NONE', ( #119807 ), #83677, .F. ) ;
#66152 = ORIENTED_EDGE ( 'NONE', *, *, #21704, .F. ) ;
#66153 = CARTESIAN_POINT ( 'NONE',  ( -77.99451991528749772, 28.92564299267992567, 4.000000000000000000 ) ) ;
#66154 = DIRECTION ( 'NONE',  ( 2.781805975412906507E-17, 0.3543493200069153248, 0.9351131265310292928 ) ) ;
#66155 = ORIENTED_EDGE ( 'NONE', *, *, #22875, .F. ) ;
#66156 = CARTESIAN_POINT ( 'NONE',  ( 19.49999999999986500, 16.77039438581780928, 0.4657186855307289264 ) ) ;
#66158 = EDGE_LOOP ( 'NONE', ( #36862, #124873, #54003, #22157 ) ) ;
#66157 = DIRECTION ( 'NONE',  ( 0.7071067811865487940, 0.7071067811865463515, 0.000000000000000000 ) ) ;
#66159 = ORIENTED_EDGE ( 'NONE', *, *, #120953, .F. ) ;
#66160 = CARTESIAN_POINT ( 'NONE',  ( -22.49999999999984723, -15.29013452822856323, 0.3645803511609828629 ) ) ;
#66161 = CARTESIAN_POINT ( 'NONE',  ( -4.499999999999968914, -4.216083040037257312, -7.486842126848645584 ) ) ;
#66162 = ORIENTED_EDGE ( 'NONE', *, *, #40573, .T. ) ;
#66163 = EDGE_CURVE ( 'NONE', #89577, #127256, #51748, .T. ) ;
#66164 = LINE ( 'NONE', #111038, #143114 ) ;
#66165 = CARTESIAN_POINT ( 'NONE',  ( -32.99999999999976552, 13.93112307739204248, 4.000000000000000000 ) ) ;
#66166 = DIRECTION ( 'NONE',  ( 0.7071067811865487940, 0.7071067811865463515, 0.000000000000000000 ) ) ;
#66167 = EDGE_LOOP ( 'NONE', ( #27247, #27831, #33068, #68695 ) ) ;
#66168 = DIRECTION ( 'NONE',  ( 1.000000000000000000, 0.000000000000000000, 0.000000000000000000 ) ) ;
#66169 = EDGE_CURVE ( 'NONE', #91146, #5100, #129272, .T. ) ;
#66170 = DIRECTION ( 'NONE',  ( -0.000000000000000000, 0.000000000000000000, 1.000000000000000000 ) ) ;
#66171 = CARTESIAN_POINT ( 'NONE',  ( -10.49999999999992539, -11.56887692260769640, 4.000000000000000000 ) ) ;
#66172 = CARTESIAN_POINT ( 'NONE',  ( -74.99451991528749772, 28.92564299267990435, 4.000000000000000000 ) ) ;
#66173 = CARTESIAN_POINT ( 'NONE',  ( 29.07876352523144803, -7.482591942790327058E-16, 6.109999999999999432 ) ) ;
#66174 = LINE ( 'NONE', #76327, #51230 ) ;
#66175 = ORIENTED_EDGE ( 'NONE', *, *, #3693, .F. ) ;
#66176 = ORIENTED_EDGE ( 'NONE', *, *, #69709, .T. ) ;
#66177 = PRESENTATION_STYLE_ASSIGNMENT (( #23350 ) ) ;
#66178 = ORIENTED_EDGE ( 'NONE', *, *, #130929, .T. ) ;
#66179 = EDGE_CURVE ( 'NONE', #74851, #2777, #76973, .T. ) ;
#66180 = ORIENTED_EDGE ( 'NONE', *, *, #125148, .F. ) ;
#66181 = CARTESIAN_POINT ( 'NONE',  ( 31.49999999999977263, -12.08601207473287253, -10.46905243149102027 ) ) ;
#66182 = CARTESIAN_POINT ( 'NONE',  ( -14.29289321881335262, -9.740707523384180888, 5.000000000000000000 ) ) ;
#66183 = EDGE_LOOP ( 'NONE', ( #49921, #97801, #126533, #17481 ) ) ;
#66184 = LINE ( 'NONE', #11031, #46291 ) ;
#66185 = CARTESIAN_POINT ( 'NONE',  ( 18.70710678118641468, 14.25929247661557042, 5.000000000000000000 ) ) ;
#66186 = LINE ( 'NONE', #56042, #118044 ) ;
#66187 = LINE ( 'NONE', #24102, #95119 ) ;
#66188 = CARTESIAN_POINT ( 'NONE',  ( 126.7295968585647614, -6.110000000000000320, -1.637169565754161393 ) ) ;
#66189 = ADVANCED_FACE ( 'NONE', ( #30716 ), #20498, .F. ) ;
#66190 = EDGE_LOOP ( 'NONE', ( #18995, #103541, #116628, #70915 ) ) ;
#66191 = DIRECTION ( 'NONE',  ( -0.7071067811865486830, -0.7071067811865464625, -0.000000000000000000 ) ) ;
#66192 =( LENGTH_UNIT ( ) NAMED_UNIT ( * ) SI_UNIT ( .MILLI., .METRE. ) );
#66193 = FACE_OUTER_BOUND ( 'NONE', #8179, .T. ) ;
#66194 = DIRECTION ( 'NONE',  ( -0.7071067811865487940, 0.7071067811865463515, -0.000000000000000000 ) ) ;
#66195 = PLANE ( 'NONE',  #89077 ) ;
#66196 = DIRECTION ( 'NONE',  ( -0.3543493200069162685, -0.000000000000000000, -0.9351131265310288487 ) ) ;
#66197 = DIRECTION ( 'NONE',  ( -1.000000000000000000, -0.000000000000000000, -0.000000000000000000 ) ) ;
#66198 = CARTESIAN_POINT ( 'NONE',  ( 51.99586038379622011, -3.974999999999998312, -6.884901960086286188 ) ) ;
#66199 = VECTOR ( 'NONE', #86190, 1000.000000000000000 ) ;
#66200 = DIRECTION ( 'NONE',  ( 2.781805975412906507E-17, 0.3543493200069153248, 0.9351131265310292928 ) ) ;
#66201 = LINE ( 'NONE', #132175, #92371 ) ;
#66202 = ORIENTED_EDGE ( 'NONE', *, *, #88190, .T. ) ;
#66203 = ORIENTED_EDGE ( 'NONE', *, *, #126556, .T. ) ;
#66204 = CARTESIAN_POINT ( 'NONE',  ( 43.43749999999998579, 5.819803920172573974, -5.819803920172572198 ) ) ;
#66205 = VECTOR ( 'NONE', #82285, 1000.000000000000000 ) ;
#66206 = CARTESIAN_POINT ( 'NONE',  ( -34.42500000000001137, -10.45860074219788416, 5.000000000000000000 ) ) ;
#66207 = CARTESIAN_POINT ( 'NONE',  ( -32.99451991528749062, 28.92564299267960948, 4.000000000000000000 ) ) ;
#66208 = ORIENTED_EDGE ( 'NONE', *, *, #140571, .T. ) ;
#66209 = PLANE ( 'NONE',  #57150 ) ;
#66210 = LINE ( 'NONE', #42323, #76970 ) ;
#66211 = CARTESIAN_POINT ( 'NONE',  ( 33.54209685856476852, 5.291415217122923842, -3.054999999999996163 ) ) ;
#66212 = ADVANCED_FACE ( 'NONE', ( #21946 ), #21238, .F. ) ;
#66214 = ORIENTED_EDGE ( 'NONE', *, *, #19912, .F. ) ;
#66213 = AXIS2_PLACEMENT_3D ( 'NONE', #59769, #70663, #3887 ) ;
#66215 = FACE_OUTER_BOUND ( 'NONE', #79528, .T. ) ;
#66216 = ORIENTED_EDGE ( 'NONE', *, *, #7630, .F. ) ;
#66217 = EDGE_LOOP ( 'NONE', ( #27754, #141187, #137734, #102865 ) ) ;
#66218 = FACE_OUTER_BOUND ( 'NONE', #87174, .T. ) ;
#66219 = DIRECTION ( 'NONE',  ( -0.000000000000000000, 0.3543493200069153248, 0.9351131265310292928 ) ) ;
#66220 = CARTESIAN_POINT ( 'NONE',  ( -8.843876922607519120, -22.22500000000000497, 4.000000000000000000 ) ) ;
#66221 = CARTESIAN_POINT ( 'NONE',  ( -27.18398860626900060, 28.73617430169806042, 5.000000000000000000 ) ) ;
#66223 = EDGE_CURVE ( 'NONE', #558, #48968, #97738, .T. ) ;
#66222 = ORIENTED_EDGE ( 'NONE', *, *, #67139, .T. ) ;
#66224 = LINE ( 'NONE', #109708, #90539 ) ;
#66226 = ORIENTED_EDGE ( 'NONE', *, *, #16802, .F. ) ;
#66225 = DIRECTION ( 'NONE',  ( 1.321231229586337907E-16, -0.9647414015272155474, 0.2631995976047525887 ) ) ;
#66227 = CARTESIAN_POINT ( 'NONE',  ( 84.29209685856477563, -5.291415217122921177, 3.054999999999999272 ) ) ;
#66228 = ADVANCED_FACE ( 'NONE', ( #121258 ), #132167, .F. ) ;
#66229 = FACE_OUTER_BOUND ( 'NONE', #46932, .T. ) ;
#66230 = CARTESIAN_POINT ( 'NONE',  ( 0.000000000000000000, 0.000000000000000000, 5.000000000000000000 ) ) ;
#66231 = FACE_OUTER_BOUND ( 'NONE', #70688, .T. ) ;
#66232 = CARTESIAN_POINT ( 'NONE',  ( 0.000000000000000000, 0.000000000000000000, 5.000000000000000000 ) ) ;
#66233 = VECTOR ( 'NONE', #94534, 1000.000000000000000 ) ;
#66234 = VECTOR ( 'NONE', #142353, 1000.000000000000000 ) ;
#66235 = ORIENTED_EDGE ( 'NONE', *, *, #9246, .F. ) ;
#66236 = DIRECTION ( 'NONE',  ( -0.7071067811865486830, -0.7071067811865464625, -0.000000000000000000 ) ) ;
#66237 = CARTESIAN_POINT ( 'NONE',  ( 71.07876352523146579, -7.482591942790325086E-16, 6.109999999999998543 ) ) ;
#66238 = CONICAL_SURFACE ( 'NONE', #61598, 2.500000000000000888, 0.9599310885968822538 ) ;
#66239 = CARTESIAN_POINT ( 'NONE',  ( 6.540657738503846907, 2.055000000000001048, 2.516649172247811554E-16 ) ) ;
#66240 = CARTESIAN_POINT ( 'NONE',  ( 15.29974487139158867, -27.71228299555216879, 4.000000000000000000 ) ) ;
#66241 = ORIENTED_EDGE ( 'NONE', *, *, #125676, .T. ) ;
#66242 = ORIENTED_EDGE ( 'NONE', *, *, #54143, .F. ) ;
#66243 = VECTOR ( 'NONE', #136398, 1000.000000000000000 ) ;
#66244 = DIRECTION ( 'NONE',  ( 0.7071067811865487940, -0.7071067811865463515, 0.000000000000000000 ) ) ;
#66245 =( NAMED_UNIT ( * ) PLANE_ANGLE_UNIT ( ) SI_UNIT ( $, .RADIAN. ) );
#66246 = VERTEX_POINT ( 'NONE', #121957 ) ;
#66247 = EDGE_CURVE ( 'NONE', #32991, #87440, #44456, .T. ) ;
#66248 = CARTESIAN_POINT ( 'NONE',  ( -34.92500000000001137, 15.00612307739177709, 4.000000000000000000 ) ) ;
#66249 = ORIENTED_EDGE ( 'NONE', *, *, #24865, .F. ) ;
#66250 = PLANE ( 'NONE',  #134913 ) ;
#66251 = DIRECTION ( 'NONE',  ( -0.7071067811865487940, 0.7071067811865463515, 0.000000000000000000 ) ) ;
#66252 = CARTESIAN_POINT ( 'NONE',  ( -1.499999999999987788, -19.91253812416055524, 4.000000000000000000 ) ) ;
#66253 = FACE_BOUND ( 'NONE', #8656, .T. ) ;
#66254 = DIRECTION ( 'NONE',  ( 0.7071067811865487940, 0.7071067811865463515, -0.000000000000000000 ) ) ;
#66255 = CARTESIAN_POINT ( 'NONE',  ( -4.499999999999974243, 21.43112307739196964, 4.000000000000000000 ) ) ;
#66256 = DIRECTION ( 'NONE',  ( 0.7071067811865487940, 0.7071067811865463515, 0.000000000000000000 ) ) ;
#66257 = PLANE ( 'NONE',  #8611 ) ;
#66259 = ORIENTED_EDGE ( 'NONE', *, *, #131848, .T. ) ;
#66258 = LINE ( 'NONE', #8253, #82875 ) ;
#66260 = DIRECTION ( 'NONE',  ( 0.000000000000000000, 0.000000000000000000, 1.000000000000000000 ) ) ;
#66261 = ITEM_DEFINED_TRANSFORMATION ( 'NONE', 'NONE', #81736,  #127880 ) ;
#66262 = VERTEX_POINT ( 'NONE', #34266 ) ;
#66264 = EDGE_LOOP ( 'NONE', ( #13689, #58804, #133224, #68370 ) ) ;
#66263 = EDGE_CURVE ( 'NONE', #22970, #90775, #123449, .T. ) ;
#66265 = CARTESIAN_POINT ( 'NONE',  ( 72.82876352523145158, 0.000000000000000000, -6.109999999999998543 ) ) ;
#66266 = ORIENTED_EDGE ( 'NONE', *, *, #11695, .F. ) ;
#66267 = DIRECTION ( 'NONE',  ( -0.000000000000000000, 0.3543493200069153248, 0.9351131265310292928 ) ) ;
#66268 =( BOUNDED_CURVE ( )  B_SPLINE_CURVE ( 3, ( #141777, #110526, #143179, #86678 ),
 .UNSPECIFIED., .F., .T. ) 
 B_SPLINE_CURVE_WITH_KNOTS ( ( 4, 4 ),
 ( 0.1773996044403679528, 1.570796326794896558 ),
 .UNSPECIFIED. ) 
 CURVE ( )  GEOMETRIC_REPRESENTATION_ITEM ( )  RATIONAL_B_SPLINE_CURVE ( ( 1.000000000000000000, 0.8446433258982463110, 0.8446433258982463110, 1.000000000000000000 ) ) 
 REPRESENTATION_ITEM ( '' )  );
#66269 = CARTESIAN_POINT ( 'NONE',  ( 31.49999999999977263, 16.08746187583908949, 4.000000000000000000 ) ) ;
#66270 = EDGE_CURVE ( 'NONE', #136439, #106829, #46863, .T. ) ;
#66271 = ORIENTED_EDGE ( 'NONE', *, *, #2449, .F. ) ;
#66272 = PLANE ( 'NONE',  #72282 ) ;
#66273 = EDGE_CURVE ( 'NONE', #97224, #94242, #22628, .T. ) ;
#66274 = EDGE_CURVE ( 'NONE', #109576, #111037, #32119, .T. ) ;
#66275 = CARTESIAN_POINT ( 'NONE',  ( 30.77004279457771574, 21.73644205237998150, 5.000000000000000888 ) ) ;
#66276 = DIRECTION ( 'NONE',  ( 0.7071067811865487940, 0.7071067811865463515, -0.000000000000000000 ) ) ;
#66277 = DIRECTION ( 'NONE',  ( 1.000000000000000000, 0.000000000000000000, -0.000000000000000000 ) ) ;
#66278 = CARTESIAN_POINT ( 'NONE',  ( -6.328169399223490643, 5.259292476615663681, 4.000000000000000000 ) ) ;
#66279 = DIRECTION ( 'NONE',  ( 0.000000000000000000, -1.000000000000000000, 0.000000000000000000 ) ) ;
#66280 = FACE_OUTER_BOUND ( 'NONE', #10489, .T. ) ;
#66281 = VERTEX_POINT ( 'NONE', #66894 ) ;
#66282 = VECTOR ( 'NONE', #22099, 1000.000000000000000 ) ;
#66283 = DIRECTION ( 'NONE',  ( -0.000000000000000000, 0.3543493200069153248, 0.9351131265310292928 ) ) ;
#66284 = VERTEX_POINT ( 'NONE', #111074 ) ;
#66285 = DIRECTION ( 'NONE',  ( 0.7071067811865486830, -0.7071067811865464625, -0.000000000000000000 ) ) ;
#66286 = ORIENTED_EDGE ( 'NONE', *, *, #31110, .F. ) ;
#66287 = ORIENTED_EDGE ( 'NONE', *, *, #124678, .F. ) ;
#66289 = EDGE_CURVE ( 'NONE', #110269, #128513, #45177, .T. ) ;
#66288 = DIRECTION ( 'NONE',  ( 0.7071067811865486830, -0.7071067811865464625, -0.000000000000000000 ) ) ;
#66290 = EDGE_CURVE ( 'NONE', #92018, #3467, #61649, .T. ) ;
#66291 = PLANE ( 'NONE',  #127220 ) ;
#66292 = ORIENTED_EDGE ( 'NONE', *, *, #101358, .T. ) ;
#66293 = CARTESIAN_POINT ( 'NONE',  ( 131.5423521607622774, -49.05583548141699168, -39.86617647058817226 ) ) ;
#66294 =( BOUNDED_CURVE ( )  B_SPLINE_CURVE ( 2, ( #38527, #27631, #93625, #114637, #104479, #3705, #69029, #50126, #59587, #103748, #49436, #103072, #82752 ),
 .UNSPECIFIED., .F., .T. ) 
 B_SPLINE_CURVE_WITH_KNOTS ( ( 3, 2, 2, 2, 2, 2, 3 ),
 ( 0.9499999999999999556, 0.9527777777777777235, 0.9555555555555556024, 0.9583333333333333703, 0.9611111111111111382, 0.9638888888888889062, 0.9666666666666666741 ),
 .UNSPECIFIED. ) 
 CURVE ( )  GEOMETRIC_REPRESENTATION_ITEM ( )  RATIONAL_B_SPLINE_CURVE ( ( 1.000000000000000000, 0.9659258262890683122, 1.000000000000000000, 0.9659258262890683122, 1.000000000000000000, 0.9659258262890683122, 1.000000000000000000, 0.9659258262890683122, 1.000000000000000000, 0.9659258262890683122, 1.000000000000000000, 0.9659258262890683122, 1.000000000000000000 ) ) 
 REPRESENTATION_ITEM ( '' )  );
#66295 = AXIS2_PLACEMENT_3D ( 'NONE', #59165, #89604, #122218 ) ;
#66296 = LINE ( 'NONE', #110468, #30475 ) ;
#66297 = CARTESIAN_POINT ( 'NONE',  ( 28.19163961620376924, 6.094999999999988205, -1.633150327867694651 ) ) ;
#66298 = CARTESIAN_POINT ( 'NONE',  ( 13.39767433127539498, 6.360963242914233540, -31.21237421153560021 ) ) ;
#66299 = EDGE_CURVE ( 'NONE', #40076, #85488, #56776, .T. ) ;
#66300 = EDGE_LOOP ( 'NONE', ( #125586, #22228, #118021, #29031, #37971 ) ) ;
#66301 = VECTOR ( 'NONE', #36801, 1000.000000000000000 ) ;
#66302 = PLANE ( 'NONE',  #80437 ) ;
#66303 = ORIENTED_EDGE ( 'NONE', *, *, #55831, .T. ) ;
#66304 = CARTESIAN_POINT ( 'NONE',  ( -26.99999999999981526, 7.931123077392106424, 4.000000000000000000 ) ) ;
#66305 = CARTESIAN_POINT ( 'NONE',  ( 0.000000000000000000, -21.72500000000000142, 4.500000000000000888 ) ) ;
#66306 = ADVANCED_FACE ( 'NONE', ( #109674 ), #13908, .F. ) ;
#66308 = VERTEX_POINT ( 'NONE', #103769 ) ;
#66307 = PLANE ( 'NONE',  #118859 ) ;
#66309 = VERTEX_POINT ( 'NONE', #91511 ) ;
#66310 = DIRECTION ( 'NONE',  ( -0.7071067811865486830, -0.7071067811865464625, 0.000000000000000000 ) ) ;
#66311 = CARTESIAN_POINT ( 'NONE',  ( 6.489213562373093325, -27.52281430457059841, 5.000000000000000000 ) ) ;
#66312 = PLANE ( 'NONE',  #104994 ) ;
#66313 = ORIENTED_EDGE ( 'NONE', *, *, #138809, .T. ) ;
#66314 = FACE_OUTER_BOUND ( 'NONE', #25299, .T. ) ;
#66315 = EDGE_LOOP ( 'NONE', ( #110162, #118325, #24669 ) ) ;
#66316 = VECTOR ( 'NONE', #53405, 1000.000000000000114 ) ;
#66317 = CARTESIAN_POINT ( 'NONE',  ( -34.42500000000001137, 13.54139925780187603, 5.000000000000000000 ) ) ;
#66318 =( NAMED_UNIT ( * ) PLANE_ANGLE_UNIT ( ) SI_UNIT ( $, .RADIAN. ) );
#66319 = CARTESIAN_POINT ( 'NONE',  ( 1.199999999999999956, 0.000000000000000000, 4.582731094065999322 ) ) ;
#66320 = EDGE_CURVE ( 'NONE', #14802, #11535, #37855, .T. ) ;
#66321 = DIRECTION ( 'NONE',  ( -0.000000000000000000, 0.3543493200069153248, 0.9351131265310292928 ) ) ;
#66322 = FILL_AREA_STYLE ('',( #121385 ) ) ;
#66323 = CARTESIAN_POINT ( 'NONE',  ( 129.0581452878471680, 0.000000000000000000, -7.029999999999999361 ) ) ;
#66324 = CARTESIAN_POINT ( 'NONE',  ( 0.000000000000000000, 0.000000000000000000, 5.000000000000000000 ) ) ;
#66325 = CIRCLE ( 'NONE', #91751, 2.500000000000000444 ) ;
#66326 = DIRECTION ( 'NONE',  ( -1.000000000000000000, -0.000000000000000000, -0.000000000000000000 ) ) ;
#66327 = EDGE_LOOP ( 'NONE', ( #36757, #109710, #22549, #93667 ) ) ;
#66328 = CARTESIAN_POINT ( 'NONE',  ( 8.994519915287490619, 28.92564299267944250, 4.000000000000000000 ) ) ;
#66329 = ADVANCED_FACE ( 'NONE', ( #124836 ), #125570, .F. ) ;
#66330 = VERTEX_POINT ( 'NONE', #27653 ) ;
#66331 = EDGE_CURVE ( 'NONE', #108671, #113821, #48715, .T. ) ;
#66332 = DIRECTION ( 'NONE',  ( 0.7071067811865486830, -0.7071067811865464625, -0.000000000000000000 ) ) ;
#66333 = AXIS2_PLACEMENT_3D ( 'NONE', #47535, #61271, #38052 ) ;
#66334 = VECTOR ( 'NONE', #137205, 1000.000000000000114 ) ;
#66335 = ADVANCED_FACE ( 'NONE', ( #115343 ), #47342, .F. ) ;
#66336 = SURFACE_STYLE_USAGE ( .BOTH. , #13337 ) ;
#66337 = CARTESIAN_POINT ( 'NONE',  ( 8.999999999999937828, 10.93112307739207267, 4.000000000000000000 ) ) ;
#66338 = VECTOR ( 'NONE', #3351, 1000.000000000000227 ) ;
#66339 = EDGE_LOOP ( 'NONE', ( #113399, #65615, #28028, #132517 ) ) ;
#66340 = CARTESIAN_POINT ( 'NONE',  ( -34.92500000000001137, -5.143876922607502955, 4.000000000000000000 ) ) ;
#66341 = DIRECTION ( 'NONE',  ( 0.3543493200069162685, -0.000000000000000000, -0.9351131265310288487 ) ) ;
#66342 = CARTESIAN_POINT ( 'NONE',  ( -11.51078643762690490, -27.52281430457047406, 5.000000000000000000 ) ) ;
#66343 = ORIENTED_EDGE ( 'NONE', *, *, #97819, .T. ) ;
#66344 = SURFACE_STYLE_FILL_AREA ( #22085 ) ;
#66345 = DIRECTION ( 'NONE',  ( 0.000000000000000000, -1.000000000000000000, -0.000000000000000000 ) ) ;
#66346 = LINE ( 'NONE', #88085, #16836 ) ;
#66347 = CARTESIAN_POINT ( 'NONE',  ( 4.828169399223496860, -5.240707523384231514, 4.000000000000000000 ) ) ;
#66348 = CARTESIAN_POINT ( 'NONE',  ( 61.89126352523144448, -4.472830434245839371, -4.472830434245839371 ) ) ;
#66349 = DIRECTION ( 'NONE',  ( -0.7071067811865486830, 0.7071067811865464625, 0.000000000000000000 ) ) ;
#66350 = DIRECTION ( 'NONE',  ( -0.7071067811865486830, -0.7071067811865464625, -0.000000000000000000 ) ) ;
#66351 = CARTESIAN_POINT ( 'NONE',  ( -13.82816939922344091, 9.759292476615621936, 4.000000000000000000 ) ) ;
#66352 = CARTESIAN_POINT ( 'NONE',  ( 83.24999999999998579, -9.735942053221458872E-16, 7.950000000000000178 ) ) ;
#66353 = EDGE_LOOP ( 'NONE', ( #131978, #110533, #3067, #137335 ) ) ;
#66354 = LINE ( 'NONE', #101091, #106740 ) ;
#66355 = ORIENTED_EDGE ( 'NONE', *, *, #42869, .T. ) ;
#66356 = DIRECTION ( 'NONE',  ( -0.000000000000000000, -0.3543493200069152693, 0.9351131265310292928 ) ) ;
#66357 = FACE_OUTER_BOUND ( 'NONE', #127908, .T. ) ;
#66358 = DIRECTION ( 'NONE',  ( 0.000000000000000000, -1.000000000000000000, 0.000000000000000000 ) ) ;
#66359 = DIRECTION ( 'NONE',  ( -1.000000000000000000, -0.000000000000000000, -0.000000000000000000 ) ) ;
#66360 = FACE_OUTER_BOUND ( 'NONE', #95721, .T. ) ;
#66361 = DIRECTION ( 'NONE',  ( -0.7071067811865486830, 0.7071067811865464625, 0.000000000000000000 ) ) ;
#66362 = ORIENTED_EDGE ( 'NONE', *, *, #95376, .F. ) ;
#66363 = ORIENTED_EDGE ( 'NONE', *, *, #141278, .F. ) ;
#66364 = CARTESIAN_POINT ( 'NONE',  ( -7.251544128675710965, -11.24070752338417201, 10.39518518046010698 ) ) ;
#66365 = CARTESIAN_POINT ( 'NONE',  ( 26.80526891258047328, -5.499261314031188341, -3.175000000000002487 ) ) ;
#66366 = UNCERTAINTY_MEASURE_WITH_UNIT (LENGTH_MEASURE( 1.000000000000000082E-05 ), #12189, 'distance_accuracy_value', 'NONE');
#66367 = CARTESIAN_POINT ( 'NONE',  ( -24.29974487139158867, -27.71228299555223273, 4.000000000000000000 ) ) ;
#66368 = DIRECTION ( 'NONE',  ( -0.000000000000000000, -0.3543493200069152693, 0.9351131265310292928 ) ) ;
#66369 = CARTESIAN_POINT ( 'NONE',  ( 82.03752705046288440, -9.735942053221456900E-16, 7.949999999999998401 ) ) ;
#66370 = FACE_OUTER_BOUND ( 'NONE', #82733, .T. ) ;
#66371 = VECTOR ( 'NONE', #81108, 1000.000000000000000 ) ;
#66372 = DIRECTION ( 'NONE',  ( 0.000000000000000000, -1.000000000000000000, 0.000000000000000000 ) ) ;
#66373 = ORIENTED_EDGE ( 'NONE', *, *, #29910, .T. ) ;
#66374 = CARTESIAN_POINT ( 'NONE',  ( 69.97916666666665719, -7.950000000000001066, 2.130196079827424427 ) ) ;
#66375 = DIRECTION ( 'NONE',  ( 0.6830127018922181881, 0.6830127018922202975, -0.2588190451025214056 ) ) ;
#66376 = CARTESIAN_POINT ( 'NONE',  ( -0.3281693992235185098, 5.259292476615672562, 4.000000000000000000 ) ) ;
#66377 = LINE ( 'NONE', #68532, #40565 ) ;
#66378 = VECTOR ( 'NONE', #14493, 1000.000000000000000 ) ;
#66379 = VERTEX_POINT ( 'NONE', #137153 ) ;
#66380 = CARTESIAN_POINT ( 'NONE',  ( -33.48921356237309510, -27.52281430457078670, 5.000000000000000000 ) ) ;
#66381 = ORIENTED_EDGE ( 'NONE', *, *, #57929, .F. ) ;
#66382 = LINE ( 'NONE', #22128, #88212 ) ;
#66383 = CARTESIAN_POINT ( 'NONE',  ( 78.31293019189810423, -1.637169565754159617, -6.110000000000001208 ) ) ;
#66384 = DIRECTION ( 'NONE',  ( 0.6830127018922180770, -0.6830127018922204085, -0.2588190451025213501 ) ) ;
#66385 = VECTOR ( 'NONE', #74928, 1000.000000000000000 ) ;
#66386 = ORIENTED_EDGE ( 'NONE', *, *, #81553, .T. ) ;
#66387 = CARTESIAN_POINT ( 'NONE',  ( 8.816011393731004731, 28.73617430169781173, 5.000000000000000000 ) ) ;
#66388 = LINE ( 'NONE', #87424, #26790 ) ;
#66389 = DIRECTION ( 'NONE',  ( -1.000000000000000000, -1.224606353822377258E-16, -0.000000000000000000 ) ) ;
#66390 = VECTOR ( 'NONE', #63065, 1000.000000000000227 ) ;
#66391 = CARTESIAN_POINT ( 'NONE',  ( -24.28001967989388632, 0.7592924766157104211, 14.27032725228003329 ) ) ;
#66392 = EDGE_CURVE ( 'NONE', #130071, #137119, #25510, .T. ) ;
#66393 = CARTESIAN_POINT ( 'NONE',  ( 3.000000000000000000, 0.9892420537897061994, -14.41609864557725729 ) ) ;
#66395 = VERTEX_POINT ( 'NONE', #37110 ) ;
#66394 = CARTESIAN_POINT ( 'NONE',  ( -14.99999999999990230, -0.2811185226894407085, -5.995736974527478225 ) ) ;
#66396 = ADVANCED_FACE ( 'NONE', ( #136416 ), #82090, .F. ) ;
#66397 = CARTESIAN_POINT ( 'NONE',  ( 48.18398860626899705, 28.73617430169820608, 5.000000000000000000 ) ) ;
#66398 = PLANE ( 'NONE',  #137939 ) ;
#66399 = CARTESIAN_POINT ( 'NONE',  ( 77.12500000000000000, -7.950000000000000178, -4.867971026610729436E-16 ) ) ;
#66400 = DIRECTION ( 'NONE',  ( 0.7071067811865487940, -0.7071067811865463515, 0.000000000000000000 ) ) ;
#66401 = ORIENTED_EDGE ( 'NONE', *, *, #55235, .F. ) ;
#66402 = AXIS2_PLACEMENT_3D ( 'NONE', #114041, #116894, #14732 ) ;
#66403 = ORIENTED_EDGE ( 'NONE', *, *, #110521, .T. ) ;
#66404 = CARTESIAN_POINT ( 'NONE',  ( 63.87543019189810423, -5.291415217122920289, -3.055000000000001492 ) ) ;
#66405 = EDGE_LOOP ( 'NONE', ( #68061, #42791, #109592, #116943 ) ) ;
#66406 = AXIS2_PLACEMENT_3D ( 'NONE', #44712, #78015, #24329 ) ;
#66407 = ADVANCED_FACE ( 'NONE', ( #35734 ), #60325, .F. ) ;
#66408 = DIRECTION ( 'NONE',  ( 0.3543493200069162685, -0.000000000000000000, -0.9351131265310288487 ) ) ;
#66409 = LINE ( 'NONE', #112050, #17882 ) ;
#66410 = CARTESIAN_POINT ( 'NONE',  ( 0.000000000000000000, -21.72500000000000142, 4.500000000000000888 ) ) ;
#66411 = CARTESIAN_POINT ( 'NONE',  ( 125.4979281168462961, -3.948843003177505473, -6.900003709242945149 ) ) ;
#66412 = DIRECTION ( 'NONE',  ( -0.7071067811865486830, -0.7071067811865464625, 0.000000000000000000 ) ) ;
#66413 = ORIENTED_EDGE ( 'NONE', *, *, #33154, .T. ) ;
#66414 = EDGE_LOOP ( 'NONE', ( #58622, #44708, #11609, #101249 ) ) ;
#66415 = CARTESIAN_POINT ( 'NONE',  ( 6.005480084712508493, 28.92564299267933947, 4.000000000000000000 ) ) ;
#66416 = CARTESIAN_POINT ( 'NONE',  ( 9.591592354503321260, 3.061616997868378211E-16, -2.500000000000001332 ) ) ;
#66417 = EDGE_CURVE ( 'NONE', #75931, #128706, #50609, .T. ) ;
#66418 = VERTEX_POINT ( 'NONE', #14653 ) ;
#66419 = DIRECTION ( 'NONE',  ( -0.3543493200069162685, -0.000000000000000000, -0.9351131265310288487 ) ) ;
#66420 = DIRECTION ( 'NONE',  ( 0.7071067811865486830, -0.7071067811865464625, -0.000000000000000000 ) ) ;
#66421 = CARTESIAN_POINT ( 'NONE',  ( -5.207106781186495503, -20.24070752338407431, 5.000000000000000000 ) ) ;
#66422 = EDGE_CURVE ( 'NONE', #117563, #90351, #56160, .T. ) ;
#66423 = ORIENTED_EDGE ( 'NONE', *, *, #64767, .T. ) ;
#66424 = VECTOR ( 'NONE', #17011, 1000.000000000000000 ) ;
#66425 = FACE_BOUND ( 'NONE', #77552, .T. ) ;
#66426 = CARTESIAN_POINT ( 'NONE',  ( -34.92500000000001137, -22.22500000000000142, 4.000000000000000000 ) ) ;
#66427 = CARTESIAN_POINT ( 'NONE',  ( -18.29974487139159223, -27.71228299555219010, 4.000000000000000000 ) ) ;
#66428 = DIRECTION ( 'NONE',  ( 1.000000000000000000, 0.000000000000000000, 0.000000000000000000 ) ) ;
#66429 = EDGE_CURVE ( 'NONE', #72171, #4761, #3727, .T. ) ;
#66430 = EDGE_CURVE ( 'NONE', #3531, #60140, #105227, .T. ) ;
#66431 = AXIS2_PLACEMENT_3D ( 'NONE', #88169, #132419, #85279 ) ;
#66432 = VECTOR ( 'NONE', #99357, 1000.000000000000227 ) ;
#66433 = FILL_AREA_STYLE ('',( #121493 ) ) ;
#66434 = ORIENTED_EDGE ( 'NONE', *, *, #141453, .T. ) ;
#66435 = VECTOR ( 'NONE', #117160, 1000.000000000000000 ) ;
#66436 = EDGE_LOOP ( 'NONE', ( #3617, #47671, #129170, #5889 ) ) ;
#66437 = CARTESIAN_POINT ( 'NONE',  ( 100.2454301918981230, -5.291415217122918513, -3.055000000000000160 ) ) ;
#66438 = ORIENTED_EDGE ( 'NONE', *, *, #119900, .T. ) ;
#66439 = ORIENTED_EDGE ( 'NONE', *, *, #24351, .F. ) ;
#66440 = EDGE_CURVE ( 'NONE', #123646, #141302, #15326, .T. ) ;
#66441 = VECTOR ( 'NONE', #99148, 1000.000000000000000 ) ;
#66442 = VECTOR ( 'NONE', #72682, 1000.000000000000000 ) ;
#66443 = LINE ( 'NONE', #22181, #21527 ) ;
#66444 = CARTESIAN_POINT ( 'NONE',  ( -9.489213562373095101, -27.52281430457062328, 5.000000000000000000 ) ) ;
#66445 = ADVANCED_FACE ( 'NONE', ( #6577 ), #107363, .F. ) ;
#66446 = ADVANCED_FACE ( 'NONE', ( #139321 ), #110025, .F. ) ;
#66447 = DIRECTION ( 'NONE',  ( 0.000000000000000000, -1.000000000000000000, 0.000000000000000000 ) ) ;
#66448 = EDGE_LOOP ( 'NONE', ( #42200, #123672, #30524, #131031 ) ) ;
#66449 = DIRECTION ( 'NONE',  ( 0.7071067811865487940, 0.7071067811865463515, -0.000000000000000000 ) ) ;
#66450 = DIRECTION ( 'NONE',  ( -1.000000000000000000, -0.000000000000000000, -0.000000000000000000 ) ) ;
#66451 = DIRECTION ( 'NONE',  ( -0.7071067811865487940, 0.7071067811865463515, -0.000000000000000000 ) ) ;
#66453 = DIRECTION ( 'NONE',  ( 0.6830127018922180770, -0.6830127018922204085, -0.2588190451025213501 ) ) ;
#66452 = CARTESIAN_POINT ( 'NONE',  ( -6.299744871391586898, -27.71228299555210484, 4.000000000000000000 ) ) ;
#66454 = DIRECTION ( 'NONE',  ( -0.3543493200069162685, -0.000000000000000000, -0.9351131265310288487 ) ) ;
#66455 = CARTESIAN_POINT ( 'NONE',  ( 0.000000000000000000, 0.000000000000000000, 5.000000000000000000 ) ) ;
#66456 = ORIENTED_EDGE ( 'NONE', *, *, #130779, .T. ) ;
#66457 = EDGE_CURVE ( 'NONE', #12864, #31545, #16787, .T. ) ;
#66458 = CARTESIAN_POINT ( 'NONE',  ( 88.35416666666665719, -2.130196079827463507, -7.949999999999979750 ) ) ;
#66459 = CARTESIAN_POINT ( 'NONE',  ( 3.398789304146614398, -2.055000000000000160, 0.000000000000000000 ) ) ;
#66460 = VERTEX_POINT ( 'NONE', #88306 ) ;
#66461 = EDGE_LOOP ( 'NONE', ( #111337, #55608, #45591, #103409 ) ) ;
#66462 = EDGE_CURVE ( 'NONE', #90802, #49877, #95773, .T. ) ;
#66464 = ORIENTED_EDGE ( 'NONE', *, *, #143484, .F. ) ;
#66463 = ADVANCED_FACE ( 'NONE', ( #106622 ), #71922, .F. ) ;
#66465 = CARTESIAN_POINT ( 'NONE',  ( 54.25043019189811133, 3.055000000000002824, -5.291415217122919401 ) ) ;
#66466 = VECTOR ( 'NONE', #117232, 1000.000000000000000 ) ;
#66467 = ORIENTED_EDGE ( 'NONE', *, *, #30997, .T. ) ;
#66468 = LINE ( 'NONE', #110632, #58301 ) ;
#66469 = AXIS2_PLACEMENT_3D ( 'NONE', #16099, #71980, #94401 ) ;
#66470 = CARTESIAN_POINT ( 'NONE',  ( 0.9208062828704389746, 3.047499999999997655, 5.278424836066143655 ) ) ;
#66471 = CARTESIAN_POINT ( 'NONE',  ( 98.72959685856477563, -6.110000000000000320, -1.637169565754161393 ) ) ;
#66472 = CARTESIAN_POINT ( 'NONE',  ( 19.83957586139685247, 9.091547215995101183, 4.000000000000000000 ) ) ;
#66473 = EDGE_CURVE ( 'NONE', #63744, #117579, #28394, .T. ) ;
#66474 = ORIENTED_EDGE ( 'NONE', *, *, #24057, .F. ) ;
#66475 = DIRECTION ( 'NONE',  ( 0.7071067811865487940, 0.7071067811865463515, 0.000000000000000000 ) ) ;
#66476 = VECTOR ( 'NONE', #101065, 1000.000000000000000 ) ;
#66477 = ADVANCED_FACE ( 'NONE', ( #21611 ), #32495, .F. ) ;
#66478 = PLANE ( 'NONE',  #84131 ) ;
#66479 = CARTESIAN_POINT ( 'NONE',  ( 25.39999999999999858, 0.000000000000000000, 0.000000000000000000 ) ) ;
#66480 = DIRECTION ( 'NONE',  ( -0.7071067811865486830, 0.7071067811865464625, 0.000000000000000000 ) ) ;
#66481 = ORIENTED_EDGE ( 'NONE', *, *, #113676, .T. ) ;
#66482 = DIRECTION ( 'NONE',  ( 0.7071067811865487940, 0.7071067811865463515, 0.000000000000000000 ) ) ;
#66483 = VERTEX_POINT ( 'NONE', #84225 ) ;
#66484 = VERTEX_POINT ( 'NONE', #128421 ) ;
#66485 = ORIENTED_EDGE ( 'NONE', *, *, #87454, .F. ) ;
#66487 = VECTOR ( 'NONE', #3717, 1000.000000000000000 ) ;
#66486 = CARTESIAN_POINT ( 'NONE',  ( 120.5162635252314374, -4.472830434245838482, 4.472830434245838482 ) ) ;
#66488 = DIRECTION ( 'NONE',  ( 0.000000000000000000, 0.000000000000000000, 1.000000000000000000 ) ) ;
#66489 = VECTOR ( 'NONE', #57902, 1000.000000000000000 ) ;
#66490 = CARTESIAN_POINT ( 'NONE',  ( -10.39656807105350467, -14.24070752338413648, 19.24067776001723473 ) ) ;
#66491 = ORIENTED_EDGE ( 'NONE', *, *, #140761, .T. ) ;
#66492 = PLANE ( 'NONE',  #44232 ) ;
#66493 = VERTEX_POINT ( 'NONE', #54966 ) ;
#66494 = EDGE_CURVE ( 'NONE', #134557, #116711, #62456, .T. ) ;
#66495 = EDGE_CURVE ( 'NONE', #23600, #68847, #65869, .T. ) ;
#66496 = CARTESIAN_POINT ( 'NONE',  ( 11.20790314143521904, -6.871911579029513106, -3.967499999999993587 ) ) ;
#66497 = DIRECTION ( 'NONE',  ( -0.6830127018922180770, -0.6830127018922204085, -0.2588190451025213501 ) ) ;
#66498 = PLANE ( 'NONE',  #1978 ) ;
#66499 = VECTOR ( 'NONE', #40759, 1000.000000000000000 ) ;
#66500 = DIRECTION ( 'NONE',  ( -1.000000000000000000, -1.224606353822377258E-16, -0.000000000000000000 ) ) ;
#66501 = VERTEX_POINT ( 'NONE', #10692 ) ;
#66502 = ORIENTED_EDGE ( 'NONE', *, *, #125759, .T. ) ;
#66503 = ORIENTED_EDGE ( 'NONE', *, *, #97515, .T. ) ;
#66504 = CARTESIAN_POINT ( 'NONE',  ( 1.171830600776463838, -11.24070752338416845, 4.000000000000000000 ) ) ;
#66505 = LINE ( 'NONE', #123020, #104234 ) ;
#66506 = UNCERTAINTY_MEASURE_WITH_UNIT (LENGTH_MEASURE( 1.000000000000000082E-05 ), #60554, 'distance_accuracy_value', 'NONE');
#66507 = CARTESIAN_POINT ( 'NONE',  ( 0.000000000000000000, -8.616843969807042924, 0.000000000000000000 ) ) ;
#66508 = DIRECTION ( 'NONE',  ( -0.000000000000000000, -0.3543493200069152693, 0.9351131265310292928 ) ) ;
#66509 = CARTESIAN_POINT ( 'NONE',  ( -27.18398860626900060, 28.73617430169806042, 5.000000000000000000 ) ) ;
#66510 = DIRECTION ( 'NONE',  ( -1.000000000000000000, 0.000000000000000000, 0.000000000000000000 ) ) ;
#66511 = CARTESIAN_POINT ( 'NONE',  ( 69.18398860626899705, 28.73617430169835529, 5.000000000000000000 ) ) ;
#66512 = DIRECTION ( 'NONE',  ( -0.3543493200069162685, -0.000000000000000000, -0.9351131265310288487 ) ) ;
#66513 = ORIENTED_EDGE ( 'NONE', *, *, #42517, .T. ) ;
#66514 = DIRECTION ( 'NONE',  ( 0.7071067811865487940, 0.7071067811865463515, 0.000000000000000000 ) ) ;
#66515 = ORIENTED_EDGE ( 'NONE', *, *, #124051, .F. ) ;
#66516 = CARTESIAN_POINT ( 'NONE',  ( 3.792893218813432998, 6.759292476615651246, 5.000000000000000000 ) ) ;
#66517 = ORIENTED_EDGE ( 'NONE', *, *, #7309, .F. ) ;
#66518 = PLANE ( 'NONE',  #80738 ) ;
#66520 = ORIENTED_EDGE ( 'NONE', *, *, #141747, .T. ) ;
#66519 = PLANE ( 'NONE',  #32559 ) ;
#66521 = VECTOR ( 'NONE', #108621, 1000.000000000000000 ) ;
#66522 = DIRECTION ( 'NONE',  ( -0.7071067811865487940, 0.7071067811865463515, -0.000000000000000000 ) ) ;
#66523 = ORIENTED_EDGE ( 'NONE', *, *, #17378, .T. ) ;
#66524 = FACE_OUTER_BOUND ( 'NONE', #134282, .T. ) ;
#66525 = ORIENTED_EDGE ( 'NONE', *, *, #58628, .T. ) ;
#66526 = CARTESIAN_POINT ( 'NONE',  ( -44.99451991528749772, 28.92564299267969474, 4.000000000000000000 ) ) ;
#66527 = ORIENTED_EDGE ( 'NONE', *, *, #59446, .T. ) ;
#66528 = AXIS2_PLACEMENT_3D ( 'NONE', #56109, #77147, #32927 ) ;
#66529 = AXIS2_PLACEMENT_3D ( 'NONE', #74630, #51449, #39138 ) ;
#66530 = DIRECTION ( 'NONE',  ( -1.000000000000000000, -1.224606353822377258E-16, -0.000000000000000000 ) ) ;
#66532 = CARTESIAN_POINT ( 'NONE',  ( 115.7250270504628702, 5.819803920172573086, -5.819803920172572198 ) ) ;
#66531 = AXIS2_PLACEMENT_3D ( 'NONE', #92041, #89904, #58778 ) ;
#66533 = DIRECTION ( 'NONE',  ( 0.7071067811865486830, -0.7071067811865464625, -0.000000000000000000 ) ) ;
#66534 = DIRECTION ( 'NONE',  ( 0.7071067811865487940, 0.7071067811865463515, 0.000000000000000000 ) ) ;
#66535 = CARTESIAN_POINT ( 'NONE',  ( -35.99451991528749772, 28.92564299267963079, 4.000000000000000000 ) ) ;
#66536 = LINE ( 'NONE', #11383, #50820 ) ;
#66537 = CARTESIAN_POINT ( 'NONE',  ( 9.916666666666667851, 5.278424836066147208, 3.047499999999990550 ) ) ;
#66538 = CARTESIAN_POINT ( 'NONE',  ( 14.70790314143522082, -6.871911579029513106, -3.967499999999993587 ) ) ;
#66539 = VECTOR ( 'NONE', #136813, 1000.000000000000000 ) ;
#66540 = FACE_OUTER_BOUND ( 'NONE', #1326, .T. ) ;
#66541 = DIRECTION ( 'NONE',  ( 1.000000000000000000, 1.224606353822377258E-16, 0.000000000000000000 ) ) ;
#66542 = ORIENTED_EDGE ( 'NONE', *, *, #30562, .F. ) ;
#66543 = ORIENTED_EDGE ( 'NONE', *, *, #111896, .F. ) ;
#66544 = CARTESIAN_POINT ( 'NONE',  ( 45.18398860626900415, 28.73617430169818832, 5.000000000000000000 ) ) ;
#66545 = ORIENTED_EDGE ( 'NONE', *, *, #35233, .T. ) ;
#66546 = CARTESIAN_POINT ( 'NONE',  ( -18.18398860626898994, 28.73617430169800002, 5.000000000000000000 ) ) ;
#66547 = LINE ( 'NONE', #110718, #27812 ) ;
#66548 = CARTESIAN_POINT ( 'NONE',  ( -1.180000000000000604, 10.00000000000000178, 6.750000000000000888 ) ) ;
#66549 = ORIENTED_EDGE ( 'NONE', *, *, #17417, .T. ) ;
#66550 = CARTESIAN_POINT ( 'NONE',  ( 17.67183060077634948, 14.25929247661557397, 4.000000000000000000 ) ) ;
#66551 = LINE ( 'NONE', #131808, #118152 ) ;
#66552 =( BOUNDED_CURVE ( )  B_SPLINE_CURVE ( 2, ( #118611, #120750, #141071, #141823, #85993, #22141, #66399, #130951, #110569, #87434, #21457, #86723, #119314 ),
 .UNSPECIFIED., .F., .T. ) 
 B_SPLINE_CURVE_WITH_KNOTS ( ( 3, 2, 2, 2, 2, 2, 3 ),
 ( 0.4666666666666666741, 0.4694444444444444420, 0.4722222222222222099, 0.4749999999999999778, 0.4777777777777778012, 0.4805555555555555691, 0.4833333333333333370 ),
 .UNSPECIFIED. ) 
 CURVE ( )  GEOMETRIC_REPRESENTATION_ITEM ( )  RATIONAL_B_SPLINE_CURVE ( ( 1.000000000000000000, 0.9659258262890683122, 1.000000000000000000, 0.9659258262890683122, 1.000000000000000000, 0.9659258262890683122, 1.000000000000000000, 0.9659258262890683122, 1.000000000000000000, 0.9659258262890683122, 1.000000000000000000, 0.9659258262890683122, 1.000000000000000000 ) ) 
 REPRESENTATION_ITEM ( '' )  );
#66553 = EDGE_CURVE ( 'NONE', #69267, #130434, #138581, .T. ) ;
#66554 = LINE ( 'NONE', #14298, #28013 ) ;
#66555 = CARTESIAN_POINT ( 'NONE',  ( 24.48921356237309510, -27.52281430457072631, 5.000000000000000000 ) ) ;
#66556 = ADVANCED_FACE ( 'NONE', ( #78144 ), #14294, .T. ) ;
#66557 = ADVANCED_FACE ( 'NONE', ( #57832 ), #35374, .F. ) ;
#66558 = LINE ( 'NONE', #46999, #74957 ) ;
#66560 = ORIENTED_EDGE ( 'NONE', *, *, #109366, .T. ) ;
#66559 = CARTESIAN_POINT ( 'NONE',  ( -7.828169399223478209, 18.75929247661553134, 4.000000000000000000 ) ) ;
#66561 = PLANE ( 'NONE',  #120653 ) ;
#66562 = CARTESIAN_POINT ( 'NONE',  ( -33.18398860626899705, 28.73617430169810305, 5.000000000000000000 ) ) ;
#66563 = CARTESIAN_POINT ( 'NONE',  ( 2.999999999999987121, -1.447814304570818500, 5.000000000000000000 ) ) ;
#66564 = CARTESIAN_POINT ( 'NONE',  ( 36.18398860626899705, 28.73617430169812437, 5.000000000000000000 ) ) ;
#66565 = CARTESIAN_POINT ( 'NONE',  ( -72.29974487139158157, -27.71228299555256669, 4.000000000000000000 ) ) ;
#66566 = ADVANCED_FACE ( 'NONE', ( #45537 ), #36073, .F. ) ;
#66568 = VERTEX_POINT ( 'NONE', #22281 ) ;
#66567 = EDGE_CURVE ( 'NONE', #118822, #29420, #1463, .T. ) ;
#66569 = EDGE_LOOP ( 'NONE', ( #21089, #52998, #86195, #16829 ) ) ;
#66570 = ORIENTED_EDGE ( 'NONE', *, *, #89884, .F. ) ;
#66571 = CARTESIAN_POINT ( 'NONE',  ( 88.52126352523143282, -4.472830434245839371, -4.472830434245840259 ) ) ;
#66572 = STYLED_ITEM ( 'NONE', ( #47119 ), #34639 ) ;
#66573 = ORIENTED_EDGE ( 'NONE', *, *, #128471, .T. ) ;
#66574 = ADVANCED_FACE ( 'NONE', ( #101305 ), #134923, .T. ) ;
#66575 = DIRECTION ( 'NONE',  ( -0.6830127018922181881, 0.6830127018922202975, -0.2588190451025214056 ) ) ;
#66576 = LINE ( 'NONE', #121636, #91905 ) ;
#66577 = AXIS2_PLACEMENT_3D ( 'NONE', #44689, #47547, #56974 ) ;
#66578 = CARTESIAN_POINT ( 'NONE',  ( -8.999999999999932498, -15.41253812416059787, 4.000000000000000000 ) ) ;
#66579 = DIRECTION ( 'NONE',  ( -1.000000000000000000, -1.224606353822377258E-16, -0.000000000000000000 ) ) ;
#66580 = ORIENTED_EDGE ( 'NONE', *, *, #2889, .F. ) ;
#66581 = DIRECTION ( 'NONE',  ( -0.5735764363510503783, -0.8191520442889886899, 0.000000000000000000 ) ) ;
#66582 = CARTESIAN_POINT ( 'NONE',  ( 32.20710678118632586, 9.759292476615621936, 5.000000000000000000 ) ) ;
#66583 = EDGE_CURVE ( 'NONE', #65533, #41309, #102025, .T. ) ;
#66584 = CARTESIAN_POINT ( 'NONE',  ( 88.43293019189809456, 1.637169565754156508, 6.110000000000000320 ) ) ;
#66585 = ORIENTED_EDGE ( 'NONE', *, *, #131857, .T. ) ;
#66586 = CARTESIAN_POINT ( 'NONE',  ( 184.1500000000000057, -43.14999999999999147, -40.92499999999998295 ) ) ;
#66587 = VECTOR ( 'NONE', #26068, 1000.000000000000000 ) ;
#66588 = CARTESIAN_POINT ( 'NONE',  ( -30.79289321881324781, -20.24070752338407431, 5.000000000000000000 ) ) ;
#66589 = EDGE_CURVE ( 'NONE', #141779, #43430, #23753, .T. ) ;
#66590 = ORIENTED_EDGE ( 'NONE', *, *, #109095, .T. ) ;
#66591 = ORIENTED_EDGE ( 'NONE', *, *, #93787, .F. ) ;
#66592 = ORIENTED_EDGE ( 'NONE', *, *, #79086, .T. ) ;
#66593 = CARTESIAN_POINT ( 'NONE',  ( -13.49999999999991118, 12.43112307739206024, 4.000000000000000000 ) ) ;
#66594 = DIRECTION ( 'NONE',  ( 0.000000000000000000, -1.000000000000000000, 0.000000000000000000 ) ) ;
#66595 = CARTESIAN_POINT ( 'NONE',  ( 17.42123647476855908, -9.717572351234235426E-16, -7.934999999999990727 ) ) ;
#66596 = LINE ( 'NONE', #54313, #97400 ) ;
#66597 = EDGE_CURVE ( 'NONE', #8328, #58706, #91848, .T. ) ;
#66598 = CARTESIAN_POINT ( 'NONE',  ( 63.18398860626900415, 28.73617430169831621, 5.000000000000000000 ) ) ;
#66599 = LINE ( 'NONE', #110769, #46494 ) ;
#66600 = CARTESIAN_POINT ( 'NONE',  ( -51.18398860626899705, 28.73617430169823095, 5.000000000000000000 ) ) ;
#66601 = ORIENTED_EDGE ( 'NONE', *, *, #102841, .T. ) ;
#66602 = VECTOR ( 'NONE', #60955, 1000.000000000000000 ) ;
#66603 = ORIENTED_EDGE ( 'NONE', *, *, #67017, .F. ) ;
#66604 = CARTESIAN_POINT ( 'NONE',  ( 12.49289321881344605, -22.06289321881344634, -3.073261146000583341E-16 ) ) ;
#66605 = VERTEX_POINT ( 'NONE', #46991 ) ;
#66606 = VERTEX_POINT ( 'NONE', #56429 ) ;
#66607 = EDGE_CURVE ( 'NONE', #19355, #61417, #80298, .T. ) ;
#66608 = ADVANCED_FACE ( 'NONE', ( #44840 ), #112201, .F. ) ;
#66609 = LINE ( 'NONE', #19517, #130825 ) ;
#66610 = ORIENTED_EDGE ( 'NONE', *, *, #116199, .T. ) ;
#66611 = CARTESIAN_POINT ( 'NONE',  ( 0.000000000000000000, 0.000000000000000000, 5.000000000000000000 ) ) ;
#66612 = CARTESIAN_POINT ( 'NONE',  ( 12.18398860626900060, 28.73617430169795739, 5.000000000000000000 ) ) ;
#66613 = ADVANCED_FACE ( 'NONE', ( #25160 ), #110719, .F. ) ;
#66614 = CARTESIAN_POINT ( 'NONE',  ( -21.48921356237309155, -27.52281430457070499, 5.000000000000000000 ) ) ;
#66615 = DIRECTION ( 'NONE',  ( -0.000000000000000000, 0.000000000000000000, 1.000000000000000000 ) ) ;
#66616 = AXIS2_PLACEMENT_3D ( 'NONE', #124582, #25259, #122422 ) ;
#66617 = VERTEX_POINT ( 'NONE', #123799 ) ;
#66618 = EDGE_CURVE ( 'NONE', #102321, #13412, #69412, .T. ) ;
#66619 = LINE ( 'NONE', #55033, #90383 ) ;
#66620 = TOROIDAL_SURFACE ( 'NONE', #110562, 25.00000000000002487, 3.000000000000000000 ) ;
#66621 = VERTEX_POINT ( 'NONE', #113598 ) ;
#66622 = FACE_OUTER_BOUND ( 'NONE', #26959, .T. ) ;
#66623 = ORIENTED_EDGE ( 'NONE', *, *, #13533, .T. ) ;
#66624 = FACE_OUTER_BOUND ( 'NONE', #55961, .T. ) ;
#66625 = VERTEX_POINT ( 'NONE', #134678 ) ;
#66626 = LINE ( 'NONE', #10077, #101486 ) ;
#66627 = VERTEX_POINT ( 'NONE', #24454 ) ;
#66628 = EDGE_LOOP ( 'NONE', ( #799, #115772, #39022, #131058 ) ) ;
#66629 = AXIS2_PLACEMENT_3D ( 'NONE', #37566, #36827, #137585 ) ;
#66630 = ORIENTED_EDGE ( 'NONE', *, *, #86749, .T. ) ;
#66631 = CONICAL_SURFACE ( 'NONE', #43442, 2.500000000000000444, 0.9599310885968830309 ) ;
#66632 = CARTESIAN_POINT ( 'NONE',  ( 0.000000000000000000, 0.000000000000000000, 5.000000000000000000 ) ) ;
#66633 = LINE ( 'NONE', #91258, #18282 ) ;
#66634 = CARTESIAN_POINT ( 'NONE',  ( 15.48921356237309510, -27.52281430457066236, 5.000000000000000000 ) ) ;
#66635 = CARTESIAN_POINT ( 'NONE',  ( 125.4170968585647756, 3.054999999999998828, 5.291415217122922066 ) ) ;
#66636 = CARTESIAN_POINT ( 'NONE',  ( 13.49999999999990052, 16.18958161055404332, -11.56426086740808223 ) ) ;
#66637 = EDGE_CURVE ( 'NONE', #93700, #99074, #89030, .T. ) ;
#66638 = LINE ( 'NONE', #55053, #78362 ) ;
#66639 = DIRECTION ( 'NONE',  ( -0.7071067811865486830, -0.7071067811865464625, -0.000000000000000000 ) ) ;
#66640 = CARTESIAN_POINT ( 'NONE',  ( -9.707013264292978505, -21.74070752338405654, 4.999753212805220670 ) ) ;
#66641 =( NAMED_UNIT ( * ) SI_UNIT ( $, .STERADIAN. ) SOLID_ANGLE_UNIT ( ) );
#66642 = ORIENTED_EDGE ( 'NONE', *, *, #22790, .T. ) ;
#66644 = EDGE_CURVE ( 'NONE', #2187, #106533, #55681, .T. ) ;
#66643 = FACE_OUTER_BOUND ( 'NONE', #1994, .T. ) ;
#66645 = LINE ( 'NONE', #121002, #68077 ) ;
#66646 = VERTEX_POINT ( 'NONE', #51227 ) ;
#66647 = ORIENTED_EDGE ( 'NONE', *, *, #115258, .F. ) ;
#66648 = ORIENTED_EDGE ( 'NONE', *, *, #45372, .F. ) ;
#66649 = DIRECTION ( 'NONE',  ( 0.7071067811865487940, 0.7071067811865463515, 0.000000000000000000 ) ) ;
#66650 = ORIENTED_EDGE ( 'NONE', *, *, #44549, .T. ) ;
#66651 = ORIENTED_EDGE ( 'NONE', *, *, #33224, .F. ) ;
#66652 = DIRECTION ( 'NONE',  ( -1.000000000000000000, -0.000000000000000000, -0.000000000000000000 ) ) ;
#66653 = CARTESIAN_POINT ( 'NONE',  ( 14.62913961620377101, 5.278424836066147208, 3.047499999999990550 ) ) ;
#66654 = DIRECTION ( 'NONE',  ( -0.7071067811865486830, -0.7071067811865464625, 0.000000000000000000 ) ) ;
#66655 = EDGE_CURVE ( 'NONE', #88422, #93029, #26479, .T. ) ;
#66656 = DIRECTION ( 'NONE',  ( -0.7071067811865486830, -0.7071067811865464625, 0.000000000000000000 ) ) ;
#66657 = DIRECTION ( 'NONE',  ( -0.7071067811865486830, 0.7071067811865464625, 0.000000000000000000 ) ) ;
#66658 = ADVANCED_FACE ( 'NONE', ( #14995 ), #92544, .F. ) ;
#66659 = VERTEX_POINT ( 'NONE', #37498 ) ;
#66660 = VECTOR ( 'NONE', #141322, 1000.000000000000000 ) ;
#66661 = CARTESIAN_POINT ( 'NONE',  ( 51.18398860626899705, 28.73617430169823095, 5.000000000000000000 ) ) ;
#66662 = ORIENTED_EDGE ( 'NONE', *, *, #39052, .F. ) ;
#66663 = CARTESIAN_POINT ( 'NONE',  ( -10.82816939922344979, -17.24070752338410628, 4.000000000000000000 ) ) ;
#66664 = EDGE_CURVE ( 'NONE', #109399, #20187, #49093, .T. ) ;
#66665 = CARTESIAN_POINT ( 'NONE',  ( 16.54623647476855552, -7.934999999999990727, 4.858786175617117713E-16 ) ) ;
#66666 = ORIENTED_EDGE ( 'NONE', *, *, #58843, .T. ) ;
#66667 = CARTESIAN_POINT ( 'NONE',  ( 82.30793019189809456, -6.109999999999999432, 1.637169565754158507 ) ) ;
#66668 =( BOUNDED_CURVE ( )  B_SPLINE_CURVE ( 3, ( #58026, #125394, #48539, #5712 ),
 .UNSPECIFIED., .F., .T. ) 
 B_SPLINE_CURVE_WITH_KNOTS ( ( 4, 4 ),
 ( 5.005968288816736944, 5.074607125596340751 ),
 .UNSPECIFIED. ) 
 CURVE ( )  GEOMETRIC_REPRESENTATION_ITEM ( )  RATIONAL_B_SPLINE_CURVE ( ( 1.000000000000000000, 0.9996074310407765395, 0.9996074310407765395, 1.000000000000000000 ) ) 
 REPRESENTATION_ITEM ( '' )  );
#66669 = CARTESIAN_POINT ( 'NONE',  ( -3.792893218813431222, 3.759292476615678336, 5.000000000000000000 ) ) ;
#66670 = CARTESIAN_POINT ( 'NONE',  ( 0.3281693992235323876, -6.740707523384212863, 4.000000000000000000 ) ) ;
#66671 = ORIENTED_EDGE ( 'NONE', *, *, #101707, .T. ) ;
#66672 = ORIENTED_EDGE ( 'NONE', *, *, #26359, .F. ) ;
#66673 = VERTEX_POINT ( 'NONE', #81734 ) ;
#66674 = PLANE ( 'NONE',  #98225 ) ;
#66675 = DIRECTION ( 'NONE',  ( -1.000000000000000000, -1.224606353822377258E-16, -0.000000000000000000 ) ) ;
#66676 = CARTESIAN_POINT ( 'NONE',  ( 34.75611968250419181, -1.294349301475941072, 4.955485411084880276 ) ) ;
#66677 = CARTESIAN_POINT ( 'NONE',  ( 16.84504724602342662, -0.2737008427375496322, -34.33975653689201124 ) ) ;
#66678 = DIRECTION ( 'NONE',  ( -0.7071067811865487940, 0.7071067811865463515, 0.000000000000000000 ) ) ;
#66679 = DIRECTION ( 'NONE',  ( -0.6830127018922181881, 0.6830127018922202975, -0.2588190451025214056 ) ) ;
#66680 = ORIENTED_EDGE ( 'NONE', *, *, #108355, .F. ) ;
#66681 = FACE_OUTER_BOUND ( 'NONE', #78792, .T. ) ;
#66682 = EDGE_CURVE ( 'NONE', #72725, #17934, #59271, .T. ) ;
#66683 = CARTESIAN_POINT ( 'NONE',  ( 0.08314806772930470602, 21.75929247661549581, 7.311836541448051285 ) ) ;
#66684 = DIRECTION ( 'NONE',  ( 0.7071067811865487940, 0.7071067811865463515, 0.000000000000000000 ) ) ;
#66685 = ORIENTED_EDGE ( 'NONE', *, *, #6709, .F. ) ;
#66686 = CARTESIAN_POINT ( 'NONE',  ( -14.99999999999989164, -6.412538124160687580, 4.000000000000000000 ) ) ;
#66687 = PLANE ( 'NONE',  #16905 ) ;
#66688 = VERTEX_POINT ( 'NONE', #137517 ) ;
#66690 = VERTEX_POINT ( 'NONE', #59962 ) ;
#66689 = DIRECTION ( 'NONE',  ( 0.3543493200069162685, -0.000000000000000000, -0.9351131265310288487 ) ) ;
#66691 = EDGE_LOOP ( 'NONE', ( #75380, #137846, #142545, #36201 ) ) ;
#66692 = EDGE_CURVE ( 'NONE', #83448, #94185, #72302, .T. ) ;
#66693 = DIRECTION ( 'NONE',  ( -0.7071067811865486830, -0.7071067811865464625, -0.000000000000000000 ) ) ;
#66694 = DIRECTION ( 'NONE',  ( 0.7071067811865487940, 0.7071067811865463515, 0.000000000000000000 ) ) ;
#66695 = ORIENTED_EDGE ( 'NONE', *, *, #53833, .F. ) ;
#66696 = CARTESIAN_POINT ( 'NONE',  ( 63.48921356237309510, -27.52281430457099631, 5.000000000000000000 ) ) ;
#66697 = LINE ( 'NONE', #11556, #46267 ) ;
#66698 = VECTOR ( 'NONE', #19187, 1000.000000000000000 ) ;
#66699 = CARTESIAN_POINT ( 'NONE',  ( 4.171830600776447184, -2.240707523384257716, 4.000000000000000000 ) ) ;
#66700 = LINE ( 'NONE', #12300, #55903 ) ;
#66701 = DIRECTION ( 'NONE',  ( 0.6830127018922180770, -0.6830127018922204085, -0.2588190451025213501 ) ) ;
#66702 = PLANE ( 'NONE',  #114302 ) ;
#66703 = LINE ( 'NONE', #122482, #8947 ) ;
#66704 = CARTESIAN_POINT ( 'NONE',  ( 23.45790314143522437, 6.871911579029515771, 3.967499999999989146 ) ) ;
#66705 = FACE_OUTER_BOUND ( 'NONE', #107748, .T. ) ;
#66706 = FACE_OUTER_BOUND ( 'NONE', #24472, .T. ) ;
#66707 = LINE ( 'NONE', #97907, #122932 ) ;
#66708 = DIRECTION ( 'NONE',  ( 0.7071067811865487940, 0.7071067811865463515, 0.000000000000000000 ) ) ;
#66709 = EDGE_LOOP ( 'NONE', ( #58436, #98578, #32233, #20003 ) ) ;
#66710 = ORIENTED_EDGE ( 'NONE', *, *, #59442, .F. ) ;
#66711 = CARTESIAN_POINT ( 'NONE',  ( 100.8958333333333144, -2.130196079827427091, 7.949999999999999289 ) ) ;
#66712 = ORIENTED_EDGE ( 'NONE', *, *, #91486, .F. ) ;
#66713 = EDGE_LOOP ( 'NONE', ( #88545, #101789, #117560, #101197 ) ) ;
#66714 = ORIENTED_EDGE ( 'NONE', *, *, #7999, .T. ) ;
#66715 = LINE ( 'NONE', #123259, #103485 ) ;
#66716 = DIRECTION ( 'NONE',  ( -0.3543493200069163240, 0.000000000000000000, -0.9351131265310288487 ) ) ;
#66717 = EDGE_LOOP ( 'NONE', ( #109012, #125487, #58824, #44944 ) ) ;
#66718 = AXIS2_PLACEMENT_3D ( 'NONE', #79540, #36676, #46176 ) ;
#66719 = FACE_OUTER_BOUND ( 'NONE', #25067, .T. ) ;
#66720 = DIRECTION ( 'NONE',  ( 0.000000000000000000, -1.000000000000000000, 0.000000000000000000 ) ) ;
#66721 = AXIS2_PLACEMENT_3D ( 'NONE', #4659, #38784, #72167 ) ;
#66722 = DIRECTION ( 'NONE',  ( -0.2248289345038712861, 0.9743982503113672866, -2.004349902429943025E-16 ) ) ;
#66723 = FACE_OUTER_BOUND ( 'NONE', #21322, .T. ) ;
#66724 = EDGE_LOOP ( 'NONE', ( #46854, #136068, #62372, #9015, #10601 ) ) ;
#66725 = EDGE_CURVE ( 'NONE', #80548, #77764, #61424, .T. ) ;
#66726 = EDGE_CURVE ( 'NONE', #70409, #123460, #80998, .T. ) ;
#66727 = CARTESIAN_POINT ( 'NONE',  ( 20.21837311707492191, 21.74787736706807095, 4.999607392498048419 ) ) ;
#66728 = DIRECTION ( 'NONE',  ( -0.000000000000000000, 1.000000000000000000, -0.000000000000000000 ) ) ;
#66729 = DIRECTION ( 'NONE',  ( 0.7071067811865486830, -0.7071067811865464625, -0.000000000000000000 ) ) ;
#66731 = CARTESIAN_POINT ( 'NONE',  ( 26.99999999999999645, 4.648385311654464225, 5.846484084903029732 ) ) ;
#66730 = VECTOR ( 'NONE', #24887, 1000.000000000000000 ) ;
#66732 = CARTESIAN_POINT ( 'NONE',  ( -11.81601139373100651, 28.73617430169779041, 5.000000000000000000 ) ) ;
#66733 = CARTESIAN_POINT ( 'NONE',  ( 12.32816939922343913, -18.74070752338409562, 4.000000000000000000 ) ) ;
#66734 = VECTOR ( 'NONE', #31149, 1000.000000000000000 ) ;
#66735 = CARTESIAN_POINT ( 'NONE',  ( 86.99586038379622721, -3.974999999999998312, -6.884901960086286188 ) ) ;
#66736 = DIRECTION ( 'NONE',  ( 0.7071067811865486830, 0.7071067811865464625, 0.000000000000000000 ) ) ;
#66737 = EDGE_CURVE ( 'NONE', #120060, #134557, #25889, .T. ) ;
#66738 = EDGE_CURVE ( 'NONE', #57857, #122903, #27296, .T. ) ;
#66739 = VERTEX_POINT ( 'NONE', #136787 ) ;
#66740 = ORIENTED_EDGE ( 'NONE', *, *, #120773, .F. ) ;
#66741 = CARTESIAN_POINT ( 'NONE',  ( 119.2920968585647756, -5.291415217122921177, 3.054999999999999272 ) ) ;
#66742 = EDGE_CURVE ( 'NONE', #88957, #46507, #71550, .T. ) ;
#66743 = ORIENTED_EDGE ( 'NONE', *, *, #15385, .T. ) ;
#66744 = EDGE_CURVE ( 'NONE', #32976, #79589, #114087, .T. ) ;
#66745 = CARTESIAN_POINT ( 'NONE',  ( -54.18398860626899705, 28.73617430169825226, 5.000000000000000000 ) ) ;
#66746 = EDGE_CURVE ( 'NONE', #43903, #57318, #17835, .T. ) ;
#66747 = CARTESIAN_POINT ( 'NONE',  ( 26.99999999999980815, 16.55218569542899587, 5.000000000000000000 ) ) ;
#66748 = DIRECTION ( 'NONE',  ( 1.000000000000000000, 1.224606353822377258E-16, 0.000000000000000000 ) ) ;
#66749 = CARTESIAN_POINT ( 'NONE',  ( -9.989119713460445027, -22.02621442084248216, 4.990779571109223767 ) ) ;
#66750 = ADVANCED_FACE ( 'NONE', ( #50503 ), #93987, .F. ) ;
#66751 = CARTESIAN_POINT ( 'NONE',  ( 118.1829301918981372, -1.637169565754158951, -6.109999999999998543 ) ) ;
#66752 = ORIENTED_EDGE ( 'NONE', *, *, #102751, .F. ) ;
#66753 = ORIENTED_EDGE ( 'NONE', *, *, #52470, .F. ) ;
#66754 = DIRECTION ( 'NONE',  ( -0.000000000000000000, 0.3543493200069153248, 0.9351131265310292928 ) ) ;
#66755 = VECTOR ( 'NONE', #6376, 1000.000000000000000 ) ;
#66756 = PLANE ( 'NONE',  #1497 ) ;
#66757 = VECTOR ( 'NONE', #53281, 1000.000000000000000 ) ;
#66758 = EDGE_CURVE ( 'NONE', #133870, #4434, #138948, .T. ) ;
#66759 = ORIENTED_EDGE ( 'NONE', *, *, #839, .F. ) ;
#66760 = ORIENTED_EDGE ( 'NONE', *, *, #44490, .F. ) ;
#66761 = CARTESIAN_POINT ( 'NONE',  ( 35.72959685856475431, -6.110000000000000320, -1.637169565754161393 ) ) ;
#66762 = ORIENTED_EDGE ( 'NONE', *, *, #123761, .T. ) ;
#66763 = DIRECTION ( 'NONE',  ( -1.000000000000000000, 0.000000000000000000, 0.000000000000000000 ) ) ;
#66764 = CARTESIAN_POINT ( 'NONE',  ( -34.92500000000001137, -12.18334561358944335, 4.500000000000000888 ) ) ;
#66765 = DIRECTION ( 'NONE',  ( -0.7071067811865486830, -0.7071067811865464625, 0.000000000000000000 ) ) ;
#66766 = EDGE_CURVE ( 'NONE', #92427, #69962, #116469, .T. ) ;
#66767 = CARTESIAN_POINT ( 'NONE',  ( 27.32876352523144803, 0.000000000000000000, -6.109999999999998543 ) ) ;
#66768 = VERTEX_POINT ( 'NONE', #39652 ) ;
#66769 = CARTESIAN_POINT ( 'NONE',  ( 12.48921356237309155, -27.52281430457064104, 5.000000000000000000 ) ) ;
#66770 = VERTEX_POINT ( 'NONE', #83876 ) ;
#66771 = ORIENTED_EDGE ( 'NONE', *, *, #40962, .T. ) ;
#66772 = AXIS2_PLACEMENT_3D ( 'NONE', #97457, #140964, #38287 ) ;
#66773 = ORIENTED_EDGE ( 'NONE', *, *, #140904, .T. ) ;
#66774 =( GEOMETRIC_REPRESENTATION_CONTEXT ( 3 ) GLOBAL_UNCERTAINTY_ASSIGNED_CONTEXT ( ( #2842 ) ) GLOBAL_UNIT_ASSIGNED_CONTEXT ( ( #105526, #41005, #50464 ) ) REPRESENTATION_CONTEXT ( 'NONE', 'WORKASPACE' ) );
#66775 = DIRECTION ( 'NONE',  ( 0.6830127018922181881, 0.6830127018922202975, -0.2588190451025214056 ) ) ;
#66776 = FACE_OUTER_BOUND ( 'NONE', #9536, .T. ) ;
#66777 = VERTEX_POINT ( 'NONE', #128081 ) ;
#66778 = DIRECTION ( 'NONE',  ( 0.7071067811865487940, 0.7071067811865463515, 0.000000000000000000 ) ) ;
#66779 = EDGE_CURVE ( 'NONE', #81042, #96318, #73008, .T. ) ;
#66780 = FACE_OUTER_BOUND ( 'NONE', #74685, .T. ) ;
#66781 = CARTESIAN_POINT ( 'NONE',  ( -28.06996025486391133, -0.7407075233842701500, 13.87443053587617747 ) ) ;
#66782 = EDGE_CURVE ( 'NONE', #137008, #20082, #6940, .T. ) ;
#66783 = LINE ( 'NONE', #1481, #49045 ) ;
#66784 = FACE_BOUND ( 'NONE', #92743, .T. ) ;
#66785 = VERTEX_POINT ( 'NONE', #19990 ) ;
#66786 = CARTESIAN_POINT ( 'NONE',  ( -12.18398860626900060, 28.73617430169795739, 5.000000000000000000 ) ) ;
#66787 = DIRECTION ( 'NONE',  ( -0.000000000000000000, 0.000000000000000000, -1.000000000000000000 ) ) ;
#66788 = VERTEX_POINT ( 'NONE', #85249 ) ;
#66789 = DIRECTION ( 'NONE',  ( 0.000000000000000000, 0.000000000000000000, -1.000000000000000000 ) ) ;
#66790 = ORIENTED_EDGE ( 'NONE', *, *, #57757, .T. ) ;
#66791 = ORIENTED_EDGE ( 'NONE', *, *, #105935, .T. ) ;
#66792 = DIRECTION ( 'NONE',  ( 0.7071067811865487940, -0.7071067811865463515, 0.000000000000000000 ) ) ;
#66793 = EDGE_CURVE ( 'NONE', #77659, #130555, #97558, .T. ) ;
#66794 = EDGE_LOOP ( 'NONE', ( #100273, #66826, #93211, #34109 ) ) ;
#66795 = CARTESIAN_POINT ( 'NONE',  ( 48.47459685856478018, 1.637169565754164280, -6.109999999999996767 ) ) ;
#66796 = ORIENTED_EDGE ( 'NONE', *, *, #92697, .F. ) ;
#66797 = DIRECTION ( 'NONE',  ( -0.000000000000000000, -0.3543493200069152693, 0.9351131265310292928 ) ) ;
#66798 = CARTESIAN_POINT ( 'NONE',  ( -3.707106781186507938, -18.74070752338409207, 5.000000000000000000 ) ) ;
#66799 = EDGE_CURVE ( 'NONE', #75381, #3378, #95550, .T. ) ;
#66800 = DIRECTION ( 'NONE',  ( -0.7071067811865487940, 0.7071067811865463515, -0.000000000000000000 ) ) ;
#66801 = ORIENTED_EDGE ( 'NONE', *, *, #2875, .T. ) ;
#66802 = CARTESIAN_POINT ( 'NONE',  ( 12.69999999999999574, 0.000000000000000000, -39.50000000000000000 ) ) ;
#66803 = CARTESIAN_POINT ( 'NONE',  ( 71.53752705046289861, -9.735942053221456900E-16, 7.949999999999998401 ) ) ;
#66804 = CARTESIAN_POINT ( 'NONE',  ( 1.953608656376216022E-15, -6.270000000000002238, -37.00000000000000000 ) ) ;
#66805 = DIRECTION ( 'NONE',  ( 0.7071067811865487940, -0.7071067811865463515, 0.000000000000000000 ) ) ;
#66807 = EDGE_CURVE ( 'NONE', #139229, #96774, #62828, .T. ) ;
#66806 = PLANE ( 'NONE',  #1877 ) ;
#66808 = CARTESIAN_POINT ( 'NONE',  ( -34.92500000000001137, 22.22500000000000142, 4.500000000000000888 ) ) ;
#66809 = FACE_OUTER_BOUND ( 'NONE', #31739, .T. ) ;
#66810 = ORIENTED_EDGE ( 'NONE', *, *, #83919, .F. ) ;
#66811 = ORIENTED_EDGE ( 'NONE', *, *, #132864, .T. ) ;
#66812 = ORIENTED_EDGE ( 'NONE', *, *, #120840, .T. ) ;
#66813 = FACE_OUTER_BOUND ( 'NONE', #49635, .T. ) ;
#66814 = AXIS2_PLACEMENT_3D ( 'NONE', #51993, #9137, #96174 ) ;
#66816 = DIRECTION ( 'NONE',  ( -0.7071067811865486830, 0.7071067811865464625, 0.000000000000000000 ) ) ;
#66815 = VECTOR ( 'NONE', #52205, 1000.000000000000000 ) ;
#66817 = VERTEX_POINT ( 'NONE', #109155 ) ;
#66818 = AXIS2_PLACEMENT_3D ( 'NONE', #79115, #68248, #69658 ) ;
#66820 = VERTEX_POINT ( 'NONE', #40366 ) ;
#66819 = AXIS2_PLACEMENT_3D ( 'NONE', #121838, #34157, #134924 ) ;
#66821 = DIRECTION ( 'NONE',  ( 0.7071067811865486830, -0.7071067811865463515, 0.000000000000000000 ) ) ;
#66822 = EDGE_CURVE ( 'NONE', #123220, #23205, #42508, .T. ) ;
#66823 = VECTOR ( 'NONE', #112155, 1000.000000000000000 ) ;
#66824 = ADVANCED_FACE ( 'NONE', ( #142521 ), #96124, .T. ) ;
#66825 = LINE ( 'NONE', #123366, #106390 ) ;
#66826 = ORIENTED_EDGE ( 'NONE', *, *, #114687, .F. ) ;
#66827 = CARTESIAN_POINT ( 'NONE',  ( -0.1561230773924060511, -22.22499999999999787, 4.000000000000000000 ) ) ;
#66828 = VECTOR ( 'NONE', #25418, 1000.000000000000000 ) ;
#66829 = AXIS2_PLACEMENT_3D ( 'NONE', #36582, #91684, #92373 ) ;
#66830 = CARTESIAN_POINT ( 'NONE',  ( 14.70025512860841133, -27.71228299555195917, 4.000000000000000000 ) ) ;
#66831 = EDGE_CURVE ( 'NONE', #62699, #50020, #74411, .T. ) ;
#66832 = CARTESIAN_POINT ( 'NONE',  ( 23.83790314143521982, -6.871911579029513106, -3.967499999999993587 ) ) ;
#66833 = DIRECTION ( 'NONE',  ( -0.6830127018922181881, 0.6830127018922202975, -0.2588190451025214056 ) ) ;
#66834 = ORIENTED_EDGE ( 'NONE', *, *, #79496, .T. ) ;
#66835 = CARTESIAN_POINT ( 'NONE',  ( 111.7662635252314516, 4.472830434245839371, -4.472830434245839371 ) ) ;
#66836 = CARTESIAN_POINT ( 'NONE',  ( 20.70025512860841133, -27.71228299555191654, 4.000000000000000000 ) ) ;
#66837 = LINE ( 'NONE', #142956, #109774 ) ;
#66839 = ORIENTED_EDGE ( 'NONE', *, *, #48955, .F. ) ;
#66838 = CYLINDRICAL_SURFACE ( 'NONE', #10095, 0.5000000000000004441 ) ;
#66840 = COLOUR_RGB ( '', 0.08235294, 0.09019608, 0.10196078) ;
#66841 = FACE_OUTER_BOUND ( 'NONE', #44137, .T. ) ;
#66842 = EDGE_LOOP ( 'NONE', ( #102619, #118283, #61792, #53643, #107227 ) ) ;
#66843 = CARTESIAN_POINT ( 'NONE',  ( 20.99999999999986855, 17.96639925780208458, 5.000000000000000000 ) ) ;
#66844 = FACE_OUTER_BOUND ( 'NONE', #52713, .T. ) ;
#66845 = CARTESIAN_POINT ( 'NONE',  ( 33.18398860626899705, 28.73617430169810305, 5.000000000000000000 ) ) ;
#66847 = EDGE_CURVE ( 'NONE', #33404, #128631, #107007, .T. ) ;
#66846 = EDGE_LOOP ( 'NONE', ( #46745, #3411, #124492, #23049 ) ) ;
#66848 = CARTESIAN_POINT ( 'NONE',  ( -34.49999999999976552, -2.945670655169033481, 4.994342998332163219 ) ) ;
#66849 = ADVANCED_FACE ( 'NONE', ( #9081 ), #8376, .T. ) ;
#66850 = DIRECTION ( 'NONE',  ( 1.000000000000000000, 0.000000000000000000, 0.000000000000000000 ) ) ;
#66851 = DIRECTION ( 'NONE',  ( 0.7071067811865487940, -0.7071067811865463515, 0.000000000000000000 ) ) ;
#66852 = VERTEX_POINT ( 'NONE', #52624 ) ;
#66853 = VECTOR ( 'NONE', #33400, 1000.000000000000000 ) ;
#66854 = CARTESIAN_POINT ( 'NONE',  ( 10.49999999999993960, 16.08746187583908593, 4.000000000000000000 ) ) ;
#66855 = VECTOR ( 'NONE', #95788, 1000.000000000000000 ) ;
#66857 = AXIS2_PLACEMENT_3D ( 'NONE', #136039, #103390, #36724 ) ;
#66856 = PLANE ( 'NONE',  #116350 ) ;
#66858 = ORIENTED_EDGE ( 'NONE', *, *, #15031, .T. ) ;
#66859 = VECTOR ( 'NONE', #29696, 1000.000000000000000 ) ;
#66860 = PLANE ( 'NONE',  #55396 ) ;
#66862 = ORIENTED_EDGE ( 'NONE', *, *, #40914, .F. ) ;
#66861 = DIRECTION ( 'NONE',  ( -0.000000000000000000, -0.000000000000000000, 1.000000000000000000 ) ) ;
#66863 = EDGE_CURVE ( 'NONE', #65778, #85291, #75138, .T. ) ;
#66864 = EDGE_LOOP ( 'NONE', ( #111525, #67018, #87889, #27877, #115920, #59141 ) ) ;
#66865 = CARTESIAN_POINT ( 'NONE',  ( 0.000000000000000000, 0.000000000000000000, 7.950000000000000178 ) ) ;
#66866 = AXIS2_PLACEMENT_3D ( 'NONE', #86323, #110178, #142830 ) ;
#66867 = ORIENTED_EDGE ( 'NONE', *, *, #64449, .F. ) ;
#66868 = VECTOR ( 'NONE', #81652, 1000.000000000000000 ) ;
#66869 = CARTESIAN_POINT ( 'NONE',  ( 30.18398860626900060, 28.73617430169808173, 5.000000000000000000 ) ) ;
#66870 = CARTESIAN_POINT ( 'NONE',  ( -4.499999999999962697, 10.46639925780215563, 5.000000000000000000 ) ) ;
#66871 = ORIENTED_EDGE ( 'NONE', *, *, #107950, .F. ) ;
#66872 = CARTESIAN_POINT ( 'NONE',  ( 31.49999999999977973, 13.56627193232217188, -10.57019076586061423 ) ) ;
#66873 = DIRECTION ( 'NONE',  ( -0.000000000000000000, 0.3543493200069153248, 0.9351131265310292928 ) ) ;
#66874 = DIRECTION ( 'NONE',  ( -0.000000000000000000, 1.000000000000000000, -0.000000000000000000 ) ) ;
#66875 = VECTOR ( 'NONE', #132312, 1000.000000000000000 ) ;
#66876 = CARTESIAN_POINT ( 'NONE',  ( -20.99999999999984723, -21.84840872380826582, 2.849755605029559380 ) ) ;
#66877 = CARTESIAN_POINT ( 'NONE',  ( 127.9750270504628702, -5.819803920172572198, 5.819803920172572198 ) ) ;
#66878 = CARTESIAN_POINT ( 'NONE',  ( 14.42840764549667476, 9.139736423841732040E-16, 0.000000000000000000 ) ) ;
#66879 = ORIENTED_EDGE ( 'NONE', *, *, #121692, .F. ) ;
#66880 = VERTEX_POINT ( 'NONE', #141061 ) ;
#66881 = LINE ( 'NONE', #45861, #32723 ) ;
#66882 = ORIENTED_EDGE ( 'NONE', *, *, #39790, .T. ) ;
#66883 = EDGE_LOOP ( 'NONE', ( #101663, #83664, #67040, #105780 ) ) ;
#66884 = CARTESIAN_POINT ( 'NONE',  ( -72.48921356237309510, -27.52281430457106026, 5.000000000000000000 ) ) ;
#66885 = CARTESIAN_POINT ( 'NONE',  ( -8.588385094051634638, 22.22500000000000497, 4.777194822843819466 ) ) ;
#66886 = ORIENTED_EDGE ( 'NONE', *, *, #16096, .F. ) ;
#66887 = CARTESIAN_POINT ( 'NONE',  ( 0.2100385686636474791, 0.3999999999999995781, 2.083955130345453099 ) ) ;
#66888 = CARTESIAN_POINT ( 'NONE',  ( 34.92499999999998295, -11.33753812416086504, 4.000000000000000000 ) ) ;
#66889 = DIRECTION ( 'NONE',  ( -0.000000000000000000, 0.000000000000000000, 1.000000000000000000 ) ) ;
#66890 = FACE_OUTER_BOUND ( 'NONE', #36633, .T. ) ;
#66891 = CARTESIAN_POINT ( 'NONE',  ( 119.7295968585647614, -6.110000000000000320, -1.637169565754161393 ) ) ;
#66892 = ORIENTED_EDGE ( 'NONE', *, *, #82787, .T. ) ;
#66893 = DIRECTION ( 'NONE',  ( 0.3543493200069163795, -9.265275131829747941E-33, -0.9351131265310288487 ) ) ;
#66894 = CARTESIAN_POINT ( 'NONE',  ( -7.499999999999944045, -17.56887692260763245, 4.000000000000000000 ) ) ;
#66895 = DIRECTION ( 'NONE',  ( 1.000000000000000000, 0.000000000000000000, 0.000000000000000000 ) ) ;
#66896 = DIRECTION ( 'NONE',  ( 0.6830127018922180770, -0.6830127018922204085, -0.2588190451025213501 ) ) ;
#66897 = CARTESIAN_POINT ( 'NONE',  ( -15.48921356237309510, -27.52281430457066236, 5.000000000000000000 ) ) ;
#66898 = CARTESIAN_POINT ( 'NONE',  ( -18.48921356237309510, -27.52281430457068367, 5.000000000000000000 ) ) ;
#66899 = PLANE ( 'NONE',  #105893 ) ;
#66900 = CARTESIAN_POINT ( 'NONE',  ( 49.22502705046289151, 5.819803920172573086, -5.819803920172572198 ) ) ;
#66901 = CARTESIAN_POINT ( 'NONE',  ( 0.005480084712502889671, 28.92564299267938210, 4.000000000000000000 ) ) ;
#66902 = EDGE_CURVE ( 'NONE', #123251, #119070, #41766, .T. ) ;
#66903 = DIRECTION ( 'NONE',  ( -0.7071067811865487940, 0.7071067811865463515, 0.000000000000000000 ) ) ;
#66904 = EDGE_LOOP ( 'NONE', ( #87635, #125862, #111334, #56460 ) ) ;
#66905 = ORIENTED_EDGE ( 'NONE', *, *, #64644, .T. ) ;
#66906 = CARTESIAN_POINT ( 'NONE',  ( 46.79166666666666430, 3.975000000000003642, -6.884901960086285300 ) ) ;
#66907 = EDGE_CURVE ( 'NONE', #125640, #22650, #130215, .T. ) ;
#66908 = CARTESIAN_POINT ( 'NONE',  ( 0.000000000000000000, 0.000000000000000000, 5.000000000000000000 ) ) ;
#66909 = ADVANCED_FACE ( 'NONE', ( #53341 ), #29442, .F. ) ;
#66910 = DIRECTION ( 'NONE',  ( 0.7071067811865486830, -0.7071067811865464625, -0.000000000000000000 ) ) ;
#66911 = ORIENTED_EDGE ( 'NONE', *, *, #112576, .T. ) ;
#66912 = EDGE_CURVE ( 'NONE', #139562, #58036, #20709, .T. ) ;
#66913 = CARTESIAN_POINT ( 'NONE',  ( -1.320799999999936025, -0.1740827700035259273, 3.775643966265910034 ) ) ;
#66914 = FACE_OUTER_BOUND ( 'NONE', #50242, .T. ) ;
#66915 = CARTESIAN_POINT ( 'NONE',  ( 33.97959685856477563, 6.109999999999999432, 1.637169565754164280 ) ) ;
#66917 = EDGE_CURVE ( 'NONE', #36381, #117254, #5286, .T. ) ;
#66916 = VERTEX_POINT ( 'NONE', #51942 ) ;
#66918 = CARTESIAN_POINT ( 'NONE',  ( 32.48334561358932149, 22.22500000000000142, 4.500000000000000888 ) ) ;
#66919 = ORIENTED_EDGE ( 'NONE', *, *, #121442, .F. ) ;
#66920 = ORIENTED_EDGE ( 'NONE', *, *, #85066, .T. ) ;
#66921 = CARTESIAN_POINT ( 'NONE',  ( 9.299744871391588674, -27.71228299555212971, 4.000000000000000000 ) ) ;
#66922 = AXIS2_PLACEMENT_3D ( 'NONE', #19184, #30043, #7571 ) ;
#66923 = AXIS2_PLACEMENT_3D ( 'NONE', #27241, #61369, #27977 ) ;
#66924 = CARTESIAN_POINT ( 'NONE',  ( 81.16252705046289861, 7.949999999999998401, 1.460391307983218338E-15 ) ) ;
#66925 = PRESENTATION_LAYER_ASSIGNMENT (  '', '', ( #9009 ) ) ;
#66926 = EDGE_CURVE ( 'NONE', #136439, #4199, #5984, .T. ) ;
#66927 = CARTESIAN_POINT ( 'NONE',  ( -14.85700540165867345, 7.427722529079425762, 4.951096321256158284 ) ) ;
#66928 = ORIENTED_EDGE ( 'NONE', *, *, #86789, .F. ) ;
#66929 = EDGE_CURVE ( 'NONE', #11288, #49817, #71305, .T. ) ;
#66930 = LINE ( 'NONE', #35766, #125201 ) ;
#66931 = EDGE_LOOP ( 'NONE', ( #53705, #75899, #139573, #14353, #43360 ) ) ;
#66932 = CARTESIAN_POINT ( 'NONE',  ( 80.06293019189807580, 1.637169565754157174, 6.110000000000002984 ) ) ;
#66933 = DIRECTION ( 'NONE',  ( 1.000000000000000000, 0.000000000000000000, 0.000000000000000000 ) ) ;
#66934 = CARTESIAN_POINT ( 'NONE',  ( 0.000000000000000000, -4.870000000000014317, -40.00000000000000000 ) ) ;
#66935 = DIRECTION ( 'NONE',  ( 0.6830127018922180770, -0.6830127018922204085, -0.2588190451025213501 ) ) ;
#66936 = DIRECTION ( 'NONE',  ( 0.7071067811865487940, 0.7071067811865463515, -0.000000000000000000 ) ) ;
#66937 = EDGE_CURVE ( 'NONE', #2809, #874, #73441, .T. ) ;
#66938 = ORIENTED_EDGE ( 'NONE', *, *, #135385, .F. ) ;
#66939 = LINE ( 'NONE', #122735, #3630 ) ;
#66940 = CARTESIAN_POINT ( 'NONE',  ( 54.01626352523143737, -4.472830434245839371, 4.472830434245839371 ) ) ;
#66941 = DIRECTION ( 'NONE',  ( 0.6830127018922180770, -0.6830127018922204085, -0.2588190451025213501 ) ) ;
#66942 = CARTESIAN_POINT ( 'NONE',  ( 63.29974487139158867, -27.71228299555250274, 4.000000000000000000 ) ) ;
#66943 = DIRECTION ( 'NONE',  ( 1.000000000000000000, 0.000000000000000000, 0.000000000000000000 ) ) ;
#66944 = VERTEX_POINT ( 'NONE', #95165 ) ;
#66945 = VECTOR ( 'NONE', #32644, 1000.000000000000000 ) ;
#66946 = DIRECTION ( 'NONE',  ( -0.6830127018922180770, -0.6830127018922204085, -0.2588190451025213501 ) ) ;
#66947 = SURFACE_STYLE_USAGE ( .BOTH. , #77827 ) ;
#66948 = VERTEX_POINT ( 'NONE', #126369 ) ;
#66949 =( BOUNDED_CURVE ( )  B_SPLINE_CURVE ( 3, ( #130765, #31432, #75654, #21259 ),
 .UNSPECIFIED., .F., .F. ) 
 B_SPLINE_CURVE_WITH_KNOTS ( ( 4, 4 ),
 ( 4.130769849943813909, 4.183600770845220751 ),
 .UNSPECIFIED. ) 
 CURVE ( )  GEOMETRIC_REPRESENTATION_ITEM ( )  RATIONAL_B_SPLINE_CURVE ( ( 1.000000000000000000, 0.9997674213408587196, 0.9997674213408587196, 1.000000000000000000 ) ) 
 REPRESENTATION_ITEM ( '' )  );
#66950 = VECTOR ( 'NONE', #137163, 1000.000000000000000 ) ;
#66951 = CARTESIAN_POINT ( 'NONE',  ( 60.18398860626900415, 28.73617430169829490, 5.000000000000000000 ) ) ;
#66952 = ORIENTED_EDGE ( 'NONE', *, *, #18248, .T. ) ;
#66953 = CARTESIAN_POINT ( 'NONE',  ( 48.18398860626899705, 28.73617430169820608, 5.000000000000000000 ) ) ;
#66954 = FACE_OUTER_BOUND ( 'NONE', #64026, .T. ) ;
#66955 = ADVANCED_FACE ( 'NONE', ( #61862 ), #17594, .F. ) ;
#66956 = FACE_OUTER_BOUND ( 'NONE', #87772, .T. ) ;
#66957 = B_SPLINE_CURVE_WITH_KNOTS ( 'NONE', 3,
 ( #98773, #64741, #66887, #143011 ),
 .UNSPECIFIED., .F., .F.,
 ( 4, 4 ),
 ( 0.003913914403404827880, 0.004162342877716043374 ),
 .UNSPECIFIED. ) ;
#66958 = VECTOR ( 'NONE', #40211, 1000.000000000000000 ) ;
#66959 = VECTOR ( 'NONE', #138919, 1000.000000000000000 ) ;
#66961 = VECTOR ( 'NONE', #82389, 1000.000000000000227 ) ;
#66960 = CARTESIAN_POINT ( 'NONE',  ( -7.140000000000001457, -35.56014942880461405, -8.278119684037248405 ) ) ;
#66962 = FACE_BOUND ( 'NONE', #69486, .T. ) ;
#66963 = DIRECTION ( 'NONE',  ( -0.7071067811865486830, -0.7071067811865464625, 0.000000000000000000 ) ) ;
#66964 = CARTESIAN_POINT ( 'NONE',  ( -1.499999999999984013, -11.94781430457070215, 5.000000000000000000 ) ) ;
#66965 = CARTESIAN_POINT ( 'NONE',  ( -23.99999999999983302, -0.2811185226894510891, -5.995736974527457797 ) ) ;
#66967 = ORIENTED_EDGE ( 'NONE', *, *, #91179, .T. ) ;
#66966 = CARTESIAN_POINT ( 'NONE',  ( 18.63425672184678916, 4.584330080086930965E-16, 0.000000000000000000 ) ) ;
#66968 = VECTOR ( 'NONE', #76719, 1000.000000000000000 ) ;
#66969 = VECTOR ( 'NONE', #38132, 1000.000000000000000 ) ;
#66970 = CARTESIAN_POINT ( 'NONE',  ( 5.816011393731002066, 28.73617430169783304, 5.000000000000000000 ) ) ;
#66971 = ADVANCED_FACE ( 'NONE', ( #127829 ), #137983, .F. ) ;
#66972 = ORIENTED_EDGE ( 'NONE', *, *, #79801, .F. ) ;
#66973 = EDGE_LOOP ( 'NONE', ( #81415, #104461, #28754, #60082 ) ) ;
#66974 = CARTESIAN_POINT ( 'NONE',  ( 71.66209685856478018, -5.291415217122919401, 3.054999999999997939 ) ) ;
#66975 = ORIENTED_EDGE ( 'NONE', *, *, #129421, .T. ) ;
#66976 = CARTESIAN_POINT ( 'NONE',  ( -7.499999999999951150, 10.94296225409025958, -9.576120664313274133 ) ) ;
#66977 = B_SPLINE_CURVE_WITH_KNOTS ( 'NONE', 3,
 ( #32538, #65908, #56475, #55014, #99179, #23046, #44132, #78917, #59316, #79663, #123844, #125976 ),
 .UNSPECIFIED., .F., .F.,
 ( 4, 2, 2, 2, 2, 4 ),
 ( 4.336808689942017736E-19, 0.001108890051515398897, 0.001663335077273098020, 0.002217780103030797360, 0.003326670154546215123, 0.004435560206061632885 ),
 .UNSPECIFIED. ) ;
#66978 = EDGE_CURVE ( 'NONE', #118739, #112217, #50969, .T. ) ;
#66979 = ORIENTED_EDGE ( 'NONE', *, *, #121909, .F. ) ;
#66980 = CARTESIAN_POINT ( 'NONE',  ( 18.48921356237309510, -27.52281430457068367, 5.000000000000000000 ) ) ;
#66981 = AXIS2_PLACEMENT_3D ( 'NONE', #37251, #4548, #127096 ) ;
#66982 = PLANE ( 'NONE',  #26390 ) ;
#66983 = CARTESIAN_POINT ( 'NONE',  ( -60.18398860626900415, 28.73617430169829490, 5.000000000000000000 ) ) ;
#66984 = EDGE_CURVE ( 'NONE', #43368, #58880, #125832, .T. ) ;
#66985 = CARTESIAN_POINT ( 'NONE',  ( -14.20710678118643955, -11.24070752338416845, 5.000000000000000000 ) ) ;
#66987 = SURFACE_SIDE_STYLE ('',( #135806 ) ) ;
#66986 = CARTESIAN_POINT ( 'NONE',  ( 28.58990935480150952, 9.759292476615618384, 11.28811694763785489 ) ) ;
#66988 = CARTESIAN_POINT ( 'NONE',  ( -12.70000000000000284, -34.64999999999999147, 17.49210858042622263 ) ) ;
#66989 = DIRECTION ( 'NONE',  ( -0.7071067811865486830, -0.7071067811865464625, 0.000000000000000000 ) ) ;
#66990 = ORIENTED_EDGE ( 'NONE', *, *, #112961, .T. ) ;
#66991 = ORIENTED_EDGE ( 'NONE', *, *, #130833, .F. ) ;
#66992 = CARTESIAN_POINT ( 'NONE',  ( 33.18398860626899705, 28.73617430169810305, 5.000000000000000000 ) ) ;
#66993 = DIRECTION ( 'NONE',  ( 0.7071067811865487940, 0.7071067811865463515, -0.000000000000000000 ) ) ;
#66994 = ORIENTED_EDGE ( 'NONE', *, *, #117887, .T. ) ;
#66995 = ORIENTED_EDGE ( 'NONE', *, *, #75484, .T. ) ;
#66996 = EDGE_LOOP ( 'NONE', ( #62659, #32642, #47356, #133998 ) ) ;
#66997 = ADVANCED_FACE ( 'NONE', ( #7429 ), #15433, .T. ) ;
#66998 = CARTESIAN_POINT ( 'NONE',  ( 27.70876352523143993, -7.482591942790329030E-16, 6.110000000000001208 ) ) ;
#66999 = ORIENTED_EDGE ( 'NONE', *, *, #126855, .F. ) ;
#67000 = CARTESIAN_POINT ( 'NONE',  ( 11.51078643762690490, -27.52281430457047406, 5.000000000000000000 ) ) ;
#67001 = DIRECTION ( 'NONE',  ( 0.7071067811865487940, 0.7071067811865463515, 0.000000000000000000 ) ) ;
#67002 = CARTESIAN_POINT ( 'NONE',  ( 3.129569808101886341, -3.967499999999998028, -6.871911579029511330 ) ) ;
#67003 = CARTESIAN_POINT ( 'NONE',  ( -4.499999999999968914, 5.696342897626497148, -7.587980461218407413 ) ) ;
#67004 = VERTEX_POINT ( 'NONE', #59721 ) ;
#67005 = DIRECTION ( 'NONE',  ( -0.7071067811865486830, -0.7071067811865464625, -0.000000000000000000 ) ) ;
#67006 = LINE ( 'NONE', #44578, #67342 ) ;
#67007 = FACE_OUTER_BOUND ( 'NONE', #112515, .T. ) ;
#67009 = EDGE_LOOP ( 'NONE', ( #81254, #136289, #109295, #54203 ) ) ;
#67008 = CARTESIAN_POINT ( 'NONE',  ( 15.32816939922342847, -6.740707523384209310, 4.000000000000000000 ) ) ;
#67010 = ORIENTED_EDGE ( 'NONE', *, *, #115746, .T. ) ;
#67011 = CARTESIAN_POINT ( 'NONE',  ( 15.00548008471250228, 28.92564299267927552, 4.000000000000000000 ) ) ;
#67012 = CARTESIAN_POINT ( 'NONE',  ( 34.92499999999998295, 21.72500000000000142, 0.4999999999999995559 ) ) ;
#67013 = DIRECTION ( 'NONE',  ( 0.3543493200069163240, -0.000000000000000000, 0.9351131265310288487 ) ) ;
#67014 = ORIENTED_EDGE ( 'NONE', *, *, #10589, .T. ) ;
#67015 = CARTESIAN_POINT ( 'NONE',  ( 16.49999999999988631, 22.01701374228156993, 2.453858888625593426 ) ) ;
#67016 = CARTESIAN_POINT ( 'NONE',  ( -8.816011393731004731, 28.73617430169781173, 5.000000000000000000 ) ) ;
#67018 = ORIENTED_EDGE ( 'NONE', *, *, #88367, .T. ) ;
#67017 = EDGE_CURVE ( 'NONE', #2775, #19628, #27774, .T. ) ;
#67019 = CARTESIAN_POINT ( 'NONE',  ( 1.042387978378689573, -0.4000000000000003553, 2.015694669338588429 ) ) ;
#67020 = DIRECTION ( 'NONE',  ( -0.7071067811865487940, 0.7071067811865463515, 0.000000000000000000 ) ) ;
#67021 = VECTOR ( 'NONE', #82182, 1000.000000000000227 ) ;
#67022 = STYLED_ITEM ( 'NONE', ( #43312 ), #127113 ) ;
#67023 = AXIS2_PLACEMENT_3D ( 'NONE', #84081, #50708, #85448 ) ;
#67024 = CARTESIAN_POINT ( 'NONE',  ( 1.179999999999998828, 9.043340090917734386, 10.00000000000000000 ) ) ;
#67025 = DIRECTION ( 'NONE',  ( -0.7071067811865486830, -0.7071067811865464625, -0.000000000000000000 ) ) ;
#67026 = CARTESIAN_POINT ( 'NONE',  ( 0.000000000000000000, 0.000000000000000000, 0.000000000000000000 ) ) ;
#67027 = VECTOR ( 'NONE', #94750, 1000.000000000000000 ) ;
#67029 = ADVANCED_FACE ( 'NONE', ( #137267 ), #37844, .T. ) ;
#67028 = DIRECTION ( 'NONE',  ( -0.7071067811865487940, 0.7071067811865463515, 0.000000000000000000 ) ) ;
#67030 = LINE ( 'NONE', #58345, #22853 ) ;
#67031 = ORIENTED_EDGE ( 'NONE', *, *, #42439, .F. ) ;
#67032 = EDGE_CURVE ( 'NONE', #86149, #90697, #127082, .T. ) ;
#67033 = LINE ( 'NONE', #86655, #42050 ) ;
#67034 = VERTEX_POINT ( 'NONE', #16908 ) ;
#67035 = CARTESIAN_POINT ( 'NONE',  ( 153.4000000000000057, -1.600000000000086020, -34.92499999999998295 ) ) ;
#67036 = VECTOR ( 'NONE', #118746, 1000.000000000000000 ) ;
#67037 = LINE ( 'NONE', #111220, #109575 ) ;
#67038 = FACE_OUTER_BOUND ( 'NONE', #36973, .T. ) ;
#67039 = CARTESIAN_POINT ( 'NONE',  ( -3.316579611327873600, -6.740707523384216415, 11.88629033278125036 ) ) ;
#67040 = ORIENTED_EDGE ( 'NONE', *, *, #115004, .T. ) ;
#67041 = VECTOR ( 'NONE', #48132, 1000.000000000000000 ) ;
#67042 = LINE ( 'NONE', #35145, #140985 ) ;
#67043 = CARTESIAN_POINT ( 'NONE',  ( -34.49999999999976552, -14.56887692260766443, 4.000000000000000000 ) ) ;
#67044 = PLANE ( 'NONE',  #65371 ) ;
#67045 = EDGE_LOOP ( 'NONE', ( #52167, #56722, #28402, #73188, #116984 ) ) ;
#67046 = CARTESIAN_POINT ( 'NONE',  ( 112.5624999999999858, -5.819803920172573086, -5.819803920172573974 ) ) ;
#67047 = DIRECTION ( 'NONE',  ( 0.7071067811865487940, 0.7071067811865463515, 0.000000000000000000 ) ) ;
#67048 =( GEOMETRIC_REPRESENTATION_CONTEXT ( 3 ) GLOBAL_UNCERTAINTY_ASSIGNED_CONTEXT ( ( #128902 ) ) GLOBAL_UNIT_ASSIGNED_CONTEXT ( ( #122294, #65846, #78836 ) ) REPRESENTATION_CONTEXT ( 'NONE', 'WORKASPACE' ) );
#67049 = VECTOR ( 'NONE', #81385, 999.9999999999998863 ) ;
#67050 = DIRECTION ( 'NONE',  ( -0.7071067811865486830, 0.7071067811865464625, 0.000000000000000000 ) ) ;
#67051 = CARTESIAN_POINT ( 'NONE',  ( 58.53709685856478728, -3.054999999999999272, -5.291415217122919401 ) ) ;
#67052 = ADVANCED_FACE ( 'NONE', ( #61180 ), #105331, .F. ) ;
#67053 = PLANE ( 'NONE',  #118129 ) ;
#67055 = CARTESIAN_POINT ( 'NONE',  ( 14.29289321881336150, 8.259292476615639700, 5.000000000000000000 ) ) ;
#67054 = VECTOR ( 'NONE', #54280, 1000.000000000000000 ) ;
#67056 = CARTESIAN_POINT ( 'NONE',  ( 31.72502705046288796, 5.819803920172573974, -5.819803920172573086 ) ) ;
#67057 = VERTEX_POINT ( 'NONE', #83619 ) ;
#67058 =( NAMED_UNIT ( * ) SI_UNIT ( $, .STERADIAN. ) SOLID_ANGLE_UNIT ( ) );
#67059 = ORIENTED_EDGE ( 'NONE', *, *, #55629, .T. ) ;
#67060 = FACE_OUTER_BOUND ( 'NONE', #75656, .T. ) ;
#67061 = VECTOR ( 'NONE', #8909, 1000.000000000000000 ) ;
#67062 = VECTOR ( 'NONE', #100928, 1000.000000000000000 ) ;
#67063 = AXIS2_PLACEMENT_3D ( 'NONE', #107331, #61720, #138549 ) ;
#67064 = DIRECTION ( 'NONE',  ( -0.7071067811865486830, -0.7071067811865464625, 0.000000000000000000 ) ) ;
#67065 = CARTESIAN_POINT ( 'NONE',  ( -60.18398860626900415, 28.73617430169829490, 5.000000000000000000 ) ) ;
#67066 = CARTESIAN_POINT ( 'NONE',  ( 149.2199999999997999, -3.180000000000061444, -31.92499999999998295 ) ) ;
#67067 = FACE_OUTER_BOUND ( 'NONE', #9457, .T. ) ;
#67068 = LINE ( 'NONE', #11945, #135747 ) ;
#67069 = ORIENTED_EDGE ( 'NONE', *, *, #76467, .F. ) ;
#67070 = AXIS2_PLACEMENT_3D ( 'NONE', #130601, #22489, #110928 ) ;
#67071 = ORIENTED_EDGE ( 'NONE', *, *, #111850, .T. ) ;
#67072 = CARTESIAN_POINT ( 'NONE',  ( -8.999999999999932498, 5.587461875839184522, 4.000000000000000000 ) ) ;
#67073 = CARTESIAN_POINT ( 'NONE',  ( -12.48921356237309155, -27.52281430457064104, 5.000000000000000000 ) ) ;
#67074 = VECTOR ( 'NONE', #8201, 1000.000000000000227 ) ;
#67075 = CARTESIAN_POINT ( 'NONE',  ( 52.60764783923757193, -49.05583548141699879, 39.86617647058822200 ) ) ;
#67076 = DIRECTION ( 'NONE',  ( -0.7071067811865487940, 0.7071067811865463515, -0.000000000000000000 ) ) ;
#67077 = CARTESIAN_POINT ( 'NONE',  ( 72.99586038379622721, -3.974999999999998312, -6.884901960086286188 ) ) ;
#67078 = PLANE ( 'NONE',  #11514 ) ;
#67079 = EDGE_CURVE ( 'NONE', #22343, #90151, #12530, .T. ) ;
#67080 = CARTESIAN_POINT ( 'NONE',  ( -32.67183060077623935, -6.740707523384205757, 4.000000000000000000 ) ) ;
#67081 = ORIENTED_EDGE ( 'NONE', *, *, #96960, .T. ) ;
#67082 = CARTESIAN_POINT ( 'NONE',  ( 73.77083333333331439, -7.949999999999999289, -2.130196079827426203 ) ) ;
#67083 = LINE ( 'NONE', #361, #7539 ) ;
#67084 = ADVANCED_FACE ( 'NONE', ( #67680 ), #112570, .F. ) ;
#67085 = CARTESIAN_POINT ( 'NONE',  ( -34.49999999999976552, -1.535744391599501490, 4.994342998332164996 ) ) ;
#67086 = CARTESIAN_POINT ( 'NONE',  ( -33.48921356237309510, -27.52281430457078670, 5.000000000000000000 ) ) ;
#67087 = CIRCLE ( 'NONE', #134241, 2.500000000000000888 ) ;
#67088 = ORIENTED_EDGE ( 'NONE', *, *, #89947, .F. ) ;
#67089 = EDGE_CURVE ( 'NONE', #71281, #94899, #7686, .T. ) ;
#67090 = ADVANCED_FACE ( 'NONE', ( #125611 ), #26286, .F. ) ;
#67091 = CARTESIAN_POINT ( 'NONE',  ( 20.51078643762690490, -27.52281430457041012, 5.000000000000000000 ) ) ;
#67092 = ORIENTED_EDGE ( 'NONE', *, *, #43191, .T. ) ;
#67093 = FACE_OUTER_BOUND ( 'NONE', #102411, .T. ) ;
#67094 = CARTESIAN_POINT ( 'NONE',  ( 64.02126352523144703, -4.472830434245839371, -4.472830434245840259 ) ) ;
#67095 = ORIENTED_EDGE ( 'NONE', *, *, #122040, .T. ) ;
#67096 = LINE ( 'NONE', #105246, #116106 ) ;
#67097 = DIRECTION ( 'NONE',  ( -0.7071067811865486830, -0.7071067811865464625, 0.000000000000000000 ) ) ;
#67098 = EDGE_CURVE ( 'NONE', #125881, #80563, #81405, .T. ) ;
#67099 = CARTESIAN_POINT ( 'NONE',  ( 10.49999999999992539, -12.66682484999665448, -0.6294897503863688959 ) ) ;
#67100 = EDGE_CURVE ( 'NONE', #71830, #12348, #23403, .T. ) ;
#67101 = DIRECTION ( 'NONE',  ( -0.3543493200069163240, -0.000000000000000000, -0.9351131265310288487 ) ) ;
#67103 = EDGE_LOOP ( 'NONE', ( #81386, #100946, #26116, #49703 ) ) ;
#67102 = DIRECTION ( 'NONE',  ( -0.7071067811865487940, 0.7071067811865463515, 0.000000000000000000 ) ) ;
#67104 = LINE ( 'NONE', #111292, #143310 ) ;
#67105 = LINE ( 'NONE', #111293, #70788 ) ;
#67106 = CARTESIAN_POINT ( 'NONE',  ( -24.14562793195488766, 0.06350461447050873010, 4.871950940718891232 ) ) ;
#67107 = DIRECTION ( 'NONE',  ( -0.000000000000000000, -0.000000000000000000, 1.000000000000000000 ) ) ;
#67108 = ORIENTED_EDGE ( 'NONE', *, *, #123740, .F. ) ;
#67109 = EDGE_CURVE ( 'NONE', #104640, #114790, #56808, .T. ) ;
#67110 = ORIENTED_EDGE ( 'NONE', *, *, #100842, .T. ) ;
#67111 = CARTESIAN_POINT ( 'NONE',  ( 64.31293019189810423, -1.637169565754159617, -6.110000000000001208 ) ) ;
#67112 = VERTEX_POINT ( 'NONE', #56088 ) ;
#67113 = LINE ( 'NONE', #133794, #15139 ) ;
#67114 = DIRECTION ( 'NONE',  ( -0.6830127018922181881, 0.6830127018922202975, -0.2588190451025214056 ) ) ;
#67115 = CARTESIAN_POINT ( 'NONE',  ( -19.05000000000000071, 3.174999999999997158, 4.000000000000000000 ) ) ;
#67116 = CARTESIAN_POINT ( 'NONE',  ( 30.79289321881324071, 18.75929247661552779, 5.000000000000000000 ) ) ;
#67117 = ORIENTED_EDGE ( 'NONE', *, *, #141225, .T. ) ;
#67119 = EDGE_CURVE ( 'NONE', #114036, #72734, #58245, .T. ) ;
#67118 = ORIENTED_EDGE ( 'NONE', *, *, #69656, .T. ) ;
#67120 = LINE ( 'NONE', #75857, #86216 ) ;
#67121 = CARTESIAN_POINT ( 'NONE',  ( -19.75037474193593567, -1.784389841569742785, -32.42466272773691571 ) ) ;
#67122 = ORIENTED_EDGE ( 'NONE', *, *, #102791, .F. ) ;
#67123 = LINE ( 'NONE', #33106, #9574 ) ;
#67124 = LINE ( 'NONE', #124353, #80405 ) ;
#67125 = ADVANCED_FACE ( 'NONE', ( #24139 ), #57499, .T. ) ;
#67126 = CARTESIAN_POINT ( 'NONE',  ( 6.489213562373093325, -27.52281430457059841, 5.000000000000000000 ) ) ;
#67127 = VECTOR ( 'NONE', #11683, 999.9999999999998863 ) ;
#67128 = AXIS2_PLACEMENT_3D ( 'NONE', #138897, #50452, #138171 ) ;
#67129 = ORIENTED_EDGE ( 'NONE', *, *, #129355, .F. ) ;
#67130 = AXIS2_PLACEMENT_3D ( 'NONE', #54691, #44556, #11857 ) ;
#67131 = FACE_BOUND ( 'NONE', #117795, .T. ) ;
#67132 = CARTESIAN_POINT ( 'NONE',  ( 11.99999999999992006, 15.45873954670186556, -0.03131636524296779744 ) ) ;
#67133 = EDGE_CURVE ( 'NONE', #142250, #98924, #100274, .T. ) ;
#67134 = FACE_OUTER_BOUND ( 'NONE', #13833, .T. ) ;
#67135 = FACE_OUTER_BOUND ( 'NONE', #86547, .T. ) ;
#67136 = LINE ( 'NONE', #120035, #131400 ) ;
#67137 = CARTESIAN_POINT ( 'NONE',  ( -33.48921356237309510, -27.52281430457078670, 5.000000000000000000 ) ) ;
#67139 = EDGE_CURVE ( 'NONE', #41149, #31359, #2344, .T. ) ;
#67138 = CARTESIAN_POINT ( 'NONE',  ( 94.86850992298123231, -53.48000000000006082, -7.940000000001945502 ) ) ;
#67140 = VERTEX_POINT ( 'NONE', #69822 ) ;
#67141 = EDGE_LOOP ( 'NONE', ( #140089, #51105, #37873, #80378 ) ) ;
#67142 = CARTESIAN_POINT ( 'NONE',  ( 103.1620968585647802, -5.291415217122919401, 3.054999999999997939 ) ) ;
#67143 = VERTEX_POINT ( 'NONE', #24842 ) ;
#67144 = CARTESIAN_POINT ( 'NONE',  ( 15.18398860626900237, 28.73617430169797871, 5.000000000000000000 ) ) ;
#67145 = EDGE_LOOP ( 'NONE', ( #24985, #108663, #40466, #112894, #58280 ) ) ;
#67146 = VECTOR ( 'NONE', #62447, 1000.000000000000000 ) ;
#67147 = LINE ( 'NONE', #111338, #58638 ) ;
#67148 = CARTESIAN_POINT ( 'NONE',  ( 3.983306282870438864, 6.094999999999991758, 1.633150327867686880 ) ) ;
#67149 = VECTOR ( 'NONE', #121988, 1000.000000000000000 ) ;
#67150 = DIRECTION ( 'NONE',  ( 0.7071067811865487940, -0.7071067811865463515, 0.000000000000000000 ) ) ;
#67151 = ORIENTED_EDGE ( 'NONE', *, *, #51055, .F. ) ;
#67152 = CARTESIAN_POINT ( 'NONE',  ( 10.77958563595370833, 4.584330080086930965E-16, 0.000000000000000000 ) ) ;
#67153 = LINE ( 'NONE', #1145, #40324 ) ;
#67154 = LINE ( 'NONE', #36644, #24666 ) ;
#67155 = CARTESIAN_POINT ( 'NONE',  ( -15.52400138585438505, 22.03583458319438648, 4.979811245910084061 ) ) ;
#67156 = CARTESIAN_POINT ( 'NONE',  ( 2.816639616203773677, -1.633150327867687102, -6.094999999999992646 ) ) ;
#67157 = DIRECTION ( 'NONE',  ( -0.000000000000000000, 0.3543493200069152138, -0.9351131265310292928 ) ) ;
#67158 = ORIENTED_EDGE ( 'NONE', *, *, #74815, .F. ) ;
#67159 = AXIS2_PLACEMENT_3D ( 'NONE', #110196, #32678, #10867 ) ;
#67160 = DIRECTION ( 'NONE',  ( -0.7071067811865487940, 0.7071067811865463515, -0.000000000000000000 ) ) ;
#67161 = LINE ( 'NONE', #133842, #4850 ) ;
#67162 = EDGE_LOOP ( 'NONE', ( #76479, #87354, #109707, #72753 ) ) ;
#67163 = ORIENTED_EDGE ( 'NONE', *, *, #28641, .T. ) ;
#67164 = AXIS2_PLACEMENT_3D ( 'NONE', #27420, #127465, #51353 ) ;
#67165 = ORIENTED_EDGE ( 'NONE', *, *, #29910, .F. ) ;
#67167 = VECTOR ( 'NONE', #56062, 1000.000000000000000 ) ;
#67166 = CARTESIAN_POINT ( 'NONE',  ( 51.47959685856477563, 6.109999999999999432, 1.637169565754164280 ) ) ;
#67168 = EDGE_LOOP ( 'NONE', ( #94935, #85996, #97299, #102485 ) ) ;
#67169 = CARTESIAN_POINT ( 'NONE',  ( -4.828169399223490643, 12.75929247661559351, 4.000000000000000000 ) ) ;
#67170 = AXIS2_PLACEMENT_3D ( 'NONE', #71988, #114027, #69121 ) ;
#67171 = CARTESIAN_POINT ( 'NONE',  ( 10.54580628287044064, 5.278424836066143655, -3.047499999999997655 ) ) ;
#67172 = CARTESIAN_POINT ( 'NONE',  ( 90.27126352523143282, 4.472830434245838482, 4.472830434245842035 ) ) ;
#67173 = CARTESIAN_POINT ( 'NONE',  ( 54.29974487139159578, -27.71228299555243879, 4.000000000000000000 ) ) ;
#67174 = EDGE_CURVE ( 'NONE', #13015, #121255, #120011, .T. ) ;
#67175 = CARTESIAN_POINT ( 'NONE',  ( 0.1161069444170879233, 0.4000000000000001332, -2.220360628129161462 ) ) ;
#67176 = ORIENTED_EDGE ( 'NONE', *, *, #130768, .F. ) ;
#67177 = CARTESIAN_POINT ( 'NONE',  ( -29.99999999999978328, -0.03360074219773898085, 5.000000000000000000 ) ) ;
#67178 = ADVANCED_FACE ( 'NONE', ( #36443 ), #14688, .F. ) ;
#67179 = VECTOR ( 'NONE', #7485, 1000.000000000000227 ) ;
#67180 = PLANE ( 'NONE',  #70190 ) ;
#67181 = ORIENTED_EDGE ( 'NONE', *, *, #128472, .T. ) ;
#67182 = CARTESIAN_POINT ( 'NONE',  ( -38.99451991528749062, 28.92564299267965211, 4.000000000000000000 ) ) ;
#67183 = FACE_OUTER_BOUND ( 'NONE', #46793, .T. ) ;
#67184 = EDGE_LOOP ( 'NONE', ( #29686, #125107, #80438, #88559 ) ) ;
#67185 = DIRECTION ( 'NONE',  ( -0.000000000000000000, 0.3543493200069153248, 0.9351131265310292928 ) ) ;
#67186 = ORIENTED_EDGE ( 'NONE', *, *, #84744, .F. ) ;
#67187 = ORIENTED_EDGE ( 'NONE', *, *, #3583, .F. ) ;
#67188 = ORIENTED_EDGE ( 'NONE', *, *, #32522, .F. ) ;
#67189 = CARTESIAN_POINT ( 'NONE',  ( 118.9120968585647802, 5.291415217122921177, -3.054999999999994831 ) ) ;
#67190 = VECTOR ( 'NONE', #112466, 1000.000000000000114 ) ;
#67191 = CARTESIAN_POINT ( 'NONE',  ( 39.48921356237310221, -27.52281430457082934, 5.000000000000000000 ) ) ;
#67192 = ADVANCED_FACE ( 'NONE', ( #35038 ), #136453, .F. ) ;
#67193 = CARTESIAN_POINT ( 'NONE',  ( 65.99451991528749772, 28.92564299267984396, 4.000000000000000000 ) ) ;
#67194 = EDGE_CURVE ( 'NONE', #124937, #18835, #48755, .T. ) ;
#67195 = CARTESIAN_POINT ( 'NONE',  ( 51.48921356237309510, -27.52281430457091460, 5.000000000000000000 ) ) ;
#67196 = ORIENTED_EDGE ( 'NONE', *, *, #53543, .F. ) ;
#67197 = AXIS2_PLACEMENT_3D ( 'NONE', #134646, #99850, #3364 ) ;
#67198 = CARTESIAN_POINT ( 'NONE',  ( -6.938893903907228378E-15, -5.527737879153195699, -7.983877177622371590 ) ) ;
#67199 = CARTESIAN_POINT ( 'NONE',  ( 14.99956980810188689, -3.967499999999998028, -6.871911579029511330 ) ) ;
#67200 = DIRECTION ( 'NONE',  ( -0.7071067811865487940, 0.000000000000000000, 0.7071067811865463515 ) ) ;
#67201 = FACE_OUTER_BOUND ( 'NONE', #9742, .T. ) ;
#67202 = ADVANCED_FACE ( 'NONE', ( #74068 ), #104542, .T. ) ;
#67203 = CARTESIAN_POINT ( 'NONE',  ( -13.17183060077638324, -11.24070752338417556, 4.000000000000000000 ) ) ;
#67204 = ORIENTED_EDGE ( 'NONE', *, *, #4612, .T. ) ;
#67205 = ORIENTED_EDGE ( 'NONE', *, *, #49610, .T. ) ;
#67206 = ORIENTED_EDGE ( 'NONE', *, *, #28856, .F. ) ;
#67207 = DIRECTION ( 'NONE',  ( 1.000000000000000000, 0.000000000000000000, 0.000000000000000000 ) ) ;
#67208 = PLANE ( 'NONE',  #130698 ) ;
#67209 = VECTOR ( 'NONE', #77411, 1000.000000000000227 ) ;
#67210 = DIRECTION ( 'NONE',  ( 0.7071067811865487940, 0.7071067811865463515, 0.000000000000000000 ) ) ;
#67211 = CARTESIAN_POINT ( 'NONE',  ( 6.093288859525676671, 9.434732237030869939, -1.147367193843239930 ) ) ;
#67212 = ADVANCED_FACE ( 'NONE', ( #95087 ), #106665, .F. ) ;
#67213 = VECTOR ( 'NONE', #60952, 999.9999999999998863 ) ;
#67214 = AXIS2_PLACEMENT_3D ( 'NONE', #75927, #9939, #65807 ) ;
#67215 = DIRECTION ( 'NONE',  ( -0.6830127018922180770, -0.6830127018922204085, -0.2588190451025213501 ) ) ;
#67216 = DIRECTION ( 'NONE',  ( 0.000000000000000000, -1.000000000000000000, 0.000000000000000000 ) ) ;
#67217 = CARTESIAN_POINT ( 'NONE',  ( 48.29974487139158867, -27.71228299555239971, 4.000000000000000000 ) ) ;
#67218 = DIRECTION ( 'NONE',  ( 0.6830127018922181881, 0.6830127018922202975, -0.2588190451025214056 ) ) ;
#67219 = VERTEX_POINT ( 'NONE', #126999 ) ;
#67220 = DIRECTION ( 'NONE',  ( -0.000000000000000000, -0.3543493200069152693, 0.9351131265310292928 ) ) ;
#67221 = EDGE_LOOP ( 'NONE', ( #43893, #112269, #62212, #90406 ) ) ;
#67223 = ADVANCED_FACE ( 'NONE', ( #26984 ), #71958, .F. ) ;
#67222 = VECTOR ( 'NONE', #42776, 1000.000000000000000 ) ;
#67224 = VECTOR ( 'NONE', #55827, 1000.000000000000227 ) ;
#67225 =( GEOMETRIC_REPRESENTATION_CONTEXT ( 3 ) GLOBAL_UNCERTAINTY_ASSIGNED_CONTEXT ( ( #117296 ) ) GLOBAL_UNIT_ASSIGNED_CONTEXT ( ( #65087, #28874, #106379 ) ) REPRESENTATION_CONTEXT ( 'NONE', 'WORKASPACE' ) );
#67226 = CARTESIAN_POINT ( 'NONE',  ( 17.47198025047039494, -2.800541402284825843, -34.03206192796267970 ) ) ;
#67227 = EDGE_LOOP ( 'NONE', ( #81501, #136451, #23279, #77356 ) ) ;
#67228 = VECTOR ( 'NONE', #142249, 1000.000000000000227 ) ;
#67229 = CARTESIAN_POINT ( 'NONE',  ( 17.10830628287044419, 1.633150327867706864, -6.094999999999981100 ) ) ;
#67231 = ORIENTED_EDGE ( 'NONE', *, *, #72353, .T. ) ;
#67230 = CARTESIAN_POINT ( 'NONE',  ( 45.18398860626900415, 28.73617430169818832, 5.000000000000000000 ) ) ;
#67232 = FACE_OUTER_BOUND ( 'NONE', #89224, .T. ) ;
#67233 = ORIENTED_EDGE ( 'NONE', *, *, #93584, .T. ) ;
#67234 = DIRECTION ( 'NONE',  ( 0.000000000000000000, -1.000000000000000000, 0.000000000000000000 ) ) ;
#67235 = ORIENTED_EDGE ( 'NONE', *, *, #128326, .F. ) ;
#67236 = CARTESIAN_POINT ( 'NONE',  ( -20.99451991528748707, 28.92564299267952777, 4.000000000000000000 ) ) ;
#67237 = CIRCLE ( 'NONE', #48718, 3.000000000000000000 ) ;
#67238 = ORIENTED_EDGE ( 'NONE', *, *, #40147, .T. ) ;
#67239 = CARTESIAN_POINT ( 'NONE',  ( -36.48921356237310221, -27.52281430457080802, 5.000000000000000000 ) ) ;
#67240 = CARTESIAN_POINT ( 'NONE',  ( 112.0791937171295558, 3.975000000000002753, -6.884901960086283523 ) ) ;
#67241 = DIRECTION ( 'NONE',  ( 0.000000000000000000, 0.000000000000000000, 1.000000000000000000 ) ) ;
#67242 = DIRECTION ( 'NONE',  ( 0.7071067811865487940, -0.7071067811865463515, 0.000000000000000000 ) ) ;
#67243 = CARTESIAN_POINT ( 'NONE',  ( -7.499999999999947597, 22.01701374228154506, 2.453858888625646273 ) ) ;
#67245 = EDGE_CURVE ( 'NONE', #50205, #49451, #51616, .T. ) ;
#67244 = LINE ( 'NONE', #98438, #58798 ) ;
#67246 = CARTESIAN_POINT ( 'NONE',  ( 42.18398860626899705, 28.73617430169816700, 5.000000000000000000 ) ) ;
#67247 = CARTESIAN_POINT ( 'NONE',  ( 10.50000000000000000, 0.000000000000000000, 6.094999999999989981 ) ) ;
#67249 = VECTOR ( 'NONE', #23932, 1000.000000000000227 ) ;
#67248 = CARTESIAN_POINT ( 'NONE',  ( 15.81246187583935914, -22.22500000000000142, 4.000000000000000000 ) ) ;
#67250 = CARTESIAN_POINT ( 'NONE',  ( -25.49999999999981526, 3.073033219394602611, -6.593910359671030008 ) ) ;
#67251 = CARTESIAN_POINT ( 'NONE',  ( 20.99065804761471199, 4.584330080086930965E-16, 0.000000000000000000 ) ) ;
#67252 = ORIENTED_EDGE ( 'NONE', *, *, #61176, .F. ) ;
#67254 = ORIENTED_EDGE ( 'NONE', *, *, #112036, .F. ) ;
#67253 = ADVANCED_FACE ( 'NONE', ( #140055 ), #137195, .T. ) ;
#67255 = EDGE_CURVE ( 'NONE', #96844, #140981, #138621, .T. ) ;
#67256 = VECTOR ( 'NONE', #30569, 1000.000000000000000 ) ;
#67257 = CARTESIAN_POINT ( 'NONE',  ( -22.49999999999984368, -1.695981523266240076, 4.571483868317929300 ) ) ;
#67258 = ORIENTED_EDGE ( 'NONE', *, *, #103841, .T. ) ;
#67259 = AXIS2_PLACEMENT_3D ( 'NONE', #25406, #23260, #67536 ) ;
#67260 = CARTESIAN_POINT ( 'NONE',  ( 89.97959685856477563, 6.109999999999999432, 1.637169565754164280 ) ) ;
#67261 = VECTOR ( 'NONE', #112374, 1000.000000000000227 ) ;
#67262 = DIRECTION ( 'NONE',  ( -0.000000000000000000, -0.3543493200069152693, 0.9351131265310292928 ) ) ;
#67263 = CARTESIAN_POINT ( 'NONE',  ( 0.000000000000000000, -21.72500000000000142, 4.500000000000000888 ) ) ;
#67264 = CARTESIAN_POINT ( 'NONE',  ( 33.48921356237309510, -27.52281430457078670, 5.000000000000000000 ) ) ;
#67265 = CARTESIAN_POINT ( 'NONE',  ( -1.475890350552386376, 22.22500000000000142, 17.67511803955545702 ) ) ;
#67266 = ORIENTED_EDGE ( 'NONE', *, *, #76020, .F. ) ;
#67268 = EDGE_CURVE ( 'NONE', #108717, #8845, #115379, .T. ) ;
#67267 = VECTOR ( 'NONE', #101808, 1000.000000000000000 ) ;
#67269 = DIRECTION ( 'NONE',  ( 0.000000000000000000, 0.000000000000000000, 1.000000000000000000 ) ) ;
#67270 = DIRECTION ( 'NONE',  ( 0.3543493200069162685, -0.000000000000000000, -0.9351131265310288487 ) ) ;
#67271 = CARTESIAN_POINT ( 'NONE',  ( 6.183988606268994381, 28.73617430169791476, 5.000000000000000000 ) ) ;
#67272 = EDGE_CURVE ( 'NONE', #122674, #15871, #39312, .T. ) ;
#67273 = DIRECTION ( 'NONE',  ( -0.000000000000000000, 0.000000000000000000, 1.000000000000000000 ) ) ;
#67274 = ADVANCED_FACE ( 'NONE', ( #71231 ), #6607, .T. ) ;
#67275 = PRESENTATION_STYLE_ASSIGNMENT (( #46260 ) ) ;
#67277 = ORIENTED_EDGE ( 'NONE', *, *, #74104, .T. ) ;
#67276 = CARTESIAN_POINT ( 'NONE',  ( 33.48921356237309510, -27.52281430457078670, 5.000000000000000000 ) ) ;
#67278 = CARTESIAN_POINT ( 'NONE',  ( -6.183988606268994381, 28.73617430169791476, 5.000000000000000000 ) ) ;
#67279 = CARTESIAN_POINT ( 'NONE',  ( 101.7250270504628986, 5.819803920172573974, -5.819803920172573086 ) ) ;
#67280 = PLANE ( 'NONE',  #116447 ) ;
#67281 = CARTESIAN_POINT ( 'NONE',  ( 8.356812572482565926, -20.24070752338407431, 21.22881796311214941 ) ) ;
#67282 = LINE ( 'NONE', #66565, #35418 ) ;
#67283 = ORIENTED_EDGE ( 'NONE', *, *, #46607, .T. ) ;
#67284 = ORIENTED_EDGE ( 'NONE', *, *, #5607, .F. ) ;
#67285 = ORIENTED_EDGE ( 'NONE', *, *, #67312, .F. ) ;
#67287 = ADVANCED_FACE ( 'NONE', ( #116850 ), #139357, .F. ) ;
#67286 = CARTESIAN_POINT ( 'NONE',  ( 92.02126352523143282, -4.472830434245839371, -4.472830434245840259 ) ) ;
#67288 = VECTOR ( 'NONE', #119265, 1000.000000000000000 ) ;
#67289 = ORIENTED_EDGE ( 'NONE', *, *, #49454, .T. ) ;
#67290 = ADVANCED_FACE ( 'NONE', ( #29129 ), #17525, .T. ) ;
#67291 = PLANE ( 'NONE',  #129646 ) ;
#67292 = CARTESIAN_POINT ( 'NONE',  ( -34.92500000000001137, 10.80009451602710513, 4.759050581649340472 ) ) ;
#67293 = VECTOR ( 'NONE', #94862, 1000.000000000000000 ) ;
#67294 = CARTESIAN_POINT ( 'NONE',  ( 39.66846741159832135, -18.74070752338409562, 20.73178291233850246 ) ) ;
#67295 = DIRECTION ( 'NONE',  ( -0.000000000000000000, 0.3543493200069153248, 0.9351131265310292928 ) ) ;
#67296 = VERTEX_POINT ( 'NONE', #61783 ) ;
#67297 = EDGE_CURVE ( 'NONE', #83415, #121732, #84260, .T. ) ;
#67298 = LINE ( 'NONE', #111493, #72292 ) ;
#67299 = LINE ( 'NONE', #68052, #88234 ) ;
#67300 = LINE ( 'NONE', #1286, #46578 ) ;
#67301 = CARTESIAN_POINT ( 'NONE',  ( 89.30793019189809456, -6.109999999999998543, 1.637169565754158063 ) ) ;
#67302 = ORIENTED_EDGE ( 'NONE', *, *, #105038, .T. ) ;
#67303 = LINE ( 'NONE', #56467, #134632 ) ;
#67304 = DIRECTION ( 'NONE',  ( -1.000000000000000000, -0.000000000000000000, -0.000000000000000000 ) ) ;
#67305 = AXIS2_PLACEMENT_3D ( 'NONE', #120269, #21715, #65249 ) ;
#67306 = ORIENTED_EDGE ( 'NONE', *, *, #113987, .F. ) ;
#67307 = ORIENTED_EDGE ( 'NONE', *, *, #47335, .F. ) ;
#67308 = CARTESIAN_POINT ( 'NONE',  ( 72.18398860626899705, 28.73617430169837661, 5.000000000000000000 ) ) ;
#67309 = CARTESIAN_POINT ( 'NONE',  ( -25.39999999999996305, 3.061616997868383141E-16, -2.500000000000000000 ) ) ;
#67310 = CARTESIAN_POINT ( 'NONE',  ( 24.71290314143521982, 3.967499999999992699, -6.871911579029513994 ) ) ;
#67311 = CARTESIAN_POINT ( 'NONE',  ( 2.301729841053981485, 3.821174125832445049E-16, 0.000000000000000000 ) ) ;
#67312 = EDGE_CURVE ( 'NONE', #20345, #14571, #137909, .T. ) ;
#67313 = AXIS2_PLACEMENT_3D ( 'NONE', #127131, #103239, #50309 ) ;
#67314 = VECTOR ( 'NONE', #121735, 1000.000000000000000 ) ;
#67315 = CARTESIAN_POINT ( 'NONE',  ( 9.005480084712511157, 28.92564299267931816, 4.000000000000000000 ) ) ;
#67316 = DIRECTION ( 'NONE',  ( 0.6830127018922180770, -0.6830127018922204085, -0.2588190451025213501 ) ) ;
#67317 = EDGE_CURVE ( 'NONE', #4021, #85291, #73370, .T. ) ;
#67318 = CARTESIAN_POINT ( 'NONE',  ( 33.29974487139158867, -27.71228299555229313, 4.000000000000000000 ) ) ;
#67320 = EDGE_CURVE ( 'NONE', #126030, #136740, #117537, .T. ) ;
#67319 = PRESENTATION_STYLE_ASSIGNMENT (( #55016 ) ) ;
#67321 = ORIENTED_EDGE ( 'NONE', *, *, #80568, .F. ) ;
#67322 = ORIENTED_EDGE ( 'NONE', *, *, #15795, .T. ) ;
#67323 = DIRECTION ( 'NONE',  ( 0.000000000000000000, 0.000000000000000000, -1.000000000000000000 ) ) ;
#67324 = EDGE_LOOP ( 'NONE', ( #34129, #86241, #36327 ) ) ;
#67325 = ORIENTED_EDGE ( 'NONE', *, *, #24287, .T. ) ;
#67327 = EDGE_CURVE ( 'NONE', #47375, #57071, #75498, .T. ) ;
#67326 = AXIS2_PLACEMENT_3D ( 'NONE', #25241, #113682, #36147 ) ;
#67328 = VECTOR ( 'NONE', #118093, 999.9999999999998863 ) ;
#67329 = VECTOR ( 'NONE', #61960, 1000.000000000000227 ) ;
#67330 = DIRECTION ( 'NONE',  ( -0.6830127018922180770, -0.6830127018922204085, -0.2588190451025214056 ) ) ;
#67331 = ORIENTED_EDGE ( 'NONE', *, *, #31858, .F. ) ;
#67332 = CARTESIAN_POINT ( 'NONE',  ( -68.99451991528748351, 28.92564299267986172, 4.000000000000000000 ) ) ;
#67333 = DIRECTION ( 'NONE',  ( 0.6830127018922180770, -0.6830127018922204085, -0.2588190451025213501 ) ) ;
#67334 = CARTESIAN_POINT ( 'NONE',  ( 34.47516574401890921, -19.50948238788418010, 4.998110765256834398 ) ) ;
#67335 = CARTESIAN_POINT ( 'NONE',  ( 0.000000000000000000, 0.000000000000000000, 0.000000000000000000 ) ) ;
#67336 = AXIS2_PLACEMENT_3D ( 'NONE', #5110, #70465, #16738 ) ;
#67337 = CIRCLE ( 'NONE', #41871, 2.055000000000001048 ) ;
#67338 = AXIS2_PLACEMENT_3D ( 'NONE', #126055, #137645, #36871 ) ;
#67339 = CIRCLE ( 'NONE', #76559, 3.378199999999997871 ) ;
#67340 = CYLINDRICAL_SURFACE ( 'NONE', #136995, 1.749999999999999778 ) ;
#67341 = ORIENTED_EDGE ( 'NONE', *, *, #69191, .F. ) ;
#67342 = VECTOR ( 'NONE', #279, 1000.000000000000000 ) ;
#67343 = ORIENTED_EDGE ( 'NONE', *, *, #26821, .T. ) ;
#67344 = PLANE ( 'NONE',  #73561 ) ;
#67345 = ORIENTED_EDGE ( 'NONE', *, *, #103777, .F. ) ;
#67346 = CARTESIAN_POINT ( 'NONE',  ( -16.49999999999987566, 22.08746187583901843, 4.000000000000000000 ) ) ;
#67347 = VERTEX_POINT ( 'NONE', #19 ) ;
#67348 = CARTESIAN_POINT ( 'NONE',  ( -5.510786437626906675, -27.52281430457051314, 5.000000000000000000 ) ) ;
#67349 = ORIENTED_EDGE ( 'NONE', *, *, #14329, .F. ) ;
#67350 = ORIENTED_EDGE ( 'NONE', *, *, #26524, .F. ) ;
#67351 = CIRCLE ( 'NONE', #4769, 1.898649999999994842 ) ;
#67352 = ORIENTED_EDGE ( 'NONE', *, *, #21015, .T. ) ;
#67353 = DIRECTION ( 'NONE',  ( 0.7071067811865487940, 0.7071067811865463515, 0.000000000000000000 ) ) ;
#67354 = LINE ( 'NONE', #111546, #29798 ) ;
#67355 = DIRECTION ( 'NONE',  ( 0.7071067811865487940, 0.7071067811865463515, -0.000000000000000000 ) ) ;
#67356 = CARTESIAN_POINT ( 'NONE',  ( 118.7087635252314328, -7.482591942790329030E-16, 6.110000000000001208 ) ) ;
#67357 = CARTESIAN_POINT ( 'NONE',  ( 15.79289321881335795, -8.240707523384193323, 5.000000000000000000 ) ) ;
#67358 = VECTOR ( 'NONE', #128299, 999.9999999999998863 ) ;
#67359 = ADVANCED_FACE ( 'NONE', ( #88524 ), #8746, .F. ) ;
#67360 = LINE ( 'NONE', #89110, #89927 ) ;
#67361 = VECTOR ( 'NONE', #67220, 1000.000000000000000 ) ;
#67362 = CYLINDRICAL_SURFACE ( 'NONE', #123466, 0.5000000000000004441 ) ;
#67363 = AXIS2_PLACEMENT_3D ( 'NONE', #48780, #13967, #3108 ) ;
#67364 = CARTESIAN_POINT ( 'NONE',  ( 17.99999999999986855, -18.41253812416056945, 4.000000000000000000 ) ) ;
#67365 = ORIENTED_EDGE ( 'NONE', *, *, #12432, .T. ) ;
#67366 = AXIS2_PLACEMENT_3D ( 'NONE', #50343, #15520, #38048 ) ;
#67367 = LINE ( 'NONE', #57218, #98980 ) ;
#67368 = FACE_OUTER_BOUND ( 'NONE', #44449, .T. ) ;
#67369 = DIRECTION ( 'NONE',  ( -0.000000000000000000, 0.3543493200069153248, 0.9351131265310292928 ) ) ;
#67370 = ORIENTED_EDGE ( 'NONE', *, *, #58049, .F. ) ;
#67371 = AXIS2_PLACEMENT_3D ( 'NONE', #42753, #112279, #86949 ) ;
#67372 = ORIENTED_EDGE ( 'NONE', *, *, #108060, .T. ) ;
#67373 = ORIENTED_EDGE ( 'NONE', *, *, #34181, .T. ) ;
#67374 = LINE ( 'NONE', #12245, #56453 ) ;
#67375 = VERTEX_POINT ( 'NONE', #10909 ) ;
#67376 = AXIS2_PLACEMENT_3D ( 'NONE', #44257, #55849, #122488 ) ;
#67378 = ORIENTED_EDGE ( 'NONE', *, *, #47975, .F. ) ;
#67377 = EDGE_CURVE ( 'NONE', #35802, #101026, #96486, .T. ) ;
#67379 = CARTESIAN_POINT ( 'NONE',  ( -17.30701457986679870, -22.22500000000000142, -1.676113270567823221 ) ) ;
#67380 = CARTESIAN_POINT ( 'NONE',  ( 34.49999999999975842, -17.94567065516886117, 4.994342998332151673 ) ) ;
#67381 = EDGE_CURVE ( 'NONE', #45124, #37390, #31288, .T. ) ;
#67382 = AXIS2_PLACEMENT_3D ( 'NONE', #48867, #82924, #27808 ) ;
#67383 = LINE ( 'NONE', #110126, #72733 ) ;
#67384 = LINE ( 'NONE', #34743, #76556 ) ;
#67385 = ORIENTED_EDGE ( 'NONE', *, *, #127434, .F. ) ;
#67386 = DIRECTION ( 'NONE',  ( -0.3543493200069162685, -0.000000000000000000, -0.9351131265310288487 ) ) ;
#67387 = ORIENTED_EDGE ( 'NONE', *, *, #33529, .T. ) ;
#67389 = EDGE_CURVE ( 'NONE', #139347, #36309, #21098, .T. ) ;
#67388 = DIRECTION ( 'NONE',  ( -0.7071067811865487940, 0.7071067811865463515, -0.000000000000000000 ) ) ;
#67390 = ADVANCED_FACE ( 'NONE', ( #33452 ), #108079, .T. ) ;
#67391 = VECTOR ( 'NONE', #37545, 1000.000000000000000 ) ;
#67392 = CARTESIAN_POINT ( 'NONE',  ( 14.94206980810188590, 7.934999999999993392, 2.126176841940951689 ) ) ;
#67393 = ORIENTED_EDGE ( 'NONE', *, *, #11709, .T. ) ;
#67394 = CARTESIAN_POINT ( 'NONE',  ( 83.03709685856478018, -3.054999999999999272, -5.291415217122919401 ) ) ;
#67395 = DIRECTION ( 'NONE',  ( -0.7071067811865486830, 0.7071067811865464625, 0.000000000000000000 ) ) ;
#67396 = ADVANCED_FACE ( 'NONE', ( #30573 ), #64613, .T. ) ;
#67397 = DIRECTION ( 'NONE',  ( 0.6830127018922180770, -0.6830127018922204085, -0.2588190451025213501 ) ) ;
#67398 = ORIENTED_EDGE ( 'NONE', *, *, #83543, .F. ) ;
#67399 = ORIENTED_EDGE ( 'NONE', *, *, #138091, .F. ) ;
#67400 = VECTOR ( 'NONE', #22825, 1000.000000000000227 ) ;
#67401 = ORIENTED_EDGE ( 'NONE', *, *, #68057, .F. ) ;
#67402 = CARTESIAN_POINT ( 'NONE',  ( 8.816011393731004731, 28.73617430169781173, 5.000000000000000000 ) ) ;
#67403 = DIRECTION ( 'NONE',  ( 0.7071067811865486830, -0.7071067811865464625, -0.000000000000000000 ) ) ;
#67404 = LINE ( 'NONE', #99257, #39583 ) ;
#67405 = CARTESIAN_POINT ( 'NONE',  ( -3.758600742197928835, 21.72499999999999432, 5.000000000000000000 ) ) ;
#67406 = VECTOR ( 'NONE', #39961, 1000.000000000000227 ) ;
#67407 = FACE_OUTER_BOUND ( 'NONE', #37790, .T. ) ;
#67408 = ORIENTED_EDGE ( 'NONE', *, *, #26505, .T. ) ;
#67409 = DIRECTION ( 'NONE',  ( 0.000000000000000000, 0.000000000000000000, 1.000000000000000000 ) ) ;
#67410 = ADVANCED_FACE ( 'NONE', ( #10217 ), #98657, .F. ) ;
#67411 = CYLINDRICAL_SURFACE ( 'NONE', #116040, 9.524999999999995026 ) ;
#67412 = LINE ( 'NONE', #98577, #51457 ) ;
#67413 = ORIENTED_EDGE ( 'NONE', *, *, #120898, .T. ) ;
#67414 = DIRECTION ( 'NONE',  ( 0.000000000000000000, -1.000000000000000000, 0.000000000000000000 ) ) ;
#67415 = VECTOR ( 'NONE', #103359, 1000.000000000000000 ) ;
#67416 = ADVANCED_FACE ( 'NONE', ( #43571 ), #42170, .F. ) ;
#67417 = CARTESIAN_POINT ( 'NONE',  ( -54.29974487139159578, -27.71228299555243879, 4.000000000000000000 ) ) ;
#67418 = ORIENTED_EDGE ( 'NONE', *, *, #89427, .T. ) ;
#67420 = ORIENTED_EDGE ( 'NONE', *, *, #20684, .F. ) ;
#67419 = DIRECTION ( 'NONE',  ( -0.7071067811865486830, -0.7071067811865464625, 0.000000000000000000 ) ) ;
#67421 = ORIENTED_EDGE ( 'NONE', *, *, #91009, .F. ) ;
#67422 = CARTESIAN_POINT ( 'NONE',  ( -32.99999999999976552, -16.02097659208073566, -11.96015758381200733 ) ) ;
#67423 = PLANE ( 'NONE',  #4354 ) ;
#67424 = EDGE_CURVE ( 'NONE', #30921, #109630, #142886, .T. ) ;
#67426 = ORIENTED_EDGE ( 'NONE', *, *, #33006, .F. ) ;
#67425 = AXIS2_PLACEMENT_3D ( 'NONE', #42135, #129831, #42847 ) ;
#67427 = CARTESIAN_POINT ( 'NONE',  ( -27.18398860626900060, 28.73617430169806042, 5.000000000000000000 ) ) ;
#67428 = DIRECTION ( 'NONE',  ( 0.7071067811865486830, -0.7071067811865464625, -0.000000000000000000 ) ) ;
#67429 = LINE ( 'NONE', #14451, #76405 ) ;
#67430 = CARTESIAN_POINT ( 'NONE',  ( -69.48921356237309510, -27.52281430457103895, 5.000000000000000000 ) ) ;
#67431 = CARTESIAN_POINT ( 'NONE',  ( -7.140000000000001457, -39.92999999999999261, -7.899272885403729738 ) ) ;
#67432 = CARTESIAN_POINT ( 'NONE',  ( 36.48921356237310221, -27.52281430457080802, 5.000000000000000000 ) ) ;
#67433 = CARTESIAN_POINT ( 'NONE',  ( 18.60486233187509697, 21.75929247661549226, 21.32995629748182154 ) ) ;
#67435 = EDGE_CURVE ( 'NONE', #32728, #122903, #118989, .T. ) ;
#67434 = LINE ( 'NONE', #56588, #93398 ) ;
#67436 = LINE ( 'NONE', #111633, #103867 ) ;
#67437 = CARTESIAN_POINT ( 'NONE',  ( 22.72873647476856007, 5.808823158059031044, -5.808823158059038150 ) ) ;
#67438 = DIRECTION ( 'NONE',  ( -0.3543493200069163240, 0.000000000000000000, 0.9351131265310288487 ) ) ;
#67439 = FACE_OUTER_BOUND ( 'NONE', #131415, .T. ) ;
#67440 = VECTOR ( 'NONE', #99251, 1000.000000000000000 ) ;
#67441 = CARTESIAN_POINT ( 'NONE',  ( -39.18398860626899705, 28.73617430169814568, 5.000000000000000000 ) ) ;
#67442 = DIRECTION ( 'NONE',  ( 0.6830127018922180770, -0.6830127018922204085, -0.2588190451025213501 ) ) ;
#67443 = ORIENTED_EDGE ( 'NONE', *, *, #7716, .T. ) ;
#67444 = ORIENTED_EDGE ( 'NONE', *, *, #71199, .F. ) ;
#67446 = EDGE_CURVE ( 'NONE', #23445, #58187, #74811, .T. ) ;
#67445 = AXIS2_PLACEMENT_3D ( 'NONE', #107776, #41113, #32395 ) ;
#67447 = CARTESIAN_POINT ( 'NONE',  ( 100.0208333333333286, 7.949999999999999289, 2.130196079827431532 ) ) ;
#67448 = VECTOR ( 'NONE', #5583, 999.9999999999998863 ) ;
#67449 = VERTEX_POINT ( 'NONE', #41424 ) ;
#67450 = ORIENTED_EDGE ( 'NONE', *, *, #111440, .F. ) ;
#67451 = EDGE_CURVE ( 'NONE', #22127, #49472, #32721, .T. ) ;
#67452 = EDGE_LOOP ( 'NONE', ( #129826, #127408, #113617, #59100, #14006 ) ) ;
#67453 = CARTESIAN_POINT ( 'NONE',  ( 34.45011844616451668, -5.997695858405997171, 5.000000000000000888 ) ) ;
#67454 = LINE ( 'NONE', #79055, #78853 ) ;
#67455 = AXIS2_PLACEMENT_3D ( 'NONE', #89835, #111604, #1380 ) ;
#67456 = CIRCLE ( 'NONE', #85944, 5.968999999999998529 ) ;
#67457 = AXIS2_PLACEMENT_3D ( 'NONE', #50112, #73296, #94306 ) ;
#67458 = VECTOR ( 'NONE', #44115, 1000.000000000000000 ) ;
#67459 = CARTESIAN_POINT ( 'NONE',  ( -34.17183060077623935, 3.759292476615681888, 4.000000000000000000 ) ) ;
#67460 = ORIENTED_EDGE ( 'NONE', *, *, #59959, .F. ) ;
#67461 = LINE ( 'NONE', #13728, #30089 ) ;
#67462 = EDGE_CURVE ( 'NONE', #142044, #42523, #121123, .T. ) ;
#67463 = VECTOR ( 'NONE', #3153, 1000.000000000000000 ) ;
#67464 = FACE_OUTER_BOUND ( 'NONE', #84312, .T. ) ;
#67465 = DIRECTION ( 'NONE',  ( 0.000000000000000000, -1.000000000000000000, 0.000000000000000000 ) ) ;
#67466 = DIRECTION ( 'NONE',  ( 0.7071067811865487940, 0.7071067811865463515, 0.000000000000000000 ) ) ;
#67467 = VERTEX_POINT ( 'NONE', #97200 ) ;
#67468 = DIRECTION ( 'NONE',  ( -1.000000000000000000, -0.000000000000000000, -0.000000000000000000 ) ) ;
#67469 = FACE_OUTER_BOUND ( 'NONE', #78983, .T. ) ;
#67470 = LINE ( 'NONE', #134134, #5616 ) ;
#67471 = CARTESIAN_POINT ( 'NONE',  ( 31.49999999999979039, 19.46639925780206326, 5.000000000000000000 ) ) ;
#67472 = DIRECTION ( 'NONE',  ( -0.000000000000000000, -0.3543493200069152693, 0.9351131265310292928 ) ) ;
#67473 = CARTESIAN_POINT ( 'NONE',  ( -1.499999999999994449, 22.22500000000000142, 4.362957392718788796 ) ) ;
#67474 = CARTESIAN_POINT ( 'NONE',  ( -20.70025512860841133, -27.71228299555191654, 4.000000000000000000 ) ) ;
#67475 = LINE ( 'NONE', #90639, #49888 ) ;
#67476 = DIRECTION ( 'NONE',  ( 0.000000000000000000, -1.000000000000000000, 0.000000000000000000 ) ) ;
#67477 = ORIENTED_EDGE ( 'NONE', *, *, #133816, .T. ) ;
#67478 = VERTEX_POINT ( 'NONE', #141466 ) ;
#67479 = CARTESIAN_POINT ( 'NONE',  ( 119.0004301918981184, -3.055000000000002380, 5.291415217122920289 ) ) ;
#67480 = VERTEX_POINT ( 'NONE', #97961 ) ;
#67481 = ADVANCED_FACE ( 'NONE', ( #21822 ), #110227, .F. ) ;
#67482 = DIRECTION ( 'NONE',  ( 0.7071067811865487940, 0.7071067811865463515, 0.000000000000000000 ) ) ;
#67483 = FACE_OUTER_BOUND ( 'NONE', #114764, .T. ) ;
#67484 = ADVANCED_FACE ( 'NONE', ( #11620 ), #34138, .T. ) ;
#67485 = CARTESIAN_POINT ( 'NONE',  ( 22.07159235450331991, 9.902892378096218942E-16, 0.000000000000000000 ) ) ;
#67486 = FACE_OUTER_BOUND ( 'NONE', #80993, .T. ) ;
#67487 = CIRCLE ( 'NONE', #139297, 2.500000000000000444 ) ;
#67488 = VECTOR ( 'NONE', #110590, 1000.000000000000000 ) ;
#67489 = CARTESIAN_POINT ( 'NONE',  ( 110.5995968585647802, -6.109999999999997655, -1.637169565754160283 ) ) ;
#67490 = ORIENTED_EDGE ( 'NONE', *, *, #121701, .T. ) ;
#67491 = VECTOR ( 'NONE', #29517, 999.9999999999998863 ) ;
#67492 = ORIENTED_EDGE ( 'NONE', *, *, #106476, .T. ) ;
#67493 = LINE ( 'NONE', #111684, #94762 ) ;
#67494 = VECTOR ( 'NONE', #133930, 1000.000000000000000 ) ;
#67495 = DIRECTION ( 'NONE',  ( -0.6830127018922180770, -0.6830127018922204085, -0.2588190451025213501 ) ) ;
#67496 = ORIENTED_EDGE ( 'NONE', *, *, #108806, .F. ) ;
#67497 = ORIENTED_EDGE ( 'NONE', *, *, #137661, .F. ) ;
#67498 = CARTESIAN_POINT ( 'NONE',  ( 35.43793019189810423, -6.110000000000001208, 1.637169565754158951 ) ) ;
#67499 = ORIENTED_EDGE ( 'NONE', *, *, #135915, .T. ) ;
#67500 = VECTOR ( 'NONE', #119283, 1000.000000000000000 ) ;
#67501 = FACE_OUTER_BOUND ( 'NONE', #121649, .T. ) ;
#67502 = FACE_OUTER_BOUND ( 'NONE', #9710, .T. ) ;
#67503 = EDGE_CURVE ( 'NONE', #119351, #129380, #134900, .T. ) ;
#67504 = VECTOR ( 'NONE', #100485, 999.9999999999998863 ) ;
#67505 = CARTESIAN_POINT ( 'NONE',  ( 31.12043019189811233, 3.055000000000001936, -5.291415217122916737 ) ) ;
#67506 = ORIENTED_EDGE ( 'NONE', *, *, #99262, .T. ) ;
#67507 = DIRECTION ( 'NONE',  ( 0.000000000000000000, -1.000000000000000000, 0.000000000000000000 ) ) ;
#67508 = ORIENTED_EDGE ( 'NONE', *, *, #74455, .T. ) ;
#67509 = ORIENTED_EDGE ( 'NONE', *, *, #56708, .T. ) ;
#67510 = VECTOR ( 'NONE', #110921, 1000.000000000000000 ) ;
#67511 = ORIENTED_EDGE ( 'NONE', *, *, #26766, .T. ) ;
#67512 = CIRCLE ( 'NONE', #104406, 2.055000000000000604 ) ;
#67513 = CARTESIAN_POINT ( 'NONE',  ( 34.42499999999998295, -22.22500000000000142, 5.000000000000000000 ) ) ;
#67514 = PLANE ( 'NONE',  #11735 ) ;
#67515 = ORIENTED_EDGE ( 'NONE', *, *, #129540, .T. ) ;
#67516 = CARTESIAN_POINT ( 'NONE',  ( 5.501836514860404037, -17.24070752338409918, 8.407044977365213612 ) ) ;
#67517 = DIRECTION ( 'NONE',  ( 1.000000000000000000, 0.000000000000000000, 0.000000000000000000 ) ) ;
#67518 = AXIS2_PLACEMENT_3D ( 'NONE', #130880, #75773, #98233 ) ;
#67519 = CARTESIAN_POINT ( 'NONE',  ( -31.44665057663198482, 2.259292476615694323, 14.86850063742361705 ) ) ;
#67520 = CARTESIAN_POINT ( 'NONE',  ( -5.671830600776424092, -18.74070752338409207, 4.000000000000000000 ) ) ;
#67521 = FACE_BOUND ( 'NONE', #143486, .T. ) ;
#67522 = ORIENTED_EDGE ( 'NONE', *, *, #60411, .T. ) ;
#67523 = DIRECTION ( 'NONE',  ( 1.000000000000000000, 0.000000000000000000, 0.000000000000000000 ) ) ;
#67524 = LINE ( 'NONE', #14542, #29949 ) ;
#67525 = CARTESIAN_POINT ( 'NONE',  ( 14.30673006690391702, -3.740707523384251942, 12.88036043432864020 ) ) ;
#67526 = FACE_OUTER_BOUND ( 'NONE', #13874, .T. ) ;
#67527 = ORIENTED_EDGE ( 'NONE', *, *, #120584, .T. ) ;
#67528 = CARTESIAN_POINT ( 'NONE',  ( 24.10830628287044419, 1.633150327867706864, -6.094999999999981100 ) ) ;
#67529 = VERTEX_POINT ( 'NONE', #22496 ) ;
#67530 = VERTEX_POINT ( 'NONE', #135594 ) ;
#67531 = VECTOR ( 'NONE', #103957, 1000.000000000000000 ) ;
#67532 = ORIENTED_EDGE ( 'NONE', *, *, #118347, .T. ) ;
#67533 = CARTESIAN_POINT ( 'NONE',  ( 50.80793019189810167, -6.109999999999998543, 1.637169565754158507 ) ) ;
#67534 = ORIENTED_EDGE ( 'NONE', *, *, #379, .T. ) ;
#67535 =( BOUNDED_SURFACE ( )  B_SPLINE_SURFACE ( 3, 2, ( 
 ( #119348, #20765, #7736 ),
 ( #29492, #76618, #40411 ),
 ( #129519, #109922, #96170 ),
 ( #9132, #10586, #109206 ),
 ( #41819, #141868, #128818 ),
 ( #42563, #120789, #21500 ),
 ( #118657, #141110, #30219 ),
 ( #62880, #52681, #41100 ),
 ( #54164, #86035, #85295 ),
 ( #95470, #20042, #86764 ),
 ( #65759, #30963, #130987 ),
 ( #75882, #98350, #139736 ) ),
 .UNSPECIFIED., .F., .F., .F. ) 
 B_SPLINE_SURFACE_WITH_KNOTS ( ( 4, 2, 2, 2, 2, 4 ),
 ( 3, 3 ),
 ( 0.000000000000000000, 0.001647923167088021727, 0.002471884750632032807, 0.003295846334176043453, 0.004943769501264065613, 0.006591692668352086906 ),
 ( 0.000000000000000000, 1.000000000000000000 ),
 .UNSPECIFIED. ) 
 GEOMETRIC_REPRESENTATION_ITEM ( )  RATIONAL_B_SPLINE_SURFACE ( (
 ( 1.000000000000000000, 0.7071067811865475727, 1.000000000000000000),
 ( 1.000000000000000000, 0.7122033721490172997, 1.000000000000000000),
 ( 1.000000000000000000, 0.7158366153114614772, 1.000000000000000000),
 ( 1.000000000000000000, 0.7192720032936079644, 1.000000000000000000),
 ( 1.000000000000000000, 0.7200809050419507695, 1.000000000000000000),
 ( 1.000000000000000000, 0.7210491446662772308, 1.000000000000000000),
 ( 1.000000000000000000, 0.7212054070302064135, 1.000000000000000000),
 ( 1.000000000000000000, 0.7207522793910704495, 1.000000000000000000),
 ( 1.000000000000000000, 0.7192424821650112987, 1.000000000000000000),
 ( 1.000000000000000000, 0.7143802006613869660, 1.000000000000000000),
 ( 1.000000000000000000, 0.7109884861397428590, 1.000000000000000000),
 ( 1.000000000000000000, 0.7071067811865475727, 1.000000000000000000) ) ) 
 REPRESENTATION_ITEM ( '' )  SURFACE ( )  );
#67536 = DIRECTION ( 'NONE',  ( -0.7071067811865486830, 0.7071067811865464625, 0.000000000000000000 ) ) ;
#67537 = CARTESIAN_POINT ( 'NONE',  ( 23.91508676806224187, -12.74070752338414536, 18.74364270924359843 ) ) ;
#67538 = ORIENTED_EDGE ( 'NONE', *, *, #37997, .T. ) ;
#67539 = VECTOR ( 'NONE', #42459, 1000.000000000000000 ) ;
#67540 = VECTOR ( 'NONE', #69890, 999.9999999999998863 ) ;
#67541 = VECTOR ( 'NONE', #66993, 1000.000000000000000 ) ;
#67542 = AXIS2_PLACEMENT_3D ( 'NONE', #141671, #9701, #119180 ) ;
#67543 = CARTESIAN_POINT ( 'NONE',  ( 15.05159235450332034, 9.902892378096218942E-16, 0.000000000000000000 ) ) ;
#67544 = DIRECTION ( 'NONE',  ( 0.6830127018922181881, 0.6830127018922202975, -0.2588190451025214056 ) ) ;
#67545 = FACE_OUTER_BOUND ( 'NONE', #129931, .T. ) ;
#67546 = CARTESIAN_POINT ( 'NONE',  ( 63.48921356237309510, -27.52281430457099631, 5.000000000000000000 ) ) ;
#67547 = ORIENTED_EDGE ( 'NONE', *, *, #40358, .T. ) ;
#67548 = EDGE_CURVE ( 'NONE', #28316, #89814, #12359, .T. ) ;
#67549 = ORIENTED_EDGE ( 'NONE', *, *, #100458, .T. ) ;
#67550 = VECTOR ( 'NONE', #81692, 999.9999999999998863 ) ;
#67551 = VECTOR ( 'NONE', #39820, 1000.000000000000000 ) ;
#67552 = ORIENTED_EDGE ( 'NONE', *, *, #6913, .T. ) ;
#67553 = AXIS2_PLACEMENT_3D ( 'NONE', #23145, #68854, #101444 ) ;
#67554 = VERTEX_POINT ( 'NONE', #79100 ) ;
#67555 = LINE ( 'NONE', #89967, #31117 ) ;
#67556 = LINE ( 'NONE', #121177, #104656 ) ;
#67557 = EDGE_LOOP ( 'NONE', ( #57962, #106031, #126810, #98187, #103084 ) ) ;
#67558 = VECTOR ( 'NONE', #68302, 1000.000000000000000 ) ;
#67559 = ORIENTED_EDGE ( 'NONE', *, *, #51807, .T. ) ;
#67560 = DIRECTION ( 'NONE',  ( -0.7071067811865486830, -0.7071067811865464625, -0.000000000000000000 ) ) ;
#67561 = DIRECTION ( 'NONE',  ( -0.000000000000000000, -0.000000000000000000, 1.000000000000000000 ) ) ;
#67562 = EDGE_CURVE ( 'NONE', #31625, #18811, #24664, .T. ) ;
#67563 = EDGE_CURVE ( 'NONE', #33856, #83993, #131751, .T. ) ;
#67564 = LINE ( 'NONE', #112464, #117981 ) ;
#67565 = ORIENTED_EDGE ( 'NONE', *, *, #111236, .F. ) ;
#67566 = PLANE ( 'NONE',  #104305 ) ;
#67568 = EDGE_CURVE ( 'NONE', #12106, #122233, #68228, .T. ) ;
#67567 = CARTESIAN_POINT ( 'NONE',  ( 23.24240614354803114, -1.100504885936606669, 4.183743008713594058 ) ) ;
#67569 = EDGE_CURVE ( 'NONE', #51167, #137268, #14509, .T. ) ;
#67570 = CARTESIAN_POINT ( 'NONE',  ( 27.77540314143521982, -2.126176841940958351, -7.934999999999989839 ) ) ;
#67571 = VERTEX_POINT ( 'NONE', #112405 ) ;
#67572 = CARTESIAN_POINT ( 'NONE',  ( 114.9745968585647660, 1.637169565754164280, -6.109999999999997655 ) ) ;
#67573 = ADVANCED_FACE ( 'NONE', ( #90670 ), #69642, .F. ) ;
#67574 = CARTESIAN_POINT ( 'NONE',  ( 62.78752705046289151, 0.000000000000000000, -7.949999999999998401 ) ) ;
#67575 = DIRECTION ( 'NONE',  ( 0.000000000000000000, 0.2631995976047483699, 0.9647414015272167687 ) ) ;
#67576 = CARTESIAN_POINT ( 'NONE',  ( 21.48921356237309155, -27.52281430457070499, 5.000000000000000000 ) ) ;
#67578 = ORIENTED_EDGE ( 'NONE', *, *, #29661, .F. ) ;
#67577 = CARTESIAN_POINT ( 'NONE',  ( 24.48921356237309510, -27.52281430457072631, 5.000000000000000000 ) ) ;
#67579 = DIRECTION ( 'NONE',  ( -0.000000000000000000, 0.000000000000000000, 1.000000000000000000 ) ) ;
#67580 = ORIENTED_EDGE ( 'NONE', *, *, #74032, .F. ) ;
#67581 = EDGE_CURVE ( 'NONE', #8995, #29676, #91384, .T. ) ;
#67582 = DIRECTION ( 'NONE',  ( 0.6830127018922181881, 0.6830127018922202975, -0.2588190451025214056 ) ) ;
#67583 = DIRECTION ( 'NONE',  ( 0.7071067811865487940, -0.7071067811865463515, 0.000000000000000000 ) ) ;
#67584 = DIRECTION ( 'NONE',  ( 0.7071067811865487940, 0.7071067811865463515, 0.000000000000000000 ) ) ;
#67585 = ORIENTED_EDGE ( 'NONE', *, *, #85527, .F. ) ;
#67586 = STYLED_ITEM ( 'NONE', ( #103648 ), #98966 ) ;
#67587 = FACE_OUTER_BOUND ( 'NONE', #142692, .T. ) ;
#67588 = ADVANCED_FACE ( 'NONE', ( #25372 ), #2908, .T. ) ;
#67589 = VECTOR ( 'NONE', #98331, 1000.000000000000000 ) ;
#67590 = VECTOR ( 'NONE', #20432, 1000.000000000000114 ) ;
#67591 = DIRECTION ( 'NONE',  ( -0.7071067811865487940, 0.7071067811865463515, -0.000000000000000000 ) ) ;
#67592 = LINE ( 'NONE', #111782, #111565 ) ;
#67593 = VERTEX_POINT ( 'NONE', #35595 ) ;
#67594 = AXIS2_PLACEMENT_3D ( 'NONE', #26257, #115352, #138587 ) ;
#67595 = DIRECTION ( 'NONE',  ( 0.7071067811865487940, 0.7071067811865463515, 0.000000000000000000 ) ) ;
#67596 = VERTEX_POINT ( 'NONE', #79822 ) ;
#67597 = EDGE_CURVE ( 'NONE', #102769, #139749, #47891, .T. ) ;
#67598 = DIRECTION ( 'NONE',  ( -0.3543493200069162685, -0.000000000000000000, -0.9351131265310288487 ) ) ;
#67600 = ORIENTED_EDGE ( 'NONE', *, *, #46495, .F. ) ;
#67599 = CARTESIAN_POINT ( 'NONE',  ( 14.99999999999990230, -16.02097659208069658, -11.96015758381211924 ) ) ;
#67601 = ORIENTED_EDGE ( 'NONE', *, *, #97226, .T. ) ;
#67602 = CARTESIAN_POINT ( 'NONE',  ( -13.10966639810773771, 3.759292476615678336, 4.164048746910666843 ) ) ;
#67603 = SURFACE_STYLE_FILL_AREA ( #87178 ) ;
#67604 = ADVANCED_FACE ( 'NONE', ( #67501 ), #124701, .F. ) ;
#67605 = ORIENTED_EDGE ( 'NONE', *, *, #80794, .T. ) ;
#67606 = DIRECTION ( 'NONE',  ( -0.7071067811865486830, -0.7071067811865464625, -0.000000000000000000 ) ) ;
#67607 = FILL_AREA_STYLE ('',( #1560 ) ) ;
#67608 = CARTESIAN_POINT ( 'NONE',  ( 18.72281430457046270, -21.72500000000000142, 5.000000000000000000 ) ) ;
#67609 = ORIENTED_EDGE ( 'NONE', *, *, #7920, .F. ) ;
#67610 = LINE ( 'NONE', #123416, #85987 ) ;
#67611 = CARTESIAN_POINT ( 'NONE',  ( 19.49999999999986500, 16.18958161055405043, -11.56426086740806802 ) ) ;
#67612 = AXIS2_PLACEMENT_3D ( 'NONE', #58043, #70357, #59464 ) ;
#67614 = ADVANCED_FACE ( 'NONE', ( #47205 ), #77653, .F. ) ;
#67613 = LINE ( 'NONE', #111802, #125810 ) ;
#67615 = VECTOR ( 'NONE', #99461, 1000.000000000000000 ) ;
#67616 = CARTESIAN_POINT ( 'NONE',  ( 125.5568156377396605, -3.969148909990495078, 6.850047280582228559 ) ) ;
#67617 = CARTESIAN_POINT ( 'NONE',  ( 128.8500270504628986, -5.819803920172572198, -5.819803920172572198 ) ) ;
#67618 = CARTESIAN_POINT ( 'NONE',  ( 9.994118527364397764, 2.500000000000000888, 0.000000000000000000 ) ) ;
#67619 = ORIENTED_EDGE ( 'NONE', *, *, #36600, .F. ) ;
#67620 = ORIENTED_EDGE ( 'NONE', *, *, #100449, .F. ) ;
#67621 = ORIENTED_EDGE ( 'NONE', *, *, #125138, .F. ) ;
#67622 = EDGE_CURVE ( 'NONE', #29169, #73773, #55904, .T. ) ;
#67623 = DIRECTION ( 'NONE',  ( 1.000000000000000000, 0.000000000000000000, 0.000000000000000000 ) ) ;
#67624 = ORIENTED_EDGE ( 'NONE', *, *, #141851, .F. ) ;
#67625 = EDGE_LOOP ( 'NONE', ( #111438, #14287, #105468, #129845 ) ) ;
#67626 = ADVANCED_FACE ( 'NONE', ( #100102 ), #63091, .T. ) ;
#67627 = ORIENTED_EDGE ( 'NONE', *, *, #40962, .F. ) ;
#67628 = LINE ( 'NONE', #33568, #94187 ) ;
#67629 = DIRECTION ( 'NONE',  ( 0.7071067811865487940, 0.7071067811865463515, 0.000000000000000000 ) ) ;
#67630 = VERTEX_POINT ( 'NONE', #111691 ) ;
#67631 = EDGE_CURVE ( 'NONE', #89838, #29880, #1461, .T. ) ;
#67632 = PLANE ( 'NONE',  #80931 ) ;
#67634 = EDGE_CURVE ( 'NONE', #104233, #105152, #137737, .T. ) ;
#67633 = PLANE ( 'NONE',  #81426 ) ;
#67635 = CARTESIAN_POINT ( 'NONE',  ( -13.49999999999990052, 15.05218569542901363, 5.000000000000000000 ) ) ;
#67636 = PLANE ( 'NONE',  #60394 ) ;
#67637 = CARTESIAN_POINT ( 'NONE',  ( 119.2920968585647756, -5.291415217122921177, 3.054999999999999272 ) ) ;
#67638 = ORIENTED_EDGE ( 'NONE', *, *, #141379, .F. ) ;
#67639 = DIRECTION ( 'NONE',  ( -0.7071067811865487940, 0.7071067811865463515, -0.000000000000000000 ) ) ;
#67640 = CARTESIAN_POINT ( 'NONE',  ( -7.001930566820925961, -22.22500000000000142, 4.500000000000000888 ) ) ;
#67642 = AXIS2_PLACEMENT_3D ( 'NONE', #76894, #108023, #43517 ) ;
#67641 = LINE ( 'NONE', #111835, #105088 ) ;
#67643 = CARTESIAN_POINT ( 'NONE',  ( 26.99451991528749417, 28.92564299267956685, 4.000000000000000000 ) ) ;
#67644 = FACE_OUTER_BOUND ( 'NONE', #108612, .T. ) ;
#67645 = PLANE ( 'NONE',  #21456 ) ;
#67646 = DIRECTION ( 'NONE',  ( 1.000000000000000000, 0.000000000000000000, 0.000000000000000000 ) ) ;
#67647 = CARTESIAN_POINT ( 'NONE',  ( 48.35002705046287730, -5.819803920172572198, -5.819803920172572198 ) ) ;
#67648 = LINE ( 'NONE', #102408, #125523 ) ;
#67649 = FACE_OUTER_BOUND ( 'NONE', #82852, .T. ) ;
#67650 = ORIENTED_EDGE ( 'NONE', *, *, #89283, .F. ) ;
#67651 = ORIENTED_EDGE ( 'NONE', *, *, #121803, .T. ) ;
#67652 = CARTESIAN_POINT ( 'NONE',  ( 42.70833333333333570, -3.974999999999999201, -6.884901960086287964 ) ) ;
#67653 = EDGE_CURVE ( 'NONE', #65849, #104144, #71059, .T. ) ;
#67654 = PLANE ( 'NONE',  #134340 ) ;
#67655 = DIRECTION ( 'NONE',  ( 0.6830127018922181881, 0.6830127018922202975, -0.2588190451025214056 ) ) ;
#67656 = ORIENTED_EDGE ( 'NONE', *, *, #69741, .T. ) ;
#67657 = AXIS2_PLACEMENT_3D ( 'NONE', #71329, #15464, #115486 ) ;
#67658 = CIRCLE ( 'NONE', #28196, 2.500000000000000444 ) ;
#67659 = VECTOR ( 'NONE', #7891, 1000.000000000000227 ) ;
#67660 = DIRECTION ( 'NONE',  ( -0.7071067811865486830, -0.7071067811865464625, 0.000000000000000000 ) ) ;
#67661 = FACE_OUTER_BOUND ( 'NONE', #94313, .T. ) ;
#67662 = VECTOR ( 'NONE', #107097, 1000.000000000000000 ) ;
#67663 = AXIS2_PLACEMENT_3D ( 'NONE', #120402, #43596, #108823 ) ;
#67664 = CARTESIAN_POINT ( 'NONE',  ( 39.08376352523143282, -6.110000000000001208, -3.741295971395164515E-16 ) ) ;
#67665 = EDGE_CURVE ( 'NONE', #66690, #12661, #62318, .T. ) ;
#67666 = EDGE_LOOP ( 'NONE', ( #129689, #23610, #12246, #80163 ) ) ;
#67667 = DIRECTION ( 'NONE',  ( 0.3543493200069162685, -0.000000000000000000, -0.9351131265310288487 ) ) ;
#67668 = ORIENTED_EDGE ( 'NONE', *, *, #61374, .T. ) ;
#67669 = ORIENTED_EDGE ( 'NONE', *, *, #83543, .T. ) ;
#67670 = AXIS2_PLACEMENT_3D ( 'NONE', #107712, #105561, #29436 ) ;
#67671 = VECTOR ( 'NONE', #51203, 1000.000000000000227 ) ;
#67672 = TOROIDAL_SURFACE ( 'NONE', #30599, 31.92999999999999261, 3.000000000000000000 ) ;
#67673 = CYLINDRICAL_SURFACE ( 'NONE', #58916, 0.5000000000000004441 ) ;
#67674 = DIRECTION ( 'NONE',  ( -0.7071067811865487940, 0.7071067811865463515, 0.000000000000000000 ) ) ;
#67675 = DIRECTION ( 'NONE',  ( -0.7071067811865486830, -0.7071067811865463515, 0.000000000000000000 ) ) ;
#67676 = ORIENTED_EDGE ( 'NONE', *, *, #36841, .F. ) ;
#67677 = EDGE_CURVE ( 'NONE', #111310, #57451, #130230, .T. ) ;
#67678 = DIRECTION ( 'NONE',  ( -0.7071067811865486830, -0.7071067811865464625, -0.000000000000000000 ) ) ;
#67679 = EDGE_LOOP ( 'NONE', ( #12921, #68632, #28342, #39074 ) ) ;
#67680 = FACE_OUTER_BOUND ( 'NONE', #141638, .T. ) ;
#67681 = CARTESIAN_POINT ( 'NONE',  ( 0.000000000000000000, 0.000000000000000000, 7.950000000000000178 ) ) ;
#67682 = FACE_OUTER_BOUND ( 'NONE', #125835, .T. ) ;
#67683 = CARTESIAN_POINT ( 'NONE',  ( -72.18398860626899705, 28.73617430169837661, 5.000000000000000000 ) ) ;
#67684 = CARTESIAN_POINT ( 'NONE',  ( -23.60898926630779826, -0.6778661889157658882, 4.000000000000000000 ) ) ;
#67685 = EDGE_CURVE ( 'NONE', #108226, #101224, #60922, .T. ) ;
#67686 = ORIENTED_EDGE ( 'NONE', *, *, #63323, .T. ) ;
#67687 = CARTESIAN_POINT ( 'NONE',  ( -15.48921356237309510, -27.52281430457066236, 5.000000000000000000 ) ) ;
#67688 = CARTESIAN_POINT ( 'NONE',  ( 62.62043019189811588, 3.055000000000001936, -5.291415217122916737 ) ) ;
#67689 = CARTESIAN_POINT ( 'NONE',  ( -29.52663903635766829, -5.240707523384225297, 16.25846745537488758 ) ) ;
#67690 = CARTESIAN_POINT ( 'NONE',  ( 14.81601139373099585, 28.73617430169776910, 5.000000000000000000 ) ) ;
#67691 = CARTESIAN_POINT ( 'NONE',  ( 0.000000000000000000, 9.735942053221458872E-16, -7.950000000000000178 ) ) ;
#67692 = ORIENTED_EDGE ( 'NONE', *, *, #28429, .F. ) ;
#67693 = LINE ( 'NONE', #25565, #130305 ) ;
#67694 = DIRECTION ( 'NONE',  ( 0.000000000000000000, 0.000000000000000000, 1.000000000000000000 ) ) ;
#67695 = ORIENTED_EDGE ( 'NONE', *, *, #23351, .F. ) ;
#67696 = EDGE_CURVE ( 'NONE', #126832, #113508, #61619, .T. ) ;
#67697 = AXIS2_PLACEMENT_3D ( 'NONE', #56495, #91243, #58649 ) ;
#67698 = VECTOR ( 'NONE', #72529, 999.9999999999998863 ) ;
#67699 = EDGE_CURVE ( 'NONE', #70301, #11420, #116673, .T. ) ;
#67700 = FACE_OUTER_BOUND ( 'NONE', #127959, .T. ) ;
#67701 = ORIENTED_EDGE ( 'NONE', *, *, #21636, .T. ) ;
#67702 = AXIS2_PLACEMENT_3D ( 'NONE', #115096, #15092, #25998 ) ;
#67703 = LINE ( 'NONE', #48063, #42283 ) ;
#67704 = DIRECTION ( 'NONE',  ( -1.000000000000000000, 0.000000000000000000, 0.000000000000000000 ) ) ;
#67705 = CARTESIAN_POINT ( 'NONE',  ( -10.99806943317894437, -22.22500000000000142, 4.500000000000000888 ) ) ;
#67706 = VECTOR ( 'NONE', #97170, 1000.000000000000000 ) ;
#67707 = CARTESIAN_POINT ( 'NONE',  ( -3.328169399223500413, 14.25929247661557575, 4.000000000000000000 ) ) ;
#67708 = FACE_BOUND ( 'NONE', #74658, .T. ) ;
#67709 = EDGE_CURVE ( 'NONE', #56788, #87398, #81953, .T. ) ;
#67710 = CARTESIAN_POINT ( 'NONE',  ( -14.24715658456393541, 6.719242673238161601, 5.000000000000000000 ) ) ;
#67711 = LINE ( 'NONE', #69113, #32767 ) ;
#67712 = DIRECTION ( 'NONE',  ( 0.7071067811865486830, -0.7071067811865464625, -0.000000000000000000 ) ) ;
#67714 = EDGE_LOOP ( 'NONE', ( #92676, #138450, #17837, #122646 ) ) ;
#67713 = CARTESIAN_POINT ( 'NONE',  ( 0.000000000000000000, 21.72500000000000142, 4.500000000000000888 ) ) ;
#67715 = DIRECTION ( 'NONE',  ( 0.6830127018922181881, 0.6830127018922202975, -0.2588190451025214056 ) ) ;
#67716 = VERTEX_POINT ( 'NONE', #37715 ) ;
#67717 = ORIENTED_EDGE ( 'NONE', *, *, #82196, .F. ) ;
#67718 = CARTESIAN_POINT ( 'NONE',  ( 71.07876352523146579, -7.482591942790325086E-16, 6.109999999999998543 ) ) ;
#67719 = ORIENTED_EDGE ( 'NONE', *, *, #28322, .T. ) ;
#67720 = DIRECTION ( 'NONE',  ( 0.6830127018922180770, 0.6830127018922202975, -0.2588190451025213501 ) ) ;
#67721 = DIRECTION ( 'NONE',  ( 0.3543493200069162685, -0.000000000000000000, -0.9351131265310288487 ) ) ;
#67722 = CIRCLE ( 'NONE', #139539, 2.055000000000001048 ) ;
#67723 = ORIENTED_EDGE ( 'NONE', *, *, #74287, .T. ) ;
#67724 = DIRECTION ( 'NONE',  ( -0.000000000000000000, 0.3543493200069153248, 0.9351131265310292928 ) ) ;
#67725 = VECTOR ( 'NONE', #91326, 1000.000000000000000 ) ;
#67726 = CARTESIAN_POINT ( 'NONE',  ( 122.3333333333333286, -6.884901960086287964, 3.974999999999998312 ) ) ;
#67727 = FACE_OUTER_BOUND ( 'NONE', #120841, .T. ) ;
#67728 = SURFACE_STYLE_USAGE ( .BOTH. , #35088 ) ;
#67729 = DIRECTION ( 'NONE',  ( 0.7071067811865487940, 0.7071067811865463515, 0.000000000000000000 ) ) ;
#67730 = CARTESIAN_POINT ( 'NONE',  ( 15.18398860626900237, 28.73617430169797871, 5.000000000000000000 ) ) ;
#67731 = DIRECTION ( 'NONE',  ( 0.000000000000000000, 0.000000000000000000, 1.000000000000000000 ) ) ;
#67732 = ORIENTED_EDGE ( 'NONE', *, *, #82503, .F. ) ;
#67733 = VECTOR ( 'NONE', #5831, 1000.000000000000000 ) ;
#67734 = TOROIDAL_SURFACE ( 'NONE', #104738, 3.000000000000000000, 3.000000000000000000 ) ;
#67735 = ORIENTED_EDGE ( 'NONE', *, *, #131677, .T. ) ;
#67736 = FACE_OUTER_BOUND ( 'NONE', #13468, .T. ) ;
#67737 = ORIENTED_EDGE ( 'NONE', *, *, #113563, .T. ) ;
#67738 = ORIENTED_EDGE ( 'NONE', *, *, #46056, .F. ) ;
#67739 = VERTEX_POINT ( 'NONE', #83346 ) ;
#67740 = DIRECTION ( 'NONE',  ( -1.000000000000000000, -1.224606353822377258E-16, -0.000000000000000000 ) ) ;
#67741 = EDGE_CURVE ( 'NONE', #129269, #115465, #110957, .T. ) ;
#67742 = CARTESIAN_POINT ( 'NONE',  ( 28.29209685856476497, -5.291415217122921177, 3.054999999999999272 ) ) ;
#67743 = VECTOR ( 'NONE', #140699, 1000.000000000000000 ) ;
#67744 = ORIENTED_EDGE ( 'NONE', *, *, #36552, .F. ) ;
#67745 = DIRECTION ( 'NONE',  ( -0.000000000000000000, 0.3543493200069153248, 0.9351131265310292928 ) ) ;
#67747 = EDGE_CURVE ( 'NONE', #141224, #7871, #50715, .T. ) ;
#67746 = DIRECTION ( 'NONE',  ( -0.000000000000000000, -0.3543493200069152693, 0.9351131265310292928 ) ) ;
#67748 = ADVANCED_FACE ( 'NONE', ( #94902 ), #28960, .F. ) ;
#67749 = CARTESIAN_POINT ( 'NONE',  ( 1.087903141435219379, 6.871911579029515771, 3.967499999999989146 ) ) ;
#67750 = DIRECTION ( 'NONE',  ( -0.000000000000000000, 0.3543493200069153248, 0.9351131265310292928 ) ) ;
#67751 = EDGE_CURVE ( 'NONE', #15312, #30859, #117363, .T. ) ;
#67752 = EDGE_LOOP ( 'NONE', ( #132499, #64802, #116292 ) ) ;
#67753 = DIRECTION ( 'NONE',  ( -0.7071067811865487940, 0.7071067811865463515, 0.000000000000000000 ) ) ;
#67754 = EDGE_CURVE ( 'NONE', #75784, #55041, #38411, .T. ) ;
#67755 = PLANE ( 'NONE',  #99808 ) ;
#67756 = DIRECTION ( 'NONE',  ( 0.7071067811865487940, 0.7071067811865463515, 0.000000000000000000 ) ) ;
#67757 = VECTOR ( 'NONE', #34969, 1000.000000000000227 ) ;
#67758 = AXIS2_PLACEMENT_3D ( 'NONE', #87351, #22754, #131567 ) ;
#67760 = ORIENTED_EDGE ( 'NONE', *, *, #76056, .F. ) ;
#67759 = PLANE ( 'NONE',  #31027 ) ;
#67761 = ORIENTED_EDGE ( 'NONE', *, *, #125732, .F. ) ;
#67762 = EDGE_CURVE ( 'NONE', #21857, #52815, #81610, .T. ) ;
#67763 = SURFACE_STYLE_USAGE ( .BOTH. , #12612 ) ;
#67764 = CARTESIAN_POINT ( 'NONE',  ( -56.99451991528749062, 28.92564299267978001, 4.000000000000000000 ) ) ;
#67765 = VECTOR ( 'NONE', #56176, 1000.000000000000000 ) ;
#67766 = DIRECTION ( 'NONE',  ( 0.000000000000000000, 0.000000000000000000, 1.000000000000000000 ) ) ;
#67768 = ORIENTED_EDGE ( 'NONE', *, *, #86436, .T. ) ;
#67767 = PRESENTATION_LAYER_ASSIGNMENT (  '', '', ( #137180 ) ) ;
#67769 = CARTESIAN_POINT ( 'NONE',  ( -26.99999999999980460, -10.06887692260771772, 4.000000000000000000 ) ) ;
#67770 = DIRECTION ( 'NONE',  ( -0.000000000000000000, -0.3543493200069152693, 0.9351131265310292928 ) ) ;
#67771 = EDGE_CURVE ( 'NONE', #114208, #7168, #16637, .T. ) ;
#67772 = VERTEX_POINT ( 'NONE', #70370 ) ;
#67773 = EDGE_CURVE ( 'NONE', #60350, #117136, #105082, .T. ) ;
#67774 = LINE ( 'NONE', #11896, #135195 ) ;
#67775 = DIRECTION ( 'NONE',  ( 0.7071067811865486830, -0.7071067811865464625, -0.000000000000000000 ) ) ;
#67776 = FACE_OUTER_BOUND ( 'NONE', #95359, .T. ) ;
#67777 = CONICAL_SURFACE ( 'NONE', #65380, 2.500000000000000888, 0.9599310885968822538 ) ;
#67778 = AXIS2_PLACEMENT_3D ( 'NONE', #80811, #81540, #16207 ) ;
#67779 =( GEOMETRIC_REPRESENTATION_CONTEXT ( 3 ) GLOBAL_UNCERTAINTY_ASSIGNED_CONTEXT ( ( #19947 ) ) GLOBAL_UNIT_ASSIGNED_CONTEXT ( ( #57177, #136118, #1304 ) ) REPRESENTATION_CONTEXT ( 'NONE', 'WORKASPACE' ) );
#67780 = CARTESIAN_POINT ( 'NONE',  ( 33.70710678118631165, 11.25929247661560062, 5.000000000000000000 ) ) ;
#67781 = DIRECTION ( 'NONE',  ( 0.6830127018922180770, -0.6830127018922204085, -0.2588190451025213501 ) ) ;
#67782 = ADVANCED_FACE ( 'NONE', ( #92773 ), #137009, .F. ) ;
#67783 = LINE ( 'NONE', #13324, #54038 ) ;
#67784 = DIRECTION ( 'NONE',  ( -4.681814790819591790E-17, -0.3543493200069152693, 0.9351131265310292928 ) ) ;
#67785 = EDGE_CURVE ( 'NONE', #46733, #1294, #142022, .T. ) ;
#67786 = ORIENTED_EDGE ( 'NONE', *, *, #27193, .F. ) ;
#67787 = EDGE_LOOP ( 'NONE', ( #9269, #67095, #58852 ) ) ;
#67788 = DIRECTION ( 'NONE',  ( 0.000000000000000000, 5.559056632600921604E-15, -1.000000000000000000 ) ) ;
#67789 = CARTESIAN_POINT ( 'NONE',  ( 21.29974487139158512, -27.71228299555221142, 4.000000000000000000 ) ) ;
#67790 = EDGE_CURVE ( 'NONE', #6272, #2363, #65903, .T. ) ;
#67791 = CARTESIAN_POINT ( 'NONE',  ( 64.97502705046288440, -5.819803920172573086, 5.819803920172573086 ) ) ;
#67792 = ORIENTED_EDGE ( 'NONE', *, *, #100153, .T. ) ;
#67793 = AXIS2_PLACEMENT_3D ( 'NONE', #68306, #55986, #100185 ) ;
#67794 = DIRECTION ( 'NONE',  ( -0.7071067811865486830, -0.7071067811865464625, 0.000000000000000000 ) ) ;
#67795 = DIRECTION ( 'NONE',  ( -1.000000000000000000, 0.000000000000000000, 0.000000000000000000 ) ) ;
#67796 = DIRECTION ( 'NONE',  ( 0.3543493200069162685, -0.000000000000000000, -0.9351131265310288487 ) ) ;
#67797 = ORIENTED_EDGE ( 'NONE', *, *, #127986, .T. ) ;
#67798 = DIRECTION ( 'NONE',  ( -0.000000000000000000, -0.3543493200069152693, 0.9351131265310292928 ) ) ;
#67799 = CARTESIAN_POINT ( 'NONE',  ( 3.792893218813427669, 9.759292476615620160, 5.000000000000000000 ) ) ;
#67800 = SURFACE_SIDE_STYLE ('',( #26402 ) ) ;
#67801 = CARTESIAN_POINT ( 'NONE',  ( 56.78709685856478728, 3.054999999999997939, 5.291415217122920289 ) ) ;
#67802 = VECTOR ( 'NONE', #127982, 1000.000000000000227 ) ;
#67803 = DIRECTION ( 'NONE',  ( -0.7071067811865486830, 0.7071067811865464625, 0.000000000000000000 ) ) ;
#67804 = SURFACE_SIDE_STYLE ('',( #45332 ) ) ;
#67805 = CARTESIAN_POINT ( 'NONE',  ( 84.99999999999998579, 0.000000000000000000, -7.950000000000000178 ) ) ;
#67806 = VECTOR ( 'NONE', #45465, 999.9999999999998863 ) ;
#67807 = VERTEX_POINT ( 'NONE', #98489 ) ;
#67808 = CARTESIAN_POINT ( 'NONE',  ( -5.229957205422024913, 21.73644205237998150, 5.000000000000000888 ) ) ;
#67809 = EDGE_CURVE ( 'NONE', #133121, #66646, #63747, .T. ) ;
#67810 = EDGE_LOOP ( 'NONE', ( #142039, #6351, #6416, #40429 ) ) ;
#67811 = VECTOR ( 'NONE', #54977, 1000.000000000000000 ) ;
#67812 = DIRECTION ( 'NONE',  ( -1.000000000000000000, -1.224606353822377258E-16, -0.000000000000000000 ) ) ;
#67813 = TOROIDAL_SURFACE ( 'NONE', #86304, 5.000000000000000000, 1.000000000000000000 ) ;
#67814 = CARTESIAN_POINT ( 'NONE',  ( 3.489213562373097322, -27.52281430457057709, 5.000000000000000000 ) ) ;
#67815 = CARTESIAN_POINT ( 'NONE',  ( 9.489213562373095101, -27.52281430457062328, 5.000000000000000000 ) ) ;
#67816 = CARTESIAN_POINT ( 'NONE',  ( 19.58200623001875940, 2.499999999999998224, 3.061616997868380183E-16 ) ) ;
#67817 = LINE ( 'NONE', #11204, #121741 ) ;
#67818 = ORIENTED_EDGE ( 'NONE', *, *, #52351, .T. ) ;
#67819 = ORIENTED_EDGE ( 'NONE', *, *, #96211, .F. ) ;
#67820 = CARTESIAN_POINT ( 'NONE',  ( -9.793339364578404371, 21.75929247661549581, 4.998822639870701856 ) ) ;
#67821 = DIRECTION ( 'NONE',  ( -1.000000000000000000, -1.224606353822377258E-16, -0.000000000000000000 ) ) ;
#67822 = UNCERTAINTY_MEASURE_WITH_UNIT (LENGTH_MEASURE( 1.000000000000000082E-05 ), #14391, 'distance_accuracy_value', 'NONE');
#67823 = LINE ( 'NONE', #112013, #91369 ) ;
#67824 = EDGE_CURVE ( 'NONE', #142842, #24092, #55009, .T. ) ;
#67825 = LINE ( 'NONE', #75815, #22581 ) ;
#67826 = CARTESIAN_POINT ( 'NONE',  ( 72.26669371712955581, -7.949999999999999289, 2.130196079827424427 ) ) ;
#67827 = CARTESIAN_POINT ( 'NONE',  ( -34.82816939922328459, -20.24070752338408141, 4.000000000000000000 ) ) ;
#67828 = CARTESIAN_POINT ( 'NONE',  ( 13.60986171580761805, 4.202752102959690472E-16, 0.000000000000000000 ) ) ;
#67829 = ORIENTED_EDGE ( 'NONE', *, *, #17321, .T. ) ;
#67830 = CARTESIAN_POINT ( 'NONE',  ( 75.08333333333332860, 6.884901960086290629, -3.974999999999994316 ) ) ;
#67831 = CARTESIAN_POINT ( 'NONE',  ( 4.495848767239241539, -2.500000000000000000, 3.061616997868383634E-16 ) ) ;
#67832 = EDGE_CURVE ( 'NONE', #102967, #63922, #129680, .T. ) ;
#67833 = DIRECTION ( 'NONE',  ( -0.7071067811865486830, -0.7071067811865464625, 0.000000000000000000 ) ) ;
#67835 = VECTOR ( 'NONE', #114202, 999.9999999999998863 ) ;
#67834 = DIRECTION ( 'NONE',  ( -0.6830127018922180770, -0.6830127018922204085, -0.2588190451025213501 ) ) ;
#67836 = AXIS2_PLACEMENT_3D ( 'NONE', #122877, #87411, #109860 ) ;
#67837 = ORIENTED_EDGE ( 'NONE', *, *, #65365, .F. ) ;
#67838 =( BOUNDED_CURVE ( )  B_SPLINE_CURVE ( 3, ( #28049, #116479, #92559, #83144 ),
 .UNSPECIFIED., .F., .F. ) 
 B_SPLINE_CURVE_WITH_KNOTS ( ( 4, 4 ),
 ( 2.779374508378133601, 4.199602562396839822 ),
 .UNSPECIFIED. ) 
 CURVE ( )  GEOMETRIC_REPRESENTATION_ITEM ( )  RATIONAL_B_SPLINE_CURVE ( ( 1.000000000000000000, 0.8388583629366622718, 0.8388583629366622718, 1.000000000000000000 ) ) 
 REPRESENTATION_ITEM ( '' )  );
#67839 = DIRECTION ( 'NONE',  ( -0.6830127018922181881, 0.6830127018922202975, -0.2588190451025214056 ) ) ;
#67840 = EDGE_CURVE ( 'NONE', #88862, #142768, #21653, .T. ) ;
#67841 = CARTESIAN_POINT ( 'NONE',  ( 18.95159235450331892, 3.061616997868380183E-16, -2.500000000000001332 ) ) ;
#67842 = CARTESIAN_POINT ( 'NONE',  ( 61.83376352523143993, 6.110000000000001208, 1.122388791418549305E-15 ) ) ;
#67843 = ORIENTED_EDGE ( 'NONE', *, *, #123034, .T. ) ;
#67844 = ORIENTED_EDGE ( 'NONE', *, *, #30200, .F. ) ;
#67845 = VECTOR ( 'NONE', #30196, 1000.000000000000227 ) ;
#67846 =( BOUNDED_CURVE ( )  B_SPLINE_CURVE ( 3, ( #99834, #13512, #498, #22244 ),
 .UNSPECIFIED., .F., .T. ) 
 B_SPLINE_CURVE_WITH_KNOTS ( ( 4, 4 ),
 ( 0.06988172079111462653, 0.1872541115065305961 ),
 .UNSPECIFIED. ) 
 CURVE ( )  GEOMETRIC_REPRESENTATION_ITEM ( )  RATIONAL_B_SPLINE_CURVE ( ( 1.000000000000000000, 0.9988523062762910687, 0.9988523062762910687, 1.000000000000000000 ) ) 
 REPRESENTATION_ITEM ( '' )  );
#67847 = CARTESIAN_POINT ( 'NONE',  ( -12.00548008471251293, 28.92564299267929684, 4.000000000000000000 ) ) ;
#67848 = CARTESIAN_POINT ( 'NONE',  ( 11.15159235450332176, 9.902892378096218942E-16, 0.000000000000000000 ) ) ;
#67849 = LINE ( 'NONE', #103269, #64883 ) ;
#67850 = ADVANCED_FACE ( 'NONE', ( #29648 ), #131127, .F. ) ;
#67851 = CARTESIAN_POINT ( 'NONE',  ( -44.99451991528749772, 28.92564299267969474, 4.000000000000000000 ) ) ;
#67853 = ORIENTED_EDGE ( 'NONE', *, *, #94999, .T. ) ;
#67852 = CARTESIAN_POINT ( 'NONE',  ( -32.99451991528749062, 28.92564299267960948, 4.000000000000000000 ) ) ;
#67854 = CARTESIAN_POINT ( 'NONE',  ( 4.969723521325230209, 2.055000000000001048, 2.516649172247811554E-16 ) ) ;
#67855 = DIRECTION ( 'NONE',  ( -0.7071067811865486830, -0.7071067811865464625, -0.000000000000000000 ) ) ;
#67856 = VECTOR ( 'NONE', #26781, 1000.000000000000000 ) ;
#67857 = CARTESIAN_POINT ( 'NONE',  ( -48.18398860626899705, 28.73617430169820608, 5.000000000000000000 ) ) ;
#67858 = PLANE ( 'NONE',  #131806 ) ;
#67859 = VERTEX_POINT ( 'NONE', #131846 ) ;
#67860 = VERTEX_POINT ( 'NONE', #65179 ) ;
#67861 = CARTESIAN_POINT ( 'NONE',  ( 52.64626352523142572, -4.472830434245840259, 4.472830434245839371 ) ) ;
#67862 = ORIENTED_EDGE ( 'NONE', *, *, #52631, .F. ) ;
#67863 = CARTESIAN_POINT ( 'NONE',  ( 13.18000000000000149, 9.521314400968980422E-16, 0.000000000000000000 ) ) ;
#67864 = CARTESIAN_POINT ( 'NONE',  ( 9.524999999999991473, -4.870000000000013429, -10.00000000000000178 ) ) ;
#67865 = CARTESIAN_POINT ( 'NONE',  ( 15.83159235450332147, -3.851859888774471706E-31, 2.500000000000001332 ) ) ;
#67866 = DIRECTION ( 'NONE',  ( -0.000000000000000000, 0.000000000000000000, 1.000000000000000000 ) ) ;
#67867 = CARTESIAN_POINT ( 'NONE',  ( 54.81249999999999289, 5.819803920172571310, 5.819803920172576639 ) ) ;
#67868 = ORIENTED_EDGE ( 'NONE', *, *, #137477, .F. ) ;
#67869 = ORIENTED_EDGE ( 'NONE', *, *, #118277, .F. ) ;
#67870 = VECTOR ( 'NONE', #46579, 1000.000000000000000 ) ;
#67871 = CARTESIAN_POINT ( 'NONE',  ( -28.49999999999979039, 1.087461875839230707, 4.000000000000000000 ) ) ;
#67872 = VECTOR ( 'NONE', #112486, 999.9999999999998863 ) ;
#67873 = VECTOR ( 'NONE', #4500, 1000.000000000000000 ) ;
#67874 = EDGE_LOOP ( 'NONE', ( #35786, #55615, #112917, #60912 ) ) ;
#67875 = EDGE_CURVE ( 'NONE', #36751, #26060, #142714, .T. ) ;
#67876 =( LENGTH_UNIT ( ) NAMED_UNIT ( * ) SI_UNIT ( .MILLI., .METRE. ) );
#67878 = CARTESIAN_POINT ( 'NONE',  ( 112.9541937171295558, 6.884901960086283523, 3.975000000000002753 ) ) ;
#67877 = VECTOR ( 'NONE', #5274, 1000.000000000000000 ) ;
#67879 = LINE ( 'NONE', #123671, #58750 ) ;
#67880 = AXIS2_PLACEMENT_3D ( 'NONE', #127711, #51582, #5879 ) ;
#67881 = AXIS2_PLACEMENT_3D ( 'NONE', #80878, #78024, #36631 ) ;
#67882 = VERTEX_POINT ( 'NONE', #97020 ) ;
#67883 = FACE_BOUND ( 'NONE', #45942, .T. ) ;
#67884 = ADVANCED_FACE ( 'NONE', ( #53573 ), #75332, .T. ) ;
#67885 = CARTESIAN_POINT ( 'NONE',  ( 26.99999999999982236, 20.58746187583902909, 4.000000000000000000 ) ) ;
#67886 = LINE ( 'NONE', #112070, #81421 ) ;
#67887 = CYLINDRICAL_SURFACE ( 'NONE', #41339, 6.349999999999997868 ) ;
#67888 = AXIS2_PLACEMENT_3D ( 'NONE', #75470, #20336, #97929 ) ;
#67889 = DIRECTION ( 'NONE',  ( -0.7071067811865486830, -0.7071067811865464625, -0.000000000000000000 ) ) ;
#67890 = PRODUCT_RELATED_PRODUCT_CATEGORY ( 'part', '', ( #76820 ) ) ;
#67891 = LINE ( 'NONE', #67137, #120632 ) ;
#67892 = DIRECTION ( 'NONE',  ( 0.2885027572699951914, 5.495630694990785950E-32, -0.9574790645479464013 ) ) ;
#67893 = VERTEX_POINT ( 'NONE', #31812 ) ;
#67894 = AXIS2_PLACEMENT_3D ( 'NONE', #109650, #110341, #90029 ) ;
#67895 = ORIENTED_EDGE ( 'NONE', *, *, #6266, .F. ) ;
#67896 = CARTESIAN_POINT ( 'NONE',  ( 107.2454301918981088, -5.291415217122918513, -3.055000000000000160 ) ) ;
#67897 = VERTEX_POINT ( 'NONE', #141271 ) ;
#67898 = PLANE ( 'NONE',  #55886 ) ;
#67899 = ORIENTED_EDGE ( 'NONE', *, *, #143015, .T. ) ;
#67900 = DIRECTION ( 'NONE',  ( -0.000000000000000000, 0.000000000000000000, 1.000000000000000000 ) ) ;
#67901 = EDGE_CURVE ( 'NONE', #92475, #94800, #76030, .T. ) ;
#67902 = VECTOR ( 'NONE', #133330, 1000.000000000000000 ) ;
#67903 = FACE_OUTER_BOUND ( 'NONE', #70241, .T. ) ;
#67904 = DIRECTION ( 'NONE',  ( -0.7071067811865486830, -0.7071067811865464625, 0.000000000000000000 ) ) ;
#67905 = ORIENTED_EDGE ( 'NONE', *, *, #34700, .T. ) ;
#67906 = FACE_OUTER_BOUND ( 'NONE', #14032, .T. ) ;
#67907 = LINE ( 'NONE', #99764, #107439 ) ;
#67908 = SURFACE_STYLE_USAGE ( .BOTH. , #135967 ) ;
#67909 = CONICAL_SURFACE ( 'NONE', #104903, 2.500000000000000444, 0.9599310885968830309 ) ;
#67910 = DIRECTION ( 'NONE',  ( 0.7071067811865487940, 0.7071067811865463515, 0.000000000000000000 ) ) ;
#67912 = DIRECTION ( 'NONE',  ( 1.000000000000000000, 0.000000000000000000, -0.000000000000000000 ) ) ;
#67911 = LINE ( 'NONE', #136673, #140622 ) ;
#67913 = DIRECTION ( 'NONE',  ( -0.7071067811865486830, 0.7071067811865464625, 0.000000000000000000 ) ) ;
#67914 = DIRECTION ( 'NONE',  ( 0.6830127018922181881, 0.6830127018922202975, -0.2588190451025214056 ) ) ;
#67915 = ORIENTED_EDGE ( 'NONE', *, *, #97716, .F. ) ;
#67916 = CARTESIAN_POINT ( 'NONE',  ( -19.05000000000000071, 3.174999999999997158, 4.000000000000000000 ) ) ;
#67917 = PLANE ( 'NONE',  #9425 ) ;
#67918 = EDGE_LOOP ( 'NONE', ( #67818, #11816, #76088, #125619 ) ) ;
#67919 = ORIENTED_EDGE ( 'NONE', *, *, #8312, .T. ) ;
#67920 = VERTEX_POINT ( 'NONE', #118810 ) ;
#67921 = CARTESIAN_POINT ( 'NONE',  ( 59.06293019189810423, 1.637169565754157174, 6.110000000000002984 ) ) ;
#67922 = ORIENTED_EDGE ( 'NONE', *, *, #32912, .F. ) ;
#67923 = AXIS2_PLACEMENT_3D ( 'NONE', #123936, #133384, #23902 ) ;
#67924 = CARTESIAN_POINT ( 'NONE',  ( 20.24139925780189841, 21.72500000000000853, 5.000000000000000000 ) ) ;
#67925 = EDGE_CURVE ( 'NONE', #32412, #122448, #119498, .T. ) ;
#67926 = VECTOR ( 'NONE', #54046, 1000.000000000000227 ) ;
#67927 = CARTESIAN_POINT ( 'NONE',  ( 7.045806282870439752, 5.278424836066143655, -3.047499999999997655 ) ) ;
#67928 = CARTESIAN_POINT ( 'NONE',  ( 94.35459685856476142, -1.637169565754161615, 6.110000000000000320 ) ) ;
#67929 = DIRECTION ( 'NONE',  ( -0.000000000000000000, -0.3543493200069152693, 0.9351131265310292928 ) ) ;
#67930 = VERTEX_POINT ( 'NONE', #40561 ) ;
#67931 = EDGE_CURVE ( 'NONE', #20411, #96207, #96311, .T. ) ;
#67933 = ORIENTED_EDGE ( 'NONE', *, *, #32566, .T. ) ;
#67932 = EDGE_CURVE ( 'NONE', #56401, #139347, #85455, .T. ) ;
#67934 = CARTESIAN_POINT ( 'NONE',  ( -9.489213562373095101, -27.52281430457062328, 5.000000000000000000 ) ) ;
#67935 = AXIS2_PLACEMENT_3D ( 'NONE', #7502, #130017, #51761 ) ;
#67936 = CARTESIAN_POINT ( 'NONE',  ( 34.49999999999976552, 3.054329344830917670, 4.994342998332163219 ) ) ;
#67937 = ORIENTED_EDGE ( 'NONE', *, *, #89196, .F. ) ;
#67938 = EDGE_CURVE ( 'NONE', #91617, #70701, #86914, .T. ) ;
#67939 = CARTESIAN_POINT ( 'NONE',  ( -24.48921356237309510, -27.52281430457072631, 5.000000000000000000 ) ) ;
#67940 = CARTESIAN_POINT ( 'NONE',  ( -16.49999999999987921, 16.08746187583907528, 4.000000000000000000 ) ) ;
#67941 = DIRECTION ( 'NONE',  ( -0.7071067811865486830, 0.7071067811865464625, 0.000000000000000000 ) ) ;
#67942 = EDGE_LOOP ( 'NONE', ( #10141, #133955, #76728, #30826 ) ) ;
#67943 = DIRECTION ( 'NONE',  ( 0.3543493200069162685, -0.000000000000000000, -0.9351131265310288487 ) ) ;
#67944 = EDGE_LOOP ( 'NONE', ( #36584, #24745, #55272, #122050 ) ) ;
#67945 = VERTEX_POINT ( 'NONE', #19499 ) ;
#67946 = EDGE_LOOP ( 'NONE', ( #77605, #107204, #121285, #143419 ) ) ;
#67947 = CARTESIAN_POINT ( 'NONE',  ( 15.00548008471250228, 28.92564299267927552, 4.000000000000000000 ) ) ;
#67948 = AXIS2_PLACEMENT_3D ( 'NONE', #70722, #39507, #114868 ) ;
#67949 = LINE ( 'NONE', #99067, #100157 ) ;
#67950 = ADVANCED_FACE ( 'NONE', ( #73892 ), #32533, .F. ) ;
#67951 = DIRECTION ( 'NONE',  ( -0.3543493200069162685, -0.000000000000000000, -0.9351131265310288487 ) ) ;
#67952 = CARTESIAN_POINT ( 'NONE',  ( 60.48921356237309510, -27.52281430457097500, 5.000000000000000000 ) ) ;
#67953 = EDGE_CURVE ( 'NONE', #99104, #113229, #76775, .T. ) ;
#67954 = CARTESIAN_POINT ( 'NONE',  ( -34.49999999999975131, -7.420205493532929353, -2.617629953481332539 ) ) ;
#67955 = COLOUR_RGB ( '', 0.08235294, 0.09019608, 0.10196078) ;
#67956 = ORIENTED_EDGE ( 'NONE', *, *, #79764, .F. ) ;
#67957 = EDGE_CURVE ( 'NONE', #117376, #3502, #63046, .T. ) ;
#67958 = CARTESIAN_POINT ( 'NONE',  ( 11.49956980810188689, -3.967499999999998028, -6.871911579029511330 ) ) ;
#67959 = DIRECTION ( 'NONE',  ( -0.7071067811865487940, 0.7071067811865463515, -0.000000000000000000 ) ) ;
#67960 = CARTESIAN_POINT ( 'NONE',  ( 33.18398860626899705, 28.73617430169810305, 5.000000000000000000 ) ) ;
#67961 = ORIENTED_EDGE ( 'NONE', *, *, #97458, .T. ) ;
#67962 = ORIENTED_EDGE ( 'NONE', *, *, #35240, .F. ) ;
#67963 = ORIENTED_EDGE ( 'NONE', *, *, #119198, .T. ) ;
#67964 = PLANE ( 'NONE',  #120466 ) ;
#67965 = UNCERTAINTY_MEASURE_WITH_UNIT (LENGTH_MEASURE( 1.000000000000000082E-05 ), #30207, 'distance_accuracy_value', 'NONE');
#67966 = EDGE_CURVE ( 'NONE', #120720, #138900, #68064, .T. ) ;
#67967 = VECTOR ( 'NONE', #17449, 1000.000000000000000 ) ;
#67968 = DIRECTION ( 'NONE',  ( -0.7071067811865486830, -0.7071067811865464625, 0.000000000000000000 ) ) ;
#67969 = CARTESIAN_POINT ( 'NONE',  ( -2.510786437626908008, -27.52281430457053446, 5.000000000000000000 ) ) ;
#67970 = LINE ( 'NONE', #25839, #107975 ) ;
#67971 = VECTOR ( 'NONE', #108131, 1000.000000000000000 ) ;
#67972 = CARTESIAN_POINT ( 'NONE',  ( -14.99999999999989519, 4.384688058510551656, -7.090945410444718711 ) ) ;
#67973 = LINE ( 'NONE', #112159, #13210 ) ;
#67974 = LINE ( 'NONE', #112161, #53332 ) ;
#67975 = DIRECTION ( 'NONE',  ( 0.6830127018922180770, -0.6830127018922204085, -0.2588190451025213501 ) ) ;
#67976 = ORIENTED_EDGE ( 'NONE', *, *, #107516, .T. ) ;
#67977 = DIRECTION ( 'NONE',  ( 0.000000000000000000, 0.000000000000000000, -1.000000000000000000 ) ) ;
#67978 = ADVANCED_FACE ( 'NONE', ( #121652 ), #55721, .F. ) ;
#67979 = VECTOR ( 'NONE', #82199, 1000.000000000000000 ) ;
#67980 = AXIS2_PLACEMENT_3D ( 'NONE', #6202, #82398, #49060 ) ;
#67981 = ORIENTED_EDGE ( 'NONE', *, *, #93868, .T. ) ;
#67982 = SURFACE_STYLE_USAGE ( .BOTH. , #78107 ) ;
#67983 = ORIENTED_EDGE ( 'NONE', *, *, #83873, .T. ) ;
#67984 = CARTESIAN_POINT ( 'NONE',  ( -34.42500000000001137, 21.72500000000000142, 0.000000000000000000 ) ) ;
#67986 = ORIENTED_EDGE ( 'NONE', *, *, #76217, .F. ) ;
#67985 = CARTESIAN_POINT ( 'NONE',  ( 11.99999999999991651, -11.35517001088071076, -1.126524801160080358 ) ) ;
#67987 = DIRECTION ( 'NONE',  ( 0.7071067811865486830, -0.7071067811865464625, -0.000000000000000000 ) ) ;
#67988 = CARTESIAN_POINT ( 'NONE',  ( 9.183988606268997046, 28.73617430169793607, 5.000000000000000000 ) ) ;
#67989 = APPLICATION_CONTEXT ( 'automotive_design' ) ;
#67990 = ORIENTED_EDGE ( 'NONE', *, *, #68126, .F. ) ;
#67991 = DIRECTION ( 'NONE',  ( -0.6830127018922180770, -0.6830127018922204085, -0.2588190451025213501 ) ) ;
#67992 = EDGE_LOOP ( 'NONE', ( #35058, #133222, #77415, #120869 ) ) ;
#67993 = CARTESIAN_POINT ( 'NONE',  ( -4.499999999999972466, 3.653845994658382779, -4.504631822206361491 ) ) ;
#67994 = VERTEX_POINT ( 'NONE', #113641 ) ;
#67995 = AXIS2_PLACEMENT_3D ( 'NONE', #106692, #8778, #53037 ) ;
#67996 = PLANE ( 'NONE',  #47613 ) ;
#67997 = EDGE_CURVE ( 'NONE', #100863, #49400, #46295, .T. ) ;
#67998 = CARTESIAN_POINT ( 'NONE',  ( 101.7250270504628844, 5.819803920172573086, -5.819803920172572198 ) ) ;
#67999 = SURFACE_SIDE_STYLE ('',( #100589 ) ) ;
#68000 = VECTOR ( 'NONE', #113765, 1000.000000000000000 ) ;
#68001 = CARTESIAN_POINT ( 'NONE',  ( 39.29974487139159578, -27.71228299555233576, 4.000000000000000000 ) ) ;
#68002 = VERTEX_POINT ( 'NONE', #135432 ) ;
#68003 = LINE ( 'NONE', #131788, #16653 ) ;
#68004 = DIRECTION ( 'NONE',  ( -0.7071067811865486830, 0.7071067811865464625, 0.000000000000000000 ) ) ;
#68005 = CARTESIAN_POINT ( 'NONE',  ( 27.18398860626900060, 28.73617430169806042, 5.000000000000000000 ) ) ;
#68006 = CARTESIAN_POINT ( 'NONE',  ( 11.22916666666666430, -6.094999999999989093, 1.633150327867691765 ) ) ;
#68007 = CARTESIAN_POINT ( 'NONE',  ( 24.77040314143521726, -7.934999999999988951, 2.126176841940957907 ) ) ;
#68008 = DIRECTION ( 'NONE',  ( -0.000000000000000000, -0.3543493200069152693, 0.9351131265310292928 ) ) ;
#68009 = LINE ( 'NONE', #112193, #94142 ) ;
#68010 = ORIENTED_EDGE ( 'NONE', *, *, #39893, .F. ) ;
#68011 = AXIS2_PLACEMENT_3D ( 'NONE', #14759, #113339, #37229 ) ;
#68012 = ORIENTED_EDGE ( 'NONE', *, *, #19378, .T. ) ;
#68013 = CARTESIAN_POINT ( 'NONE',  ( -20.70025512860841133, -27.71228299555191654, 4.000000000000000000 ) ) ;
#68014 = ORIENTED_EDGE ( 'NONE', *, *, #13510, .T. ) ;
#68015 = AXIS2_PLACEMENT_3D ( 'NONE', #80064, #1701, #56887 ) ;
#68016 = EDGE_CURVE ( 'NONE', #36869, #126961, #69459, .T. ) ;
#68017 = CARTESIAN_POINT ( 'NONE',  ( 90.56293019189811844, 1.637169565754157174, 6.110000000000002984 ) ) ;
#68018 = CARTESIAN_POINT ( 'NONE',  ( -1.110173228882102459, -22.22500000000000497, 4.785647885939354751 ) ) ;
#68019 = CARTESIAN_POINT ( 'NONE',  ( 17.99451991528748351, 28.92564299267950645, 4.000000000000000000 ) ) ;
#68020 = CARTESIAN_POINT ( 'NONE',  ( -5.700255128608413102, -27.71228299555201957, 4.000000000000000000 ) ) ;
#68021 = CARTESIAN_POINT ( 'NONE',  ( 127.6280169629029331, -46.44627868284427308, -35.89947574910254957 ) ) ;
#68022 = EDGE_LOOP ( 'NONE', ( #28575, #106145, #128743, #53925 ) ) ;
#68023 = CARTESIAN_POINT ( 'NONE',  ( -34.92500000000001137, 12.66246187583886318, 4.000000000000000000 ) ) ;
#68024 = DIRECTION ( 'NONE',  ( 0.000000000000000000, -1.000000000000000000, 0.000000000000000000 ) ) ;
#68025 = VECTOR ( 'NONE', #38685, 1000.000000000000000 ) ;
#68026 = CARTESIAN_POINT ( 'NONE',  ( -34.42499999999997584, -21.76999999999999247, 0.000000000000000000 ) ) ;
#68027 = ORIENTED_EDGE ( 'NONE', *, *, #121811, .T. ) ;
#68028 = DIRECTION ( 'NONE',  ( -0.000000000000000000, 0.3543493200069153248, 0.9351131265310292928 ) ) ;
#68029 = ADVANCED_FACE ( 'NONE', ( #78184 ), #123125, .T. ) ;
#68030 = PLANE ( 'NONE',  #12403 ) ;
#68032 = ORIENTED_EDGE ( 'NONE', *, *, #98573, .T. ) ;
#68031 = CARTESIAN_POINT ( 'NONE',  ( -45.18398860626900415, 28.73617430169818832, 5.000000000000000000 ) ) ;
#68033 = DIRECTION ( 'NONE',  ( 0.7071067811865486830, -0.7071067811865464625, -0.000000000000000000 ) ) ;
#68034 = PLANE ( 'NONE',  #91015 ) ;
#68035 = LINE ( 'NONE', #91193, #101182 ) ;
#68036 =( BOUNDED_CURVE ( )  B_SPLINE_CURVE ( 2, ( #72712, #61801, #82140, #128473, #105276, #29146, #5226, #73389, #51631, #5927, #59664, #114706, #95822 ),
 .UNSPECIFIED., .F., .T. ) 
 B_SPLINE_CURVE_WITH_KNOTS ( ( 3, 2, 2, 2, 2, 2, 3 ),
 ( 0.6500000000000000222, 0.6527777777777777901, 0.6555555555555555580, 0.6583333333333333259, 0.6611111111111110938, 0.6638888888888888618, 0.6666666666666666297 ),
 .UNSPECIFIED. ) 
 CURVE ( )  GEOMETRIC_REPRESENTATION_ITEM ( )  RATIONAL_B_SPLINE_CURVE ( ( 1.000000000000000000, 0.9659258262890683122, 1.000000000000000000, 0.9659258262890683122, 1.000000000000000000, 0.9659258262890683122, 1.000000000000000000, 0.9659258262890683122, 1.000000000000000000, 0.9659258262890683122, 1.000000000000000000, 0.9659258262890683122, 1.000000000000000000 ) ) 
 REPRESENTATION_ITEM ( '' )  );
#68037 = DIRECTION ( 'NONE',  ( -0.7071067811865486830, -0.7071067811865464625, 0.000000000000000000 ) ) ;
#68038 = VECTOR ( 'NONE', #85144, 1000.000000000000000 ) ;
#68039 = ORIENTED_EDGE ( 'NONE', *, *, #19686, .F. ) ;
#68040 = ORIENTED_EDGE ( 'NONE', *, *, #20473, .F. ) ;
#68041 = ORIENTED_EDGE ( 'NONE', *, *, #137161, .T. ) ;
#68042 = CARTESIAN_POINT ( 'NONE',  ( 85.31293019189811844, -1.637169565754159617, -6.110000000000001208 ) ) ;
#68043 = ORIENTED_EDGE ( 'NONE', *, *, #10444, .F. ) ;
#68044 = CARTESIAN_POINT ( 'NONE',  ( 27.29974487139158512, -27.71228299555225405, 4.000000000000000000 ) ) ;
#68045 = EDGE_CURVE ( 'NONE', #58958, #38790, #1295, .T. ) ;
#68046 = CARTESIAN_POINT ( 'NONE',  ( 39.18398860626899705, 28.73617430169814568, 5.000000000000000000 ) ) ;
#68047 = VECTOR ( 'NONE', #113608, 1000.000000000000000 ) ;
#68048 = DIRECTION ( 'NONE',  ( 0.7071067811865487940, -0.7071067811865463515, 0.000000000000000000 ) ) ;
#68049 = CARTESIAN_POINT ( 'NONE',  ( 10.49999999999992539, -14.70932175296476352, -11.46312253303839768 ) ) ;
#68050 = ORIENTED_EDGE ( 'NONE', *, *, #98039, .F. ) ;
#68051 = DIRECTION ( 'NONE',  ( -0.7071067811865486830, -0.7071067811865464625, 0.000000000000000000 ) ) ;
#68052 = CARTESIAN_POINT ( 'NONE',  ( 34.92499999999998295, 16.32446447596926831, 2.764066516344042324 ) ) ;
#68053 = CARTESIAN_POINT ( 'NONE',  ( 10.82816939922345512, 12.75929247661558641, 4.000000000000000000 ) ) ;
#68054 = CARTESIAN_POINT ( 'NONE',  ( 84.05793019189810877, 6.110000000000000320, -1.637169565754156064 ) ) ;
#68055 = ORIENTED_EDGE ( 'NONE', *, *, #86285, .T. ) ;
#68056 = EDGE_CURVE ( 'NONE', #111777, #122541, #35421, .T. ) ;
#68057 = EDGE_CURVE ( 'NONE', #25059, #45436, #56471, .T. ) ;
#68058 = DIRECTION ( 'NONE',  ( 0.7071067811865486830, -0.7071067811865464625, -0.000000000000000000 ) ) ;
#68059 = VECTOR ( 'NONE', #16335, 1000.000000000000000 ) ;
#68060 = LINE ( 'NONE', #115036, #30773 ) ;
#68061 = ORIENTED_EDGE ( 'NONE', *, *, #61517, .F. ) ;
#68062 = ORIENTED_EDGE ( 'NONE', *, *, #88000, .T. ) ;
#68063 = EDGE_CURVE ( 'NONE', #51456, #131551, #89067, .T. ) ;
#68064 = LINE ( 'NONE', #33968, #83901 ) ;
#68065 = ADVANCED_FACE ( 'NONE', ( #91222 ), #102064, .T. ) ;
#68066 = CARTESIAN_POINT ( 'NONE',  ( -19.49999999999986144, -7.912538124160673370, 4.000000000000000000 ) ) ;
#68067 = LINE ( 'NONE', #68752, #134493 ) ;
#68068 = LINE ( 'NONE', #4112, #122814 ) ;
#68069 = LINE ( 'NONE', #66600, #12600 ) ;
#68070 = VECTOR ( 'NONE', #9164, 1000.000000000000000 ) ;
#68071 = ORIENTED_EDGE ( 'NONE', *, *, #130304, .F. ) ;
#68072 = ORIENTED_EDGE ( 'NONE', *, *, #97878, .T. ) ;
#68073 = CARTESIAN_POINT ( 'NONE',  ( -3.183988606268992161, 28.73617430169789699, 5.000000000000000000 ) ) ;
#68074 = EDGE_LOOP ( 'NONE', ( #27, #7513, #82122, #124091, #54906 ) ) ;
#68075 = ORIENTED_EDGE ( 'NONE', *, *, #123252, .T. ) ;
#68076 = EDGE_CURVE ( 'NONE', #12889, #78582, #12187, .T. ) ;
#68077 = VECTOR ( 'NONE', #2046, 999.9999999999998863 ) ;
#68078 = DIRECTION ( 'NONE',  ( 0.6830127018922180770, -0.6830127018922204085, -0.2588190451025213501 ) ) ;
#68079 = VERTEX_POINT ( 'NONE', #90479 ) ;
#68080 = LINE ( 'NONE', #134747, #55227 ) ;
#68081 = LINE ( 'NONE', #123860, #109729 ) ;
#68082 = CARTESIAN_POINT ( 'NONE',  ( 12.71159235450332048, 9.902892378096218942E-16, 0.000000000000000000 ) ) ;
#68083 = FACE_OUTER_BOUND ( 'NONE', #142402, .T. ) ;
#68084 = ORIENTED_EDGE ( 'NONE', *, *, #83609, .T. ) ;
#68085 = CARTESIAN_POINT ( 'NONE',  ( -38.00492477221170873, -5.240707523384228850, 12.38332538355504653 ) ) ;
#68086 = ORIENTED_EDGE ( 'NONE', *, *, #87896, .F. ) ;
#68087 = CARTESIAN_POINT ( 'NONE',  ( 3.710381658649933634, 3.061616997868382648E-16, -2.500000000000000444 ) ) ;
#68088 = ORIENTED_EDGE ( 'NONE', *, *, #61401, .T. ) ;
#68089 = CARTESIAN_POINT ( 'NONE',  ( 115.7250270504628844, 5.819803920172573974, -5.819803920172573086 ) ) ;
#68090 = ORIENTED_EDGE ( 'NONE', *, *, #21404, .F. ) ;
#68091 = PLANE ( 'NONE',  #6434 ) ;
#68092 = VERTEX_POINT ( 'NONE', #66593 ) ;
#68093 = VERTEX_POINT ( 'NONE', #12892 ) ;
#68094 = AXIS2_PLACEMENT_3D ( 'NONE', #65032, #99041, #8436 ) ;
#68095 = ORIENTED_EDGE ( 'NONE', *, *, #1376, .T. ) ;
#68096 = DIRECTION ( 'NONE',  ( -0.3543493200069162685, -0.000000000000000000, -0.9351131265310288487 ) ) ;
#68097 = VECTOR ( 'NONE', #113233, 1000.000000000000000 ) ;
#68098 = ADVANCED_FACE ( 'NONE', ( #79659 ), #1983, .F. ) ;
#68099 = CARTESIAN_POINT ( 'NONE',  ( 26.20710678118635784, -11.24070752338417556, 5.000000000000000000 ) ) ;
#68100 = FACE_OUTER_BOUND ( 'NONE', #108789, .T. ) ;
#68101 = CARTESIAN_POINT ( 'NONE',  ( 116.0837635252314470, -6.110000000000001208, -3.741295971395164515E-16 ) ) ;
#68102 = CARTESIAN_POINT ( 'NONE',  ( 75.48921356237309510, -27.52281430457107803, 5.000000000000000000 ) ) ;
#68103 = ADVANCED_FACE ( 'NONE', ( #77485 ), #101344, .F. ) ;
#68104 = LINE ( 'NONE', #103509, #15791 ) ;
#68105 = CARTESIAN_POINT ( 'NONE',  ( -18.18398860626898994, 28.73617430169800002, 5.000000000000000000 ) ) ;
#68107 = CARTESIAN_POINT ( 'NONE',  ( -0.4892135623730947680, -27.52281430457055578, 5.000000000000000000 ) ) ;
#68106 = VECTOR ( 'NONE', #123383, 1000.000000000000227 ) ;
#68108 = ADVANCED_FACE ( 'NONE', ( #588 ), #44885, .T. ) ;
#68109 = ADVANCED_FACE ( 'NONE', ( #57880 ), #2738, .F. ) ;
#68110 = CARTESIAN_POINT ( 'NONE',  ( -34.42499999999997584, 0.000000000000000000, -0.5000000000000000000 ) ) ;
#68111 = ORIENTED_EDGE ( 'NONE', *, *, #24259, .F. ) ;
#68112 = CARTESIAN_POINT ( 'NONE',  ( 0.000000000000000000, 1.399999999999987699, -20.40202195861970580 ) ) ;
#68113 = VECTOR ( 'NONE', #29043, 1000.000000000000000 ) ;
#68114 = DIRECTION ( 'NONE',  ( 1.000000000000000000, 0.000000000000000000, 0.000000000000000000 ) ) ;
#68115 = VECTOR ( 'NONE', #124149, 999.9999999999998863 ) ;
#68116 = ORIENTED_EDGE ( 'NONE', *, *, #132488, .F. ) ;
#68117 = ORIENTED_EDGE ( 'NONE', *, *, #18276, .F. ) ;
#68118 = DIRECTION ( 'NONE',  ( 0.5735764363510453823, -0.8191520442889923537, 1.003171929053525486E-16 ) ) ;
#68119 = EDGE_LOOP ( 'NONE', ( #96293, #17408, #15834, #18628 ) ) ;
#68120 = VERTEX_POINT ( 'NONE', #70202 ) ;
#68121 = DIRECTION ( 'NONE',  ( -0.7071067811865487940, 0.7071067811865463515, -0.000000000000000000 ) ) ;
#68122 = FACE_OUTER_BOUND ( 'NONE', #121515, .T. ) ;
#68123 = EDGE_CURVE ( 'NONE', #26660, #53545, #104166, .T. ) ;
#68124 = VECTOR ( 'NONE', #108868, 1000.000000000000000 ) ;
#68125 = CARTESIAN_POINT ( 'NONE',  ( 10.49999999999992539, -8.568876922607726598, 4.000000000000000000 ) ) ;
#68126 = EDGE_CURVE ( 'NONE', #72906, #143427, #141485, .T. ) ;
#68127 = DIRECTION ( 'NONE',  ( 1.000000000000000000, 0.000000000000000000, 0.000000000000000000 ) ) ;
#68128 = ORIENTED_EDGE ( 'NONE', *, *, #135572, .T. ) ;
#68129 = DIRECTION ( 'NONE',  ( 0.6830127018922181881, 0.6830127018922202975, -0.2588190451025214056 ) ) ;
#68130 = ORIENTED_EDGE ( 'NONE', *, *, #19857, .T. ) ;
#68132 = AXIS2_PLACEMENT_3D ( 'NONE', #55765, #55050, #99216 ) ;
#68131 = DIRECTION ( 'NONE',  ( -0.7071067811865486830, -0.7071067811865464625, 0.000000000000000000 ) ) ;
#68133 = AXIS2_PLACEMENT_3D ( 'NONE', #17596, #6694, #71307 ) ;
#68134 = CARTESIAN_POINT ( 'NONE',  ( 18.87956980810189123, 3.967499999999998916, 6.871911579029510442 ) ) ;
#68135 = EDGE_LOOP ( 'NONE', ( #30214, #93436, #137566, #136839 ) ) ;
#68136 = CARTESIAN_POINT ( 'NONE',  ( 81.43293019189809456, 1.637169565754156730, 6.110000000000001208 ) ) ;
#68137 = ADVANCED_FACE ( 'NONE', ( #104912 ), #119174, .F. ) ;
#68138 = CARTESIAN_POINT ( 'NONE',  ( 21.18398860626899349, 28.73617430169802134, 5.000000000000000000 ) ) ;
#68139 = CARTESIAN_POINT ( 'NONE',  ( 99.53752705046289861, -9.735942053221456900E-16, 7.949999999999998401 ) ) ;
#68140 = VERTEX_POINT ( 'NONE', #93326 ) ;
#68141 = VERTEX_POINT ( 'NONE', #19158 ) ;
#68142 = ORIENTED_EDGE ( 'NONE', *, *, #59434, .F. ) ;
#68143 = LINE ( 'NONE', #21734, #93559 ) ;
#68144 = CARTESIAN_POINT ( 'NONE',  ( 36.29974487139159578, -27.71228299555231445, 4.000000000000000000 ) ) ;
#68145 = EDGE_CURVE ( 'NONE', #59858, #107388, #114364, .T. ) ;
#68146 = DIRECTION ( 'NONE',  ( -0.6830127018922180770, -0.6830127018922204085, -0.2588190451025213501 ) ) ;
#68147 = PLANE ( 'NONE',  #58914 ) ;
#68148 = ORIENTED_EDGE ( 'NONE', *, *, #83883, .F. ) ;
#68149 = CARTESIAN_POINT ( 'NONE',  ( -17.99451991528748351, 28.92564299267950645, 4.000000000000000000 ) ) ;
#68150 = AXIS2_PLACEMENT_3D ( 'NONE', #129362, #74298, #32213 ) ;
#68151 = LINE ( 'NONE', #100731, #11825 ) ;
#68152 = CARTESIAN_POINT ( 'NONE',  ( 48.18398860626899705, 28.73617430169820608, 5.000000000000000000 ) ) ;
#68153 = EDGE_LOOP ( 'NONE', ( #31709, #8946, #50526, #125308 ) ) ;
#68154 = DIRECTION ( 'NONE',  ( -0.5735764363510499342, -0.8191520442889891340, 0.000000000000000000 ) ) ;
#68156 = ADVANCED_FACE ( 'NONE', ( #96677 ), #102794, .T. ) ;
#68155 = VECTOR ( 'NONE', #46383, 1000.000000000000227 ) ;
#68157 = DIRECTION ( 'NONE',  ( 0.7071067811865487940, 0.7071067811865463515, -0.000000000000000000 ) ) ;
#68158 = ORIENTED_EDGE ( 'NONE', *, *, #96074, .F. ) ;
#68160 = EDGE_LOOP ( 'NONE', ( #58120, #56737, #69565, #61835 ) ) ;
#68159 = CARTESIAN_POINT ( 'NONE',  ( 61.46640106136302961, -43.14999999999999147, -34.92499999999998295 ) ) ;
#68161 = EDGE_LOOP ( 'NONE', ( #21411, #125904, #2407, #124462 ) ) ;
#68162 = ADVANCED_FACE ( 'NONE', ( #3436 ), #94024, .T. ) ;
#68163 = FACE_OUTER_BOUND ( 'NONE', #94257, .T. ) ;
#68165 = ADVANCED_FACE ( 'NONE', ( #40919 ), #136827, .F. ) ;
#68164 = CARTESIAN_POINT ( 'NONE',  ( -34.42500000000001137, -22.22500000000000142, 5.000000000000000000 ) ) ;
#68166 = ORIENTED_EDGE ( 'NONE', *, *, #14273, .F. ) ;
#68167 = SURFACE_STYLE_FILL_AREA ( #123233 ) ;
#68168 = UNCERTAINTY_MEASURE_WITH_UNIT (LENGTH_MEASURE( 1.000000000000000082E-05 ), #118302, 'distance_accuracy_value', 'NONE');
#68169 = ORIENTED_EDGE ( 'NONE', *, *, #133838, .T. ) ;
#68170 = LINE ( 'NONE', #88460, #68412 ) ;
#68171 = DIRECTION ( 'NONE',  ( -0.6830127018922180770, -0.6830127018922204085, -0.2588190451025213501 ) ) ;
#68172 = EDGE_CURVE ( 'NONE', #143372, #128366, #140921, .T. ) ;
#68173 = CARTESIAN_POINT ( 'NONE',  ( -8.700255128608413102, -27.71228299555199825, 4.000000000000000000 ) ) ;
#68174 = DIRECTION ( 'NONE',  ( -0.6830127018922180770, -0.6830127018922204085, -0.2588190451025213501 ) ) ;
#68175 = DIRECTION ( 'NONE',  ( 0.6830127018922180770, -0.6830127018922204085, -0.2588190451025213501 ) ) ;
#68176 = CYLINDRICAL_SURFACE ( 'NONE', #125548, 0.5000000000000004441 ) ;
#68177 = CARTESIAN_POINT ( 'NONE',  ( -5.939889289559763697, -9.740707523384184441, 10.89222023123382144 ) ) ;
#68178 = CARTESIAN_POINT ( 'NONE',  ( 3.398789304146613954, 4.202752102959690472E-16, 0.000000000000000000 ) ) ;
#68179 = CARTESIAN_POINT ( 'NONE',  ( 17.77040314143522082, -7.934999999999989839, 2.126176841940957907 ) ) ;
#68180 = DIRECTION ( 'NONE',  ( -0.000000000000000000, 0.3543493200069153248, 0.9351131265310292928 ) ) ;
#68181 = CARTESIAN_POINT ( 'NONE',  ( 111.2500000000000000, -9.735942053221458872E-16, 7.950000000000000178 ) ) ;
#68182 = DIRECTION ( 'NONE',  ( 0.6830127018922180770, -0.6830127018922204085, -0.2588190451025213501 ) ) ;
#68183 = ORIENTED_EDGE ( 'NONE', *, *, #99069, .F. ) ;
#68184 = AXIS2_PLACEMENT_3D ( 'NONE', #82857, #27738, #142239 ) ;
#68185 = ORIENTED_EDGE ( 'NONE', *, *, #138606, .T. ) ;
#68186 = CARTESIAN_POINT ( 'NONE',  ( 89.22916666666667140, 7.950000000000001954, -2.130196079827421762 ) ) ;
#68187 = VERTEX_POINT ( 'NONE', #41619 ) ;
#68188 = EDGE_LOOP ( 'NONE', ( #99240, #61308, #143352, #112219 ) ) ;
#68189 = ORIENTED_EDGE ( 'NONE', *, *, #58485, .T. ) ;
#68190 = LINE ( 'NONE', #112364, #61941 ) ;
#68191 = DIRECTION ( 'NONE',  ( -0.7071067811865487940, 0.7071067811865463515, -0.000000000000000000 ) ) ;
#68192 = CARTESIAN_POINT ( 'NONE',  ( 0.000000000000000000, 0.000000000000000000, 5.000000000000000000 ) ) ;
#68193 = ORIENTED_EDGE ( 'NONE', *, *, #103670, .T. ) ;
#68194 = DIRECTION ( 'NONE',  ( 4.681814790819592407E-17, 0.3543493200069153248, 0.9351131265310292928 ) ) ;
#68195 = CARTESIAN_POINT ( 'NONE',  ( 0.000000000000000000, 0.000000000000000000, 0.000000000000000000 ) ) ;
#68196 = FACE_OUTER_BOUND ( 'NONE', #83885, .T. ) ;
#68197 = CARTESIAN_POINT ( 'NONE',  ( -25.39999999999996305, 0.000000000000000000, 0.000000000000000000 ) ) ;
#68198 = VERTEX_POINT ( 'NONE', #130073 ) ;
#68199 = CARTESIAN_POINT ( 'NONE',  ( 19.27928215921719612, -2.789594763390444321, 4.000000000000000000 ) ) ;
#68200 = CARTESIAN_POINT ( 'NONE',  ( 21.62762920772360786, 8.558752285115851066, 4.000000000000000000 ) ) ;
#68201 = LINE ( 'NONE', #33422, #63628 ) ;
#68202 = VECTOR ( 'NONE', #23277, 999.9999999999998863 ) ;
#68203 = CARTESIAN_POINT ( 'NONE',  ( 11.81601139373100651, 28.73617430169779041, 5.000000000000000000 ) ) ;
#68204 = CARTESIAN_POINT ( 'NONE',  ( 15.70701326429294475, -21.74070752338405654, 4.999753212805220670 ) ) ;
#68205 = PLANE ( 'NONE',  #59324 ) ;
#68206 = CARTESIAN_POINT ( 'NONE',  ( 152.4000000000000057, 25.96999999999993847, 33.92499999999998295 ) ) ;
#68207 = LINE ( 'NONE', #123278, #26071 ) ;
#68208 = AXIS2_PLACEMENT_3D ( 'NONE', #125572, #93649, #37856 ) ;
#68209 = ORIENTED_EDGE ( 'NONE', *, *, #59010, .T. ) ;
#68210 = ORIENTED_EDGE ( 'NONE', *, *, #137074, .T. ) ;
#68211 = CARTESIAN_POINT ( 'NONE',  ( 117.3962635252314470, 4.472830434245840259, -4.472830434245839371 ) ) ;
#68212 = ORIENTED_EDGE ( 'NONE', *, *, #70327, .F. ) ;
#68213 = AXIS2_PLACEMENT_3D ( 'NONE', #127890, #40861, #61240 ) ;
#68214 = EDGE_CURVE ( 'NONE', #101003, #49304, #27566, .T. ) ;
#68215 = PLANE ( 'NONE',  #117235 ) ;
#68216 = CARTESIAN_POINT ( 'NONE',  ( -60.18398860626900415, 28.73617430169829490, 5.000000000000000000 ) ) ;
#68217 = PLANE ( 'NONE',  #106888 ) ;
#68218 = LINE ( 'NONE', #81204, #134607 ) ;
#68219 = CARTESIAN_POINT ( 'NONE',  ( 110.4537635252314516, -6.109999999999998543, -3.741295971395162543E-16 ) ) ;
#68220 = VECTOR ( 'NONE', #133204, 1000.000000000000000 ) ;
#68221 = ORIENTED_EDGE ( 'NONE', *, *, #63457, .F. ) ;
#68222 = ORIENTED_EDGE ( 'NONE', *, *, #133470, .T. ) ;
#68223 = DIRECTION ( 'NONE',  ( -0.7071067811865486830, 0.7071067811865464625, 0.000000000000000000 ) ) ;
#68224 = ORIENTED_EDGE ( 'NONE', *, *, #47396, .T. ) ;
#68225 = ORIENTED_EDGE ( 'NONE', *, *, #2146, .T. ) ;
#68226 = EDGE_CURVE ( 'NONE', #24063, #95958, #75000, .T. ) ;
#68227 = ORIENTED_EDGE ( 'NONE', *, *, #84145, .T. ) ;
#68228 = LINE ( 'NONE', #101513, #74566 ) ;
#68229 = EDGE_CURVE ( 'NONE', #19139, #136292, #81775, .T. ) ;
#68231 = EDGE_CURVE ( 'NONE', #43460, #115656, #81044, .T. ) ;
#68230 = AXIS2_PLACEMENT_3D ( 'NONE', #125494, #61681, #139244 ) ;
#68232 = AXIS2_PLACEMENT_3D ( 'NONE', #22330, #112939, #2745 ) ;
#68233 = TOROIDAL_SURFACE ( 'NONE', #61307, 2.000000000000000000, 1.000000000000000000 ) ;
#68234 = CARTESIAN_POINT ( 'NONE',  ( 27.91209685856478728, 5.291415217122921177, -3.054999999999994831 ) ) ;
#68235 = ORIENTED_EDGE ( 'NONE', *, *, #112266, .F. ) ;
#68237 = ORIENTED_EDGE ( 'NONE', *, *, #62675, .T. ) ;
#68236 = EDGE_CURVE ( 'NONE', #93893, #100719, #76414, .T. ) ;
#68238 = CARTESIAN_POINT ( 'NONE',  ( -26.29298673570676925, -21.74070752338405299, 4.999753212805220670 ) ) ;
#68239 = ORIENTED_EDGE ( 'NONE', *, *, #113154, .T. ) ;
#68240 = ORIENTED_EDGE ( 'NONE', *, *, #127793, .T. ) ;
#68241 = ORIENTED_EDGE ( 'NONE', *, *, #68724, .F. ) ;
#68242 =( BOUNDED_CURVE ( )  B_SPLINE_CURVE ( 2, ( #125255, #135443, #47049, #17709, #59325, #25947, #36127, #124544, #92606, #25215, #125984, #23806, #136837 ),
 .UNSPECIFIED., .F., .F. ) 
 B_SPLINE_CURVE_WITH_KNOTS ( ( 3, 2, 2, 2, 2, 2, 3 ),
 ( 0.2500000000000000000, 0.2583333333333333592, 0.2666666666666666630, 0.2750000000000000222, 0.2833333333333333814, 0.2916666666666667407, 0.3000000000000000444 ),
 .UNSPECIFIED. ) 
 CURVE ( )  GEOMETRIC_REPRESENTATION_ITEM ( )  RATIONAL_B_SPLINE_CURVE ( ( 1.000000000000000000, 0.9659258262890683122, 1.000000000000000000, 0.9659258262890683122, 1.000000000000000000, 0.9659258262890683122, 1.000000000000000000, 0.9659258262890683122, 1.000000000000000000, 0.9659258262890683122, 1.000000000000000000, 0.9659258262890680902, 1.000000000000000222 ) ) 
 REPRESENTATION_ITEM ( '' )  );
#68243 = DIRECTION ( 'NONE',  ( 0.6830127018922181881, 0.6830127018922202975, -0.2588190451025214056 ) ) ;
#68244 = EDGE_CURVE ( 'NONE', #71647, #86576, #75693, .T. ) ;
#68245 = CARTESIAN_POINT ( 'NONE',  ( 9.489213562373095101, -27.52281430457062328, 5.000000000000000000 ) ) ;
#68246 = DIRECTION ( 'NONE',  ( 0.000000000000000000, 0.2631995976047483699, 0.9647414015272167687 ) ) ;
#68247 = VERTEX_POINT ( 'NONE', #97404 ) ;
#68248 = DIRECTION ( 'NONE',  ( -0.6830127018922181881, 0.6830127018922202975, -0.2588190451025214056 ) ) ;
#68249 = EDGE_CURVE ( 'NONE', #104684, #10438, #22683, .T. ) ;
#68250 = CARTESIAN_POINT ( 'NONE',  ( -57.18398860626899705, 28.73617430169827358, 5.000000000000000000 ) ) ;
#68251 = FACE_BOUND ( 'NONE', #61689, .T. ) ;
#68252 = VERTEX_POINT ( 'NONE', #89412 ) ;
#68253 = LINE ( 'NONE', #57358, #117368 ) ;
#68254 = DIRECTION ( 'NONE',  ( -0.9707728879609285322, 0.000000000000000000, 0.2399999999999971323 ) ) ;
#68255 = DIRECTION ( 'NONE',  ( 1.000000000000000000, 0.000000000000000000, 0.000000000000000000 ) ) ;
#68256 = FACE_OUTER_BOUND ( 'NONE', #4674, .T. ) ;
#68257 = ORIENTED_EDGE ( 'NONE', *, *, #57950, .F. ) ;
#68258 = LINE ( 'NONE', #34892, #29547 ) ;
#68259 = ORIENTED_EDGE ( 'NONE', *, *, #64449, .T. ) ;
#68261 = ORIENTED_EDGE ( 'NONE', *, *, #12952, .T. ) ;
#68260 = ADVANCED_FACE ( 'NONE', ( #32178 ), #120578, .F. ) ;
#68262 = ADVANCED_FACE ( 'NONE', ( #133641 ), #66250, .F. ) ;
#68263 = VERTEX_POINT ( 'NONE', #55372 ) ;
#68264 = CARTESIAN_POINT ( 'NONE',  ( 46.72459685856477307, -1.637169565754160949, 6.109999999999997655 ) ) ;
#68265 = ORIENTED_EDGE ( 'NONE', *, *, #11749, .T. ) ;
#68266 = CARTESIAN_POINT ( 'NONE',  ( 19.04500000000000881, 3.130000000000007887, -2.396719511207313368E-16 ) ) ;
#68267 = CARTESIAN_POINT ( 'NONE',  ( 25.17183060077629619, -20.24070752338406720, 4.000000000000000000 ) ) ;
#68268 = EDGE_CURVE ( 'NONE', #98637, #88783, #41603, .T. ) ;
#68269 = ORIENTED_EDGE ( 'NONE', *, *, #86309, .F. ) ;
#68270 = DIRECTION ( 'NONE',  ( -0.000000000000000000, -0.3543493200069152693, 0.9351131265310292928 ) ) ;
#68271 = LINE ( 'NONE', #44360, #38921 ) ;
#68272 = AXIS2_PLACEMENT_3D ( 'NONE', #21694, #99218, #11488 ) ;
#68273 = EDGE_CURVE ( 'NONE', #143262, #138986, #111134, .T. ) ;
#68274 = EDGE_CURVE ( 'NONE', #97938, #3869, #141666, .T. ) ;
#68275 = LINE ( 'NONE', #55952, #133553 ) ;
#68276 = LINE ( 'NONE', #134948, #97121 ) ;
#68277 = CARTESIAN_POINT ( 'NONE',  ( -2.510786437626908008, -27.52281430457053446, 5.000000000000000000 ) ) ;
#68278 = DIRECTION ( 'NONE',  ( -0.000000000000000000, 0.000000000000000000, 1.000000000000000000 ) ) ;
#68279 = ORIENTED_EDGE ( 'NONE', *, *, #68435, .T. ) ;
#68280 = VERTEX_POINT ( 'NONE', #119861 ) ;
#68281 = VERTEX_POINT ( 'NONE', #10404 ) ;
#68282 = ORIENTED_EDGE ( 'NONE', *, *, #137466, .F. ) ;
#68283 = DIRECTION ( 'NONE',  ( 0.6830127018922181881, 0.6830127018922202975, -0.2588190451025214056 ) ) ;
#68284 = ORIENTED_EDGE ( 'NONE', *, *, #142207, .T. ) ;
#68285 = EDGE_CURVE ( 'NONE', #85221, #112404, #87984, .T. ) ;
#68286 = ORIENTED_EDGE ( 'NONE', *, *, #58854, .T. ) ;
#68287 = CARTESIAN_POINT ( 'NONE',  ( 166.3240464593592947, 26.96999999999994557, -33.19920214581096474 ) ) ;
#68288 = DIRECTION ( 'NONE',  ( 0.6830127018922180770, -0.6830127018922204085, -0.2588190451025213501 ) ) ;
#68289 = EDGE_CURVE ( 'NONE', #11322, #102158, #132954, .T. ) ;
#68290 = DIRECTION ( 'NONE',  ( 0.6830127018922181881, 0.6830127018922202975, -0.2588190451025214056 ) ) ;
#68291 = ORIENTED_EDGE ( 'NONE', *, *, #140260, .T. ) ;
#68292 = PLANE ( 'NONE',  #11580 ) ;
#68293 = DIRECTION ( 'NONE',  ( -0.000000000000000000, 0.000000000000000000, 1.000000000000000000 ) ) ;
#68294 = AXIS2_PLACEMENT_3D ( 'NONE', #76739, #10018, #54282 ) ;
#68295 = CARTESIAN_POINT ( 'NONE',  ( 24.12956980810188767, -3.967499999999998028, -6.871911579029511330 ) ) ;
#68296 = PLANE ( 'NONE',  #76285 ) ;
#68297 = ORIENTED_EDGE ( 'NONE', *, *, #131134, .T. ) ;
#68299 = LINE ( 'NONE', #102334, #137947 ) ;
#68298 = CARTESIAN_POINT ( 'NONE',  ( 107.8287635252314516, 0.000000000000000000, -6.109999999999999432 ) ) ;
#68300 = EDGE_CURVE ( 'NONE', #66246, #96290, #33633, .T. ) ;
#68301 = VECTOR ( 'NONE', #71569, 1000.000000000000000 ) ;
#68302 = DIRECTION ( 'NONE',  ( 1.000000000000000000, 0.000000000000000000, 0.000000000000000000 ) ) ;
#68303 = CARTESIAN_POINT ( 'NONE',  ( -20.70025512860841133, -27.71228299555191654, 4.000000000000000000 ) ) ;
#68304 = ORIENTED_EDGE ( 'NONE', *, *, #42171, .T. ) ;
#68305 = CYLINDRICAL_SURFACE ( 'NONE', #142195, 5.968999999999998529 ) ;
#68307 = EDGE_LOOP ( 'NONE', ( #64469, #51957, #139019, #115685 ) ) ;
#68306 = CARTESIAN_POINT ( 'NONE',  ( -54.18398860626899705, 28.73617430169825226, 5.000000000000000000 ) ) ;
#68308 = CARTESIAN_POINT ( 'NONE',  ( -18.87485380690754511, -14.24070752338414181, 9.401115078912701151 ) ) ;
#68309 = VERTEX_POINT ( 'NONE', #121318 ) ;
#68310 = EDGE_CURVE ( 'NONE', #112531, #44739, #143078, .T. ) ;
#68311 = FACE_OUTER_BOUND ( 'NONE', #134405, .T. ) ;
#68312 = FACE_OUTER_BOUND ( 'NONE', #42206, .T. ) ;
#68313 = ORIENTED_EDGE ( 'NONE', *, *, #44603, .T. ) ;
#68314 = DIRECTION ( 'NONE',  ( 0.6830127018922181881, 0.6830127018922202975, -0.2588190451025214056 ) ) ;
#68315 = VECTOR ( 'NONE', #88086, 1000.000000000000000 ) ;
#68316 = LINE ( 'NONE', #92863, #69633 ) ;
#68317 = PLANE ( 'NONE',  #123179 ) ;
#68318 = ORIENTED_EDGE ( 'NONE', *, *, #141689, .T. ) ;
#68319 = DIRECTION ( 'NONE',  ( 0.000000000000000000, 0.000000000000000000, 1.000000000000000000 ) ) ;
#68320 = VERTEX_POINT ( 'NONE', #19860 ) ;
#68321 = CARTESIAN_POINT ( 'NONE',  ( -31.49999999999977973, -4.796895815301051691, -3.611700055028753908 ) ) ;
#68323 = ORIENTED_EDGE ( 'NONE', *, *, #44212, .T. ) ;
#68322 = LINE ( 'NONE', #123404, #32356 ) ;
#68324 = ORIENTED_EDGE ( 'NONE', *, *, #74108, .F. ) ;
#68325 = CARTESIAN_POINT ( 'NONE',  ( 16.52898522435346607, 6.019049105522195298, -28.93301309892516215 ) ) ;
#68326 = DIRECTION ( 'NONE',  ( 0.7071067811865487940, 0.7071067811865463515, 0.000000000000000000 ) ) ;
#68327 = EDGE_LOOP ( 'NONE', ( #82009, #51893, #80510, #72941 ) ) ;
#68328 = AXIS2_PLACEMENT_3D ( 'NONE', #132370, #100428, #362 ) ;
#68329 = CARTESIAN_POINT ( 'NONE',  ( -34.92500000000001137, -20.14387692260736529, 4.000000000000000000 ) ) ;
#68330 = ADVANCED_FACE ( 'NONE', ( #53960 ), #132231, .F. ) ;
#68331 = AXIS2_PLACEMENT_3D ( 'NONE', #81830, #26696, #28844 ) ;
#68332 = FACE_OUTER_BOUND ( 'NONE', #10357, .T. ) ;
#68333 = DIRECTION ( 'NONE',  ( 0.6830127018922181881, 0.6830127018922202975, -0.2588190451025214056 ) ) ;
#68334 = EDGE_LOOP ( 'NONE', ( #126131, #87443, #109997, #103591 ) ) ;
#68335 = EDGE_CURVE ( 'NONE', #133491, #94283, #11823, .T. ) ;
#68337 = VECTOR ( 'NONE', #50680, 1000.000000000000227 ) ;
#68336 = DIRECTION ( 'NONE',  ( -0.000000000000000000, -0.3543493200069152693, 0.9351131265310292928 ) ) ;
#68338 = LINE ( 'NONE', #57440, #2679 ) ;
#68339 = CARTESIAN_POINT ( 'NONE',  ( 24.00548008471250938, 28.92564299267921513, 4.000000000000000000 ) ) ;
#68340 = DIRECTION ( 'NONE',  ( -0.7071067811865486830, 0.7071067811865464625, 0.000000000000000000 ) ) ;
#68341 = DIRECTION ( 'NONE',  ( 0.000000000000000000, 0.000000000000000000, 1.000000000000000000 ) ) ;
#68342 = CARTESIAN_POINT ( 'NONE',  ( 29.99451991528749417, 28.92564299267958816, 4.000000000000000000 ) ) ;
#68343 = VERTEX_POINT ( 'NONE', #43075 ) ;
#68344 = EDGE_LOOP ( 'NONE', ( #63401, #114599, #10819, #4180 ) ) ;
#68345 = ORIENTED_EDGE ( 'NONE', *, *, #125134, .T. ) ;
#68346 = DIRECTION ( 'NONE',  ( 0.7071067811865487940, 0.7071067811865463515, -0.000000000000000000 ) ) ;
#68347 = ORIENTED_EDGE ( 'NONE', *, *, #13487, .T. ) ;
#68348 = ORIENTED_EDGE ( 'NONE', *, *, #79627, .T. ) ;
#68349 = ORIENTED_EDGE ( 'NONE', *, *, #26154, .F. ) ;
#68350 = LINE ( 'NONE', #57454, #66487 ) ;
#68351 = CARTESIAN_POINT ( 'NONE',  ( 23.28769006033955691, -21.73547319004781642, 4.999917730833664642 ) ) ;
#68352 = ORIENTED_EDGE ( 'NONE', *, *, #83986, .F. ) ;
#68353 = FACE_OUTER_BOUND ( 'NONE', #116048, .T. ) ;
#68354 = DIRECTION ( 'NONE',  ( 0.6830127018922180770, -0.6830127018922204085, -0.2588190451025214056 ) ) ;
#68355 = LINE ( 'NONE', #126264, #111127 ) ;
#68356 = DIRECTION ( 'NONE',  ( -0.000000000000000000, 0.3543493200069153248, 0.9351131265310292928 ) ) ;
#68357 = CARTESIAN_POINT ( 'NONE',  ( 121.6254301918981184, 5.291415217122919401, 3.055000000000002824 ) ) ;
#68358 = ORIENTED_EDGE ( 'NONE', *, *, #54815, .T. ) ;
#68359 = DIRECTION ( 'NONE',  ( -0.7071067811865487940, 0.7071067811865463515, -0.000000000000000000 ) ) ;
#68360 = CARTESIAN_POINT ( 'NONE',  ( -33.18398860626899705, 28.73617430169810305, 5.000000000000000000 ) ) ;
#68361 = PLANE ( 'NONE',  #139891 ) ;
#68362 = CARTESIAN_POINT ( 'NONE',  ( 29.20710678118634718, -2.240707523384257716, 5.000000000000000000 ) ) ;
#68363 = DIRECTION ( 'NONE',  ( -0.000000000000000000, -0.3543493200069152693, 0.9351131265310292928 ) ) ;
#68364 = PLANE ( 'NONE',  #97812 ) ;
#68365 = DIRECTION ( 'NONE',  ( 0.6830127018922180770, -0.6830127018922204085, -0.2588190451025213501 ) ) ;
#68366 = CARTESIAN_POINT ( 'NONE',  ( 50.39169371712955581, 2.130196079827421762, 7.950000000000001066 ) ) ;
#68367 = CARTESIAN_POINT ( 'NONE',  ( -36.48921356237310221, -27.52281430457080802, 5.000000000000000000 ) ) ;
#68368 = CARTESIAN_POINT ( 'NONE',  ( 21.48921356237309155, -27.52281430457070499, 5.000000000000000000 ) ) ;
#68369 = ORIENTED_EDGE ( 'NONE', *, *, #43, .F. ) ;
#68370 = ORIENTED_EDGE ( 'NONE', *, *, #134198, .T. ) ;
#68371 = CARTESIAN_POINT ( 'NONE',  ( 49.85416666666665719, -2.130196079827425315, -7.950000000000001066 ) ) ;
#68372 = DIRECTION ( 'NONE',  ( -1.000000000000000000, -0.000000000000000000, -0.000000000000000000 ) ) ;
#68373 = EDGE_CURVE ( 'NONE', #98765, #90432, #49220, .T. ) ;
#68374 = VERTEX_POINT ( 'NONE', #8933 ) ;
#68375 = DIRECTION ( 'NONE',  ( 2.496005001405478586E-15, 1.000000000000000000, -0.000000000000000000 ) ) ;
#68376 = CARTESIAN_POINT ( 'NONE',  ( 1.499999999999990896, 13.46639925780212721, 5.000000000000000000 ) ) ;
#68377 = EDGE_CURVE ( 'NONE', #16488, #23262, #53201, .T. ) ;
#68378 = CARTESIAN_POINT ( 'NONE',  ( 39.22959685856475431, -6.110000000000000320, -1.637169565754161393 ) ) ;
#68379 = VERTEX_POINT ( 'NONE', #13252 ) ;
#68380 = DIRECTION ( 'NONE',  ( 0.7071067811865486830, -0.7071067811865464625, -0.000000000000000000 ) ) ;
#68381 = EDGE_LOOP ( 'NONE', ( #67378, #135259 ) ) ;
#68382 = CARTESIAN_POINT ( 'NONE',  ( 6.328169399223488867, -15.74070752338412049, 4.000000000000000000 ) ) ;
#68383 = CARTESIAN_POINT ( 'NONE',  ( 16.30000000000000071, -2.055000000000000160, 2.789133085058098087E-16 ) ) ;
#68384 = ADVANCED_FACE ( 'NONE', ( #15380 ), #112596, .F. ) ;
#68385 = DIRECTION ( 'NONE',  ( 0.7071067811865487940, -0.7071067811865463515, 0.000000000000000000 ) ) ;
#68386 = ORIENTED_EDGE ( 'NONE', *, *, #111958, .F. ) ;
#68387 = DIRECTION ( 'NONE',  ( -0.6830127018922181881, 0.6830127018922202975, -0.2588190451025214056 ) ) ;
#68388 = EDGE_CURVE ( 'NONE', #109916, #96830, #48776, .T. ) ;
#68389 = ADVANCED_FACE ( 'NONE', ( #59666 ), #103816, .F. ) ;
#68390 = ORIENTED_EDGE ( 'NONE', *, *, #129444, .F. ) ;
#68391 = CARTESIAN_POINT ( 'NONE',  ( 33.29974487139158867, -27.71228299555229313, 4.000000000000000000 ) ) ;
#68392 = LINE ( 'NONE', #112571, #124896 ) ;
#68393 = CARTESIAN_POINT ( 'NONE',  ( 48.18398860626899705, 28.73617430169820608, 5.000000000000000000 ) ) ;
#68394 = CARTESIAN_POINT ( 'NONE',  ( 34.92499999999998295, -16.29806943317885271, 4.500000000000000888 ) ) ;
#68395 = EDGE_CURVE ( 'NONE', #28531, #120155, #67703, .T. ) ;
#68396 = ADVANCED_FACE ( 'NONE', ( #137213 ), #111886, .T. ) ;
#68397 = AXIS2_PLACEMENT_3D ( 'NONE', #67276, #1263, #86881 ) ;
#68398 = ORIENTED_EDGE ( 'NONE', *, *, #71263, .T. ) ;
#68399 =( BOUNDED_CURVE ( )  B_SPLINE_CURVE ( 2, ( #11277, #64273, #21488, #88175, #108441, #8411, #96854, #20028, #55551, #33117, #19338, #53390, #63594 ),
 .UNSPECIFIED., .F., .T. ) 
 B_SPLINE_CURVE_WITH_KNOTS ( ( 3, 2, 2, 2, 2, 2, 3 ),
 ( 0.000000000000000000, 0.002777777777777391474, 0.005555555555554782948, 0.008333333333332174422, 0.01111111111110956590, 0.01388888888888695737, 0.01666666666666434884 ),
 .UNSPECIFIED. ) 
 CURVE ( )  GEOMETRIC_REPRESENTATION_ITEM ( )  RATIONAL_B_SPLINE_CURVE ( ( 1.000000000000000000, 0.9659258262890683122, 1.000000000000000000, 0.9659258262890683122, 1.000000000000000000, 0.9659258262890683122, 1.000000000000000000, 0.9659258262890683122, 1.000000000000000000, 0.9659258262890683122, 1.000000000000000000, 0.9659258262890967339, 0.9999999999999715783 ) ) 
 REPRESENTATION_ITEM ( '' )  );
#68400 = CARTESIAN_POINT ( 'NONE',  ( -26.29289321881326913, -6.740707523384207533, 5.000000000000000000 ) ) ;
#68401 = CARTESIAN_POINT ( 'NONE',  ( 58.39126352523145158, -4.472830434245839371, -4.472830434245839371 ) ) ;
#68402 = VECTOR ( 'NONE', #10695, 999.9999999999998863 ) ;
#68403 = CARTESIAN_POINT ( 'NONE',  ( 27.32816939922334143, 8.259292476615632594, 4.000000000000000000 ) ) ;
#68404 = EDGE_CURVE ( 'NONE', #20953, #123646, #37910, .T. ) ;
#68405 = CARTESIAN_POINT ( 'NONE',  ( 18.29974487139159223, -27.71228299555219010, 4.000000000000000000 ) ) ;
#68407 = ORIENTED_EDGE ( 'NONE', *, *, #52942, .F. ) ;
#68406 = CARTESIAN_POINT ( 'NONE',  ( -7.499999999999944045, -16.53360074219757081, 5.000000000000000000 ) ) ;
#68408 = VERTEX_POINT ( 'NONE', #135776 ) ;
#68409 = DIRECTION ( 'NONE',  ( -0.7071067811865486830, 0.7071067811865464625, 0.000000000000000000 ) ) ;
#68410 = VERTEX_POINT ( 'NONE', #124895 ) ;
#68411 = EDGE_CURVE ( 'NONE', #94185, #30378, #32255, .T. ) ;
#68412 = VECTOR ( 'NONE', #80441, 1000.000000000000000 ) ;
#68413 = CARTESIAN_POINT ( 'NONE',  ( -39.88837638105217565, 9.759292476615614831, 17.35367589129221955 ) ) ;
#68414 = VERTEX_POINT ( 'NONE', #136473 ) ;
#68415 = FILL_AREA_STYLE_COLOUR ( '', #58570 ) ;
#68416 = DIRECTION ( 'NONE',  ( -0.000000000000000000, -0.3543493200069152693, 0.9351131265310292928 ) ) ;
#68417 = CARTESIAN_POINT ( 'NONE',  ( 36.29974487139159578, -27.71228299555231445, 4.000000000000000000 ) ) ;
#68418 = FACE_BOUND ( 'NONE', #98000, .T. ) ;
#68419 = CARTESIAN_POINT ( 'NONE',  ( -34.92500000000001137, 22.22500000000000142, 4.000000000000000000 ) ) ;
#68420 = CARTESIAN_POINT ( 'NONE',  ( 151.4000000000000057, -16.48000000000005016, -34.92499999999998295 ) ) ;
#68421 = CARTESIAN_POINT ( 'NONE',  ( 54.29974487139159578, -27.71228299555243879, 4.000000000000000000 ) ) ;
#68422 = CARTESIAN_POINT ( 'NONE',  ( 0.000000000000000000, 0.000000000000000000, 5.000000000000000000 ) ) ;
#68424 = VERTEX_POINT ( 'NONE', #46682 ) ;
#68423 = DIRECTION ( 'NONE',  ( -0.000000000000000000, -0.3543493200069152693, 0.9351131265310292928 ) ) ;
#68425 = ADVANCED_FACE ( 'NONE', ( #26305 ), #13964, .T. ) ;
#68426 = DIRECTION ( 'NONE',  ( 1.000000000000000000, 0.000000000000000000, 0.000000000000000000 ) ) ;
#68427 = VECTOR ( 'NONE', #58029, 1000.000000000000000 ) ;
#68428 = ORIENTED_EDGE ( 'NONE', *, *, #116149, .T. ) ;
#68430 = ORIENTED_EDGE ( 'NONE', *, *, #11576, .T. ) ;
#68429 = VECTOR ( 'NONE', #56262, 1000.000000000000000 ) ;
#68431 = CARTESIAN_POINT ( 'NONE',  ( 72.68293019189810877, -1.637169565754158951, -6.109999999999998543 ) ) ;
#68432 = ORIENTED_EDGE ( 'NONE', *, *, #137577, .T. ) ;
#68433 = AXIS2_PLACEMENT_3D ( 'NONE', #89238, #33464, #79112 ) ;
#68434 = DIRECTION ( 'NONE',  ( -0.7071067811865486830, -0.7071067811865464625, 0.000000000000000000 ) ) ;
#68435 = EDGE_CURVE ( 'NONE', #135110, #77074, #91562, .T. ) ;
#68436 = ORIENTED_EDGE ( 'NONE', *, *, #40975, .F. ) ;
#68437 = DIRECTION ( 'NONE',  ( 0.7071067811865487940, -0.7071067811865463515, 0.000000000000000000 ) ) ;
#68438 = DIRECTION ( 'NONE',  ( -0.7071067811865487940, 0.7071067811865463515, 0.000000000000000000 ) ) ;
#68439 = ADVANCED_FACE ( 'NONE', ( #14706 ), #103140, .T. ) ;
#68440 = LINE ( 'NONE', #12578, #105775 ) ;
#68441 = CARTESIAN_POINT ( 'NONE',  ( -34.45011844616453800, 10.51628081163737249, 5.000000000000000888 ) ) ;
#68443 = DIRECTION ( 'NONE',  ( 0.6830127018922180770, -0.6830127018922204085, -0.2588190451025213501 ) ) ;
#68442 = CARTESIAN_POINT ( 'NONE',  ( -26.99999999999981526, -10.77435723561697145, -9.972017380717165480 ) ) ;
#68444 = EDGE_CURVE ( 'NONE', #97623, #53287, #123504, .T. ) ;
#68445 = CARTESIAN_POINT ( 'NONE',  ( -8.207106781186489286, 3.759292476615680112, 5.000000000000000000 ) ) ;
#68446 = LINE ( 'NONE', #90897, #64743 ) ;
#68447 = VERTEX_POINT ( 'NONE', #1647 ) ;
#68448 = EDGE_LOOP ( 'NONE', ( #87851, #105696, #56259, #76621 ) ) ;
#68449 = LINE ( 'NONE', #45271, #21879 ) ;
#68450 =( LENGTH_UNIT ( ) NAMED_UNIT ( * ) SI_UNIT ( .MILLI., .METRE. ) );
#68451 = EDGE_LOOP ( 'NONE', ( #79511, #33125, #126041 ) ) ;
#68452 = ADVANCED_FACE ( 'NONE', ( #134361 ), #102456, .T. ) ;
#68453 = ORIENTED_EDGE ( 'NONE', *, *, #124168, .T. ) ;
#68454 = ORIENTED_EDGE ( 'NONE', *, *, #123365, .T. ) ;
#68455 = CARTESIAN_POINT ( 'NONE',  ( 28.00043019189810067, -3.055000000000002380, 5.291415217122920289 ) ) ;
#68456 = VERTEX_POINT ( 'NONE', #37170 ) ;
#68457 = PLANE ( 'NONE',  #83340 ) ;
#68458 = ADVANCED_FACE ( 'NONE', ( #24157 ), #48283, .T. ) ;
#68459 = CARTESIAN_POINT ( 'NONE',  ( -2.999999999999975131, 12.83542986846996925, -1.025386466790363826 ) ) ;
#68460 = CARTESIAN_POINT ( 'NONE',  ( 3.421236474768552860, -9.717572351234235426E-16, -7.934999999999990727 ) ) ;
#68461 = PLANE ( 'NONE',  #44992 ) ;
#68462 = EDGE_LOOP ( 'NONE', ( #94386, #93916, #142291, #7665 ) ) ;
#68463 = EDGE_CURVE ( 'NONE', #15691, #109971, #114708, .T. ) ;
#68464 = FACE_OUTER_BOUND ( 'NONE', #112864, .T. ) ;
#68465 = CARTESIAN_POINT ( 'NONE',  ( 9.005480084712511157, 28.92564299267931816, 4.000000000000000000 ) ) ;
#68466 = CARTESIAN_POINT ( 'NONE',  ( 0.7071067811865432429, 8.259292476615634371, 5.000000000000000000 ) ) ;
#68468 = VERTEX_POINT ( 'NONE', #50912 ) ;
#68467 = FACE_OUTER_BOUND ( 'NONE', #61021, .T. ) ;
#68469 = ORIENTED_EDGE ( 'NONE', *, *, #29725, .T. ) ;
#68470 = LINE ( 'NONE', #122081, #98203 ) ;
#68471 = DIRECTION ( 'NONE',  ( 0.7071067811865486830, -0.7071067811865464625, -0.000000000000000000 ) ) ;
#68472 = DIRECTION ( 'NONE',  ( -0.000000000000000000, 0.3543493200069153248, 0.9351131265310292928 ) ) ;
#68473 = ORIENTED_EDGE ( 'NONE', *, *, #44476, .F. ) ;
#68474 = FACE_OUTER_BOUND ( 'NONE', #19491, .T. ) ;
#68475 = DIRECTION ( 'NONE',  ( 0.6830127018922180770, -0.6830127018922204085, -0.2588190451025213501 ) ) ;
#68476 = FILL_AREA_STYLE ('',( #56185 ) ) ;
#68477 = CARTESIAN_POINT ( 'NONE',  ( -28.82816939922332367, 15.75929247661555443, 4.000000000000000000 ) ) ;
#68478 = CARTESIAN_POINT ( 'NONE',  ( -34.49999999999976552, 0.05432934483094037370, 4.994342998332168548 ) ) ;
#68479 = DIRECTION ( 'NONE',  ( -0.7071067811865486830, 0.7071067811865464625, 0.000000000000000000 ) ) ;
#68480 = DIRECTION ( 'NONE',  ( -0.5735764363510501562, 0.8191520442889890230, 1.003171929053521419E-16 ) ) ;
#68481 = CARTESIAN_POINT ( 'NONE',  ( -12.19999999999999574, -60.26999999999998892, 25.00000000000000000 ) ) ;
#68482 = DIRECTION ( 'NONE',  ( -1.000000000000000000, -1.224606353822377258E-16, -0.000000000000000000 ) ) ;
#68483 = ORIENTED_EDGE ( 'NONE', *, *, #121521, .T. ) ;
#68484 = EDGE_CURVE ( 'NONE', #56571, #118999, #40751, .T. ) ;
#68485 = VERTEX_POINT ( 'NONE', #39333 ) ;
#68486 = CARTESIAN_POINT ( 'NONE',  ( 25.89892480454907542, 0.000000000000000000, -6.350000000000003197 ) ) ;
#68487 = DIRECTION ( 'NONE',  ( -1.000000000000000000, -0.000000000000000000, -0.000000000000000000 ) ) ;
#68488 = CARTESIAN_POINT ( 'NONE',  ( -0.02126352523144718967, -5.808823158059033709, 5.808823158059035485 ) ) ;
#68489 = VECTOR ( 'NONE', #48926, 1000.000000000000000 ) ;
#68490 = DIRECTION ( 'NONE',  ( 0.7071067811865486830, -0.7071067811865464625, -0.000000000000000000 ) ) ;
#68491 = EDGE_CURVE ( 'NONE', #34745, #138332, #41541, .T. ) ;
#68492 = ORIENTED_EDGE ( 'NONE', *, *, #16602, .T. ) ;
#68493 = DIRECTION ( 'NONE',  ( -0.000000000000000000, 0.000000000000000000, 1.000000000000000000 ) ) ;
#68494 = DIRECTION ( 'NONE',  ( 0.7071067811865486830, -0.7071067811865464625, -0.000000000000000000 ) ) ;
#68495 = LINE ( 'NONE', #55454, #86144 ) ;
#68496 = MECHANICAL_DESIGN_GEOMETRIC_PRESENTATION_REPRESENTATION (  '', ( #24283 ), #63818 ) ;
#68497 = ORIENTED_EDGE ( 'NONE', *, *, #81411, .F. ) ;
#68498 = CARTESIAN_POINT ( 'NONE',  ( -14.99999999999988098, 20.58746187583902554, 4.000000000000000000 ) ) ;
#68499 = PLANE ( 'NONE',  #123340 ) ;
#68500 = CARTESIAN_POINT ( 'NONE',  ( 1.147419327679491285, 22.22500000000000142, 18.66918814110288238 ) ) ;
#68501 = CARTESIAN_POINT ( 'NONE',  ( 52.70376352523144448, 6.109999999999999432, 1.122388791418549108E-15 ) ) ;
#68502 = CARTESIAN_POINT ( 'NONE',  ( -19.43312800248730099, -21.74070752338405654, 6.915939825044120859 ) ) ;
#68503 = EDGE_CURVE ( 'NONE', #70270, #36313, #140746, .T. ) ;
#68504 = CARTESIAN_POINT ( 'NONE',  ( -34.92500000000001137, 19.70193056682081334, 4.500000000000000888 ) ) ;
#68505 = DIRECTION ( 'NONE',  ( 0.7071067811865487940, 0.7071067811865463515, 0.000000000000000000 ) ) ;
#68506 = ORIENTED_EDGE ( 'NONE', *, *, #133712, .T. ) ;
#68507 = DIRECTION ( 'NONE',  ( -0.6830127018922180770, -0.6830127018922204085, -0.2588190451025213501 ) ) ;
#68508 = ORIENTED_EDGE ( 'NONE', *, *, #49747, .F. ) ;
#68509 = CARTESIAN_POINT ( 'NONE',  ( 5.443598275411213550, 3.821174125832445049E-16, 0.000000000000000000 ) ) ;
#68510 = SURFACE_STYLE_USAGE ( .BOTH. , #3883 ) ;
#68511 = LINE ( 'NONE', #122860, #92868 ) ;
#68512 = CARTESIAN_POINT ( 'NONE',  ( 1.146006882977913088, 0.4000000000000001332, -2.166563419957292957 ) ) ;
#68513 = EDGE_CURVE ( 'NONE', #103695, #75761, #74088, .T. ) ;
#68514 = PLANE ( 'NONE',  #9294 ) ;
#68515 = LINE ( 'NONE', #33744, #131082 ) ;
#68516 = VERTEX_POINT ( 'NONE', #8077 ) ;
#68517 = VERTEX_POINT ( 'NONE', #106680 ) ;
#68518 = CARTESIAN_POINT ( 'NONE',  ( -9.183988606268997046, 28.73617430169793607, 5.000000000000000000 ) ) ;
#68519 = CYLINDRICAL_SURFACE ( 'NONE', #113877, 7.950000000000000178 ) ;
#68520 = CARTESIAN_POINT ( 'NONE',  ( 0.000000000000000000, 0.000000000000000000, 8.094999999999991758 ) ) ;
#68521 = AXIS2_PLACEMENT_3D ( 'NONE', #1783, #46085, #90261 ) ;
#68522 = CARTESIAN_POINT ( 'NONE',  ( 31.03163515922171811, 2.259292476615690770, 13.77329220150644673 ) ) ;
#68523 = CARTESIAN_POINT ( 'NONE',  ( 73.28752705046288440, 0.000000000000000000, -7.949999999999998401 ) ) ;
#68524 = DIRECTION ( 'NONE',  ( -0.3543493200069162685, -0.000000000000000000, -0.9351131265310288487 ) ) ;
#68525 = CIRCLE ( 'NONE', #19841, 2.500000000000000444 ) ;
#68526 = DIRECTION ( 'NONE',  ( -0.000000000000000000, 0.3543493200069153248, 0.9351131265310292928 ) ) ;
#68527 = VERTEX_POINT ( 'NONE', #139379 ) ;
#68528 = CARTESIAN_POINT ( 'NONE',  ( 76.68750000000000000, -5.819803920172573086, 5.819803920172572198 ) ) ;
#68529 = AXIS2_PLACEMENT_3D ( 'NONE', #56129, #106148, #97426 ) ;
#68530 = PLANE ( 'NONE',  #5255 ) ;
#68531 = LINE ( 'NONE', #90991, #9157 ) ;
#68532 = CARTESIAN_POINT ( 'NONE',  ( 17.81601139373099940, 28.73617430169775133, 5.000000000000000000 ) ) ;
#68533 = VECTOR ( 'NONE', #39784, 999.9999999999998863 ) ;
#68534 = VERTEX_POINT ( 'NONE', #105964 ) ;
#68535 = LINE ( 'NONE', #46812, #86159 ) ;
#68536 = CARTESIAN_POINT ( 'NONE',  ( 13.13598696172163116, -2.500000000000000000, 3.061616997868383634E-16 ) ) ;
#68537 = CARTESIAN_POINT ( 'NONE',  ( 62.70876352523143993, -7.482591942790329030E-16, 6.110000000000001208 ) ) ;
#68538 = EDGE_CURVE ( 'NONE', #91497, #74755, #16275, .T. ) ;
#68539 = VERTEX_POINT ( 'NONE', #27003 ) ;
#68540 = ORIENTED_EDGE ( 'NONE', *, *, #106738, .T. ) ;
#68541 = CARTESIAN_POINT ( 'NONE',  ( -42.29974487139158157, -27.71228299555235708, 4.000000000000000000 ) ) ;
#68542 = DIRECTION ( 'NONE',  ( 0.7071067811865487940, 0.7071067811865463515, -0.000000000000000000 ) ) ;
#68543 = FACE_OUTER_BOUND ( 'NONE', #80369, .T. ) ;
#68544 = EDGE_CURVE ( 'NONE', #97146, #18696, #117552, .T. ) ;
#68546 = VERTEX_POINT ( 'NONE', #104564 ) ;
#68545 = CARTESIAN_POINT ( 'NONE',  ( 86.02083333333331439, 7.949999999999998401, 2.130196079827431532 ) ) ;
#68547 = CARTESIAN_POINT ( 'NONE',  ( -12.18398860626900060, 28.73617430169795739, 5.000000000000000000 ) ) ;
#68548 = DIRECTION ( 'NONE',  ( 0.7071067811865487940, 0.7071067811865463515, -0.000000000000000000 ) ) ;
#68549 = DIRECTION ( 'NONE',  ( 1.000000000000000000, 0.000000000000000000, 0.000000000000000000 ) ) ;
#68550 = CARTESIAN_POINT ( 'NONE',  ( 25.21321903303343248, 12.75929247661558641, 10.29404684609041176 ) ) ;
#68551 = ORIENTED_EDGE ( 'NONE', *, *, #94255, .T. ) ;
#68553 = VERTEX_POINT ( 'NONE', #93701 ) ;
#68552 = EDGE_CURVE ( 'NONE', #66092, #81560, #5230, .T. ) ;
#68554 = EDGE_CURVE ( 'NONE', #88238, #79108, #137926, .T. ) ;
#68555 = CARTESIAN_POINT ( 'NONE',  ( 52.50043019189811133, -3.055000000000002380, 5.291415217122920289 ) ) ;
#68556 = ORIENTED_EDGE ( 'NONE', *, *, #90328, .T. ) ;
#68557 = ADVANCED_FACE ( 'NONE', ( #35 ), #11638, .F. ) ;
#68558 = CARTESIAN_POINT ( 'NONE',  ( -9.792893218813388145, 6.759292476615645029, 5.000000000000000000 ) ) ;
#68559 = CARTESIAN_POINT ( 'NONE',  ( 6.183988606268994381, 28.73617430169791476, 5.000000000000000000 ) ) ;
#68561 = EDGE_CURVE ( 'NONE', #87397, #36671, #83062, .T. ) ;
#68560 = CARTESIAN_POINT ( 'NONE',  ( 8.700255128608413102, -27.71228299555199825, 4.000000000000000000 ) ) ;
#68562 = PLANE ( 'NONE',  #48034 ) ;
#68563 = PLANE ( 'NONE',  #119561 ) ;
#68564 = ORIENTED_EDGE ( 'NONE', *, *, #79867, .T. ) ;
#68565 = ORIENTED_EDGE ( 'NONE', *, *, #110779, .T. ) ;
#68566 = EDGE_CURVE ( 'NONE', #34037, #142123, #31301, .T. ) ;
#68567 = DIRECTION ( 'NONE',  ( 0.000000000000000000, -1.000000000000000000, 0.000000000000000000 ) ) ;
#68568 = CARTESIAN_POINT ( 'NONE',  ( -17.33028271673254750, -2.068042672074010380, -32.75052031823620524 ) ) ;
#68569 = EDGE_CURVE ( 'NONE', #106062, #133913, #42903, .T. ) ;
#68570 = EDGE_LOOP ( 'NONE', ( #128192, #129792, #104821, #59885 ) ) ;
#68571 = SURFACE_STYLE_FILL_AREA ( #134535 ) ;
#68572 = LINE ( 'NONE', #25021, #111890 ) ;
#68573 = ORIENTED_EDGE ( 'NONE', *, *, #126311, .F. ) ;
#68574 = EDGE_CURVE ( 'NONE', #120179, #130843, #77666, .T. ) ;
#68575 = FACE_BOUND ( 'NONE', #6893, .T. ) ;
#68576 = CARTESIAN_POINT ( 'NONE',  ( -8.994519915287490619, 28.92564299267944250, 4.000000000000000000 ) ) ;
#68577 = PLANE ( 'NONE',  #326 ) ;
#68578 = CARTESIAN_POINT ( 'NONE',  ( 14.14818355038136133, 17.25929247661554555, 8.802941693769234632 ) ) ;
#68579 = CARTESIAN_POINT ( 'NONE',  ( -81.29974487139159578, -27.71228299555262709, 4.000000000000000000 ) ) ;
#68580 = EDGE_CURVE ( 'NONE', #69001, #83013, #103820, .T. ) ;
#68581 = PLANE ( 'NONE',  #76715 ) ;
#68582 = DIRECTION ( 'NONE',  ( 0.000000000000000000, 0.000000000000000000, 1.000000000000000000 ) ) ;
#68584 = VERTEX_POINT ( 'NONE', #63928 ) ;
#68583 = AXIS2_PLACEMENT_3D ( 'NONE', #62066, #49769, #5490 ) ;
#68585 = ORIENTED_EDGE ( 'NONE', *, *, #102081, .F. ) ;
#68586 = CARTESIAN_POINT ( 'NONE',  ( 101.9954301918981230, 5.291415217122916737, 3.055000000000001936 ) ) ;
#68587 = VERTEX_POINT ( 'NONE', #121137 ) ;
#68588 = VECTOR ( 'NONE', #17359, 999.9999999999998863 ) ;
#68589 = DIRECTION ( 'NONE',  ( 1.000000000000000000, 0.000000000000000000, 0.000000000000000000 ) ) ;
#68590 = VERTEX_POINT ( 'NONE', #55918 ) ;
#68591 = FACE_OUTER_BOUND ( 'NONE', #131003, .T. ) ;
#68592 = DIRECTION ( 'NONE',  ( 0.7071067811865486830, -0.7071067811865464625, -0.000000000000000000 ) ) ;
#68593 = ORIENTED_EDGE ( 'NONE', *, *, #89475, .T. ) ;
#68594 = LINE ( 'NONE', #35263, #6628 ) ;
#68595 = FILL_AREA_STYLE_COLOUR ( '', #80176 ) ;
#68596 = AXIS2_PLACEMENT_3D ( 'NONE', #18341, #9620, #141599 ) ;
#68598 = CARTESIAN_POINT ( 'NONE',  ( -0.4981634851395633223, -17.24070752338410628, 8.407044977365226046 ) ) ;
#68597 = LINE ( 'NONE', #122960, #87464 ) ;
#68599 = ADVANCED_FACE ( 'NONE', ( #55194 ), #33467, .F. ) ;
#68600 = LINE ( 'NONE', #135971, #53129 ) ;
#68601 = CARTESIAN_POINT ( 'NONE',  ( 7.499999999999958256, 4.466399257802219580, 5.000000000000000000 ) ) ;
#68602 = EDGE_LOOP ( 'NONE', ( #120429, #5929, #71462, #20552 ) ) ;
#68603 = DIRECTION ( 'NONE',  ( -0.7071067811865486830, -0.7071067811865464625, 0.000000000000000000 ) ) ;
#68604 = EDGE_CURVE ( 'NONE', #81804, #127735, #44333, .T. ) ;
#68605 = CARTESIAN_POINT ( 'NONE',  ( 26.99999999999981526, -15.03360074219758147, 5.000000000000000000 ) ) ;
#68606 = ORIENTED_EDGE ( 'NONE', *, *, #103705, .F. ) ;
#68608 = EDGE_LOOP ( 'NONE', ( #134333, #133653, #64899, #111688 ) ) ;
#68607 = VECTOR ( 'NONE', #60903, 1000.000000000000000 ) ;
#68609 = VERTEX_POINT ( 'NONE', #108813 ) ;
#68610 = CARTESIAN_POINT ( 'NONE',  ( 49.87543019189810423, -5.291415217122920289, -3.055000000000001492 ) ) ;
#68611 = EDGE_LOOP ( 'NONE', ( #95757, #117088, #68349, #15336 ) ) ;
#68612 = EDGE_CURVE ( 'NONE', #109110, #138595, #66080, .T. ) ;
#68613 = VECTOR ( 'NONE', #16069, 999.9999999999998863 ) ;
#68614 = AXIS2_PLACEMENT_3D ( 'NONE', #126310, #81414, #116141 ) ;
#68615 = CARTESIAN_POINT ( 'NONE',  ( -39.29974487139159578, -27.71228299555233576, 4.000000000000000000 ) ) ;
#68616 = AXIS2_PLACEMENT_3D ( 'NONE', #7854, #17317, #49276 ) ;
#68617 = CARTESIAN_POINT ( 'NONE',  ( 4.420806282870438864, 3.047499999999997655, 5.278424836066143655 ) ) ;
#68618 = CARTESIAN_POINT ( 'NONE',  ( 92.89626352523143282, 4.472830434245840259, -4.472830434245838482 ) ) ;
#68619 = DIRECTION ( 'NONE',  ( 0.7071067811865486830, -0.7071067811865464625, -0.000000000000000000 ) ) ;
#68620 = ORIENTED_EDGE ( 'NONE', *, *, #90738, .F. ) ;
#68621 = VECTOR ( 'NONE', #134139, 1000.000000000000000 ) ;
#68622 = EDGE_CURVE ( 'NONE', #139225, #124741, #110244, .T. ) ;
#68623 = LINE ( 'NONE', #25068, #84968 ) ;
#68624 = ORIENTED_EDGE ( 'NONE', *, *, #59372, .F. ) ;
#68625 = DIRECTION ( 'NONE',  ( 0.7071067811865487940, 0.7071067811865463515, 0.000000000000000000 ) ) ;
#68626 = VECTOR ( 'NONE', #64558, 1000.000000000000114 ) ;
#68627 = DIRECTION ( 'NONE',  ( 0.7071067811865487940, 0.7071067811865463515, 0.000000000000000000 ) ) ;
#68628 = EDGE_LOOP ( 'NONE', ( #31511, #23254, #14971, #40193 ) ) ;
#68629 = FACE_OUTER_BOUND ( 'NONE', #2002, .T. ) ;
#68630 = DIRECTION ( 'NONE',  ( -0.000000000000000000, 0.3543493200069153248, 0.9351131265310292928 ) ) ;
#68631 = CARTESIAN_POINT ( 'NONE',  ( 126.3495968585647944, 6.109999999999997655, 1.637169565754163836 ) ) ;
#68632 = ORIENTED_EDGE ( 'NONE', *, *, #58313, .F. ) ;
#68633 = CARTESIAN_POINT ( 'NONE',  ( 5.671830600776432973, -9.740707523384186217, 4.000000000000000000 ) ) ;
#68634 = ORIENTED_EDGE ( 'NONE', *, *, #107140, .T. ) ;
#68635 = ORIENTED_EDGE ( 'NONE', *, *, #11756, .T. ) ;
#68636 = ORIENTED_EDGE ( 'NONE', *, *, #36440, .T. ) ;
#68637 = DIRECTION ( 'NONE',  ( 0.000000000000000000, -0.000000000000000000, -1.000000000000000000 ) ) ;
#68638 = CARTESIAN_POINT ( 'NONE',  ( -33.29974487139158867, -27.71228299555229313, 4.000000000000000000 ) ) ;
#68639 = DIRECTION ( 'NONE',  ( -0.000000000000000000, -0.3543493200069152693, 0.9351131265310292928 ) ) ;
#68640 = EDGE_CURVE ( 'NONE', #89124, #56014, #88546, .T. ) ;
#68641 = DIRECTION ( 'NONE',  ( -0.7071067811865487940, 0.7071067811865463515, -0.000000000000000000 ) ) ;
#68642 = DIRECTION ( 'NONE',  ( 0.7071067811865487940, -0.7071067811865463515, 0.000000000000000000 ) ) ;
#68643 = EDGE_LOOP ( 'NONE', ( #139001, #127308, #134849, #89562 ) ) ;
#68644 = PRESENTATION_STYLE_ASSIGNMENT (( #24395 ) ) ;
#68645 = CARTESIAN_POINT ( 'NONE',  ( 23.31206980810188512, 7.934999999999993392, 2.126176841940951689 ) ) ;
#68646 = CARTESIAN_POINT ( 'NONE',  ( 3.604862331875187564, 21.75929247661549937, 21.32995629748186062 ) ) ;
#68647 = VECTOR ( 'NONE', #106364, 999.9999999999998863 ) ;
#68648 = LINE ( 'NONE', #112832, #64531 ) ;
#68649 = CARTESIAN_POINT ( 'NONE',  ( -33.81889366174460321, 22.27000000000001023, -13.38643001103286423 ) ) ;
#68650 = ORIENTED_EDGE ( 'NONE', *, *, #84357, .T. ) ;
#68651 = ORIENTED_EDGE ( 'NONE', *, *, #126628, .T. ) ;
#68652 = VERTEX_POINT ( 'NONE', #132780 ) ;
#68653 = CARTESIAN_POINT ( 'NONE',  ( 39.18398860626899705, 28.73617430169814568, 5.000000000000000000 ) ) ;
#68654 = DIRECTION ( 'NONE',  ( 0.6830127018922181881, 0.6830127018922202975, -0.2588190451025214056 ) ) ;
#68655 = VECTOR ( 'NONE', #125589, 1000.000000000000000 ) ;
#68656 = PLANE ( 'NONE',  #91376 ) ;
#68657 = CARTESIAN_POINT ( 'NONE',  ( 34.42499999999998295, -12.02281430457047939, 5.000000000000000000 ) ) ;
#68658 = LINE ( 'NONE', #135347, #114906 ) ;
#68660 = EDGE_CURVE ( 'NONE', #92375, #50477, #2584, .T. ) ;
#68659 =( BOUNDED_CURVE ( )  B_SPLINE_CURVE ( 3, ( #124234, #23486, #136521, #69158 ),
 .UNSPECIFIED., .F., .F. ) 
 B_SPLINE_CURVE_WITH_KNOTS ( ( 4, 4 ),
 ( 2.605825008650064500, 2.701628967222373223 ),
 .UNSPECIFIED. ) 
 CURVE ( )  GEOMETRIC_REPRESENTATION_ITEM ( )  RATIONAL_B_SPLINE_CURVE ( ( 1.000000000000000000, 0.9992352797041761381, 0.9992352797041761381, 1.000000000000000000 ) ) 
 REPRESENTATION_ITEM ( '' )  );
#68661 = PLANE ( 'NONE',  #103966 ) ;
#68662 = EDGE_CURVE ( 'NONE', #130434, #14650, #136242, .T. ) ;
#68663 = LINE ( 'NONE', #132511, #96497 ) ;
#68664 = CARTESIAN_POINT ( 'NONE',  ( 20.99999999999985789, 8.966399257802171618, 5.000000000000000000 ) ) ;
#68665 = CARTESIAN_POINT ( 'NONE',  ( 152.4000000000000057, 7.919999999999947526, 21.67769999999994113 ) ) ;
#68666 = DIRECTION ( 'NONE',  ( 1.000000000000000000, 0.000000000000000000, 0.000000000000000000 ) ) ;
#68667 = VECTOR ( 'NONE', #98261, 1000.000000000000000 ) ;
#68668 = ORIENTED_EDGE ( 'NONE', *, *, #40066, .T. ) ;
#68669 = CARTESIAN_POINT ( 'NONE',  ( 18.18398860626898994, 28.73617430169800002, 5.000000000000000000 ) ) ;
#68670 = EDGE_LOOP ( 'NONE', ( #78166, #114395, #139299, #118616 ) ) ;
#68671 =( BOUNDED_CURVE ( )  B_SPLINE_CURVE ( 3, ( #77535, #121699, #20243, #131169 ),
 .UNSPECIFIED., .F., .T. ) 
 B_SPLINE_CURVE_WITH_KNOTS ( ( 4, 4 ),
 ( 1.989451877885351383, 2.205626217416131407 ),
 .UNSPECIFIED. ) 
 CURVE ( )  GEOMETRIC_REPRESENTATION_ITEM ( )  RATIONAL_B_SPLINE_CURVE ( ( 1.000000000000000000, 0.9961095111196431873, 0.9961095111196431873, 1.000000000000000000 ) ) 
 REPRESENTATION_ITEM ( '' )  );
#68672 = DIRECTION ( 'NONE',  ( -0.7071067811865486830, 0.7071067811865464625, 0.000000000000000000 ) ) ;
#68673 = ORIENTED_EDGE ( 'NONE', *, *, #24159, .F. ) ;
#68674 = ADVANCED_FACE ( 'NONE', ( #54492 ), #34424, .T. ) ;
#68675 = CARTESIAN_POINT ( 'NONE',  ( 25.39999999999999858, -16.48000000000005016, 12.69999999999954632 ) ) ;
#68676 = CARTESIAN_POINT ( 'NONE',  ( -57.29974487139158157, -27.71228299555246011, 4.000000000000000000 ) ) ;
#68677 = ORIENTED_EDGE ( 'NONE', *, *, #94380, .F. ) ;
#68678 = CARTESIAN_POINT ( 'NONE',  ( -72.18398860626899705, 28.73617430169837661, 5.000000000000000000 ) ) ;
#68679 = ORIENTED_EDGE ( 'NONE', *, *, #142085, .T. ) ;
#68680 = DIRECTION ( 'NONE',  ( 1.000000000000000000, 1.224606353822377258E-16, 0.000000000000000000 ) ) ;
#68681 = VERTEX_POINT ( 'NONE', #10925 ) ;
#68682 = CARTESIAN_POINT ( 'NONE',  ( -22.82816939922337696, -11.24070752338416490, 4.000000000000000000 ) ) ;
#68683 = CIRCLE ( 'NONE', #29224, 2.999999999999997780 ) ;
#68684 = CARTESIAN_POINT ( 'NONE',  ( 107.7041937171295558, -6.884901960086285300, -3.975000000000000089 ) ) ;
#68685 = CARTESIAN_POINT ( 'NONE',  ( 32.99999999999977263, -8.151047557385043163, -8.977947279169878669 ) ) ;
#68686 = LINE ( 'NONE', #45517, #83310 ) ;
#68687 = VERTEX_POINT ( 'NONE', #87801 ) ;
#68688 = VECTOR ( 'NONE', #88353, 1000.000000000000000 ) ;
#68689 = CARTESIAN_POINT ( 'NONE',  ( -12.69999999999998153, 0.000000000000000000, 0.000000000000000000 ) ) ;
#68690 = CARTESIAN_POINT ( 'NONE',  ( -32.67183060077624646, -12.74070752338415424, 4.000000000000000000 ) ) ;
#68691 = CARTESIAN_POINT ( 'NONE',  ( 15.75000000000000000, -7.464222240803106570E-16, -6.094999999999989981 ) ) ;
#68692 = CARTESIAN_POINT ( 'NONE',  ( -60.48921356237309510, -27.52281430457097500, 5.000000000000000000 ) ) ;
#68693 =( NAMED_UNIT ( * ) PLANE_ANGLE_UNIT ( ) SI_UNIT ( $, .RADIAN. ) );
#68694 = DIRECTION ( 'NONE',  ( -0.7071067811865486830, -0.7071067811865464625, 0.000000000000000000 ) ) ;
#68695 = ORIENTED_EDGE ( 'NONE', *, *, #117930, .F. ) ;
#68696 = DIRECTION ( 'NONE',  ( -0.7071067811865486830, -0.7071067811865464625, 0.000000000000000000 ) ) ;
#68697 = ORIENTED_EDGE ( 'NONE', *, *, #555, .T. ) ;
#68698 = CIRCLE ( 'NONE', #87201, 2.500000000000000444 ) ;
#68699 = CARTESIAN_POINT ( 'NONE',  ( 97.56293019189810423, 1.637169565754157174, 6.110000000000002984 ) ) ;
#68700 = DIRECTION ( 'NONE',  ( -0.7071067811865486830, -0.7071067811865464625, 0.000000000000000000 ) ) ;
#68701 = LINE ( 'NONE', #68019, #134317 ) ;
#68702 = DIRECTION ( 'NONE',  ( -0.000000000000000000, -0.3543493200069152693, 0.9351131265310292928 ) ) ;
#68703 = ORIENTED_EDGE ( 'NONE', *, *, #106769, .T. ) ;
#68704 = CARTESIAN_POINT ( 'NONE',  ( 8.671830600776408104, 20.25929247661551713, 4.000000000000000000 ) ) ;
#68705 = CARTESIAN_POINT ( 'NONE',  ( -9.706792507240685097, 20.25929247661552068, 20.83292124670817103 ) ) ;
#68706 = DIRECTION ( 'NONE',  ( 0.7071067811865487940, -0.7071067811865463515, 0.000000000000000000 ) ) ;
#68707 = AXIS2_PLACEMENT_3D ( 'NONE', #77135, #74989, #43065 ) ;
#68708 = ORIENTED_EDGE ( 'NONE', *, *, #112878, .T. ) ;
#68709 = CARTESIAN_POINT ( 'NONE',  ( 24.70057660522904897, 5.105512181938189897, 4.576947331497495774 ) ) ;
#68710 = CARTESIAN_POINT ( 'NONE',  ( 19.05000000000000071, 3.174999999999997158, 5.000000000000000000 ) ) ;
#68712 = ORIENTED_EDGE ( 'NONE', *, *, #49062, .T. ) ;
#68711 = CARTESIAN_POINT ( 'NONE',  ( -34.92500000000001137, -1.298069433178978382, 4.500000000000000888 ) ) ;
#68713 = CARTESIAN_POINT ( 'NONE',  ( 18.95159235450331892, -3.851859888774471706E-31, 2.500000000000001332 ) ) ;
#68714 = DIRECTION ( 'NONE',  ( -0.7071067811865487940, 0.7071067811865463515, 0.000000000000000000 ) ) ;
#68715 = CARTESIAN_POINT ( 'NONE',  ( -1.180000000000000604, 9.043340090917736163, 10.00000000000000000 ) ) ;
#68716 = PLANE ( 'NONE',  #91873 ) ;
#68717 = VECTOR ( 'NONE', #19329, 1000.000000000000000 ) ;
#68718 = CYLINDRICAL_SURFACE ( 'NONE', #90968, 2.500000000000000000 ) ;
#68719 = VECTOR ( 'NONE', #29658, 1000.000000000000000 ) ;
#68720 = VERTEX_POINT ( 'NONE', #108100 ) ;
#68721 = ORIENTED_EDGE ( 'NONE', *, *, #9052, .F. ) ;
#68722 = ORIENTED_EDGE ( 'NONE', *, *, #22162, .F. ) ;
#68724 = EDGE_CURVE ( 'NONE', #38512, #1490, #119006, .T. ) ;
#68723 = CIRCLE ( 'NONE', #6141, 1.898649999999994842 ) ;
#68725 = CARTESIAN_POINT ( 'NONE',  ( 84.14626352523144703, -4.472830434245840259, 4.472830434245839371 ) ) ;
#68726 = VERTEX_POINT ( 'NONE', #97218 ) ;
#68727 = ADVANCED_FACE ( 'NONE', ( #142215 ), #64629, .F. ) ;
#68728 = ADVANCED_FACE ( 'NONE', ( #112422 ), #25385, .T. ) ;
#68729 = CARTESIAN_POINT ( 'NONE',  ( 15.83159235450332147, 3.061616997868380183E-16, -2.500000000000001332 ) ) ;
#68730 = CARTESIAN_POINT ( 'NONE',  ( -34.92500000000001137, 10.70193056682090749, 4.500000000000000888 ) ) ;
#68731 = EDGE_CURVE ( 'NONE', #41471, #86576, #133466, .T. ) ;
#68733 = AXIS2_PLACEMENT_3D ( 'NONE', #123248, #68182, #101460 ) ;
#68732 = CARTESIAN_POINT ( 'NONE',  ( -1.180000000000000604, 10.00000000000000178, 10.00000000000000000 ) ) ;
#68734 = LINE ( 'NONE', #37524, #100967 ) ;
#68735 = ORIENTED_EDGE ( 'NONE', *, *, #121360, .T. ) ;
#68736 = ADVANCED_FACE ( 'NONE', ( #124016 ), #100824, .F. ) ;
#68737 = DIRECTION ( 'NONE',  ( -0.000000000000000000, 0.3543493200069152138, -0.9351131265310292928 ) ) ;
#68738 = FACE_OUTER_BOUND ( 'NONE', #92150, .T. ) ;
#68739 = CARTESIAN_POINT ( 'NONE',  ( 17.22560490425083657, 3.821174125832445049E-16, 0.000000000000000000 ) ) ;
#68740 = CARTESIAN_POINT ( 'NONE',  ( 80.99543019189810877, 5.291415217122916737, 3.055000000000001936 ) ) ;
#68741 = ORIENTED_EDGE ( 'NONE', *, *, #72003, .F. ) ;
#68742 = ADVANCED_FACE ( 'NONE', ( #57352 ), #15212, .F. ) ;
#68743 = DIRECTION ( 'NONE',  ( 0.000000000000000000, 0.000000000000000000, -1.000000000000000000 ) ) ;
#68744 = LINE ( 'NONE', #102790, #44667 ) ;
#68745 = ORIENTED_EDGE ( 'NONE', *, *, #97260, .T. ) ;
#68746 = ORIENTED_EDGE ( 'NONE', *, *, #138255, .F. ) ;
#68747 = ADVANCED_FACE ( 'NONE', ( #34155 ), #773, .F. ) ;
#68748 = DIRECTION ( 'NONE',  ( 1.000000000000000000, 0.000000000000000000, 0.000000000000000000 ) ) ;
#68749 = ADVANCED_FACE ( 'NONE', ( #134178 ), #111707, .T. ) ;
#68750 = CARTESIAN_POINT ( 'NONE',  ( 106.0000000000000000, 0.000000000000000000, -7.950000000000000178 ) ) ;
#68751 = CARTESIAN_POINT ( 'NONE',  ( 22.23373647476855197, 5.808823158059035485, 5.808823158059032821 ) ) ;
#68752 = CARTESIAN_POINT ( 'NONE',  ( 24.18398860626899705, 28.73617430169804265, 5.000000000000000000 ) ) ;
#68753 = CARTESIAN_POINT ( 'NONE',  ( -18.18398860626898994, 28.73617430169800002, 5.000000000000000000 ) ) ;
#68754 = EDGE_CURVE ( 'NONE', #92427, #114903, #3613, .T. ) ;
#68755 = PLANE ( 'NONE',  #18679 ) ;
#68756 = DIRECTION ( 'NONE',  ( -1.000000000000000000, -0.000000000000000000, -0.000000000000000000 ) ) ;
#68757 = SURFACE_STYLE_USAGE ( .BOTH. , #35429 ) ;
#68758 = VECTOR ( 'NONE', #75233, 1000.000000000000227 ) ;
#68759 = ORIENTED_EDGE ( 'NONE', *, *, #7980, .F. ) ;
#68760 = ORIENTED_EDGE ( 'NONE', *, *, #83055, .T. ) ;
#68761 = CARTESIAN_POINT ( 'NONE',  ( -6.707106781186496391, 14.25929247661557575, 5.000000000000000000 ) ) ;
#68762 = EDGE_LOOP ( 'NONE', ( #89848, #41786, #12424, #8347 ) ) ;
#68763 = ORIENTED_EDGE ( 'NONE', *, *, #68310, .T. ) ;
#68764 = AXIS2_PLACEMENT_3D ( 'NONE', #40713, #16048, #92937 ) ;
#68765 = DIRECTION ( 'NONE',  ( -0.7071067811865487940, 0.7071067811865463515, 0.000000000000000000 ) ) ;
#68766 = ORIENTED_EDGE ( 'NONE', *, *, #132412, .F. ) ;
#68767 = CARTESIAN_POINT ( 'NONE',  ( 56.22502705046289151, 5.819803920172573974, -5.819803920172573086 ) ) ;
#68768 = CARTESIAN_POINT ( 'NONE',  ( 24.50000000000000000, 0.000000000000000000, 6.094999999999989981 ) ) ;
#68769 = B_SPLINE_CURVE_WITH_KNOTS ( 'NONE', 3,
 ( #30940, #120027, #87456, #76597 ),
 .UNSPECIFIED., .F., .F.,
 ( 4, 4 ),
 ( 0.008853860144884175692, 0.009403245473020184833 ),
 .UNSPECIFIED. ) ;
#68770 = CARTESIAN_POINT ( 'NONE',  ( 25.58990935480152729, 9.759292476615618384, 11.28811694763784779 ) ) ;
#68771 = EDGE_CURVE ( 'NONE', #79129, #36317, #122557, .T. ) ;
#68772 = VECTOR ( 'NONE', #49449, 999.9999999999998863 ) ;
#68773 = PLANE ( 'NONE',  #34635 ) ;
#68774 = CARTESIAN_POINT ( 'NONE',  ( 21.18398860626899349, 28.73617430169802134, 5.000000000000000000 ) ) ;
#68775 = VERTEX_POINT ( 'NONE', #13780 ) ;
#68776 = DIRECTION ( 'NONE',  ( 0.3543493200069162685, -0.000000000000000000, -0.9351131265310288487 ) ) ;
#68778 = VERTEX_POINT ( 'NONE', #2928 ) ;
#68777 = VECTOR ( 'NONE', #89088, 1000.000000000000000 ) ;
#68779 = CARTESIAN_POINT ( 'NONE',  ( 0.000000000000000000, 0.000000000000000000, 5.000000000000000000 ) ) ;
#68780 = ORIENTED_EDGE ( 'NONE', *, *, #113374, .T. ) ;
#68781 = DIRECTION ( 'NONE',  ( 0.000000000000000000, 0.000000000000000000, 1.000000000000000000 ) ) ;
#68782 = EDGE_LOOP ( 'NONE', ( #24179, #67231, #6865, #99923 ) ) ;
#68783 = DIRECTION ( 'NONE',  ( 0.000000000000000000, -1.000000000000000000, 0.000000000000000000 ) ) ;
#68784 = ORIENTED_EDGE ( 'NONE', *, *, #38911, .T. ) ;
#68785 = ORIENTED_EDGE ( 'NONE', *, *, #46669, .F. ) ;
#68786 = ORIENTED_EDGE ( 'NONE', *, *, #86774, .F. ) ;
#68787 = EDGE_CURVE ( 'NONE', #122293, #90522, #81239, .T. ) ;
#68788 = COLOUR_RGB ( '', 0.72549020, 0.75294118, 0.79215686) ;
#68789 = DIRECTION ( 'NONE',  ( -0.7071067811865486830, -0.7071067811865464625, 0.000000000000000000 ) ) ;
#68790 = CARTESIAN_POINT ( 'NONE',  ( -2.999999999999964473, 11.58746187583912324, 4.000000000000000000 ) ) ;
#68791 =( NAMED_UNIT ( * ) SI_UNIT ( $, .STERADIAN. ) SOLID_ANGLE_UNIT ( ) );
#68792 = CARTESIAN_POINT ( 'NONE',  ( 11.20710678118646619, -8.240707523384200428, 5.000000000000000000 ) ) ;
#68793 = AXIS2_PLACEMENT_3D ( 'NONE', #117725, #130078, #140240 ) ;
#68794 = CARTESIAN_POINT ( 'NONE',  ( 118.1254301918981184, 5.291415217122919401, 3.055000000000002824 ) ) ;
#68795 = DIRECTION ( 'NONE',  ( -1.000000000000000000, -1.224606353822377258E-16, -0.000000000000000000 ) ) ;
#68796 = EDGE_CURVE ( 'NONE', #108299, #110346, #124718, .T. ) ;
#68797 = DIRECTION ( 'NONE',  ( 0.6830127018922180770, -0.6830127018922204085, -0.2588190451025213501 ) ) ;
#68798 = DIRECTION ( 'NONE',  ( -0.000000000000000000, 1.000000000000000000, -0.000000000000000000 ) ) ;
#68799 = CARTESIAN_POINT ( 'NONE',  ( -17.48334561358942807, 22.22500000000000142, 4.500000000000000888 ) ) ;
#68800 = CYLINDRICAL_SURFACE ( 'NONE', #41271, 0.5000000000000000000 ) ;
#68801 = VERTEX_POINT ( 'NONE', #123320 ) ;
#68802 = CARTESIAN_POINT ( 'NONE',  ( 5.281315875828549444, -2.500000000000000444, 3.061616997868384127E-16 ) ) ;
#68803 = CARTESIAN_POINT ( 'NONE',  ( -15.29974487139158867, -27.71228299555216879, 4.000000000000000000 ) ) ;
#68804 = VECTOR ( 'NONE', #138833, 1000.000000000000000 ) ;
#68805 = EDGE_CURVE ( 'NONE', #109084, #3210, #58079, .T. ) ;
#68806 = VERTEX_POINT ( 'NONE', #79840 ) ;
#68807 = ORIENTED_EDGE ( 'NONE', *, *, #119367, .T. ) ;
#68808 = CARTESIAN_POINT ( 'NONE',  ( -83.99451991528748351, 28.92564299267996830, 4.000000000000000000 ) ) ;
#68809 = VERTEX_POINT ( 'NONE', #24683 ) ;
#68810 = DIRECTION ( 'NONE',  ( 1.301042606982605074E-16, -1.000000000000000000, 0.000000000000000000 ) ) ;
#68811 = CARTESIAN_POINT ( 'NONE',  ( 32.99999999999977263, -15.41253812416059787, 4.000000000000000000 ) ) ;
#68812 = AXIS2_PLACEMENT_3D ( 'NONE', #133633, #89403, #115210 ) ;
#68813 = EDGE_CURVE ( 'NONE', #86982, #141725, #68942, .T. ) ;
#68814 = PLANE ( 'NONE',  #27782 ) ;
#68815 = CARTESIAN_POINT ( 'NONE',  ( 4.499999999999972466, -2.568876922607793212, 4.000000000000000000 ) ) ;
#68816 = ORIENTED_EDGE ( 'NONE', *, *, #130097, .F. ) ;
#68817 = SURFACE_STYLE_USAGE ( .BOTH. , #26005 ) ;
#68818 = ORIENTED_EDGE ( 'NONE', *, *, #87884, .F. ) ;
#68819 = VECTOR ( 'NONE', #112758, 999.9999999999998863 ) ;
#68822 = AXIS2_PLACEMENT_3D ( 'NONE', #81368, #2309, #111077 ) ;
#68821 = CARTESIAN_POINT ( 'NONE',  ( -36.18398860626899705, 28.73617430169812437, 5.000000000000000000 ) ) ;
#68820 = VECTOR ( 'NONE', #52499, 1000.000000000000000 ) ;
#68823 = AXIS2_PLACEMENT_3D ( 'NONE', #117520, #18194, #108062 ) ;
#68824 = CARTESIAN_POINT ( 'NONE',  ( 32.73373647476854842, 5.808823158059036373, 5.808823158059032821 ) ) ;
#68825 = ORIENTED_EDGE ( 'NONE', *, *, #21075, .F. ) ;
#68826 = FACE_OUTER_BOUND ( 'NONE', #78333, .T. ) ;
#68827 = PLANE ( 'NONE',  #53555 ) ;
#68828 = ORIENTED_EDGE ( 'NONE', *, *, #1970, .F. ) ;
#68829 = VECTOR ( 'NONE', #111479, 999.9999999999998863 ) ;
#68830 = ORIENTED_EDGE ( 'NONE', *, *, #15119, .F. ) ;
#68831 = ORIENTED_EDGE ( 'NONE', *, *, #36153, .T. ) ;
#68832 = CARTESIAN_POINT ( 'NONE',  ( -42.48921356237308800, -27.52281430457085065, 5.000000000000000000 ) ) ;
#68833 = CARTESIAN_POINT ( 'NONE',  ( -0.1839886062690032631, 28.73617430169787568, 5.000000000000000000 ) ) ;
#68834 = AXIS2_PLACEMENT_3D ( 'NONE', #71222, #16055, #69077 ) ;
#68835 = CARTESIAN_POINT ( 'NONE',  ( -34.49999999999975842, -12.66682484999669178, -0.6294897503864747002 ) ) ;
#68836 = CARTESIAN_POINT ( 'NONE',  ( 18.18398860626898994, 28.73617430169800002, 5.000000000000000000 ) ) ;
#68837 = ORIENTED_EDGE ( 'NONE', *, *, #6210, .F. ) ;
#68838 = CARTESIAN_POINT ( 'NONE',  ( -9.328169399223462221, -6.740707523384216415, 4.000000000000000000 ) ) ;
#68839 = EDGE_CURVE ( 'NONE', #40167, #31872, #113115, .T. ) ;
#68840 = CARTESIAN_POINT ( 'NONE',  ( 33.18398860626899705, 28.73617430169810305, 5.000000000000000000 ) ) ;
#68841 = DIRECTION ( 'NONE',  ( -0.000000000000000000, -0.3543493200069152693, 0.9351131265310292928 ) ) ;
#68842 = VERTEX_POINT ( 'NONE', #102278 ) ;
#68843 = CARTESIAN_POINT ( 'NONE',  ( 3.328169399223507519, 8.259292476615634371, 4.000000000000000000 ) ) ;
#68844 = EDGE_LOOP ( 'NONE', ( #12629, #135500, #47244, #54331 ) ) ;
#68845 = ADVANCED_FACE ( 'NONE', ( #36293 ), #80522, .T. ) ;
#68847 = VERTEX_POINT ( 'NONE', #47906 ) ;
#68846 = LINE ( 'NONE', #126069, #88020 ) ;
#68848 = VERTEX_POINT ( 'NONE', #73213 ) ;
#68849 = EDGE_CURVE ( 'NONE', #23467, #14718, #126159, .T. ) ;
#68850 = DIRECTION ( 'NONE',  ( -0.7071067811865487940, 0.7071067811865463515, 0.000000000000000000 ) ) ;
#68852 = VECTOR ( 'NONE', #109238, 1000.000000000000000 ) ;
#68851 = CARTESIAN_POINT ( 'NONE',  ( 34.45011844616453089, -20.99769585840584085, 5.000000000000000888 ) ) ;
#68853 = ORIENTED_EDGE ( 'NONE', *, *, #100926, .T. ) ;
#68854 = DIRECTION ( 'NONE',  ( 0.6830127018922181881, 0.6830127018922202975, -0.2588190451025214056 ) ) ;
#68855 = ORIENTED_EDGE ( 'NONE', *, *, #107350, .T. ) ;
#68856 =( BOUNDED_CURVE ( )  B_SPLINE_CURVE ( 3, ( #142552, #76595, #130251, #22158 ),
 .UNSPECIFIED., .F., .T. ) 
 B_SPLINE_CURVE_WITH_KNOTS ( ( 4, 4 ),
 ( 5.584306267627116682, 5.657315652343092971 ),
 .UNSPECIFIED. ) 
 CURVE ( )  GEOMETRIC_REPRESENTATION_ITEM ( )  RATIONAL_B_SPLINE_CURVE ( ( 1.000000000000000000, 0.9995558518042845231, 0.9995558518042845231, 1.000000000000000000 ) ) 
 REPRESENTATION_ITEM ( '' )  );
#68857 = LINE ( 'NONE', #89162, #5829 ) ;
#68858 = PLANE ( 'NONE',  #83329 ) ;
#68859 = VECTOR ( 'NONE', #95542, 1000.000000000000000 ) ;
#68860 = DIRECTION ( 'NONE',  ( 0.7071067811865487940, -0.7071067811865463515, 0.000000000000000000 ) ) ;
#68861 = CARTESIAN_POINT ( 'NONE',  ( -16.17183060077636370, -20.24070752338408141, 4.000000000000000000 ) ) ;
#68862 = CARTESIAN_POINT ( 'NONE',  ( -17.81601139373099940, 28.73617430169775133, 5.000000000000000000 ) ) ;
#68863 = CARTESIAN_POINT ( 'NONE',  ( -34.92500000000001137, 0.7592924766157104211, 4.255531930566247567 ) ) ;
#68864 = DIRECTION ( 'NONE',  ( 0.7071067811865487940, 0.7071067811865463515, 0.000000000000000000 ) ) ;
#68865 = DIRECTION ( 'NONE',  ( -0.000000000000000000, 0.000000000000000000, 1.000000000000000000 ) ) ;
#68866 = CARTESIAN_POINT ( 'NONE',  ( 17.47873647476855652, -5.808823158059033709, 5.808823158059035485 ) ) ;
#68868 = AXIS2_PLACEMENT_3D ( 'NONE', #570, #77471, #22305 ) ;
#68867 = CARTESIAN_POINT ( 'NONE',  ( 1.728736474768552522, 5.808823158059031044, -5.808823158059037262 ) ) ;
#68869 = DIRECTION ( 'NONE',  ( 0.7071067811865486830, -0.7071067811865464625, -0.000000000000000000 ) ) ;
#68870 = PLANE ( 'NONE',  #2652 ) ;
#68871 = DIRECTION ( 'NONE',  ( 1.000000000000000000, 0.000000000000000000, 0.000000000000000000 ) ) ;
#68872 = ORIENTED_EDGE ( 'NONE', *, *, #92157, .T. ) ;
#68873 = EDGE_CURVE ( 'NONE', #129051, #124700, #39882, .T. ) ;
#68874 = VERTEX_POINT ( 'NONE', #115222 ) ;
#68875 = CARTESIAN_POINT ( 'NONE',  ( 90.10416666666665719, 2.130196079827422206, 7.950000000000001954 ) ) ;
#68876 = ORIENTED_EDGE ( 'NONE', *, *, #118641, .F. ) ;
#68877 = ORIENTED_EDGE ( 'NONE', *, *, #56019, .F. ) ;
#68878 = ORIENTED_EDGE ( 'NONE', *, *, #82185, .T. ) ;
#68879 = VECTOR ( 'NONE', #2687, 1000.000000000000000 ) ;
#68880 = LINE ( 'NONE', #56602, #36465 ) ;
#68881 = CARTESIAN_POINT ( 'NONE',  ( 69.48921356237309510, -27.52281430457103895, 5.000000000000000000 ) ) ;
#68882 = CARTESIAN_POINT ( 'NONE',  ( 66.29974487139159578, -27.71228299555252406, 4.000000000000000000 ) ) ;
#68883 = VERTEX_POINT ( 'NONE', #104375 ) ;
#68884 = DIRECTION ( 'NONE',  ( 0.7071067811865486830, -0.7071067811865464625, -0.000000000000000000 ) ) ;
#68885 = FACE_OUTER_BOUND ( 'NONE', #13163, .T. ) ;
#68886 = PLANE ( 'NONE',  #118103 ) ;
#68887 = LINE ( 'NONE', #113060, #139239 ) ;
#68888 = CARTESIAN_POINT ( 'NONE',  ( 127.8079301918981230, -6.109999999999998543, 1.637169565754158507 ) ) ;
#68889 = DIRECTION ( 'NONE',  ( 0.000000000000000000, -1.000000000000000000, 0.000000000000000000 ) ) ;
#68890 = DIRECTION ( 'NONE',  ( 0.7071067811865487940, 0.7071067811865463515, 0.000000000000000000 ) ) ;
#68891 = CARTESIAN_POINT ( 'NONE',  ( 34.45011844616451668, 22.22500000000000142, 4.231322045535989673 ) ) ;
#68892 = CARTESIAN_POINT ( 'NONE',  ( 24.96654721599509941, 3.964575861396866685, 4.000000000000000000 ) ) ;
#68893 = DIRECTION ( 'NONE',  ( 0.3543493200069162685, -0.000000000000000000, -0.9351131265310288487 ) ) ;
#68894 = DIRECTION ( 'NONE',  ( 0.000000000000000000, 0.000000000000000000, 1.000000000000000000 ) ) ;
#68895 = DIRECTION ( 'NONE',  ( 1.000000000000000000, 0.000000000000000000, 0.000000000000000000 ) ) ;
#68896 = ORIENTED_EDGE ( 'NONE', *, *, #58243, .F. ) ;
#68897 = ORIENTED_EDGE ( 'NONE', *, *, #85604, .F. ) ;
#68898 = EDGE_CURVE ( 'NONE', #123192, #46180, #117377, .T. ) ;
#68899 = CARTESIAN_POINT ( 'NONE',  ( 110.5420968585647756, 5.291415217122923842, -3.054999999999996163 ) ) ;
#68900 = AXIS2_PLACEMENT_3D ( 'NONE', #33638, #133648, #34325 ) ;
#68901 = PRESENTATION_LAYER_ASSIGNMENT (  '', '', ( #131377 ) ) ;
#68902 = ORIENTED_EDGE ( 'NONE', *, *, #19138, .T. ) ;
#68903 = EDGE_CURVE ( 'NONE', #83531, #131076, #26826, .T. ) ;
#68904 = CARTESIAN_POINT ( 'NONE',  ( -32.99999999999975842, 14.96639925780210767, 5.000000000000000000 ) ) ;
#68905 = FILL_AREA_STYLE_COLOUR ( '', #135952 ) ;
#68906 = EDGE_CURVE ( 'NONE', #126702, #44187, #128303, .T. ) ;
#68907 = EDGE_CURVE ( 'NONE', #80864, #121754, #47126, .T. ) ;
#68908 = DIRECTION ( 'NONE',  ( -0.6830127018922180770, -0.6830127018922204085, -0.2588190451025213501 ) ) ;
#68909 = CARTESIAN_POINT ( 'NONE',  ( 30.18398860626900060, 28.73617430169808173, 5.000000000000000000 ) ) ;
#68910 = VECTOR ( 'NONE', #140861, 1000.000000000000000 ) ;
#68911 = CARTESIAN_POINT ( 'NONE',  ( 112.2037635252314516, 6.109999999999998543, 1.122388791418548911E-15 ) ) ;
#68912 = EDGE_LOOP ( 'NONE', ( #69013, #82707, #16194, #46473 ) ) ;
#68913 = EDGE_LOOP ( 'NONE', ( #141334, #142839, #127361, #25326 ) ) ;
#68914 = DIRECTION ( 'NONE',  ( 0.7071067811865487940, 0.7071067811865463515, 0.000000000000000000 ) ) ;
#68915 = CARTESIAN_POINT ( 'NONE',  ( 27.48921356237309155, -27.52281430457074762, 5.000000000000000000 ) ) ;
#68916 = AXIS2_PLACEMENT_3D ( 'NONE', #110813, #118862, #65234 ) ;
#68917 = EDGE_LOOP ( 'NONE', ( #67352, #106791, #45737, #73268 ) ) ;
#68918 = ORIENTED_EDGE ( 'NONE', *, *, #138746, .F. ) ;
#68919 = AXIS2_PLACEMENT_3D ( 'NONE', #14159, #70026, #39519 ) ;
#68920 = EDGE_CURVE ( 'NONE', #56677, #76836, #84782, .T. ) ;
#68921 = EDGE_LOOP ( 'NONE', ( #89340, #59188, #8634, #28109 ) ) ;
#68922 = CARTESIAN_POINT ( 'NONE',  ( 25.08376352523143638, -6.110000000000001208, -3.741295971395164515E-16 ) ) ;
#68923 = ADVANCED_FACE ( 'NONE', ( #7180 ), #50029, .F. ) ;
#68924 = CARTESIAN_POINT ( 'NONE',  ( 25.39999999999999858, -14.29000000000013593, 12.69999999999954632 ) ) ;
#68925 = VECTOR ( 'NONE', #17387, 1000.000000000000227 ) ;
#68926 = AXIS2_PLACEMENT_3D ( 'NONE', #7383, #130642, #97231 ) ;
#68927 = EDGE_CURVE ( 'NONE', #93801, #43398, #118082, .T. ) ;
#68928 = AXIS2_PLACEMENT_3D ( 'NONE', #4819, #17183, #73701 ) ;
#68929 = CARTESIAN_POINT ( 'NONE',  ( 32.57876352523145158, -7.482591942790325086E-16, 6.109999999999998543 ) ) ;
#68930 = ORIENTED_EDGE ( 'NONE', *, *, #36098, .F. ) ;
#68931 = VERTEX_POINT ( 'NONE', #18792 ) ;
#68932 = CARTESIAN_POINT ( 'NONE',  ( -29.20710678118633297, 0.7592924766157086447, 5.000000000000000000 ) ) ;
#68933 = VERTEX_POINT ( 'NONE', #37730 ) ;
#68934 = VERTEX_POINT ( 'NONE', #115956 ) ;
#68935 = AXIS2_PLACEMENT_3D ( 'NONE', #130599, #25185, #68048 ) ;
#68936 = ADVANCED_FACE ( 'NONE', ( #16660 ), #60943, .F. ) ;
#68937 = VERTEX_POINT ( 'NONE', #138458 ) ;
#68938 = FACE_OUTER_BOUND ( 'NONE', #27705, .T. ) ;
#68939 =( LENGTH_UNIT ( ) NAMED_UNIT ( * ) SI_UNIT ( .MILLI., .METRE. ) );
#68940 = LINE ( 'NONE', #89239, #30281 ) ;
#68941 = ORIENTED_EDGE ( 'NONE', *, *, #42696, .F. ) ;
#68942 = LINE ( 'NONE', #91400, #131701 ) ;
#68943 = EDGE_CURVE ( 'NONE', #68281, #87685, #39147, .T. ) ;
#68944 = DIRECTION ( 'NONE',  ( 0.7071067811865486830, -0.7071067811865464625, -0.000000000000000000 ) ) ;
#68945 = SURFACE_SIDE_STYLE ('',( #36296 ) ) ;
#68946 = FACE_BOUND ( 'NONE', #48462, .T. ) ;
#68947 = ORIENTED_EDGE ( 'NONE', *, *, #138589, .F. ) ;
#68948 = CARTESIAN_POINT ( 'NONE',  ( 64.24586038379621300, 3.974999999999996980, 6.884901960086287964 ) ) ;
#68949 = LINE ( 'NONE', #2938, #131805 ) ;
#68950 = DIRECTION ( 'NONE',  ( -0.3543493200069162685, -0.000000000000000000, -0.9351131265310288487 ) ) ;
#68951 = EDGE_LOOP ( 'NONE', ( #88743, #39471, #120699 ) ) ;
#68952 = EDGE_CURVE ( 'NONE', #53759, #112632, #4290, .T. ) ;
#68953 = CARTESIAN_POINT ( 'NONE',  ( 36.18398860626899705, 28.73617430169812437, 5.000000000000000000 ) ) ;
#68954 = ORIENTED_EDGE ( 'NONE', *, *, #21440, .F. ) ;
#68956 = EDGE_CURVE ( 'NONE', #12982, #136524, #62340, .T. ) ;
#68955 = VECTOR ( 'NONE', #112643, 1000.000000000000000 ) ;
#68957 = VERTEX_POINT ( 'NONE', #17377 ) ;
#68958 = EDGE_LOOP ( 'NONE', ( #102530, #76058, #18910, #41805 ) ) ;
#68959 = EDGE_CURVE ( 'NONE', #2613, #7898, #41282, .T. ) ;
#68960 = CARTESIAN_POINT ( 'NONE',  ( 41.03709685856478728, -3.054999999999998828, -5.291415217122919401 ) ) ;
#68961 = CONICAL_SURFACE ( 'NONE', #73503, 2.055000000000001048, 0.9599310885968758145 ) ;
#68962 = ORIENTED_EDGE ( 'NONE', *, *, #66290, .T. ) ;
#68963 = FACE_OUTER_BOUND ( 'NONE', #37213, .T. ) ;
#68964 = CARTESIAN_POINT ( 'NONE',  ( 23.24139925780185223, 21.72500000000000853, 5.000000000000000000 ) ) ;
#68965 = ORIENTED_EDGE ( 'NONE', *, *, #96369, .T. ) ;
#68966 = SURFACE_SIDE_STYLE ('',( #26852 ) ) ;
#68967 = LINE ( 'NONE', #104407, #141768 ) ;
#68968 = DIRECTION ( 'NONE',  ( -3.115803279706882722E-16, 1.000000000000000000, 0.000000000000000000 ) ) ;
#68969 = CARTESIAN_POINT ( 'NONE',  ( 7.371765549556104524, -8.240707523384203981, 11.38925528200750925 ) ) ;
#68970 =( NAMED_UNIT ( * ) PLANE_ANGLE_UNIT ( ) SI_UNIT ( $, .RADIAN. ) );
#68971 = DIRECTION ( 'NONE',  ( 0.000000000000000000, 0.000000000000000000, -1.000000000000000000 ) ) ;
#68972 = ORIENTED_EDGE ( 'NONE', *, *, #98631, .F. ) ;
#68973 = ORIENTED_EDGE ( 'NONE', *, *, #121577, .T. ) ;
#68974 = EDGE_LOOP ( 'NONE', ( #110224, #38484, #79919, #43598 ) ) ;
#68975 = VERTEX_POINT ( 'NONE', #108635 ) ;
#68976 = ORIENTED_EDGE ( 'NONE', *, *, #124388, .T. ) ;
#68977 = ORIENTED_EDGE ( 'NONE', *, *, #26518, .F. ) ;
#68978 = CARTESIAN_POINT ( 'NONE',  ( 69.48921356237309510, -27.52281430457103895, 5.000000000000000000 ) ) ;
#68979 = DIRECTION ( 'NONE',  ( -0.000000000000000000, -0.3543493200069152693, 0.9351131265310292928 ) ) ;
#68980 = ORIENTED_EDGE ( 'NONE', *, *, #115252, .F. ) ;
#68981 = DIRECTION ( 'NONE',  ( -0.000000000000000000, 0.000000000000000000, 1.000000000000000000 ) ) ;
#68982 = ORIENTED_EDGE ( 'NONE', *, *, #65669, .F. ) ;
#68983 = CARTESIAN_POINT ( 'NONE',  ( 28.06706980810189123, 2.126176841940952134, -7.934999999999993392 ) ) ;
#68984 = CARTESIAN_POINT ( 'NONE',  ( 0.06706980810188606368, 2.126176841940952134, -7.934999999999993392 ) ) ;
#68985 = VERTEX_POINT ( 'NONE', #76795 ) ;
#68986 = CARTESIAN_POINT ( 'NONE',  ( 111.0370968585647944, -3.054999999999999272, -5.291415217122919401 ) ) ;
#68987 = VECTOR ( 'NONE', #76441, 1000.000000000000000 ) ;
#68988 = PLANE ( 'NONE',  #97624 ) ;
#68989 = DIRECTION ( 'NONE',  ( 0.7071067811865486830, -0.7071067811865464625, -0.000000000000000000 ) ) ;
#68990 = EDGE_CURVE ( 'NONE', #137546, #89076, #98509, .T. ) ;
#68991 = ORIENTED_EDGE ( 'NONE', *, *, #76840, .F. ) ;
#68992 = CARTESIAN_POINT ( 'NONE',  ( 17.99999999999987210, 10.93112307739206912, 4.000000000000000000 ) ) ;
#68994 = VERTEX_POINT ( 'NONE', #9309 ) ;
#68993 = LINE ( 'NONE', #2248, #49251 ) ;
#68995 = DIRECTION ( 'NONE',  ( 0.7071067811865486830, -0.7071067811865464625, -0.000000000000000000 ) ) ;
#68996 = CARTESIAN_POINT ( 'NONE',  ( 22.49999999999984013, 10.08746187583914633, 4.000000000000000000 ) ) ;
#68997 = CARTESIAN_POINT ( 'NONE',  ( 15.48921356237309510, -27.52281430457066236, 5.000000000000000000 ) ) ;
#68998 = DIRECTION ( 'NONE',  ( 0.000000000000000000, 0.000000000000000000, 1.000000000000000000 ) ) ;
#68999 = DIRECTION ( 'NONE',  ( -0.000000000000000000, -0.3543493200069153248, 0.9351131265310292928 ) ) ;
#69000 = DIRECTION ( 'NONE',  ( 0.6830127018922180770, -0.6830127018922204085, -0.2588190451025213501 ) ) ;
#69001 = VERTEX_POINT ( 'NONE', #97037 ) ;
#69002 = DIRECTION ( 'NONE',  ( 0.000000000000000000, -1.000000000000000000, 0.000000000000000000 ) ) ;
#69003 = VECTOR ( 'NONE', #3052, 1000.000000000000000 ) ;
#69004 = LINE ( 'NONE', #113182, #58158 ) ;
#69005 = DIRECTION ( 'NONE',  ( 0.7071067811865487940, -0.7071067811865463515, 0.000000000000000000 ) ) ;
#69006 = ORIENTED_EDGE ( 'NONE', *, *, #42424, .T. ) ;
#69007 = VECTOR ( 'NONE', #71468, 1000.000000000000000 ) ;
#69008 = LINE ( 'NONE', #15990, #111803 ) ;
#69009 = ORIENTED_EDGE ( 'NONE', *, *, #137421, .F. ) ;
#69010 = VECTOR ( 'NONE', #24871, 1000.000000000000000 ) ;
#69011 = EDGE_CURVE ( 'NONE', #135494, #141475, #99194, .T. ) ;
#69013 = ORIENTED_EDGE ( 'NONE', *, *, #85182, .T. ) ;
#69012 = PLANE ( 'NONE',  #101881 ) ;
#69014 =( REPRESENTATION_RELATIONSHIP ('NONE','NONE', #69070, #428 ) REPRESENTATION_RELATIONSHIP_WITH_TRANSFORMATION ( #41629 )SHAPE_REPRESENTATION_RELATIONSHIP( ) );
#69016 = ORIENTED_EDGE ( 'NONE', *, *, #22758, .F. ) ;
#69015 = EDGE_CURVE ( 'NONE', #106679, #64810, #42006, .T. ) ;
#69017 = CARTESIAN_POINT ( 'NONE',  ( 8.671830600776416986, -3.740707523384241728, 4.000000000000000000 ) ) ;
#69018 = LINE ( 'NONE', #12458, #27379 ) ;
#69019 = AXIS2_PLACEMENT_3D ( 'NONE', #82169, #126345, #90146 ) ;
#69020 = ORIENTED_EDGE ( 'NONE', *, *, #56068, .F. ) ;
#69021 = VECTOR ( 'NONE', #56505, 1000.000000000000000 ) ;
#69022 = ORIENTED_EDGE ( 'NONE', *, *, #90339, .T. ) ;
#69023 = ADVANCED_FACE ( 'NONE', ( #143434 ), #18233, .T. ) ;
#69024 = LINE ( 'NONE', #113203, #51235 ) ;
#69025 = CARTESIAN_POINT ( 'NONE',  ( 33.18398860626899705, 28.73617430169810305, 5.000000000000000000 ) ) ;
#69026 = LINE ( 'NONE', #113205, #95668 ) ;
#69027 = CARTESIAN_POINT ( 'NONE',  ( 2.671830600776463172, 8.259292476615646805, 4.000000000000000000 ) ) ;
#69028 = CARTESIAN_POINT ( 'NONE',  ( 126.2426566364622005, -7.159809133051783014, 0.8799046258456960645 ) ) ;
#69029 = CARTESIAN_POINT ( 'NONE',  ( 28.66252705046289151, 7.949999999999998401, 1.460391307983218338E-15 ) ) ;
#69030 = LINE ( 'NONE', #27632, #43068 ) ;
#69031 = ORIENTED_EDGE ( 'NONE', *, *, #22116, .F. ) ;
#69032 = EDGE_CURVE ( 'NONE', #25524, #42897, #63764, .T. ) ;
#69033 = VERTEX_POINT ( 'NONE', #109386 ) ;
#69034 = ORIENTED_EDGE ( 'NONE', *, *, #121692, .T. ) ;
#69035 = CARTESIAN_POINT ( 'NONE',  ( 121.0208333333333144, 7.949999999999999289, 2.130196079827431532 ) ) ;
#69036 = VERTEX_POINT ( 'NONE', #140574 ) ;
#69037 = ORIENTED_EDGE ( 'NONE', *, *, #25832, .T. ) ;
#69038 = ORIENTED_EDGE ( 'NONE', *, *, #137910, .F. ) ;
#69039 = CARTESIAN_POINT ( 'NONE',  ( 0.2751413021719010255, -7.484932044345631752, 2.345161579649363670 ) ) ;
#69040 = CARTESIAN_POINT ( 'NONE',  ( -48.18398860626899705, 28.73617430169820608, 5.000000000000000000 ) ) ;
#69041 = EDGE_CURVE ( 'NONE', #79941, #102767, #131866, .T. ) ;
#69042 = ORIENTED_EDGE ( 'NONE', *, *, #37918, .F. ) ;
#69043 = DIRECTION ( 'NONE',  ( 0.000000000000000000, 1.000000000000000000, 0.000000000000000000 ) ) ;
#69045 = PRESENTATION_LAYER_ASSIGNMENT (  '', '', ( #8833 ) ) ;
#69044 = CARTESIAN_POINT ( 'NONE',  ( 34.49999999999976552, -9.462702396500981550, -9.474982329943593129 ) ) ;
#69046 = PLANE ( 'NONE',  #32414 ) ;
#69047 = FACE_OUTER_BOUND ( 'NONE', #36442, .T. ) ;
#69048 = CARTESIAN_POINT ( 'NONE',  ( 118.4170968585647756, 3.054999999999998828, 5.291415217122922066 ) ) ;
#69049 = ORIENTED_EDGE ( 'NONE', *, *, #47036, .F. ) ;
#69050 = CARTESIAN_POINT ( 'NONE',  ( 23.55512991947088963, -0.7407075233842735917, 4.307968247157003994 ) ) ;
#69051 = CARTESIAN_POINT ( 'NONE',  ( -12.18398860626900060, 28.73617430169795739, 5.000000000000000000 ) ) ;
#69052 = AXIS2_PLACEMENT_3D ( 'NONE', #26853, #137781, #138486 ) ;
#69053 = CARTESIAN_POINT ( 'NONE',  ( 2.671830600776449405, -6.740707523384212863, 4.000000000000000000 ) ) ;
#69054 = CARTESIAN_POINT ( 'NONE',  ( 0.6154894137848396785, 7.435533126890685907, -0.9100370299028263110 ) ) ;
#69055 = FILL_AREA_STYLE ('',( #113965 ) ) ;
#69056 = CARTESIAN_POINT ( 'NONE',  ( -42.29974487139158157, -27.71228299555235708, 4.000000000000000000 ) ) ;
#69057 = LINE ( 'NONE', #134308, #138425 ) ;
#69058 = CARTESIAN_POINT ( 'NONE',  ( 43.68336038379622011, -2.130196079827426203, 7.949999999999997513 ) ) ;
#69059 = DIRECTION ( 'NONE',  ( -0.000000000000000000, 0.000000000000000000, 1.000000000000000000 ) ) ;
#69060 = DIRECTION ( 'NONE',  ( 0.6830127018922181881, 0.6830127018922202975, -0.2588190451025214056 ) ) ;
#69061 = ORIENTED_EDGE ( 'NONE', *, *, #137451, .T. ) ;
#69062 = ORIENTED_EDGE ( 'NONE', *, *, #55848, .T. ) ;
#69063 = CARTESIAN_POINT ( 'NONE',  ( 31.62500000000000000, -7.950000000000000178, -4.867971026610729436E-16 ) ) ;
#69064 = ORIENTED_EDGE ( 'NONE', *, *, #129795, .F. ) ;
#69065 = CARTESIAN_POINT ( 'NONE',  ( -24.48921356237309510, -27.52281430457072631, 5.000000000000000000 ) ) ;
#69066 = EDGE_CURVE ( 'NONE', #73197, #95699, #32554, .T. ) ;
#69067 = ORIENTED_EDGE ( 'NONE', *, *, #30106, .T. ) ;
#69068 = AXIS2_PLACEMENT_3D ( 'NONE', #60222, #5064, #83392 ) ;
#69069 = LINE ( 'NONE', #115364, #82786 ) ;
#69070 = SHAPE_REPRESENTATION ( 'MAS-695', ( #130451, #37734, #42402, #650, #67881, #58680, #137283, #49340, #139685, #23855, #53995, #81736, #123437, #16921, #135029, #116470, #14642, #77178, #95648, #72535, #35590 ), #28633 ) ;
#69073 = EDGE_CURVE ( 'NONE', #44746, #122630, #10756, .T. ) ;
#69072 = AXIS2_PLACEMENT_3D ( 'NONE', #3874, #124274, #38004 ) ;
#69071 = DIRECTION ( 'NONE',  ( 0.7071067811865487940, 0.7071067811865463515, -0.000000000000000000 ) ) ;
#69074 = ADVANCED_FACE ( 'NONE', ( #88371 ), #52150, .F. ) ;
#69075 = CARTESIAN_POINT ( 'NONE',  ( 35.29209685856476852, -5.291415217122921177, 3.054999999999999272 ) ) ;
#69076 = EDGE_LOOP ( 'NONE', ( #60506, #67723, #94547, #103811 ) ) ;
#69077 = DIRECTION ( 'NONE',  ( 0.7071067811865487940, 0.7071067811865463515, 0.000000000000000000 ) ) ;
#69078 = VERTEX_POINT ( 'NONE', #130446 ) ;
#69079 = LINE ( 'NONE', #113256, #12580 ) ;
#69080 = EDGE_CURVE ( 'NONE', #41509, #142587, #142045, .T. ) ;
#69081 = DIRECTION ( 'NONE',  ( -0.7071067811865486830, 0.7071067811865464625, 0.000000000000000000 ) ) ;
#69082 = CARTESIAN_POINT ( 'NONE',  ( -34.42499999999997584, -21.76999999999999247, -0.5000000000000000000 ) ) ;
#69083 = CARTESIAN_POINT ( 'NONE',  ( 44.99451991528749772, 28.92564299267969474, 4.000000000000000000 ) ) ;
#69084 = ORIENTED_EDGE ( 'NONE', *, *, #92385, .F. ) ;
#69085 = ADVANCED_FACE ( 'NONE', ( #86934 ), #74640, .T. ) ;
#69086 = LINE ( 'NONE', #60168, #7176 ) ;
#69087 = VERTEX_POINT ( 'NONE', #76052 ) ;
#69088 = CARTESIAN_POINT ( 'NONE',  ( 39.60002705046289151, 5.819803920172570422, 5.819803920172575751 ) ) ;
#69089 = EDGE_CURVE ( 'NONE', #65792, #32200, #120222, .T. ) ;
#69090 = DIRECTION ( 'NONE',  ( -0.7071067811865487940, 0.7071067811865463515, -0.000000000000000000 ) ) ;
#69091 = LINE ( 'NONE', #113269, #105605 ) ;
#69092 = DIRECTION ( 'NONE',  ( 0.3543493200069162685, -0.000000000000000000, -0.9351131265310288487 ) ) ;
#69093 = AXIS2_PLACEMENT_3D ( 'NONE', #58298, #89434, #102480 ) ;
#69094 = ADVANCED_FACE ( 'NONE', ( #85473 ), #65199, .T. ) ;
#69095 = CARTESIAN_POINT ( 'NONE',  ( 6.160000000000001030, 9.521314400968980422E-16, 0.000000000000000000 ) ) ;
#69096 = CARTESIAN_POINT ( 'NONE',  ( 61.16209685856478728, -5.291415217122919401, 3.054999999999997939 ) ) ;
#69097 = CARTESIAN_POINT ( 'NONE',  ( -25.00934544866806064, 2.809161053235901484, 4.346514962826536710 ) ) ;
#69098 = CARTESIAN_POINT ( 'NONE',  ( 36.29974487139159578, -27.71228299555231445, 4.000000000000000000 ) ) ;
#69099 = VERTEX_POINT ( 'NONE', #12205 ) ;
#69100 = EDGE_LOOP ( 'NONE', ( #26062, #140083, #14702, #3487 ) ) ;
#69101 = DIRECTION ( 'NONE',  ( -1.000000000000000000, -0.000000000000000000, -0.000000000000000000 ) ) ;
#69102 = ADVANCED_FACE ( 'NONE', ( #11468 ), #3454, .F. ) ;
#69103 = ORIENTED_EDGE ( 'NONE', *, *, #12405, .F. ) ;
#69104 = DIRECTION ( 'NONE',  ( -0.6830127018922180770, -0.6830127018922204085, -0.2588190451025213501 ) ) ;
#69105 = ORIENTED_EDGE ( 'NONE', *, *, #48801, .F. ) ;
#69106 = CARTESIAN_POINT ( 'NONE',  ( -13.25154412867567189, -11.24070752338417201, 10.39518518046012119 ) ) ;
#69107 = CARTESIAN_POINT ( 'NONE',  ( -12.32816939922343913, -15.74070752338412404, 4.000000000000000000 ) ) ;
#69108 = PLANE ( 'NONE',  #67363 ) ;
#69109 = VECTOR ( 'NONE', #20029, 1000.000000000000000 ) ;
#69110 = FACE_BOUND ( 'NONE', #36494, .T. ) ;
#69111 = LINE ( 'NONE', #113293, #17824 ) ;
#69112 = VECTOR ( 'NONE', #8492, 1000.000000000000000 ) ;
#69113 = CARTESIAN_POINT ( 'NONE',  ( 3.005480084712505828, 28.92564299267936079, 4.000000000000000000 ) ) ;
#69114 = CARTESIAN_POINT ( 'NONE',  ( -16.49999999999988276, 21.05218569542895679, 5.000000000000000000 ) ) ;
#69115 = DIRECTION ( 'NONE',  ( -0.7071067811865486830, -0.7071067811865464625, -0.000000000000000000 ) ) ;
#69117 = EDGE_LOOP ( 'NONE', ( #58724, #51371, #70824, #125306 ) ) ;
#69116 = CARTESIAN_POINT ( 'NONE',  ( -25.39999999999996305, 0.000000000000000000, 2.500000000000000000 ) ) ;
#69118 = VECTOR ( 'NONE', #34908, 1000.000000000000000 ) ;
#69119 = EDGE_LOOP ( 'NONE', ( #18370, #78453, #93560, #82274 ) ) ;
#69120 = VECTOR ( 'NONE', #125715, 1000.000000000000000 ) ;
#69121 = DIRECTION ( 'NONE',  ( 0.000000000000000000, -1.000000000000000000, 0.000000000000000000 ) ) ;
#69122 = ORIENTED_EDGE ( 'NONE', *, *, #88510, .F. ) ;
#69123 = EDGE_CURVE ( 'NONE', #47403, #138017, #44904, .T. ) ;
#69124 = EDGE_CURVE ( 'NONE', #143125, #123729, #31152, .T. ) ;
#69125 = ORIENTED_EDGE ( 'NONE', *, *, #100962, .T. ) ;
#69126 = CARTESIAN_POINT ( 'NONE',  ( 70.93293019189810877, 1.637169565754156508, 6.110000000000000320 ) ) ;
#69127 = ORIENTED_EDGE ( 'NONE', *, *, #30596, .T. ) ;
#69128 = DIRECTION ( 'NONE',  ( 0.7071067811865487940, -0.7071067811865463515, 0.000000000000000000 ) ) ;
#69129 = ORIENTED_EDGE ( 'NONE', *, *, #5808, .F. ) ;
#69130 = PLANE ( 'NONE',  #53728 ) ;
#69131 = VECTOR ( 'NONE', #32824, 1000.000000000000000 ) ;
#69132 = CARTESIAN_POINT ( 'NONE',  ( 123.0625000000000000, -5.819803920172573086, -5.819803920172573974 ) ) ;
#69133 = VECTOR ( 'NONE', #39803, 1000.000000000000000 ) ;
#69134 = CARTESIAN_POINT ( 'NONE',  ( 9.299744871391588674, -27.71228299555212971, 4.000000000000000000 ) ) ;
#69135 = DIRECTION ( 'NONE',  ( -1.000000000000000000, 0.000000000000000000, 0.000000000000000000 ) ) ;
#69137 = FACE_OUTER_BOUND ( 'NONE', #67942, .T. ) ;
#69136 = DIRECTION ( 'NONE',  ( 0.7071067811865487940, 0.7071067811865463515, -0.000000000000000000 ) ) ;
#69138 = DIRECTION ( 'NONE',  ( 0.7071067811865486830, 0.7071067811865464625, 0.000000000000000000 ) ) ;
#69139 = PLANE ( 'NONE',  #124961 ) ;
#69140 = ORIENTED_EDGE ( 'NONE', *, *, #33107, .F. ) ;
#69141 = ORIENTED_EDGE ( 'NONE', *, *, #68016, .T. ) ;
#69142 = LINE ( 'NONE', #66992, #107564 ) ;
#69143 = DIRECTION ( 'NONE',  ( -0.000000000000000000, -0.000000000000000000, 1.000000000000000000 ) ) ;
#69144 = ORIENTED_EDGE ( 'NONE', *, *, #24976, .T. ) ;
#69145 = VECTOR ( 'NONE', #80264, 1000.000000000000000 ) ;
#69146 = ORIENTED_EDGE ( 'NONE', *, *, #69759, .T. ) ;
#69147 = VECTOR ( 'NONE', #26855, 1000.000000000000000 ) ;
#69148 = ORIENTED_EDGE ( 'NONE', *, *, #54701, .T. ) ;
#69149 = LINE ( 'NONE', #88764, #36883 ) ;
#69150 = ORIENTED_EDGE ( 'NONE', *, *, #8265, .T. ) ;
#69151 = CIRCLE ( 'NONE', #6580, 2.500000000000000444 ) ;
#69152 = CARTESIAN_POINT ( 'NONE',  ( -57.48921356237308800, -27.52281430457095368, 5.000000000000000000 ) ) ;
#69153 = CARTESIAN_POINT ( 'NONE',  ( 5.999999999999965361, -0.03360074219773551141, 5.000000000000000000 ) ) ;
#69154 = CARTESIAN_POINT ( 'NONE',  ( 1.525403141435219379, 2.126176841940962348, 7.934999999999989839 ) ) ;
#69155 = CARTESIAN_POINT ( 'NONE',  ( 16.27785539607886633, 2.500000000000000444, 0.000000000000000000 ) ) ;
#69156 = VERTEX_POINT ( 'NONE', #91240 ) ;
#69157 = CARTESIAN_POINT ( 'NONE',  ( 34.92499999999998295, -22.22500000000000142, 4.500000000000000888 ) ) ;
#69158 = CARTESIAN_POINT ( 'NONE',  ( -17.02886364525924989, -2.441401769420105339, 4.000000000000000000 ) ) ;
#69159 = DIRECTION ( 'NONE',  ( -0.7071067811865486830, -0.7071067811865464625, 0.000000000000000000 ) ) ;
#69161 = ORIENTED_EDGE ( 'NONE', *, *, #39163, .T. ) ;
#69160 = DIRECTION ( 'NONE',  ( 0.000000000000000000, -1.000000000000000000, 0.000000000000000000 ) ) ;
#69162 = ORIENTED_EDGE ( 'NONE', *, *, #66807, .T. ) ;
#69163 = LINE ( 'NONE', #133008, #7931 ) ;
#69164 = DIRECTION ( 'NONE',  ( -1.000000000000000000, -0.000000000000000000, -0.000000000000000000 ) ) ;
#69165 = AXIS2_PLACEMENT_3D ( 'NONE', #26226, #59586, #68341 ) ;
#69166 = FACE_OUTER_BOUND ( 'NONE', #100189, .T. ) ;
#69167 = VERTEX_POINT ( 'NONE', #608 ) ;
#69168 = DIRECTION ( 'NONE',  ( -0.7071067811865487940, 0.7071067811865463515, -0.000000000000000000 ) ) ;
#69169 = CARTESIAN_POINT ( 'NONE',  ( -25.39999999999996305, 0.000000000000000000, 0.000000000000000000 ) ) ;
#69170 =( LENGTH_UNIT ( ) NAMED_UNIT ( * ) SI_UNIT ( .MILLI., .METRE. ) );
#69171 = DIRECTION ( 'NONE',  ( 0.7071067811865486830, -0.7071067811865464625, -0.000000000000000000 ) ) ;
#69172 = DIRECTION ( 'NONE',  ( -0.6830127018922181881, 0.6830127018922202975, -0.2588190451025214056 ) ) ;
#69173 = ORIENTED_EDGE ( 'NONE', *, *, #77564, .F. ) ;
#69174 = CARTESIAN_POINT ( 'NONE',  ( -30.70710678118633652, 11.25929247661560773, 5.000000000000000000 ) ) ;
#69175 = LINE ( 'NONE', #113358, #56321 ) ;
#69176 = CARTESIAN_POINT ( 'NONE',  ( -25.39999999999996305, 0.000000000000000000, 0.000000000000000000 ) ) ;
#69177 = EDGE_CURVE ( 'NONE', #80880, #60780, #122386, .T. ) ;
#69178 = CARTESIAN_POINT ( 'NONE',  ( 4.495848767239241539, 4.584330080086930965E-16, 0.000000000000000000 ) ) ;
#69179 = LINE ( 'NONE', #113362, #90030 ) ;
#69180 = EDGE_CURVE ( 'NONE', #67296, #86133, #136131, .T. ) ;
#69181 = VERTEX_POINT ( 'NONE', #81063 ) ;
#69182 = ORIENTED_EDGE ( 'NONE', *, *, #53829, .F. ) ;
#69183 = CARTESIAN_POINT ( 'NONE',  ( 7.799999601179139042, 3.821174125832445049E-16, 0.000000000000000000 ) ) ;
#69184 = ADVANCED_FACE ( 'NONE', ( #33983 ), #23814, .F. ) ;
#69185 = EDGE_CURVE ( 'NONE', #139146, #127658, #68080, .T. ) ;
#69186 = CARTESIAN_POINT ( 'NONE',  ( 9.758600742197899081, 21.72500000000000853, 5.000000000000000000 ) ) ;
#69187 = DIRECTION ( 'NONE',  ( -0.7071067811865486830, -0.7071067811865464625, 0.000000000000000000 ) ) ;
#69188 = CARTESIAN_POINT ( 'NONE',  ( 8.510786437626906675, -27.52281430457049183, 5.000000000000000000 ) ) ;
#69189 = CARTESIAN_POINT ( 'NONE',  ( 30.29974487139158867, -27.71228299555227537, 4.000000000000000000 ) ) ;
#69190 = ORIENTED_EDGE ( 'NONE', *, *, #81329, .T. ) ;
#69191 = EDGE_CURVE ( 'NONE', #87366, #135494, #110783, .T. ) ;
#69192 = CARTESIAN_POINT ( 'NONE',  ( 41.99451991528749062, 28.92564299267967343, 4.000000000000000000 ) ) ;
#69193 = UNCERTAINTY_MEASURE_WITH_UNIT (LENGTH_MEASURE( 1.000000000000000082E-05 ), #102998, 'distance_accuracy_value', 'NONE');
#69194 = DIRECTION ( 'NONE',  ( -0.000000000000000000, -0.3543493200069152693, 0.9351131265310292928 ) ) ;
#69195 = CARTESIAN_POINT ( 'NONE',  ( -12.79289321881336328, -11.24070752338416845, 5.000000000000000000 ) ) ;
#69196 = CARTESIAN_POINT ( 'NONE',  ( 56.05793019189811588, 6.110000000000001208, -1.637169565754156286 ) ) ;
#69197 = LINE ( 'NONE', #112681, #18583 ) ;
#69198 = EDGE_CURVE ( 'NONE', #123136, #39115, #91910, .T. ) ;
#69199 = CARTESIAN_POINT ( 'NONE',  ( 31.57919371712955581, 3.975000000000002753, -6.884901960086283523 ) ) ;
#69200 = CARTESIAN_POINT ( 'NONE',  ( -12.69999999999998153, 3.061616997868383634E-16, -2.500000000000000444 ) ) ;
#69201 = ORIENTED_EDGE ( 'NONE', *, *, #102914, .F. ) ;
#69202 = CARTESIAN_POINT ( 'NONE',  ( 26.51360224591381254, -6.350000000000003197, -3.888253587292850026E-16 ) ) ;
#69203 = ORIENTED_EDGE ( 'NONE', *, *, #3439, .F. ) ;
#69204 = CARTESIAN_POINT ( 'NONE',  ( 11.15159235450332176, 3.061616997868380183E-16, -2.500000000000001332 ) ) ;
#69206 = EDGE_CURVE ( 'NONE', #42509, #64814, #112259, .T. ) ;
#69205 = CIRCLE ( 'NONE', #122462, 25.00000000000002487 ) ;
#69207 = VECTOR ( 'NONE', #52575, 999.9999999999998863 ) ;
#69208 = VECTOR ( 'NONE', #135606, 1000.000000000000000 ) ;
#69209 = CARTESIAN_POINT ( 'NONE',  ( 28.49999999999980460, 10.94296225409028800, -9.576120664313192421 ) ) ;
#69210 = DIRECTION ( 'NONE',  ( -0.3543493200069163240, 4.681814790819596721E-17, -0.9351131265310288487 ) ) ;
#69211 = VECTOR ( 'NONE', #23817, 999.9999999999998863 ) ;
#69212 = DIRECTION ( 'NONE',  ( 0.6830127018922181881, 0.6830127018922202975, -0.2588190451025214056 ) ) ;
#69213 = CARTESIAN_POINT ( 'NONE',  ( 13.17183060077638324, -8.240707523384196875, 4.000000000000000000 ) ) ;
#69214 = CARTESIAN_POINT ( 'NONE',  ( -7.140000000000001457, -39.92999999999999261, -40.00000000000000000 ) ) ;
#69215 = ORIENTED_EDGE ( 'NONE', *, *, #89484, .T. ) ;
#69216 = ORIENTED_EDGE ( 'NONE', *, *, #56983, .F. ) ;
#69217 = DIRECTION ( 'NONE',  ( 0.000000000000000000, 0.000000000000000000, 1.000000000000000000 ) ) ;
#69218 = CARTESIAN_POINT ( 'NONE',  ( -24.18398860626899705, 28.73617430169804265, 5.000000000000000000 ) ) ;
#69219 = UNCERTAINTY_MEASURE_WITH_UNIT (LENGTH_MEASURE( 1.000000000000000082E-05 ), #31054, 'distance_accuracy_value', 'NONE');
#69220 = EDGE_CURVE ( 'NONE', #46380, #77993, #57187, .T. ) ;
#69221 = VECTOR ( 'NONE', #3867, 1000.000000000000114 ) ;
#69222 = DIRECTION ( 'NONE',  ( 0.6830127018922181881, 0.6830127018922202975, -0.2588190451025214056 ) ) ;
#69223 = DIRECTION ( 'NONE',  ( 0.7071067811865487940, 0.7071067811865463515, -0.000000000000000000 ) ) ;
#69224 = CARTESIAN_POINT ( 'NONE',  ( 77.66252705046289861, 7.949999999999998401, 1.460391307983218338E-15 ) ) ;
#69225 = DIRECTION ( 'NONE',  ( -0.000000000000000000, 0.000000000000000000, 1.000000000000000000 ) ) ;
#69226 = DIRECTION ( 'NONE',  ( -0.3543493200069162685, -0.000000000000000000, -0.9351131265310288487 ) ) ;
#69227 = VERTEX_POINT ( 'NONE', #46318 ) ;
#69228 = CARTESIAN_POINT ( 'NONE',  ( 74.64583333333331439, 2.130196079827431976, -7.949999999999999289 ) ) ;
#69229 = CARTESIAN_POINT ( 'NONE',  ( -0.1839886062690032631, 28.73617430169787568, 5.000000000000000000 ) ) ;
#69230 = DIRECTION ( 'NONE',  ( -0.6830127018922181881, 0.6830127018922202975, -0.2588190451025214056 ) ) ;
#69231 = CARTESIAN_POINT ( 'NONE',  ( 21.85005128541011388, -8.240707523384182664, 17.25253755692243729 ) ) ;
#69232 = ADVANCED_FACE ( 'NONE', ( #113661 ), #90500, .T. ) ;
#69233 =( GEOMETRIC_REPRESENTATION_CONTEXT ( 3 ) GLOBAL_UNCERTAINTY_ASSIGNED_CONTEXT ( ( #121756 ) ) GLOBAL_UNIT_ASSIGNED_CONTEXT ( ( #136385, #50110, #139278 ) ) REPRESENTATION_CONTEXT ( 'NONE', 'WORKASPACE' ) );
#69234 = ORIENTED_EDGE ( 'NONE', *, *, #88055, .T. ) ;
#69235 = FACE_OUTER_BOUND ( 'NONE', #22248, .T. ) ;
#69236 = EDGE_CURVE ( 'NONE', #39945, #16237, #32039, .T. ) ;
#69237 = VECTOR ( 'NONE', #91670, 1000.000000000000114 ) ;
#69238 = PLANE ( 'NONE',  #95328 ) ;
#69239 = CARTESIAN_POINT ( 'NONE',  ( 69.70876352523144703, -7.482591942790329030E-16, 6.110000000000001208 ) ) ;
#69240 = EDGE_CURVE ( 'NONE', #127203, #37030, #14359, .T. ) ;
#69241 = PLANE ( 'NONE',  #92258 ) ;
#69242 = EDGE_LOOP ( 'NONE', ( #49488, #81289 ) ) ;
#69243 = VERTEX_POINT ( 'NONE', #60767 ) ;
#69244 = VECTOR ( 'NONE', #39661, 1000.000000000000000 ) ;
#69245 = EDGE_CURVE ( 'NONE', #68883, #27289, #60021, .T. ) ;
#69246 = DIRECTION ( 'NONE',  ( -0.7071067811865486830, -0.7071067811865464625, 0.000000000000000000 ) ) ;
#69247 = DIRECTION ( 'NONE',  ( -0.7071067811865486830, -0.7071067811865464625, 0.000000000000000000 ) ) ;
#69248 = LINE ( 'NONE', #24992, #57876 ) ;
#69250 = EDGE_LOOP ( 'NONE', ( #94060, #47783, #125610, #70886 ) ) ;
#69249 = CARTESIAN_POINT ( 'NONE',  ( -10.49999999999991829, -11.94781430457070748, 5.000000000000000000 ) ) ;
#69251 = CARTESIAN_POINT ( 'NONE',  ( 42.48921356237308800, -27.52281430457085065, 5.000000000000000000 ) ) ;
#69252 = CARTESIAN_POINT ( 'NONE',  ( 7.408407645496676963, 9.139736423841732040E-16, 0.000000000000000000 ) ) ;
#69253 = CARTESIAN_POINT ( 'NONE',  ( 63.29974487139158867, -27.71228299555250274, 4.000000000000000000 ) ) ;
#69254 = VECTOR ( 'NONE', #18706, 999.9999999999998863 ) ;
#69255 = LINE ( 'NONE', #47537, #20637 ) ;
#69256 = CIRCLE ( 'NONE', #64587, 2.500000000000000888 ) ;
#69257 = VERTEX_POINT ( 'NONE', #94049 ) ;
#69258 = VERTEX_POINT ( 'NONE', #138285 ) ;
#69259 = CARTESIAN_POINT ( 'NONE',  ( 51.47959685856477563, 6.109999999999999432, 1.637169565754164280 ) ) ;
#69260 = ORIENTED_EDGE ( 'NONE', *, *, #95829, .F. ) ;
#69261 = EDGE_CURVE ( 'NONE', #94085, #80926, #137574, .T. ) ;
#69262 = DIRECTION ( 'NONE',  ( -1.000000000000000000, -1.224606353822377258E-16, -0.000000000000000000 ) ) ;
#69263 = LINE ( 'NONE', #2529, #73511 ) ;
#69264 = DIRECTION ( 'NONE',  ( -0.7071067811865486830, -0.7071067811865464625, 0.000000000000000000 ) ) ;
#69265 = DIRECTION ( 'NONE',  ( -0.6830127018922180770, -0.6830127018922204085, -0.2588190451025213501 ) ) ;
#69266 = CARTESIAN_POINT ( 'NONE',  ( 39.29974487139159578, -27.71228299555233576, 4.000000000000000000 ) ) ;
#69267 = VERTEX_POINT ( 'NONE', #139005 ) ;
#69268 = ORIENTED_EDGE ( 'NONE', *, *, #102783, .F. ) ;
#69269 = AXIS2_PLACEMENT_3D ( 'NONE', #75598, #108892, #10308 ) ;
#69270 = DIRECTION ( 'NONE',  ( -1.000000000000000000, -1.224606353822377258E-16, -0.000000000000000000 ) ) ;
#69272 = ADVANCED_FACE ( 'NONE', ( #81793 ), #136844, .T. ) ;
#69271 = PRESENTATION_STYLE_ASSIGNMENT (( #12716 ) ) ;
#69273 = ORIENTED_EDGE ( 'NONE', *, *, #78062, .F. ) ;
#69274 = DIRECTION ( 'NONE',  ( -0.3543493200069162685, -0.000000000000000000, -0.9351131265310288487 ) ) ;
#69275 = ORIENTED_EDGE ( 'NONE', *, *, #40579, .T. ) ;
#69276 = LINE ( 'NONE', #113456, #140591 ) ;
#69277 = DIRECTION ( 'NONE',  ( -0.6830127018922180770, -0.6830127018922204085, -0.2588190451025213501 ) ) ;
#69278 = ORIENTED_EDGE ( 'NONE', *, *, #77324, .T. ) ;
#69279 = FACE_BOUND ( 'NONE', #54133, .T. ) ;
#69280 = CARTESIAN_POINT ( 'NONE',  ( -36.18398860626899705, 28.73617430169812437, 5.000000000000000000 ) ) ;
#69281 = ADVANCED_FACE ( 'NONE', ( #83190 ), #126668, .F. ) ;
#69282 = DIRECTION ( 'NONE',  ( -0.7071067811865486830, 0.7071067811865464625, 0.000000000000000000 ) ) ;
#69283 = DIRECTION ( 'NONE',  ( -0.6830127018922180770, -0.6830127018922204085, -0.2588190451025213501 ) ) ;
#69284 = DIRECTION ( 'NONE',  ( 0.6830127018922180770, -0.6830127018922204085, -0.2588190451025213501 ) ) ;
#69285 = SURFACE_STYLE_FILL_AREA ( #125071 ) ;
#69286 = DIRECTION ( 'NONE',  ( -6.283022375640376762E-33, -0.9242245927363030855, -0.3818493186865927203 ) ) ;
#69287 = ORIENTED_EDGE ( 'NONE', *, *, #13597, .F. ) ;
#69288 = ADVANCED_FACE ( 'NONE', ( #28091 ), #117210, .F. ) ;
#69289 = ORIENTED_EDGE ( 'NONE', *, *, #65775, .T. ) ;
#69290 = CARTESIAN_POINT ( 'NONE',  ( 105.9329301918981230, 1.637169565754156508, 6.110000000000000320 ) ) ;
#69291 = ORIENTED_EDGE ( 'NONE', *, *, #111056, .T. ) ;
#69292 = FACE_OUTER_BOUND ( 'NONE', #10671, .T. ) ;
#69293 = ORIENTED_EDGE ( 'NONE', *, *, #100410, .F. ) ;
#69294 = CARTESIAN_POINT ( 'NONE',  ( 0.000000000000000000, 0.000000000000000000, 5.000000000000000000 ) ) ;
#69295 = CARTESIAN_POINT ( 'NONE',  ( 0.000000000000000000, 0.000000000000000000, 5.000000000000000000 ) ) ;
#69297 = EDGE_CURVE ( 'NONE', #105597, #5049, #39703, .T. ) ;
#69296 = CARTESIAN_POINT ( 'NONE',  ( -2.994519915287485734, 28.92564299267940342, 4.000000000000000000 ) ) ;
#69298 = EDGE_LOOP ( 'NONE', ( #52122, #140517, #65808, #90963 ) ) ;
#69299 = DIRECTION ( 'NONE',  ( -1.000000000000000000, -0.000000000000000000, -0.000000000000000000 ) ) ;
#69300 = FACE_OUTER_BOUND ( 'NONE', #83446, .T. ) ;
#69301 =( LENGTH_UNIT ( ) NAMED_UNIT ( * ) SI_UNIT ( .MILLI., .METRE. ) );
#69303 = CARTESIAN_POINT ( 'NONE',  ( -33.51168605928411637, 6.759292476615653023, 16.35960578974477286 ) ) ;
#69302 = DIRECTION ( 'NONE',  ( 0.7071067811865487940, 0.7071067811865463515, 0.000000000000000000 ) ) ;
#69304 = CARTESIAN_POINT ( 'NONE',  ( 2.816011393730999401, 28.73617430169785436, 5.000000000000000000 ) ) ;
#69305 = VECTOR ( 'NONE', #42946, 1000.000000000000000 ) ;
#69306 = VECTOR ( 'NONE', #47232, 1000.000000000000000 ) ;
#69307 = CARTESIAN_POINT ( 'NONE',  ( -32.99999999999977263, 4.931123077392136622, 4.000000000000000000 ) ) ;
#69308 = AXIS2_PLACEMENT_3D ( 'NONE', #114164, #70699, #51065 ) ;
#69309 = ORIENTED_EDGE ( 'NONE', *, *, #74247, .F. ) ;
#69310 = CARTESIAN_POINT ( 'NONE',  ( 88.20833333333332860, -3.974999999999999201, -6.884901960086287964 ) ) ;
#69311 = DIRECTION ( 'NONE',  ( 0.7071067811865487940, 0.7071067811865463515, 0.000000000000000000 ) ) ;
#69312 = AXIS2_PLACEMENT_3D ( 'NONE', #42572, #88200, #132451 ) ;
#69313 = ORIENTED_EDGE ( 'NONE', *, *, #104776, .F. ) ;
#69314 = ORIENTED_EDGE ( 'NONE', *, *, #116323, .F. ) ;
#69315 = EDGE_CURVE ( 'NONE', #100866, #21087, #83935, .T. ) ;
#69316 = ORIENTED_EDGE ( 'NONE', *, *, #143322, .T. ) ;
#69317 = CARTESIAN_POINT ( 'NONE',  ( 57.89626352523144703, 4.472830434245840259, -4.472830434245838482 ) ) ;
#69318 = ORIENTED_EDGE ( 'NONE', *, *, #740, .T. ) ;
#69319 = VECTOR ( 'NONE', #91480, 1000.000000000000227 ) ;
#69320 = CARTESIAN_POINT ( 'NONE',  ( 1.795806282870439308, -5.278424836066144543, 3.047499999999995879 ) ) ;
#69321 = CARTESIAN_POINT ( 'NONE',  ( 90.41709685856477563, 3.054999999999998828, 5.291415217122922066 ) ) ;
#69322 = CARTESIAN_POINT ( 'NONE',  ( 23.90156419391748699, 11.25929247661560240, 10.79108189686412622 ) ) ;
#69323 = ORIENTED_EDGE ( 'NONE', *, *, #79457, .F. ) ;
#69324 = CARTESIAN_POINT ( 'NONE',  ( 2.999999999999990674, 4.552185695429124657, 5.000000000000000000 ) ) ;
#69325 = ORIENTED_EDGE ( 'NONE', *, *, #43332, .F. ) ;
#69326 = AXIS2_PLACEMENT_3D ( 'NONE', #85388, #96950, #141200 ) ;
#69327 = AXIS2_PLACEMENT_3D ( 'NONE', #75070, #53265, #77900 ) ;
#69328 = DIRECTION ( 'NONE',  ( 0.3543493200069162685, -0.000000000000000000, -0.9351131265310288487 ) ) ;
#69329 = ORIENTED_EDGE ( 'NONE', *, *, #58854, .F. ) ;
#69330 = SURFACE_SIDE_STYLE ('',( #2606 ) ) ;
#69331 = CARTESIAN_POINT ( 'NONE',  ( 3.707106781186513711, -18.74070752338409562, 5.000000000000000000 ) ) ;
#69332 = DIRECTION ( 'NONE',  ( -1.000000000000000000, -0.000000000000000000, -0.000000000000000000 ) ) ;
#69333 = EDGE_LOOP ( 'NONE', ( #6963, #43769, #36691, #72018 ) ) ;
#69334 = VECTOR ( 'NONE', #107536, 1000.000000000000000 ) ;
#69335 = CARTESIAN_POINT ( 'NONE',  ( 19.11017322888197612, -22.22500000000000142, 4.785647885939352975 ) ) ;
#69336 = ORIENTED_EDGE ( 'NONE', *, *, #111430, .F. ) ;
#69337 = ORIENTED_EDGE ( 'NONE', *, *, #51814, .F. ) ;
#69338 = ORIENTED_EDGE ( 'NONE', *, *, #88718, .F. ) ;
#69339 = EDGE_CURVE ( 'NONE', #128957, #119015, #17886, .T. ) ;
#69340 = PLANE ( 'NONE',  #125766 ) ;
#69341 = VECTOR ( 'NONE', #65539, 999.9999999999998863 ) ;
#69342 = AXIS2_PLACEMENT_3D ( 'NONE', #125564, #69043, #1583 ) ;
#69343 = FACE_BOUND ( 'NONE', #97853, .T. ) ;
#69344 = VECTOR ( 'NONE', #16008, 1000.000000000000000 ) ;
#69345 = DIRECTION ( 'NONE',  ( -0.7071067811865486830, -0.7071067811865464625, 0.000000000000000000 ) ) ;
#69346 = PLANE ( 'NONE',  #122665 ) ;
#69347 = ADVANCED_FACE ( 'NONE', ( #62160 ), #106325, .F. ) ;
#69348 = EDGE_CURVE ( 'NONE', #29421, #33782, #86878, .T. ) ;
#69349 = DIRECTION ( 'NONE',  ( 1.000000000000000000, 0.000000000000000000, 0.000000000000000000 ) ) ;
#69350 = VERTEX_POINT ( 'NONE', #20047 ) ;
#69351 = VECTOR ( 'NONE', #86141, 1000.000000000000000 ) ;
#69352 = AXIS2_PLACEMENT_3D ( 'NONE', #828, #142951, #99423 ) ;
#69353 = DIRECTION ( 'NONE',  ( 0.7071067811865486830, -0.7071067811865464625, -0.000000000000000000 ) ) ;
#69354 = EDGE_CURVE ( 'NONE', #94828, #41854, #141117, .T. ) ;
#69355 = EDGE_CURVE ( 'NONE', #28440, #62795, #87477, .T. ) ;
#69356 = CARTESIAN_POINT ( 'NONE',  ( 25.20790314143522082, -6.871911579029513106, -3.967499999999993587 ) ) ;
#69357 = CARTESIAN_POINT ( 'NONE',  ( 12.19999999999999574, -28.33999999999998565, 13.17925390838734323 ) ) ;
#69358 = EDGE_CURVE ( 'NONE', #19458, #71456, #119353, .T. ) ;
#69359 = PLANE ( 'NONE',  #133974 ) ;
#69360 = LINE ( 'NONE', #57068, #16576 ) ;
#69361 = ORIENTED_EDGE ( 'NONE', *, *, #99021, .F. ) ;
#69362 = ORIENTED_EDGE ( 'NONE', *, *, #947, .T. ) ;
#69363 = EDGE_CURVE ( 'NONE', #63037, #81871, #29498, .T. ) ;
#69364 = ORIENTED_EDGE ( 'NONE', *, *, #25974, .T. ) ;
#69365 = DIRECTION ( 'NONE',  ( -1.000000000000000000, -1.224606353822377258E-16, -0.000000000000000000 ) ) ;
#69366 = VECTOR ( 'NONE', #109842, 999.9999999999998863 ) ;
#69367 = EDGE_CURVE ( 'NONE', #34230, #22757, #87611, .T. ) ;
#69368 = FACE_OUTER_BOUND ( 'NONE', #64474, .T. ) ;
#69369 = LINE ( 'NONE', #114277, #122310 ) ;
#69370 = CARTESIAN_POINT ( 'NONE',  ( -0.8748538069076501333, -14.24070752338413826, 9.401115078912660294 ) ) ;
#69371 = ADVANCED_FACE ( 'NONE', ( #97612 ), #109215, .T. ) ;
#69372 = DIRECTION ( 'NONE',  ( -1.000000000000000000, -0.000000000000000000, -0.000000000000000000 ) ) ;
#69373 = CARTESIAN_POINT ( 'NONE',  ( 14.99999999999989164, -7.068876922607732816, 4.000000000000000000 ) ) ;
#69374 = CARTESIAN_POINT ( 'NONE',  ( -18.29974487139159223, -27.71228299555219010, 4.000000000000000000 ) ) ;
#69375 = DIRECTION ( 'NONE',  ( 0.7071067811865487940, 0.7071067811865463515, -0.000000000000000000 ) ) ;
#69376 = LINE ( 'NONE', #36717, #67361 ) ;
#69377 = ORIENTED_EDGE ( 'NONE', *, *, #13778, .F. ) ;
#69378 = CARTESIAN_POINT ( 'NONE',  ( 16.96838079760940232, -0.7556382844926715636, -35.24774147208035657 ) ) ;
#69379 = EDGE_LOOP ( 'NONE', ( #12511, #63722, #59989, #93464 ) ) ;
#69380 = EDGE_CURVE ( 'NONE', #94753, #77993, #9894, .T. ) ;
#69381 = DIRECTION ( 'NONE',  ( -1.000000000000000000, -0.000000000000000000, -0.000000000000000000 ) ) ;
#69382 = EDGE_LOOP ( 'NONE', ( #30738, #117358, #71546, #120282 ) ) ;
#69383 = LINE ( 'NONE', #78113, #94905 ) ;
#69384 = CARTESIAN_POINT ( 'NONE',  ( 12.79289321881337216, -5.240707523384223521, 5.000000000000000000 ) ) ;
#69385 = ORIENTED_EDGE ( 'NONE', *, *, #80867, .F. ) ;
#69386 = CARTESIAN_POINT ( 'NONE',  ( 16.75173015016484968, 4.202752102959690472E-16, 0.000000000000000000 ) ) ;
#69387 = VERTEX_POINT ( 'NONE', #130280 ) ;
#69388 = DIRECTION ( 'NONE',  ( -0.000000000000000000, 0.000000000000000000, 1.000000000000000000 ) ) ;
#69389 = ORIENTED_EDGE ( 'NONE', *, *, #107346, .T. ) ;
#69390 = ADVANCED_FACE ( 'NONE', ( #65024 ), #10593, .T. ) ;
#69391 = CARTESIAN_POINT ( 'NONE',  ( 18.18398860626898994, 28.73617430169800002, 5.000000000000000000 ) ) ;
#69392 = CARTESIAN_POINT ( 'NONE',  ( 105.9541937171295700, 6.884901960086283523, 3.975000000000002753 ) ) ;
#69393 = CYLINDRICAL_SURFACE ( 'NONE', #115610, 2.500000000000000444 ) ;
#69394 = DIRECTION ( 'NONE',  ( -0.7071067811865487940, 0.7071067811865463515, -0.000000000000000000 ) ) ;
#69395 = ORIENTED_EDGE ( 'NONE', *, *, #48236, .F. ) ;
#69396 = CARTESIAN_POINT ( 'NONE',  ( 30.83652871126530570, 15.75929247661555443, 9.299976744542991725 ) ) ;
#69397 = LINE ( 'NONE', #1928, #3252 ) ;
#69398 = PLANE ( 'NONE',  #15999 ) ;
#69399 = CARTESIAN_POINT ( 'NONE',  ( 24.20833333333333570, 3.047499999999997655, 5.278424836066143655 ) ) ;
#69400 = CARTESIAN_POINT ( 'NONE',  ( 25.39999999999999503, -5.131256043349313067, -6.052638797879072108 ) ) ;
#69401 = FACE_OUTER_BOUND ( 'NONE', #64286, .T. ) ;
#69402 = DIRECTION ( 'NONE',  ( 0.000000000000000000, 1.000000000000000000, 0.000000000000000000 ) ) ;
#69403 = ORIENTED_EDGE ( 'NONE', *, *, #45463, .F. ) ;
#69404 = CARTESIAN_POINT ( 'NONE',  ( 5.816011393731002066, 28.73617430169783304, 5.000000000000000000 ) ) ;
#69405 = ADVANCED_FACE ( 'NONE', ( #41105 ), #141874, .F. ) ;
#69406 = VERTEX_POINT ( 'NONE', #107069 ) ;
#69407 = CARTESIAN_POINT ( 'NONE',  ( 95.95876352523144703, 0.000000000000000000, -6.110000000000001208 ) ) ;
#69408 = ADVANCED_FACE ( 'NONE', ( #30969 ), #31667, .F. ) ;
#69409 = FACE_OUTER_BOUND ( 'NONE', #106002, .T. ) ;
#69410 = DIRECTION ( 'NONE',  ( 0.7071067811865486830, -0.7071067811865464625, -0.000000000000000000 ) ) ;
#69411 = VECTOR ( 'NONE', #1650, 1000.000000000000000 ) ;
#69412 = LINE ( 'NONE', #13556, #46990 ) ;
#69413 = CARTESIAN_POINT ( 'NONE',  ( 124.4403572661730948, -44.90675832753631624, -35.11767176072513763 ) ) ;
#69414 = ORIENTED_EDGE ( 'NONE', *, *, #42204, .F. ) ;
#69415 = CONICAL_SURFACE ( 'NONE', #6837, 2.055000000000000160, 1.047197551196600962 ) ;
#69416 = CIRCLE ( 'NONE', #6838, 2.552699999999997971 ) ;
#69417 = AXIS2_PLACEMENT_3D ( 'NONE', #112575, #3091, #124164 ) ;
#69418 = CARTESIAN_POINT ( 'NONE',  ( 2.292893218813447209, -6.740707523384214639, 5.000000000000000000 ) ) ;
#69419 = ADVANCED_FACE ( 'NONE', ( #63608 ), #108456, .F. ) ;
#69420 = AXIS2_PLACEMENT_3D ( 'NONE', #6661, #59691, #27745 ) ;
#69421 = CARTESIAN_POINT ( 'NONE',  ( 39.48921356237310221, -27.52281430457082934, 5.000000000000000000 ) ) ;
#69422 = VERTEX_POINT ( 'NONE', #42569 ) ;
#69423 = DIRECTION ( 'NONE',  ( -0.6830127018922181881, 0.6830127018922202975, -0.2588190451025214056 ) ) ;
#69424 = CARTESIAN_POINT ( 'NONE',  ( 6.938893903907228378E-15, 4.552185695429122880, 5.000000000000000000 ) ) ;
#69426 = EDGE_LOOP ( 'NONE', ( #133158, #117054, #34149, #81227 ) ) ;
#69425 = CARTESIAN_POINT ( 'NONE',  ( 21.46453280170069888, -2.055000000000000160, 2.689687640572715640E-16 ) ) ;
#69427 = CARTESIAN_POINT ( 'NONE',  ( 42.18398860626899705, 28.73617430169816700, 5.000000000000000000 ) ) ;
#69428 = LINE ( 'NONE', #3408, #137842 ) ;
#69429 = LINE ( 'NONE', #79632, #60926 ) ;
#69430 = CARTESIAN_POINT ( 'NONE',  ( -10.49999999999992184, -13.91253812416061031, 4.000000000000000000 ) ) ;
#69431 = FACE_OUTER_BOUND ( 'NONE', #11745, .T. ) ;
#69432 = ORIENTED_EDGE ( 'NONE', *, *, #121014, .F. ) ;
#69433 = ORIENTED_EDGE ( 'NONE', *, *, #60846, .T. ) ;
#69434 = VERTEX_POINT ( 'NONE', #85301 ) ;
#69435 = CARTESIAN_POINT ( 'NONE',  ( 82.10459685856476142, 1.637169565754164946, -6.109999999999999432 ) ) ;
#69436 = VECTOR ( 'NONE', #81130, 1000.000000000000000 ) ;
#69437 = VERTEX_POINT ( 'NONE', #129524 ) ;
#69438 = EDGE_CURVE ( 'NONE', #103754, #13745, #85306, .T. ) ;
#69439 = DIRECTION ( 'NONE',  ( 0.7071067811865486830, -0.7071067811865464625, -0.000000000000000000 ) ) ;
#69440 = CARTESIAN_POINT ( 'NONE',  ( -29.99999999999979394, 4.965500833774300737, -4.007596771432589300 ) ) ;
#69441 = DIRECTION ( 'NONE',  ( -0.6830127018922180770, -0.6830127018922204085, -0.2588190451025213501 ) ) ;
#69442 = PLANE ( 'NONE',  #13299 ) ;
#69443 = VERTEX_POINT ( 'NONE', #64293 ) ;
#69444 = PLANE ( 'NONE',  #116214 ) ;
#69445 = DIRECTION ( 'NONE',  ( -0.6830127018922181881, 0.6830127018922202975, -0.2588190451025214056 ) ) ;
#69446 = CARTESIAN_POINT ( 'NONE',  ( -4.499999999999968914, -15.29013452822854724, 0.3645803511610244962 ) ) ;
#69447 = VECTOR ( 'NONE', #65875, 1000.000000000000000 ) ;
#69448 = CARTESIAN_POINT ( 'NONE',  ( 78.22459685856479439, -1.637169565754160949, 6.109999999999997655 ) ) ;
#69449 = ORIENTED_EDGE ( 'NONE', *, *, #51783, .F. ) ;
#69450 = EDGE_CURVE ( 'NONE', #130548, #63481, #53409, .T. ) ;
#69451 = LINE ( 'NONE', #70195, #139302 ) ;
#69452 = FACE_OUTER_BOUND ( 'NONE', #124905, .T. ) ;
#69453 = PLANE ( 'NONE',  #125659 ) ;
#69454 = AXIS2_PLACEMENT_3D ( 'NONE', #30170, #74419, #8382 ) ;
#69455 = VECTOR ( 'NONE', #9437, 1000.000000000000000 ) ;
#69456 = ORIENTED_EDGE ( 'NONE', *, *, #88408, .F. ) ;
#69457 = ORIENTED_EDGE ( 'NONE', *, *, #143270, .F. ) ;
#69458 = EDGE_CURVE ( 'NONE', #137730, #71992, #45426, .T. ) ;
#69459 = LINE ( 'NONE', #110762, #21361 ) ;
#69460 = VECTOR ( 'NONE', #2717, 1000.000000000000000 ) ;
#69461 = LINE ( 'NONE', #14341, #84805 ) ;
#69462 = EDGE_CURVE ( 'NONE', #66625, #53418, #46038, .T. ) ;
#69463 = CARTESIAN_POINT ( 'NONE',  ( 21.50456980810188412, 6.871911579029510442, -3.967499999999998916 ) ) ;
#69464 = LINE ( 'NONE', #15038, #16466 ) ;
#69465 = VECTOR ( 'NONE', #45360, 999.9999999999998863 ) ;
#69466 = PLANE ( 'NONE',  #43338 ) ;
#69467 = CARTESIAN_POINT ( 'NONE',  ( -54.18398860626899705, 28.73617430169825226, 5.000000000000000000 ) ) ;
#69468 = CARTESIAN_POINT ( 'NONE',  ( 26.12840764549667583, -3.851859888774471706E-31, 2.500000000000001332 ) ) ;
#69469 = EDGE_CURVE ( 'NONE', #26613, #68002, #33133, .T. ) ;
#69470 = ORIENTED_EDGE ( 'NONE', *, *, #111428, .T. ) ;
#69471 = ORIENTED_EDGE ( 'NONE', *, *, #45770, .T. ) ;
#69472 = DIRECTION ( 'NONE',  ( -0.7071067811865487940, 0.7071067811865463515, 0.000000000000000000 ) ) ;
#69473 = ORIENTED_EDGE ( 'NONE', *, *, #6210, .T. ) ;
#69474 = VERTEX_POINT ( 'NONE', #112092 ) ;
#69475 = VECTOR ( 'NONE', #99482, 999.9999999999998863 ) ;
#69476 = ADVANCED_FACE ( 'NONE', ( #67906 ), #112783, .F. ) ;
#69478 = EDGE_CURVE ( 'NONE', #98372, #8776, #94524, .T. ) ;
#69477 = CARTESIAN_POINT ( 'NONE',  ( 25.65999999999999659, 2.055000000000001492, 0.000000000000000000 ) ) ;
#69479 = ORIENTED_EDGE ( 'NONE', *, *, #106544, .F. ) ;
#69480 = CARTESIAN_POINT ( 'NONE',  ( 57.10002705046289861, 5.819803920172570422, 5.819803920172575751 ) ) ;
#69481 = CARTESIAN_POINT ( 'NONE',  ( -66.29974487139159578, -27.71228299555252406, 4.000000000000000000 ) ) ;
#69482 = DIRECTION ( 'NONE',  ( -0.7071067811865486830, -0.7071067811865464625, 0.000000000000000000 ) ) ;
#69483 = DIRECTION ( 'NONE',  ( -0.000000000000000000, 0.3543493200069153248, 0.9351131265310292928 ) ) ;
#69484 = AXIS2_PLACEMENT_3D ( 'NONE', #69152, #133683, #110464 ) ;
#69485 = FACE_OUTER_BOUND ( 'NONE', #44729, .T. ) ;
#69486 = EDGE_LOOP ( 'NONE', ( #139391, #77066, #24787, #4178 ) ) ;
#69487 = CARTESIAN_POINT ( 'NONE',  ( -5.994519915287488843, 28.92564299267942118, 4.000000000000000000 ) ) ;
#69488 = CYLINDRICAL_SURFACE ( 'NONE', #41860, 0.5000000000000004441 ) ;
#69489 = ORIENTED_EDGE ( 'NONE', *, *, #51359, .F. ) ;
#69490 = DIRECTION ( 'NONE',  ( 1.000000000000000000, 0.000000000000000000, 0.000000000000000000 ) ) ;
#69491 = ORIENTED_EDGE ( 'NONE', *, *, #26150, .F. ) ;
#69492 = EDGE_CURVE ( 'NONE', #55910, #68587, #22186, .T. ) ;
#69493 = ORIENTED_EDGE ( 'NONE', *, *, #74634, .F. ) ;
#69494 = DIRECTION ( 'NONE',  ( -0.6830127018922181881, 0.6830127018922202975, -0.2588190451025214056 ) ) ;
#69495 = ORIENTED_EDGE ( 'NONE', *, *, #43746, .T. ) ;
#69496 = VERTEX_POINT ( 'NONE', #1144 ) ;
#69497 = DIRECTION ( 'NONE',  ( -0.7071067811865487940, 0.7071067811865463515, -0.000000000000000000 ) ) ;
#69499 = EDGE_LOOP ( 'NONE', ( #112236, #13465, #14506, #100162 ) ) ;
#69498 = TOROIDAL_SURFACE ( 'NONE', #81082, 9.000000000000001776, 3.000000000000000000 ) ;
#69500 = VECTOR ( 'NONE', #37055, 1000.000000000000000 ) ;
#69501 = DIRECTION ( 'NONE',  ( -0.6830127018922181881, 0.6830127018922202975, -0.2588190451025214056 ) ) ;
#69502 = LINE ( 'NONE', #45618, #72793 ) ;
#69503 = CARTESIAN_POINT ( 'NONE',  ( 120.3129301918980900, -1.637169565754159617, -6.110000000000001208 ) ) ;
#69504 = DIRECTION ( 'NONE',  ( -0.7071067811865487940, 0.7071067811865463515, 0.000000000000000000 ) ) ;
#69505 = LINE ( 'NONE', #15753, #131549 ) ;
#69507 = DIRECTION ( 'NONE',  ( -0.7071067811865487940, 0.7071067811865463515, -0.000000000000000000 ) ) ;
#69506 = DIRECTION ( 'NONE',  ( -0.000000000000000000, 1.000000000000000000, 0.000000000000000000 ) ) ;
#69508 =( LENGTH_UNIT ( ) NAMED_UNIT ( * ) SI_UNIT ( .MILLI., .METRE. ) );
#69509 = CARTESIAN_POINT ( 'NONE',  ( -12.69999999999999929, -59.76999999999998892, -40.00000000000000000 ) ) ;
#69510 = FACE_OUTER_BOUND ( 'NONE', #28670, .T. ) ;
#69512 = ORIENTED_EDGE ( 'NONE', *, *, #140363, .F. ) ;
#69511 = AXIS2_PLACEMENT_3D ( 'NONE', #115816, #60810, #104970 ) ;
#69513 = DIRECTION ( 'NONE',  ( -0.6830127018922181881, 0.6830127018922202975, -0.2588190451025214056 ) ) ;
#69514 = VERTEX_POINT ( 'NONE', #44730 ) ;
#69515 = ORIENTED_EDGE ( 'NONE', *, *, #133037, .F. ) ;
#69516 = DIRECTION ( 'NONE',  ( 0.6830127018922181881, 0.6830127018922202975, -0.2588190451025214056 ) ) ;
#69517 = STYLED_ITEM ( 'NONE', ( #124950 ), #71398 ) ;
#69518 = AXIS2_PLACEMENT_3D ( 'NONE', #142810, #32640, #87000 ) ;
#69519 = ORIENTED_EDGE ( 'NONE', *, *, #57006, .T. ) ;
#69520 = AXIS2_PLACEMENT_3D ( 'NONE', #104440, #5821, #117445 ) ;
#69521 =( BOUNDED_CURVE ( )  B_SPLINE_CURVE ( 3, ( #75253, #50622, #7066, #20108 ),
 .UNSPECIFIED., .F., .T. ) 
 B_SPLINE_CURVE_WITH_KNOTS ( ( 4, 4 ),
 ( 0.000000000000000000, 1.570796326794896558 ),
 .UNSPECIFIED. ) 
 CURVE ( )  GEOMETRIC_REPRESENTATION_ITEM ( )  RATIONAL_B_SPLINE_CURVE ( ( 1.000000000000000000, 0.8047378541243649375, 0.8047378541243649375, 1.000000000000000000 ) ) 
 REPRESENTATION_ITEM ( '' )  );
#69522 = AXIS2_PLACEMENT_3D ( 'NONE', #70933, #121872, #91938 ) ;
#69523 = DIRECTION ( 'NONE',  ( -0.000000000000000000, 0.000000000000000000, 1.000000000000000000 ) ) ;
#69524 = CARTESIAN_POINT ( 'NONE',  ( 51.29974487139158867, -27.71228299555242103, 4.000000000000000000 ) ) ;
#69525 = CARTESIAN_POINT ( 'NONE',  ( 8.700255128608413102, -27.71228299555199825, 4.000000000000000000 ) ) ;
#69526 = DIRECTION ( 'NONE',  ( 0.7071067811865487940, 0.7071067811865463515, 0.000000000000000000 ) ) ;
#69527 = LINE ( 'NONE', #102146, #139041 ) ;
#69528 = ADVANCED_FACE ( 'NONE', ( #102645 ), #88924, .F. ) ;
#69529 = EDGE_LOOP ( 'NONE', ( #74866, #74167, #104266, #88029 ) ) ;
#69530 = DIRECTION ( 'NONE',  ( -0.7071067811865486830, -0.7071067811865464625, 0.000000000000000000 ) ) ;
#69532 = VERTEX_POINT ( 'NONE', #34515 ) ;
#69531 = AXIS2_PLACEMENT_3D ( 'NONE', #61405, #28018, #125185 ) ;
#69533 = CARTESIAN_POINT ( 'NONE',  ( 25.39999999999999858, 0.000000000000000000, 6.094999999999989093 ) ) ;
#69534 = ADVANCED_FACE ( 'NONE', ( #46131 ), #88194, .F. ) ;
#69535 = CARTESIAN_POINT ( 'NONE',  ( 24.71290314143521982, 3.967499999999992699, -6.871911579029513994 ) ) ;
#69536 = ORIENTED_EDGE ( 'NONE', *, *, #105688, .T. ) ;
#69537 = EDGE_CURVE ( 'NONE', #93801, #123539, #56318, .T. ) ;
#69538 = CARTESIAN_POINT ( 'NONE',  ( 9.182220855195383891, -8.505056546645496596, 4.232972564478894029 ) ) ;
#69539 = CARTESIAN_POINT ( 'NONE',  ( 99.24586038379624142, 3.974999999999996980, 6.884901960086287964 ) ) ;
#69540 = ORIENTED_EDGE ( 'NONE', *, *, #136558, .F. ) ;
#69541 = ORIENTED_EDGE ( 'NONE', *, *, #113763, .T. ) ;
#69542 = EDGE_CURVE ( 'NONE', #39180, #35044, #42442, .T. ) ;
#69543 = ORIENTED_EDGE ( 'NONE', *, *, #133203, .T. ) ;
#69545 =( GEOMETRIC_REPRESENTATION_CONTEXT ( 3 ) GLOBAL_UNCERTAINTY_ASSIGNED_CONTEXT ( ( #112863 ) ) GLOBAL_UNIT_ASSIGNED_CONTEXT ( ( #130384, #73845, #8534 ) ) REPRESENTATION_CONTEXT ( 'NONE', 'WORKASPACE' ) );
#69544 = CARTESIAN_POINT ( 'NONE',  ( 35.99451991528749772, 28.92564299267963079, 4.000000000000000000 ) ) ;
#69546 = DIRECTION ( 'NONE',  ( -0.7071067811865486830, -0.7071067811865464625, 0.000000000000000000 ) ) ;
#69547 = DIRECTION ( 'NONE',  ( -0.7071067811865486830, -0.7071067811865464625, 0.000000000000000000 ) ) ;
#69548 = EDGE_CURVE ( 'NONE', #9933, #86313, #110615, .T. ) ;
#69549 = CARTESIAN_POINT ( 'NONE',  ( -12.48921356237309155, -27.52281430457064104, 5.000000000000000000 ) ) ;
#69550 = ORIENTED_EDGE ( 'NONE', *, *, #99233, .T. ) ;
#69551 = FACE_OUTER_BOUND ( 'NONE', #108078, .T. ) ;
#69552 = LINE ( 'NONE', #113739, #80443 ) ;
#69553 = AXIS2_PLACEMENT_3D ( 'NONE', #33774, #35919, #69247 ) ;
#69554 = AXIS2_PLACEMENT_3D ( 'NONE', #35080, #48084, #69128 ) ;
#69555 = EDGE_CURVE ( 'NONE', #110525, #138330, #55339, .T. ) ;
#69556 = CARTESIAN_POINT ( 'NONE',  ( -2.816011393730999401, 28.73617430169785436, 5.000000000000000000 ) ) ;
#69557 = CARTESIAN_POINT ( 'NONE',  ( 63.48921356237309510, -27.52281430457099631, 5.000000000000000000 ) ) ;
#69558 = VECTOR ( 'NONE', #7490, 1000.000000000000227 ) ;
#69559 = ORIENTED_EDGE ( 'NONE', *, *, #121073, .F. ) ;
#69561 = CIRCLE ( 'NONE', #81041, 3.113037248396092416 ) ;
#69560 = FACE_OUTER_BOUND ( 'NONE', #38019, .T. ) ;
#69562 = ORIENTED_EDGE ( 'NONE', *, *, #128574, .T. ) ;
#69563 = EDGE_CURVE ( 'NONE', #120482, #138203, #68594, .T. ) ;
#69565 = ORIENTED_EDGE ( 'NONE', *, *, #142705, .T. ) ;
#69564 = CARTESIAN_POINT ( 'NONE',  ( 56.09195796767219377, -46.73296206246176610, -36.09967824800666136 ) ) ;
#69566 = EDGE_LOOP ( 'NONE', ( #84657, #121277, #44585, #9984 ) ) ;
#69567 = EDGE_CURVE ( 'NONE', #2398, #81201, #33819, .T. ) ;
#69568 = VECTOR ( 'NONE', #117807, 1000.000000000000000 ) ;
#69569 = CARTESIAN_POINT ( 'NONE',  ( -3.461603553705685954, -9.740707523384180888, 17.74957260769609846 ) ) ;
#69570 = CARTESIAN_POINT ( 'NONE',  ( 39.18398860626899705, 28.73617430169814568, 5.000000000000000000 ) ) ;
#69571 = VERTEX_POINT ( 'NONE', #122215 ) ;
#69572 =( LENGTH_UNIT ( ) NAMED_UNIT ( * ) SI_UNIT ( .MILLI., .METRE. ) );
#69573 = UNCERTAINTY_MEASURE_WITH_UNIT (LENGTH_MEASURE( 1.000000000000000082E-05 ), #63765, 'distance_accuracy_value', 'NONE');
#69574 = ORIENTED_EDGE ( 'NONE', *, *, #21580, .F. ) ;
#69575 = EDGE_CURVE ( 'NONE', #15438, #132789, #115499, .T. ) ;
#69576 = CARTESIAN_POINT ( 'NONE',  ( -39.18398860626899705, 28.73617430169814568, 5.000000000000000000 ) ) ;
#69577 = DIRECTION ( 'NONE',  ( 1.000000000000000000, 0.000000000000000000, 0.000000000000000000 ) ) ;
#69578 = DIRECTION ( 'NONE',  ( 0.6830127018922180770, -0.6830127018922204085, -0.2588190451025213501 ) ) ;
#69579 = AXIS2_PLACEMENT_3D ( 'NONE', #90129, #67715, #101002 ) ;
#69580 = CARTESIAN_POINT ( 'NONE',  ( -1.828169399223514624, 15.75929247661555443, 4.000000000000000000 ) ) ;
#69581 = DIRECTION ( 'NONE',  ( -0.6830127018922181881, 0.6830127018922202975, -0.2588190451025214056 ) ) ;
#69582 = CARTESIAN_POINT ( 'NONE',  ( -17.27718569542927796, -21.72500000000000142, 5.000000000000000000 ) ) ;
#69583 = DIRECTION ( 'NONE',  ( -1.000000000000000000, -1.224606353822377258E-16, -0.000000000000000000 ) ) ;
#69585 = AXIS2_PLACEMENT_3D ( 'NONE', #15163, #24630, #37679 ) ;
#69584 = CARTESIAN_POINT ( 'NONE',  ( 19.52040314143522437, 7.934999999999989839, -2.126176841940961904 ) ) ;
#69586 = CARTESIAN_POINT ( 'NONE',  ( 0.1600000000000009748, -7.113645484598424495, 3.515717980648092045 ) ) ;
#69587 = CARTESIAN_POINT ( 'NONE',  ( 25.49999999999982947, 16.18958161055405753, -11.56426086740805559 ) ) ;
#69588 = CARTESIAN_POINT ( 'NONE',  ( 31.49999999999977973, -16.53360074219757081, 5.000000000000000000 ) ) ;
#69589 = PLANE ( 'NONE',  #22307 ) ;
#69590 = VERTEX_POINT ( 'NONE', #101911 ) ;
#69591 = ORIENTED_EDGE ( 'NONE', *, *, #105948, .F. ) ;
#69592 = CARTESIAN_POINT ( 'NONE',  ( 94.77083333333331439, -7.949999999999999289, -2.130196079827426203 ) ) ;
#69593 = ORIENTED_EDGE ( 'NONE', *, *, #88367, .F. ) ;
#69594 = ORIENTED_EDGE ( 'NONE', *, *, #80528, .T. ) ;
#69595 = ORIENTED_EDGE ( 'NONE', *, *, #121411, .F. ) ;
#69596 = ADVANCED_FACE ( 'NONE', ( #80192 ), #35969, .T. ) ;
#69597 = LINE ( 'NONE', #70330, #78078 ) ;
#69598 = LINE ( 'NONE', #49971, #94948 ) ;
#69599 = VECTOR ( 'NONE', #71842, 1000.000000000000227 ) ;
#69600 = CARTESIAN_POINT ( 'NONE',  ( 13.61885681777355472, 9.051170952377558976, -2.893263300195505039 ) ) ;
#69601 = ORIENTED_EDGE ( 'NONE', *, *, #142124, .F. ) ;
#69602 = CARTESIAN_POINT ( 'NONE',  ( -25.49999999999982236, -1.533600742197719580, 5.000000000000000000 ) ) ;
#69603 = DIRECTION ( 'NONE',  ( 0.3543493200069162685, -0.000000000000000000, -0.9351131265310288487 ) ) ;
#69604 = PLANE ( 'NONE',  #18558 ) ;
#69605 = CARTESIAN_POINT ( 'NONE',  ( 126.8279612232013562, 4.169058294950168886, 5.151117689787611198 ) ) ;
#69606 = CARTESIAN_POINT ( 'NONE',  ( 128.8287635252314658, 0.000000000000000000, -6.109999999999998543 ) ) ;
#69607 = CARTESIAN_POINT ( 'NONE',  ( -25.17183060077629619, 15.75929247661555976, 4.000000000000000000 ) ) ;
#69608 = CARTESIAN_POINT ( 'NONE',  ( -9.707106781186471522, -12.74070752338415602, 5.000000000000000000 ) ) ;
#69609 = CARTESIAN_POINT ( 'NONE',  ( 48.48921356237309510, -27.52281430457089328, 5.000000000000000000 ) ) ;
#69610 = FACE_OUTER_BOUND ( 'NONE', #20727, .T. ) ;
#69611 = CIRCLE ( 'NONE', #41842, 2.500000000000000888 ) ;
#69612 = DIRECTION ( 'NONE',  ( -0.000000000000000000, 0.3543493200069153248, 0.9351131265310292928 ) ) ;
#69613 = CARTESIAN_POINT ( 'NONE',  ( 2.999999999999999112, -43.14999999999999147, 40.92499999999998295 ) ) ;
#69614 = VECTOR ( 'NONE', #88436, 1000.000000000000000 ) ;
#69615 = DIRECTION ( 'NONE',  ( 1.000000000000000000, -0.000000000000000000, 0.000000000000000000 ) ) ;
#69616 = CARTESIAN_POINT ( 'NONE',  ( 42.18398860626899705, 28.73617430169816700, 5.000000000000000000 ) ) ;
#69617 = ORIENTED_EDGE ( 'NONE', *, *, #92965, .T. ) ;
#69618 = VERTEX_POINT ( 'NONE', #16292 ) ;
#69619 = CARTESIAN_POINT ( 'NONE',  ( 110.8337635252314470, 6.110000000000001208, 1.122388791418549305E-15 ) ) ;
#69620 = ORIENTED_EDGE ( 'NONE', *, *, #60045, .F. ) ;
#69621 = ADVANCED_FACE ( 'NONE', ( #3292 ), #5424, .F. ) ;
#69622 = DIRECTION ( 'NONE',  ( 0.000000000000000000, -1.000000000000000000, 0.000000000000000000 ) ) ;
#69623 = CARTESIAN_POINT ( 'NONE',  ( 18.18398860626898994, 28.73617430169800002, 5.000000000000000000 ) ) ;
#69624 = VECTOR ( 'NONE', #130902, 1000.000000000000000 ) ;
#69625 = LINE ( 'NONE', #60164, #83757 ) ;
#69626 = DIRECTION ( 'NONE',  ( -0.7071067811865486830, -0.7071067811865464625, -0.000000000000000000 ) ) ;
#69627 = VECTOR ( 'NONE', #95652, 1000.000000000000000 ) ;
#69628 = CARTESIAN_POINT ( 'NONE',  ( 105.2037635252314516, 6.109999999999998543, 1.122388791418548911E-15 ) ) ;
#69629 = EDGE_LOOP ( 'NONE', ( #69323, #114144, #83022, #105121 ) ) ;
#69630 = EDGE_CURVE ( 'NONE', #58576, #82619, #27916, .T. ) ;
#69631 = ORIENTED_EDGE ( 'NONE', *, *, #36800, .T. ) ;
#69632 = CARTESIAN_POINT ( 'NONE',  ( 12.25000000000000000, -7.464222240803106570E-16, -6.094999999999989981 ) ) ;
#69633 = VECTOR ( 'NONE', #26200, 1000.000000000000000 ) ;
#69634 = VECTOR ( 'NONE', #57088, 1000.000000000000000 ) ;
#69635 = VECTOR ( 'NONE', #55453, 1000.000000000000000 ) ;
#69636 = CARTESIAN_POINT ( 'NONE',  ( 98.12500000000000000, -7.950000000000000178, -4.867971026610729436E-16 ) ) ;
#69637 = VECTOR ( 'NONE', #19211, 1000.000000000000227 ) ;
#69638 = ORIENTED_EDGE ( 'NONE', *, *, #114239, .F. ) ;
#69639 = ORIENTED_EDGE ( 'NONE', *, *, #136940, .F. ) ;
#69640 = EDGE_CURVE ( 'NONE', #130911, #23774, #39079, .T. ) ;
#69641 = VERTEX_POINT ( 'NONE', #38802 ) ;
#69642 = PLANE ( 'NONE',  #60733 ) ;
#69643 = FILL_AREA_STYLE_COLOUR ( '', #64630 ) ;
#69644 = AXIS2_PLACEMENT_3D ( 'NONE', #31778, #96274, #31080 ) ;
#69645 = VERTEX_POINT ( 'NONE', #114887 ) ;
#69646 = VERTEX_POINT ( 'NONE', #6119 ) ;
#69647 = CARTESIAN_POINT ( 'NONE',  ( -26.27718569542921401, -21.72499999999999432, 5.000000000000000000 ) ) ;
#69648 = ORIENTED_EDGE ( 'NONE', *, *, #38603, .T. ) ;
#69649 = ORIENTED_EDGE ( 'NONE', *, *, #38469, .T. ) ;
#69650 = AXIS2_PLACEMENT_3D ( 'NONE', #52593, #85213, #19957 ) ;
#69651 = CARTESIAN_POINT ( 'NONE',  ( -6.489213562373093325, -27.52281430457059841, 5.000000000000000000 ) ) ;
#69652 = VECTOR ( 'NONE', #137904, 999.9999999999998863 ) ;
#69654 = DIRECTION ( 'NONE',  ( 0.7071067811865487940, -0.7071067811865463515, 0.000000000000000000 ) ) ;
#69653 = VECTOR ( 'NONE', #132930, 1000.000000000000000 ) ;
#69655 = CARTESIAN_POINT ( 'NONE',  ( -17.99451991528748351, 28.92564299267950645, 4.000000000000000000 ) ) ;
#69656 = EDGE_CURVE ( 'NONE', #43279, #82989, #60589, .T. ) ;
#69657 = ORIENTED_EDGE ( 'NONE', *, *, #84816, .T. ) ;
#69658 = DIRECTION ( 'NONE',  ( -0.7071067811865486830, -0.7071067811865464625, 0.000000000000000000 ) ) ;
#69659 = VECTOR ( 'NONE', #25509, 999.9999999999998863 ) ;
#69660 = DIRECTION ( 'NONE',  ( 1.000000000000000000, 0.000000000000000000, 0.000000000000000000 ) ) ;
#69661 = VECTOR ( 'NONE', #134455, 1000.000000000000227 ) ;
#69662 =( LENGTH_UNIT ( ) NAMED_UNIT ( * ) SI_UNIT ( .MILLI., .METRE. ) );
#69663 = EDGE_CURVE ( 'NONE', #71793, #47857, #69205, .T. ) ;
#69664 = FACE_BOUND ( 'NONE', #56757, .T. ) ;
#69665 = ORIENTED_EDGE ( 'NONE', *, *, #133971, .F. ) ;
#69666 = PLANE ( 'NONE',  #136016 ) ;
#69667 = CARTESIAN_POINT ( 'NONE',  ( 17.99999999999987566, -3.033600742197710254, 5.000000000000000000 ) ) ;
#69668 = STYLED_ITEM ( 'NONE', ( #55457 ), #82181 ) ;
#69669 = CARTESIAN_POINT ( 'NONE',  ( -23.29289321881329045, -9.740707523384187994, 5.000000000000000000 ) ) ;
#69670 = EDGE_CURVE ( 'NONE', #108960, #118884, #46139, .T. ) ;
#69671 = ORIENTED_EDGE ( 'NONE', *, *, #101575, .T. ) ;
#69672 = DIRECTION ( 'NONE',  ( 0.3543493200069163240, 0.000000000000000000, -0.9351131265310288487 ) ) ;
#69673 = VERTEX_POINT ( 'NONE', #125821 ) ;
#69674 = ORIENTED_EDGE ( 'NONE', *, *, #54876, .T. ) ;
#69675 = ORIENTED_EDGE ( 'NONE', *, *, #112062, .F. ) ;
#69676 = PRODUCT_RELATED_PRODUCT_CATEGORY ( 'part', '', ( #32831 ) ) ;
#69677 = CARTESIAN_POINT ( 'NONE',  ( 40.45376352523144448, -6.109999999999998543, -3.741295971395162543E-16 ) ) ;
#69678 = ORIENTED_EDGE ( 'NONE', *, *, #98802, .T. ) ;
#69679 = AXIS2_PLACEMENT_3D ( 'NONE', #3355, #70808, #59235 ) ;
#69680 = CARTESIAN_POINT ( 'NONE',  ( 7.637717201596474048, -2.500000000000000444, 3.061616997868384127E-16 ) ) ;
#69681 = CARTESIAN_POINT ( 'NONE',  ( -38.99451991528749062, 28.92564299267965211, 4.000000000000000000 ) ) ;
#69682 = LINE ( 'NONE', #24010, #128470 ) ;
#69683 = ORIENTED_EDGE ( 'NONE', *, *, #118062, .T. ) ;
#69684 = LINE ( 'NONE', #101549, #16750 ) ;
#69686 = SURFACE_STYLE_FILL_AREA ( #59516 ) ;
#69685 = VECTOR ( 'NONE', #10537, 1000.000000000000000 ) ;
#69687 = EDGE_CURVE ( 'NONE', #62641, #91232, #36643, .T. ) ;
#69688 = DIRECTION ( 'NONE',  ( -0.000000000000000000, -0.3543493200069152693, 0.9351131265310292928 ) ) ;
#69689 = CARTESIAN_POINT ( 'NONE',  ( 156.1500000000000057, -57.14999999999999147, 45.92499999999998295 ) ) ;
#69690 = LINE ( 'NONE', #16695, #138890 ) ;
#69691 = LINE ( 'NONE', #23270, #66828 ) ;
#69692 = DIRECTION ( 'NONE',  ( 1.000000000000000000, 0.000000000000000000, 0.000000000000000000 ) ) ;
#69693 = VERTEX_POINT ( 'NONE', #49704 ) ;
#69694 = ORIENTED_EDGE ( 'NONE', *, *, #77316, .F. ) ;
#69695 = ORIENTED_EDGE ( 'NONE', *, *, #89367, .T. ) ;
#69696 = PRESENTATION_LAYER_ASSIGNMENT (  '', '', ( #14075 ) ) ;
#69697 = EDGE_LOOP ( 'NONE', ( #14869, #137078, #30397, #45755 ) ) ;
#69698 = EDGE_LOOP ( 'NONE', ( #75848, #32871, #127782, #22261 ) ) ;
#69699 = VERTEX_POINT ( 'NONE', #4675 ) ;
#69700 = CARTESIAN_POINT ( 'NONE',  ( -8.816011393731004731, 28.73617430169781173, 5.000000000000000000 ) ) ;
#69701 = PLANE ( 'NONE',  #76335 ) ;
#69702 = ORIENTED_EDGE ( 'NONE', *, *, #29253, .F. ) ;
#69703 = CARTESIAN_POINT ( 'NONE',  ( 16.49999999999988631, -2.947814304570806065, 5.000000000000000000 ) ) ;
#69704 = VECTOR ( 'NONE', #62452, 1000.000000000000000 ) ;
#69705 = EDGE_LOOP ( 'NONE', ( #47650, #142722, #11023, #95654 ) ) ;
#69706 =( BOUNDED_CURVE ( )  B_SPLINE_CURVE ( 2, ( #64795, #54635, #98822, #107562, #64075, #74978, #21979, #141643, #74238, #53180, #140896, #143054, #43745 ),
 .UNSPECIFIED., .F., .T. ) 
 B_SPLINE_CURVE_WITH_KNOTS ( ( 3, 2, 2, 2, 2, 2, 3 ),
 ( 0.4000000000000001332, 0.4083333333333334370, 0.4166666666666667407, 0.4250000000000000444, 0.4333333333333334036, 0.4416666666666666519, 0.4500000000000000111 ),
 .UNSPECIFIED. ) 
 CURVE ( )  GEOMETRIC_REPRESENTATION_ITEM ( )  RATIONAL_B_SPLINE_CURVE ( ( 0.9999999999999995559, 0.9659258262890687563, 1.000000000000000000, 0.9659258262890683122, 1.000000000000000000, 0.9659258262890683122, 1.000000000000000000, 0.9659258262890683122, 1.000000000000000000, 0.9659258262890683122, 1.000000000000000000, 0.9659258262890683122, 1.000000000000000000 ) ) 
 REPRESENTATION_ITEM ( '' )  );
#69707 = CARTESIAN_POINT ( 'NONE',  ( 0.2569208697893814453, 4.202752102959690472E-16, 0.000000000000000000 ) ) ;
#69708 = CARTESIAN_POINT ( 'NONE',  ( -7.499999999999943157, -13.91253812416061386, 4.000000000000000000 ) ) ;
#69709 = EDGE_CURVE ( 'NONE', #129523, #69972, #26497, .T. ) ;
#69710 = CARTESIAN_POINT ( 'NONE',  ( 4.296236474768552860, 7.934999999999990727, -1.457635852685135314E-15 ) ) ;
#69711 = ORIENTED_EDGE ( 'NONE', *, *, #143542, .T. ) ;
#69713 = CARTESIAN_POINT ( 'NONE',  ( 2.999999999999985345, 11.58746187583912324, 4.000000000000000000 ) ) ;
#69712 = CARTESIAN_POINT ( 'NONE',  ( 111.6204301918981088, 3.055000000000002380, -5.291415217122917625 ) ) ;
#69714 = EDGE_CURVE ( 'NONE', #83476, #86617, #39533, .T. ) ;
#69715 = CARTESIAN_POINT ( 'NONE',  ( -0.4892135623730947680, -27.52281430457055578, 5.000000000000000000 ) ) ;
#69716 = DIRECTION ( 'NONE',  ( -0.6830127018922180770, -0.6830127018922204085, -0.2588190451025213501 ) ) ;
#69717 = EDGE_LOOP ( 'NONE', ( #9399, #16673, #91698, #8175 ) ) ;
#69718 = FILL_AREA_STYLE_COLOUR ( '', #114424 ) ;
#69719 = ORIENTED_EDGE ( 'NONE', *, *, #82956, .F. ) ;
#69720 = DIRECTION ( 'NONE',  ( 0.000000000000000000, -1.000000000000000000, 0.000000000000000000 ) ) ;
#69721 = LINE ( 'NONE', #16729, #25472 ) ;
#69722 = LINE ( 'NONE', #15977, #3375 ) ;
#69723 = VECTOR ( 'NONE', #139059, 1000.000000000000000 ) ;
#69724 = CARTESIAN_POINT ( 'NONE',  ( 14.42840764549667476, -3.851859888774471706E-31, 2.500000000000001332 ) ) ;
#69725 = EDGE_CURVE ( 'NONE', #134832, #60397, #125087, .T. ) ;
#69726 = EDGE_CURVE ( 'NONE', #96542, #92295, #15566, .T. ) ;
#69727 = ORIENTED_EDGE ( 'NONE', *, *, #11788, .F. ) ;
#69728 = VECTOR ( 'NONE', #38813, 1000.000000000000000 ) ;
#69729 = CARTESIAN_POINT ( 'NONE',  ( -18.00548008471250583, 28.92564299267925776, 4.000000000000000000 ) ) ;
#69730 = AXIS2_PLACEMENT_3D ( 'NONE', #4110, #89754, #136114 ) ;
#69731 = CARTESIAN_POINT ( 'NONE',  ( -2.999999999999975131, -6.412538124160689357, 4.000000000000000000 ) ) ;
#69732 = CARTESIAN_POINT ( 'NONE',  ( 18.48921356237309510, -27.52281430457068367, 5.000000000000000000 ) ) ;
#69733 = EDGE_LOOP ( 'NONE', ( #14437, #42941, #511, #107307 ) ) ;
#69734 = LINE ( 'NONE', #136373, #9610 ) ;
#69735 = AXIS2_PLACEMENT_3D ( 'NONE', #55481, #9047, #141781 ) ;
#69736 = VECTOR ( 'NONE', #130536, 1000.000000000000000 ) ;
#69737 = VECTOR ( 'NONE', #78900, 1000.000000000000114 ) ;
#69738 = PLANE ( 'NONE',  #46976 ) ;
#69740 = VERTEX_POINT ( 'NONE', #70742 ) ;
#69739 = VECTOR ( 'NONE', #121894, 1000.000000000000000 ) ;
#69741 = EDGE_CURVE ( 'NONE', #38431, #23319, #80889, .T. ) ;
#69743 = ORIENTED_EDGE ( 'NONE', *, *, #4569, .F. ) ;
#69742 = FACE_OUTER_BOUND ( 'NONE', #68451, .T. ) ;
#69744 = ADVANCED_FACE ( 'NONE', ( #47578 ), #138113, .F. ) ;
#69745 = VERTEX_POINT ( 'NONE', #138836 ) ;
#69746 = CARTESIAN_POINT ( 'NONE',  ( -7.217967065889526523, 12.56012801747615448, -25.25494078541189680 ) ) ;
#69747 = AXIS2_PLACEMENT_3D ( 'NONE', #52627, #96819, #32329 ) ;
#69748 = DIRECTION ( 'NONE',  ( 0.6830127018922180770, -0.6830127018922204085, -0.2588190451025213501 ) ) ;
#69749 = ORIENTED_EDGE ( 'NONE', *, *, #40631, .T. ) ;
#69750 = EDGE_CURVE ( 'NONE', #11057, #47805, #82318, .T. ) ;
#69751 = CARTESIAN_POINT ( 'NONE',  ( 7.799999601179139042, 3.061616997868383634E-16, -2.500000000000000444 ) ) ;
#69752 = VERTEX_POINT ( 'NONE', #93881 ) ;
#69753 = AXIS2_PLACEMENT_3D ( 'NONE', #17043, #83756, #107607 ) ;
#69754 = CARTESIAN_POINT ( 'NONE',  ( 31.92500000000001492, -6.269999999999992468, -37.00000000000000000 ) ) ;
#69755 = DIRECTION ( 'NONE',  ( -0.3543493200069163240, -0.000000000000000000, 0.9351131265310288487 ) ) ;
#69756 = FACE_OUTER_BOUND ( 'NONE', #125916, .T. ) ;
#69757 = FACE_OUTER_BOUND ( 'NONE', #58997, .T. ) ;
#69758 = VECTOR ( 'NONE', #80790, 999.9999999999998863 ) ;
#69759 = EDGE_CURVE ( 'NONE', #11112, #39875, #27191, .T. ) ;
#69760 = CARTESIAN_POINT ( 'NONE',  ( -39.29974487139159578, -27.71228299555233576, 4.000000000000000000 ) ) ;
#69761 = DIRECTION ( 'NONE',  ( 0.3543493200069162685, -0.000000000000000000, -0.9351131265310288487 ) ) ;
#69762 = DIRECTION ( 'NONE',  ( 0.6830127018922181881, 0.6830127018922202975, -0.2588190451025214056 ) ) ;
#69763 = DIRECTION ( 'NONE',  ( -0.6830127018922181881, 0.6830127018922202975, -0.2588190451025214056 ) ) ;
#69764 = ORIENTED_EDGE ( 'NONE', *, *, #22906, .F. ) ;
#69765 = AXIS2_PLACEMENT_3D ( 'NONE', #107420, #139383, #118280 ) ;
#69766 = ORIENTED_EDGE ( 'NONE', *, *, #103845, .T. ) ;
#69767 = VERTEX_POINT ( 'NONE', #17725 ) ;
#69768 = CARTESIAN_POINT ( 'NONE',  ( 117.2291666666666572, 7.950000000000001954, -2.130196079827421762 ) ) ;
#69769 = VECTOR ( 'NONE', #11799, 1000.000000000000227 ) ;
#69770 = VERTEX_POINT ( 'NONE', #103314 ) ;
#69771 = ORIENTED_EDGE ( 'NONE', *, *, #3777, .T. ) ;
#69772 = CIRCLE ( 'NONE', #67371, 2.500000000000000888 ) ;
#69773 = ORIENTED_EDGE ( 'NONE', *, *, #137841, .F. ) ;
#69774 = ADVANCED_FACE ( 'NONE', ( #3965 ), #104764, .T. ) ;
#69775 = DIRECTION ( 'NONE',  ( 0.7071067811865487940, -0.7071067811865463515, 0.000000000000000000 ) ) ;
#69776 = CARTESIAN_POINT ( 'NONE',  ( 5.994519915287488843, 28.92564299267942118, 4.000000000000000000 ) ) ;
#69777 = VECTOR ( 'NONE', #100915, 1000.000000000000000 ) ;
#69778 = ORIENTED_EDGE ( 'NONE', *, *, #105102, .F. ) ;
#69779 = LINE ( 'NONE', #134293, #104062 ) ;
#69780 = CARTESIAN_POINT ( 'NONE',  ( 33.29974487139158867, -27.71228299555229313, 4.000000000000000000 ) ) ;
#69781 = DIRECTION ( 'NONE',  ( -0.000000000000000000, -0.000000000000000000, 1.000000000000000000 ) ) ;
#69782 = CARTESIAN_POINT ( 'NONE',  ( 115.0629301918981042, 1.637169565754157174, 6.110000000000002984 ) ) ;
#69783 = VECTOR ( 'NONE', #138550, 1000.000000000000000 ) ;
#69784 = ORIENTED_EDGE ( 'NONE', *, *, #55759, .F. ) ;
#69785 = CARTESIAN_POINT ( 'NONE',  ( 9.489213562373095101, -27.52281430457062328, 5.000000000000000000 ) ) ;
#69786 = CARTESIAN_POINT ( 'NONE',  ( 105.2250270504628986, 5.819803920172573974, -5.819803920172573086 ) ) ;
#69787 = LINE ( 'NONE', #26947, #112244 ) ;
#69788 = DIRECTION ( 'NONE',  ( -0.7071067811865487940, 0.7071067811865463515, -0.000000000000000000 ) ) ;
#69789 = CARTESIAN_POINT ( 'NONE',  ( 0.000000000000000000, 0.000000000000000000, 5.000000000000000000 ) ) ;
#69790 = CARTESIAN_POINT ( 'NONE',  ( 3.183988606268992161, 28.73617430169789699, 5.000000000000000000 ) ) ;
#69791 = CARTESIAN_POINT ( 'NONE',  ( 42.66252705046289151, 7.949999999999998401, 1.460391307983218338E-15 ) ) ;
#69792 = EDGE_CURVE ( 'NONE', #68883, #73190, #107610, .T. ) ;
#69793 = DIRECTION ( 'NONE',  ( -0.7071067811865486830, -0.7071067811865464625, 0.000000000000000000 ) ) ;
#69794 = CARTESIAN_POINT ( 'NONE',  ( -39.48921356237310221, -27.52281430457082934, 5.000000000000000000 ) ) ;
#69795 = AXIS2_PLACEMENT_3D ( 'NONE', #118648, #22170, #101173 ) ;
#69796 = VERTEX_POINT ( 'NONE', #52517 ) ;
#69797 = ORIENTED_EDGE ( 'NONE', *, *, #82592, .T. ) ;
#69798 = CARTESIAN_POINT ( 'NONE',  ( 39.20833333333332860, -3.974999999999999201, -6.884901960086287964 ) ) ;
#69799 = VERTEX_POINT ( 'NONE', #128661 ) ;
#69800 = EDGE_LOOP ( 'NONE', ( #77523, #137248, #9552, #91319 ) ) ;
#69801 = CARTESIAN_POINT ( 'NONE',  ( -8.510786437626906675, -27.52281430457049183, 5.000000000000000000 ) ) ;
#69802 = AXIS2_PLACEMENT_3D ( 'NONE', #6230, #60710, #83880 ) ;
#69803 = CARTESIAN_POINT ( 'NONE',  ( 27.48921356237309155, -27.52281430457074762, 5.000000000000000000 ) ) ;
#69804 = ORIENTED_EDGE ( 'NONE', *, *, #86869, .F. ) ;
#69805 = VECTOR ( 'NONE', #50295, 1000.000000000000227 ) ;
#69806 = CARTESIAN_POINT ( 'NONE',  ( -34.92500000000001137, 22.22500000000000142, 4.000000000000000000 ) ) ;
#69807 = DIRECTION ( 'NONE',  ( 0.7071067811865487940, -0.7071067811865463515, 0.000000000000000000 ) ) ;
#69808 = LINE ( 'NONE', #60343, #123060 ) ;
#69809 = CARTESIAN_POINT ( 'NONE',  ( 27.27126352523142572, 4.472830434245839371, 4.472830434245842035 ) ) ;
#69810 = ORIENTED_EDGE ( 'NONE', *, *, #52981, .F. ) ;
#69811 = EDGE_CURVE ( 'NONE', #105583, #38928, #119889, .T. ) ;
#69812 = PLANE ( 'NONE',  #82681 ) ;
#69813 = ORIENTED_EDGE ( 'NONE', *, *, #71350, .T. ) ;
#69814 = AXIS2_PLACEMENT_3D ( 'NONE', #122098, #19932, #11908 ) ;
#69815 = CARTESIAN_POINT ( 'NONE',  ( 0.000000000000000000, -8.616843969807042924, 0.000000000000000000 ) ) ;
#69816 = CARTESIAN_POINT ( 'NONE',  ( 33.79289321881321939, 12.75929247661558819, 5.000000000000000000 ) ) ;
#69817 = PLANE ( 'NONE',  #16606 ) ;
#69818 = LINE ( 'NONE', #103120, #115839 ) ;
#69819 = VERTEX_POINT ( 'NONE', #140257 ) ;
#69820 = EDGE_CURVE ( 'NONE', #27138, #17308, #118485, .T. ) ;
#69821 = ORIENTED_EDGE ( 'NONE', *, *, #96338, .T. ) ;
#69822 = CARTESIAN_POINT ( 'NONE',  ( 20.67183060077632462, -18.74070752338408852, 4.000000000000000000 ) ) ;
#69823 = CARTESIAN_POINT ( 'NONE',  ( 0.000000000000000000, 0.000000000000000000, 10.00000000000000000 ) ) ;
#69824 = FACE_OUTER_BOUND ( 'NONE', #78137, .T. ) ;
#69825 = FACE_OUTER_BOUND ( 'NONE', #138999, .T. ) ;
#69826 = CARTESIAN_POINT ( 'NONE',  ( 57.80793019189810877, -6.109999999999998543, 1.637169565754158063 ) ) ;
#69827 = CARTESIAN_POINT ( 'NONE',  ( -33.48921356237309510, -27.52281430457078670, 5.000000000000000000 ) ) ;
#69828 = LINE ( 'NONE', #92234, #31550 ) ;
#69829 = ORIENTED_EDGE ( 'NONE', *, *, #100978, .T. ) ;
#69830 = EDGE_CURVE ( 'NONE', #105472, #103136, #98181, .T. ) ;
#69831 = ORIENTED_EDGE ( 'NONE', *, *, #135297, .T. ) ;
#69832 = CARTESIAN_POINT ( 'NONE',  ( -17.99451991528748351, 28.92564299267950645, 4.000000000000000000 ) ) ;
#69833 = VECTOR ( 'NONE', #27407, 999.9999999999998863 ) ;
#69834 = ORIENTED_EDGE ( 'NONE', *, *, #132464, .F. ) ;
#69835 = VECTOR ( 'NONE', #48815, 999.9999999999998863 ) ;
#69836 = VECTOR ( 'NONE', #78016, 1000.000000000000000 ) ;
#69837 = DIRECTION ( 'NONE',  ( 0.7071067811865487940, 0.7071067811865463515, 0.000000000000000000 ) ) ;
#69838 = EDGE_CURVE ( 'NONE', #27882, #142853, #108290, .T. ) ;
#69839 = ORIENTED_EDGE ( 'NONE', *, *, #73173, .F. ) ;
#69840 = DIRECTION ( 'NONE',  ( -0.6830127018922180770, -0.6830127018922204085, -0.2588190451025213501 ) ) ;
#69841 = AXIS2_PLACEMENT_3D ( 'NONE', #90578, #134814, #123218 ) ;
#69842 = VECTOR ( 'NONE', #25154, 999.9999999999998863 ) ;
#69843 = STYLED_ITEM ( 'NONE', ( #113755 ), #65144 ) ;
#69844 = VECTOR ( 'NONE', #48381, 999.9999999999998863 ) ;
#69845 = CARTESIAN_POINT ( 'NONE',  ( -62.99451991528749772, 28.92564299267982264, 4.000000000000000000 ) ) ;
#69846 = EDGE_CURVE ( 'NONE', #77053, #15867, #75717, .T. ) ;
#69847 = FACE_BOUND ( 'NONE', #40844, .T. ) ;
#69848 = CARTESIAN_POINT ( 'NONE',  ( 10.77149322861328073, 20.25929247661551358, 7.808871592221793279 ) ) ;
#69849 = SURFACE_SIDE_STYLE ('',( #137931 ) ) ;
#69851 = ADVANCED_FACE ( 'NONE', ( #109028 ), #64124, .T. ) ;
#69850 = LINE ( 'NONE', #137220, #112799 ) ;
#69853 = DIRECTION ( 'NONE',  ( 0.000000000000000000, 1.000000000000000000, 0.000000000000000000 ) ) ;
#69852 = VECTOR ( 'NONE', #92380, 1000.000000000000000 ) ;
#69855 = ORIENTED_EDGE ( 'NONE', *, *, #132289, .F. ) ;
#69854 = CYLINDRICAL_SURFACE ( 'NONE', #31948, 0.5000000000000004441 ) ;
#69856 = DIRECTION ( 'NONE',  ( -0.3543493200069162685, -0.000000000000000000, -0.9351131265310288487 ) ) ;
#69857 = ORIENTED_EDGE ( 'NONE', *, *, #94078, .F. ) ;
#69858 = ORIENTED_EDGE ( 'NONE', *, *, #118147, .T. ) ;
#69859 = CARTESIAN_POINT ( 'NONE',  ( 68.74543019189812298, -5.291415217122918513, -3.055000000000000160 ) ) ;
#69860 = ORIENTED_EDGE ( 'NONE', *, *, #52155, .F. ) ;
#69861 = EDGE_CURVE ( 'NONE', #132792, #31251, #21331, .T. ) ;
#69862 = VECTOR ( 'NONE', #67721, 1000.000000000000227 ) ;
#69863 = CARTESIAN_POINT ( 'NONE',  ( 3.489213562373097322, -27.52281430457057709, 5.000000000000000000 ) ) ;
#69864 = VERTEX_POINT ( 'NONE', #130100 ) ;
#69865 = DIRECTION ( 'NONE',  ( -0.3543493200069162685, -0.000000000000000000, -0.9351131265310288487 ) ) ;
#69866 = ADVANCED_FACE ( 'NONE', ( #142411 ), #42394, .F. ) ;
#69867 =( GEOMETRIC_REPRESENTATION_CONTEXT ( 3 ) GLOBAL_UNCERTAINTY_ASSIGNED_CONTEXT ( ( #3891 ) ) GLOBAL_UNIT_ASSIGNED_CONTEXT ( ( #7913, #96334, #98514 ) ) REPRESENTATION_CONTEXT ( 'NONE', 'WORKASPACE' ) );
#69868 = CARTESIAN_POINT ( 'NONE',  ( 5.281315875828549444, -2.500000000000000000, 3.061616997868383634E-16 ) ) ;
#69869 = AXIS2_PLACEMENT_3D ( 'NONE', #116501, #73709, #137553 ) ;
#69870 = CARTESIAN_POINT ( 'NONE',  ( 35.27083333333331439, -7.949999999999998401, -2.130196079827426203 ) ) ;
#69871 = CARTESIAN_POINT ( 'NONE',  ( 6.639999999999984581, -40.29840020119762301, 19.55137198191483350 ) ) ;
#69873 = SURFACE_STYLE_USAGE ( .BOTH. , #66987 ) ;
#69872 = LINE ( 'NONE', #101017, #15745 ) ;
#69874 = VECTOR ( 'NONE', #90334, 1000.000000000000000 ) ;
#69875 = DIRECTION ( 'NONE',  ( -0.7071067811865486830, -0.7071067811865464625, 0.000000000000000000 ) ) ;
#69876 = CARTESIAN_POINT ( 'NONE',  ( 78.18398860626899705, 28.73617430169841924, 5.000000000000000000 ) ) ;
#69877 = ORIENTED_EDGE ( 'NONE', *, *, #130757, .F. ) ;
#69878 = ORIENTED_EDGE ( 'NONE', *, *, #28374, .F. ) ;
#69879 = AXIS2_PLACEMENT_3D ( 'NONE', #18710, #96261, #31066 ) ;
#69880 = DIRECTION ( 'NONE',  ( -0.7071067811865486830, -0.7071067811865464625, -0.000000000000000000 ) ) ;
#69881 = DIRECTION ( 'NONE',  ( -0.000000000000000000, 0.000000000000000000, 1.000000000000000000 ) ) ;
#69882 = VERTEX_POINT ( 'NONE', #96702 ) ;
#69883 = VERTEX_POINT ( 'NONE', #106892 ) ;
#69884 = ORIENTED_EDGE ( 'NONE', *, *, #96017, .F. ) ;
#69885 = APPLICATION_CONTEXT ( 'automotive_design' ) ;
#69886 = CARTESIAN_POINT ( 'NONE',  ( 30.75000000000000000, -9.735942053221458872E-16, 7.950000000000000178 ) ) ;
#69887 = VERTEX_POINT ( 'NONE', #140948 ) ;
#69888 = CARTESIAN_POINT ( 'NONE',  ( 11.54939188068398259, -22.22500000000000142, -12.61088438758952535 ) ) ;
#69889 = MECHANICAL_DESIGN_GEOMETRIC_PRESENTATION_REPRESENTATION (  '', ( #49070 ), #28255 ) ;
#69891 = ADVANCED_FACE ( 'NONE', ( #43097 ), #97435, .F. ) ;
#69890 = DIRECTION ( 'NONE',  ( 0.7071067811865487940, 0.7071067811865463515, 0.000000000000000000 ) ) ;
#69892 = CARTESIAN_POINT ( 'NONE',  ( 2.400403141435218934, -7.934999999999989839, 2.126176841940957907 ) ) ;
#69893 = EDGE_CURVE ( 'NONE', #120153, #99498, #86603, .T. ) ;
#69894 = DIRECTION ( 'NONE',  ( -0.000000000000000000, 0.000000000000000000, 1.000000000000000000 ) ) ;
#69895 = ORIENTED_EDGE ( 'NONE', *, *, #43812, .T. ) ;
#69896 = LINE ( 'NONE', #69157, #3978 ) ;
#69897 = ADVANCED_FACE ( 'NONE', ( #95308 ), #74294, .T. ) ;
#69898 = CARTESIAN_POINT ( 'NONE',  ( 119.8083603837962272, 7.949999999999996625, 2.130196079827431088 ) ) ;
#69899 = AXIS2_PLACEMENT_3D ( 'NONE', #59635, #45371, #116112 ) ;
#69900 = CARTESIAN_POINT ( 'NONE',  ( -2.000000000000000000, -2.375000000000000000, 0.000000000000000000 ) ) ;
#69902 = ORIENTED_EDGE ( 'NONE', *, *, #134725, .T. ) ;
#69901 = LINE ( 'NONE', #22740, #42630 ) ;
#69903 = AXIS2_PLACEMENT_3D ( 'NONE', #118371, #21213, #77056 ) ;
#69904 = VERTEX_POINT ( 'NONE', #31494 ) ;
#69905 = DIRECTION ( 'NONE',  ( 0.000000000000000000, 0.000000000000000000, -1.000000000000000000 ) ) ;
#69906 = LINE ( 'NONE', #15436, #70153 ) ;
#69907 = ADVANCED_FACE ( 'NONE', ( #96019 ), #84469, .F. ) ;
#69908 = EDGE_CURVE ( 'NONE', #141201, #31209, #129359, .T. ) ;
#69909 = LINE ( 'NONE', #59041, #116499 ) ;
#69910 = EDGE_LOOP ( 'NONE', ( #103194, #139311, #84724 ) ) ;
#69911 = LINE ( 'NONE', #73270, #6524 ) ;
#69912 = FACE_OUTER_BOUND ( 'NONE', #25990, .T. ) ;
#69913 = VECTOR ( 'NONE', #15080, 1000.000000000000227 ) ;
#69914 = CARTESIAN_POINT ( 'NONE',  ( -17.93988928955969087, -9.740707523384180888, 10.89222023123385341 ) ) ;
#69915 = DIRECTION ( 'NONE',  ( -0.7071067811865486830, -0.7071067811865464625, 0.000000000000000000 ) ) ;
#69916 = CIRCLE ( 'NONE', #30564, 2.500000000000000888 ) ;
#69917 = EDGE_LOOP ( 'NONE', ( #102079, #55205, #77010, #76587 ) ) ;
#69918 = LINE ( 'NONE', #136540, #11429 ) ;
#69919 = EDGE_CURVE ( 'NONE', #64709, #36781, #30797, .T. ) ;
#69920 = DIRECTION ( 'NONE',  ( -0.000000000000000000, -0.3543493200069152693, 0.9351131265310292928 ) ) ;
#69921 = CARTESIAN_POINT ( 'NONE',  ( 0.1161069444170877152, -0.3999999999999998002, -2.220360628129161906 ) ) ;
#69922 = LINE ( 'NONE', #113361, #128113 ) ;
#69923 = ADVANCED_FACE ( 'NONE', ( #111161 ), #102994, .F. ) ;
#69924 = LINE ( 'NONE', #78618, #55291 ) ;
#69925 = VERTEX_POINT ( 'NONE', #37754 ) ;
#69926 = EDGE_CURVE ( 'NONE', #138697, #52621, #48613, .T. ) ;
#69927 = ORIENTED_EDGE ( 'NONE', *, *, #37292, .T. ) ;
#69928 = CIRCLE ( 'NONE', #130008, 2.500000000000000888 ) ;
#69929 = LINE ( 'NONE', #111976, #19240 ) ;
#69930 = CARTESIAN_POINT ( 'NONE',  ( 8.437069808101885116, 2.126176841940952134, -7.934999999999993392 ) ) ;
#69931 = CARTESIAN_POINT ( 'NONE',  ( 4.171830600776443632, 9.759292476615621936, 4.000000000000000000 ) ) ;
#69932 = ADVANCED_FACE ( 'NONE', ( #251 ), #126176, .T. ) ;
#69933 = CARTESIAN_POINT ( 'NONE',  ( -32.99451991528749062, 28.92564299267960948, 4.000000000000000000 ) ) ;
#69934 = CARTESIAN_POINT ( 'NONE',  ( -33.48921356237309510, -27.52281430457078670, 5.000000000000000000 ) ) ;
#69935 = ADVANCED_FACE ( 'NONE', ( #81992 ), #65589, .F. ) ;
#69936 = DIRECTION ( 'NONE',  ( -0.6830127018922180770, -0.6830127018922204085, -0.2588190451025213501 ) ) ;
#69937 = EDGE_LOOP ( 'NONE', ( #53308, #88452, #47186, #60442, #72809 ) ) ;
#69938 = LINE ( 'NONE', #79393, #129871 ) ;
#69939 = CARTESIAN_POINT ( 'NONE',  ( -0.7070132642930445632, -21.74070752338405654, 4.999753212805222446 ) ) ;
#69941 = EDGE_CURVE ( 'NONE', #60486, #70075, #22026, .T. ) ;
#69940 = VECTOR ( 'NONE', #121399, 1000.000000000000227 ) ;
#69942 = VECTOR ( 'NONE', #31181, 1000.000000000000000 ) ;
#69943 = DIRECTION ( 'NONE',  ( -0.3543493200069163240, -0.000000000000000000, 0.9351131265310288487 ) ) ;
#69944 = CARTESIAN_POINT ( 'NONE',  ( 59.41209685856478728, 5.291415217122922066, -3.054999999999995275 ) ) ;
#69945 =( BOUNDED_CURVE ( )  B_SPLINE_CURVE ( 3, ( #82845, #50213, #125636, #37920 ),
 .UNSPECIFIED., .F., .F. ) 
 B_SPLINE_CURVE_WITH_KNOTS ( ( 4, 4 ),
 ( 3.581556339957213897, 3.677360298529522176 ),
 .UNSPECIFIED. ) 
 CURVE ( )  GEOMETRIC_REPRESENTATION_ITEM ( )  RATIONAL_B_SPLINE_CURVE ( ( 1.000000000000000000, 0.9992352797041761381, 0.9992352797041761381, 1.000000000000000000 ) ) 
 REPRESENTATION_ITEM ( '' )  );
#69946 = DIRECTION ( 'NONE',  ( 0.3543493200069162685, -0.000000000000000000, -0.9351131265310288487 ) ) ;
#69947 = AXIS2_PLACEMENT_3D ( 'NONE', #68420, #13259, #47400 ) ;
#69948 = SURFACE_STYLE_FILL_AREA ( #27099 ) ;
#69949 = ORIENTED_EDGE ( 'NONE', *, *, #749, .T. ) ;
#69950 = DIRECTION ( 'NONE',  ( 0.7071067811865487940, 0.7071067811865463515, 0.000000000000000000 ) ) ;
#69951 = ORIENTED_EDGE ( 'NONE', *, *, #92415, .T. ) ;
#69952 = AXIS2_PLACEMENT_3D ( 'NONE', #38038, #138773, #40195 ) ;
#69953 = EDGE_CURVE ( 'NONE', #122015, #84039, #109758, .T. ) ;
#69954 = AXIS2_PLACEMENT_3D ( 'NONE', #134652, #24433, #2663 ) ;
#69955 = DIRECTION ( 'NONE',  ( -0.7071067811865487940, 0.7071067811865463515, 0.000000000000000000 ) ) ;
#69956 = AXIS2_PLACEMENT_3D ( 'NONE', #95277, #71405, #82993 ) ;
#69957 = CARTESIAN_POINT ( 'NONE',  ( 66.29974487139159578, -27.71228299555252406, 4.000000000000000000 ) ) ;
#69958 = DIRECTION ( 'NONE',  ( 0.6830127018922180770, -0.6830127018922204085, -0.2588190451025213501 ) ) ;
#69959 = CARTESIAN_POINT ( 'NONE',  ( 54.48921356237310221, -27.52281430457093236, 5.000000000000000000 ) ) ;
#69960 = DIRECTION ( 'NONE',  ( -1.000000000000000000, -0.000000000000000000, -0.000000000000000000 ) ) ;
#69961 = FILL_AREA_STYLE ('',( #125738 ) ) ;
#69962 = VERTEX_POINT ( 'NONE', #10431 ) ;
#69963 = VERTEX_POINT ( 'NONE', #59511 ) ;
#69964 = DIRECTION ( 'NONE',  ( 0.7071067811865487940, 0.7071067811865463515, -0.000000000000000000 ) ) ;
#69965 = CARTESIAN_POINT ( 'NONE',  ( 42.29974487139158157, -27.71228299555235708, 4.000000000000000000 ) ) ;
#69966 = EDGE_CURVE ( 'NONE', #131683, #3009, #43797, .T. ) ;
#69967 = PLANE ( 'NONE',  #3344 ) ;
#69968 = DIRECTION ( 'NONE',  ( -0.7071067811865486830, -0.7071067811865464625, 0.000000000000000000 ) ) ;
#69969 = CARTESIAN_POINT ( 'NONE',  ( 73.14169371712957002, -2.130196079827424871, -7.949999999999999289 ) ) ;
#69970 = ADVANCED_FACE ( 'NONE', ( #125465 ), #124739, .F. ) ;
#69971 = CARTESIAN_POINT ( 'NONE',  ( 44.99451991528749772, 28.92564299267969474, 4.000000000000000000 ) ) ;
#69972 = VERTEX_POINT ( 'NONE', #33657 ) ;
#69973 = CARTESIAN_POINT ( 'NONE',  ( 65.89583333333332860, -2.130196079827427091, 7.949999999999999289 ) ) ;
#69974 = FACE_OUTER_BOUND ( 'NONE', #122580, .T. ) ;
#69975 = DIRECTION ( 'NONE',  ( -0.7071067811865486830, -0.7071067811865464625, -0.000000000000000000 ) ) ;
#69976 = CARTESIAN_POINT ( 'NONE',  ( -0.7928932188134458769, 0.7592924766157069794, 5.000000000000000000 ) ) ;
#69977 = ORIENTED_EDGE ( 'NONE', *, *, #12056, .T. ) ;
#69978 = EDGE_CURVE ( 'NONE', #136091, #57246, #32953, .T. ) ;
#69979 = AXIS2_PLACEMENT_3D ( 'NONE', #34524, #45432, #113488 ) ;
#69980 = LINE ( 'NONE', #14103, #63002 ) ;
#69981 = AXIS2_PLACEMENT_3D ( 'NONE', #71409, #84444, #116328 ) ;
#69982 = CARTESIAN_POINT ( 'NONE',  ( -12.19999999999999929, -59.76999999999998892, -39.50000000000000000 ) ) ;
#69983 = CARTESIAN_POINT ( 'NONE',  ( 62.85459685856477563, -1.637169565754161615, 6.110000000000000320 ) ) ;
#69984 = AXIS2_PLACEMENT_3D ( 'NONE', #5634, #125310, #27392 ) ;
#69985 = CARTESIAN_POINT ( 'NONE',  ( 0.000000000000000000, 0.000000000000000000, 5.000000000000000000 ) ) ;
#69986 = ORIENTED_EDGE ( 'NONE', *, *, #82954, .T. ) ;
#69987 = ORIENTED_EDGE ( 'NONE', *, *, #106333, .F. ) ;
#69988 = AXIS2_PLACEMENT_3D ( 'NONE', #45886, #166, #44463 ) ;
#69989 = LINE ( 'NONE', #114152, #45354 ) ;
#69990 = LINE ( 'NONE', #93831, #69852 ) ;
#69991 = DIRECTION ( 'NONE',  ( 0.7071067811865487940, 0.7071067811865463515, 0.000000000000000000 ) ) ;
#69992 = DIRECTION ( 'NONE',  ( -0.7071067811865486830, 0.7071067811865464625, 0.000000000000000000 ) ) ;
#69994 = ORIENTED_EDGE ( 'NONE', *, *, #115481, .T. ) ;
#69993 = CARTESIAN_POINT ( 'NONE',  ( 14.34328999833778262, 3.759292476615678336, 13.27625715073268964 ) ) ;
#69995 = CARTESIAN_POINT ( 'NONE',  ( -23.81601139373100295, 28.73617430169770870, 5.000000000000000000 ) ) ;
#69996 = LINE ( 'NONE', #6072, #124165 ) ;
#69997 = CARTESIAN_POINT ( 'NONE',  ( 31.37176554955596686, -8.240707523384189770, 11.38925528200745596 ) ) ;
#69998 = AXIS2_PLACEMENT_3D ( 'NONE', #55945, #89266, #26155 ) ;
#69999 = PLANE ( 'NONE',  #69308 ) ;
#70000 = EDGE_LOOP ( 'NONE', ( #28335, #115726, #28431, #130126 ) ) ;
#70001 = VERTEX_POINT ( 'NONE', #110447 ) ;
#70002 = DIRECTION ( 'NONE',  ( -0.3543493200069162685, -0.000000000000000000, -0.9351131265310288487 ) ) ;
#70003 = DIRECTION ( 'NONE',  ( 0.7071067811865487940, 0.7071067811865463515, 0.000000000000000000 ) ) ;
#70004 = EDGE_CURVE ( 'NONE', #24590, #140445, #11122, .T. ) ;
#70005 = AXIS2_PLACEMENT_3D ( 'NONE', #32523, #131118, #33273 ) ;
#70006 = LINE ( 'NONE', #3257, #20032 ) ;
#70007 = DIRECTION ( 'NONE',  ( 0.7071067811865487940, 0.7071067811865463515, -0.000000000000000000 ) ) ;
#70008 = ORIENTED_EDGE ( 'NONE', *, *, #62571, .F. ) ;
#70009 = VERTEX_POINT ( 'NONE', #122043 ) ;
#70010 = VECTOR ( 'NONE', #88464, 1000.000000000000000 ) ;
#70011 = LINE ( 'NONE', #14858, #123284 ) ;
#70012 = ORIENTED_EDGE ( 'NONE', *, *, #13862, .F. ) ;
#70013 = CARTESIAN_POINT ( 'NONE',  ( -21.51665438641028771, 22.22500000000000142, 4.500000000000000888 ) ) ;
#70014 = EDGE_LOOP ( 'NONE', ( #63801, #688, #92448, #64410 ) ) ;
#70015 = CARTESIAN_POINT ( 'NONE',  ( 18.01107201284014536, -2.499999999999996447, 0.000000000000000000 ) ) ;
#70016 = CARTESIAN_POINT ( 'NONE',  ( -50.99451991528749062, 28.92564299267973738, 4.000000000000000000 ) ) ;
#70017 = AXIS2_PLACEMENT_3D ( 'NONE', #31201, #75419, #129779 ) ;
#70018 = VERTEX_POINT ( 'NONE', #70419 ) ;
#70019 = EDGE_CURVE ( 'NONE', #58035, #34745, #22710, .T. ) ;
#70020 = FACE_BOUND ( 'NONE', #15649, .T. ) ;
#70021 = CARTESIAN_POINT ( 'NONE',  ( -6.707013264292997157, -21.74070752338405654, 4.999753212805220670 ) ) ;
#70022 = DIRECTION ( 'NONE',  ( 0.000000000000000000, 0.000000000000000000, -1.000000000000000000 ) ) ;
#70023 = EDGE_CURVE ( 'NONE', #26531, #133481, #45262, .T. ) ;
#70024 = CARTESIAN_POINT ( 'NONE',  ( -10.49999999999993250, 13.08746187583912146, 4.000000000000000000 ) ) ;
#70025 = VECTOR ( 'NONE', #111449, 1000.000000000000000 ) ;
#70026 = DIRECTION ( 'NONE',  ( -0.000000000000000000, -0.000000000000000000, 1.000000000000000000 ) ) ;
#70027 = ADVANCED_FACE ( 'NONE', ( #136322 ), #133666, .T. ) ;
#70028 = ADVANCED_FACE ( 'NONE', ( #25407 ), #113859, .F. ) ;
#70029 = EDGE_CURVE ( 'NONE', #14841, #66142, #73235, .T. ) ;
#70030 =( NAMED_UNIT ( * ) PLANE_ANGLE_UNIT ( ) SI_UNIT ( $, .RADIAN. ) );
#70031 = DIRECTION ( 'NONE',  ( 1.000000000000000000, 0.000000000000000000, 0.000000000000000000 ) ) ;
#70032 = EDGE_LOOP ( 'NONE', ( #16259, #77045, #35717, #58164 ) ) ;
#70033 = VERTEX_POINT ( 'NONE', #29690 ) ;
#70034 = CARTESIAN_POINT ( 'NONE',  ( 97.62043019189812298, 3.055000000000001936, -5.291415217122916737 ) ) ;
#70035 = ORIENTED_EDGE ( 'NONE', *, *, #110551, .F. ) ;
#70036 = EDGE_CURVE ( 'NONE', #5681, #63125, #50754, .T. ) ;
#70037 = DIRECTION ( 'NONE',  ( 0.6830127018922181881, 0.6830127018922202975, -0.2588190451025214056 ) ) ;
#70038 = CARTESIAN_POINT ( 'NONE',  ( -15.15612307739229436, -22.22499999999999432, 4.000000000000000000 ) ) ;
#70039 = AXIS2_PLACEMENT_3D ( 'NONE', #11733, #56747, #128 ) ;
#70040 = VECTOR ( 'NONE', #133349, 1000.000000000000000 ) ;
#70041 = VECTOR ( 'NONE', #17358, 1000.000000000000227 ) ;
#70042 = CARTESIAN_POINT ( 'NONE',  ( 7.499999999999954703, 13.46639925780213076, 5.000000000000000000 ) ) ;
#70043 = VECTOR ( 'NONE', #97473, 1000.000000000000000 ) ;
#70044 = EDGE_CURVE ( 'NONE', #59056, #83800, #126858, .T. ) ;
#70045 =( GEOMETRIC_REPRESENTATION_CONTEXT ( 3 ) GLOBAL_UNCERTAINTY_ASSIGNED_CONTEXT ( ( #5845 ) ) GLOBAL_UNIT_ASSIGNED_CONTEXT ( ( #115592, #40262, #105460 ) ) REPRESENTATION_CONTEXT ( 'NONE', 'WORKASPACE' ) );
#70046 = LINE ( 'NONE', #114207, #93438 ) ;
#70047 = ORIENTED_EDGE ( 'NONE', *, *, #103142, .T. ) ;
#70048 = DIRECTION ( 'NONE',  ( -0.000000000000000000, 0.3543493200069153248, 0.9351131265310292928 ) ) ;
#70049 = DIRECTION ( 'NONE',  ( -1.000000000000000000, -1.224606353822377258E-16, -0.000000000000000000 ) ) ;
#70050 = LINE ( 'NONE', #36645, #99050 ) ;
#70051 = LINE ( 'NONE', #114892, #122101 ) ;
#70052 = CARTESIAN_POINT ( 'NONE',  ( -22.49999999999984723, 22.22500000000000853, 4.362957392718837646 ) ) ;
#70053 = VECTOR ( 'NONE', #80660, 1000.000000000000000 ) ;
#70054 = VECTOR ( 'NONE', #8188, 1000.000000000000227 ) ;
#70055 = VECTOR ( 'NONE', #130064, 1000.000000000000000 ) ;
#70056 = EDGE_CURVE ( 'NONE', #116730, #46699, #97073, .T. ) ;
#70057 = DIRECTION ( 'NONE',  ( -1.000000000000000000, -0.000000000000000000, -0.000000000000000000 ) ) ;
#70058 = ORIENTED_EDGE ( 'NONE', *, *, #115987, .T. ) ;
#70059 = CARTESIAN_POINT ( 'NONE',  ( -21.48921356237309155, -27.52281430457070499, 5.000000000000000000 ) ) ;
#70060 = PLANE ( 'NONE',  #11818 ) ;
#70061 = ORIENTED_EDGE ( 'NONE', *, *, #53978, .T. ) ;
#70062 = ORIENTED_EDGE ( 'NONE', *, *, #48911, .T. ) ;
#70063 = EDGE_LOOP ( 'NONE', ( #73582, #50616, #1034, #50949 ) ) ;
#70064 = CARTESIAN_POINT ( 'NONE',  ( 49.43793019189809002, -6.110000000000001208, 1.637169565754158951 ) ) ;
#70065 = ADVANCED_FACE ( 'NONE', ( #93545 ), #115241, .T. ) ;
#70066 = ORIENTED_EDGE ( 'NONE', *, *, #98353, .F. ) ;
#70067 = CARTESIAN_POINT ( 'NONE',  ( 9.816639616203772789, -1.633150327867691987, -6.094999999999989093 ) ) ;
#70068 = CARTESIAN_POINT ( 'NONE',  ( -11.54697671733239872, 10.46529571468478181, -26.63845132861668930 ) ) ;
#70069 = ORIENTED_EDGE ( 'NONE', *, *, #96785, .T. ) ;
#70070 = CARTESIAN_POINT ( 'NONE',  ( -18.18398860626898994, 28.73617430169800002, 5.000000000000000000 ) ) ;
#70071 = EDGE_CURVE ( 'NONE', #73688, #34146, #60816, .T. ) ;
#70072 = ORIENTED_EDGE ( 'NONE', *, *, #128752, .F. ) ;
#70073 = CARTESIAN_POINT ( 'NONE',  ( 17.48334561358943162, 22.22500000000000142, 4.500000000000000888 ) ) ;
#70075 = VERTEX_POINT ( 'NONE', #15928 ) ;
#70074 = LINE ( 'NONE', #58498, #123565 ) ;
#70076 = ORIENTED_EDGE ( 'NONE', *, *, #91531, .T. ) ;
#70077 = DIRECTION ( 'NONE',  ( 0.000000000000000000, 1.000000000000000000, 0.000000000000000000 ) ) ;
#70078 = VECTOR ( 'NONE', #92823, 1000.000000000000000 ) ;
#70079 = DIRECTION ( 'NONE',  ( -0.3543493200069162685, -0.000000000000000000, -0.9351131265310288487 ) ) ;
#70080 = EDGE_CURVE ( 'NONE', #27313, #16517, #116721, .T. ) ;
#70082 = EDGE_CURVE ( 'NONE', #73359, #57637, #60967, .T. ) ;
#70081 = CARTESIAN_POINT ( 'NONE',  ( 12.99507522778798396, -5.240707523384221744, 12.38332538355493107 ) ) ;
#70083 = ORIENTED_EDGE ( 'NONE', *, *, #100451, .T. ) ;
#70084 = CARTESIAN_POINT ( 'NONE',  ( -27.48921356237309155, -27.52281430457074762, 5.000000000000000000 ) ) ;
#70085 = ORIENTED_EDGE ( 'NONE', *, *, #110429, .T. ) ;
#70086 = VECTOR ( 'NONE', #52722, 1000.000000000000000 ) ;
#70087 = ORIENTED_EDGE ( 'NONE', *, *, #49407, .F. ) ;
#70088 = EDGE_LOOP ( 'NONE', ( #19479, #36563, #57294, #71797 ) ) ;
#70089 = SURFACE_SIDE_STYLE ('',( #125866 ) ) ;
#70090 = AXIS2_PLACEMENT_3D ( 'NONE', #74228, #63386, #140880 ) ;
#70091 = AXIS2_PLACEMENT_3D ( 'NONE', #37690, #16612, #71744 ) ;
#70092 = EDGE_CURVE ( 'NONE', #82948, #140430, #18075, .T. ) ;
#70093 = CARTESIAN_POINT ( 'NONE',  ( 27.18398860626900060, 28.73617430169806042, 5.000000000000000000 ) ) ;
#70094 = CARTESIAN_POINT ( 'NONE',  ( -8.671830600776413434, -9.740707523384187994, 4.000000000000000000 ) ) ;
#70095 = EDGE_CURVE ( 'NONE', #6993, #83571, #60218, .T. ) ;
#70096 = CARTESIAN_POINT ( 'NONE',  ( 12.19999999999999574, -40.43000000000000682, 19.06900128115122683 ) ) ;
#70097 = LINE ( 'NONE', #14932, #134572 ) ;
#70098 = ORIENTED_EDGE ( 'NONE', *, *, #26235, .T. ) ;
#70099 = DIRECTION ( 'NONE',  ( 1.000000000000000000, 0.000000000000000000, 0.000000000000000000 ) ) ;
#70100 = CARTESIAN_POINT ( 'NONE',  ( 24.91623647476855652, -7.934999999999990727, 4.858786175617117713E-16 ) ) ;
#70101 = CARTESIAN_POINT ( 'NONE',  ( 122.6835989386367345, -43.14999999999999147, 34.92499999999998295 ) ) ;
#70102 = DIRECTION ( 'NONE',  ( 0.7071067811865487940, 0.7071067811865463515, 0.000000000000000000 ) ) ;
#70103 =( BOUNDED_CURVE ( )  B_SPLINE_CURVE ( 3, ( #139189, #104373, #5034, #82649 ),
 .UNSPECIFIED., .F., .T. ) 
 B_SPLINE_CURVE_WITH_KNOTS ( ( 4, 4 ),
 ( 4.987589563512864643, 5.034563671340741564 ),
 .UNSPECIFIED. ) 
 CURVE ( )  GEOMETRIC_REPRESENTATION_ITEM ( )  RATIONAL_B_SPLINE_CURVE ( ( 1.000000000000000000, 0.9998161278856747547, 0.9998161278856747547, 1.000000000000000000 ) ) 
 REPRESENTATION_ITEM ( '' )  );
#70104 = ADVANCED_FACE ( 'NONE', ( #106521 ), #6474, .F. ) ;
#70105 = DIRECTION ( 'NONE',  ( 0.000000000000000000, 2.921639538487157626E-15, -1.000000000000000000 ) ) ;
#70106 = ORIENTED_EDGE ( 'NONE', *, *, #69575, .T. ) ;
#70107 = EDGE_LOOP ( 'NONE', ( #51108, #29303, #56660, #140382, #60560, #112102 ) ) ;
#70108 = VECTOR ( 'NONE', #70714, 1000.000000000000000 ) ;
#70109 = ORIENTED_EDGE ( 'NONE', *, *, #131011, .F. ) ;
#70110 = CARTESIAN_POINT ( 'NONE',  ( 57.29974487139158157, -27.71228299555246011, 4.000000000000000000 ) ) ;
#70111 = DIRECTION ( 'NONE',  ( 0.6830127018922180770, -0.6830127018922204085, -0.2588190451025213501 ) ) ;
#70112 = PLANE ( 'NONE',  #94001 ) ;
#70113 = AXIS2_PLACEMENT_3D ( 'NONE', #54788, #55500, #77962 ) ;
#70114 = LINE ( 'NONE', #36706, #107583 ) ;
#70115 = ADVANCED_FACE ( 'NONE', ( #94944 ), #73947, .T. ) ;
#70116 = DIRECTION ( 'NONE',  ( -0.6830127018922180770, -0.6830127018922204085, -0.2588190451025213501 ) ) ;
#70117 = CARTESIAN_POINT ( 'NONE',  ( 6.534046899938177333, 9.244424685250681506, 2.202405500345624212 ) ) ;
#70118 = DIRECTION ( 'NONE',  ( -0.000000000000000000, 0.000000000000000000, 1.000000000000000000 ) ) ;
#70119 = DIRECTION ( 'NONE',  ( 0.3543493200069162685, -0.000000000000000000, -0.9351131265310288487 ) ) ;
#70120 = LINE ( 'NONE', #39607, #51847 ) ;
#70121 = DIRECTION ( 'NONE',  ( -0.7071067811865486830, -0.7071067811865464625, 0.000000000000000000 ) ) ;
#70122 = DIRECTION ( 'NONE',  ( -0.7071067811865486830, 0.7071067811865464625, 0.000000000000000000 ) ) ;
#70123 = ORIENTED_EDGE ( 'NONE', *, *, #34376, .F. ) ;
#70124 = VECTOR ( 'NONE', #83164, 1000.000000000000000 ) ;
#70125 = CARTESIAN_POINT ( 'NONE',  ( 16.77034657092882597, -0.01012368044107444208, -34.06770708329295161 ) ) ;
#70126 = ORIENTED_EDGE ( 'NONE', *, *, #69537, .T. ) ;
#70127 = CARTESIAN_POINT ( 'NONE',  ( 8.999999999999937828, 16.93112307739201583, 4.000000000000000000 ) ) ;
#70129 = VERTEX_POINT ( 'NONE', #18818 ) ;
#70128 = DIRECTION ( 'NONE',  ( -0.3543493200069163240, -0.000000000000000000, 0.9351131265310288487 ) ) ;
#70130 = PLANE ( 'NONE',  #125039 ) ;
#70131 = CARTESIAN_POINT ( 'NONE',  ( -2.510786437626908008, -27.52281430457053446, 5.000000000000000000 ) ) ;
#70132 = EDGE_LOOP ( 'NONE', ( #117367, #52107, #101951, #24599 ) ) ;
#70133 = FACE_OUTER_BOUND ( 'NONE', #103538, .T. ) ;
#70135 = ORIENTED_EDGE ( 'NONE', *, *, #93063, .T. ) ;
#70134 = AXIS2_PLACEMENT_3D ( 'NONE', #122516, #110909, #65708 ) ;
#70136 = CARTESIAN_POINT ( 'NONE',  ( 120.8291937171295700, -3.975000000000001865, 6.884901960086284411 ) ) ;
#70137 = ORIENTED_EDGE ( 'NONE', *, *, #15132, .F. ) ;
#70138 = ADVANCED_FACE ( 'NONE', ( #7935, #31856 ), #86952, .F. ) ;
#70139 = CARTESIAN_POINT ( 'NONE',  ( 105.5166937171295558, 7.950000000000001066, -2.130196079827421318 ) ) ;
#70140 = FACE_OUTER_BOUND ( 'NONE', #12383, .T. ) ;
#70141 = CARTESIAN_POINT ( 'NONE',  ( 38.99451991528749062, 28.92564299267965211, 4.000000000000000000 ) ) ;
#70142 = ORIENTED_EDGE ( 'NONE', *, *, #77776, .F. ) ;
#70143 = LINE ( 'NONE', #58563, #107095 ) ;
#70144 = DIRECTION ( 'NONE',  ( -0.7071067811865486830, -0.7071067811865464625, -0.000000000000000000 ) ) ;
#70145 = CARTESIAN_POINT ( 'NONE',  ( 36.29974487139159578, -27.71228299555231445, 4.000000000000000000 ) ) ;
#70146 = CARTESIAN_POINT ( 'NONE',  ( 25.37500000000000000, -6.094999999999989981, 3.732111120401553285E-16 ) ) ;
#70147 = FACE_OUTER_BOUND ( 'NONE', #63106, .T. ) ;
#70148 = VECTOR ( 'NONE', #37810, 1000.000000000000000 ) ;
#70150 = LINE ( 'NONE', #46237, #72161 ) ;
#70149 = AXIS2_PLACEMENT_3D ( 'NONE', #951, #21306, #99548 ) ;
#70151 = PLANE ( 'NONE',  #133493 ) ;
#70152 = ORIENTED_EDGE ( 'NONE', *, *, #72843, .F. ) ;
#70153 = VECTOR ( 'NONE', #4529, 999.9999999999998863 ) ;
#70154 = VECTOR ( 'NONE', #21335, 1000.000000000000227 ) ;
#70155 = FACE_OUTER_BOUND ( 'NONE', #123309, .T. ) ;
#70156 = ORIENTED_EDGE ( 'NONE', *, *, #80356, .F. ) ;
#70157 = CARTESIAN_POINT ( 'NONE',  ( 98.29209685856477563, -5.291415217122921177, 3.054999999999999272 ) ) ;
#70158 = FACE_OUTER_BOUND ( 'NONE', #56100, .T. ) ;
#70159 = CARTESIAN_POINT ( 'NONE',  ( -20.99451991528748707, 28.92564299267952777, 4.000000000000000000 ) ) ;
#70160 = AXIS2_PLACEMENT_3D ( 'NONE', #92292, #91599, #58318 ) ;
#70162 = VECTOR ( 'NONE', #140021, 1000.000000000000227 ) ;
#70161 = DIRECTION ( 'NONE',  ( 0.7071067811865487940, 0.7071067811865463515, 0.000000000000000000 ) ) ;
#70163 = DIRECTION ( 'NONE',  ( -0.3543493200069162685, -0.000000000000000000, -0.9351131265310288487 ) ) ;
#70164 = ORIENTED_EDGE ( 'NONE', *, *, #42871, .T. ) ;
#70165 =( NAMED_UNIT ( * ) PLANE_ANGLE_UNIT ( ) SI_UNIT ( $, .RADIAN. ) );
#70166 = DIRECTION ( 'NONE',  ( 0.000000000000000000, 0.000000000000000000, -1.000000000000000000 ) ) ;
#70167 = ORIENTED_EDGE ( 'NONE', *, *, #79423, .F. ) ;
#70168 = DIRECTION ( 'NONE',  ( -0.7071067811865487940, 0.7071067811865463515, 0.000000000000000000 ) ) ;
#70169 = DIRECTION ( 'NONE',  ( -1.000000000000000000, 0.000000000000000000, 0.000000000000000000 ) ) ;
#70171 = ORIENTED_EDGE ( 'NONE', *, *, #8104, .T. ) ;
#70170 = CARTESIAN_POINT ( 'NONE',  ( 0.000000000000000000, -4.870000000000014317, -40.00000000000000000 ) ) ;
#70172 = FACE_OUTER_BOUND ( 'NONE', #55932, .T. ) ;
#70173 = PLANE ( 'NONE',  #93932 ) ;
#70174 = PLANE ( 'NONE',  #114162 ) ;
#70175 = DIRECTION ( 'NONE',  ( 0.6830127018922181881, 0.6830127018922202975, -0.2588190451025214056 ) ) ;
#70176 = VERTEX_POINT ( 'NONE', #53620 ) ;
#70177 = ORIENTED_EDGE ( 'NONE', *, *, #71068, .T. ) ;
#70178 = ORIENTED_EDGE ( 'NONE', *, *, #71622, .F. ) ;
#70179 = CARTESIAN_POINT ( 'NONE',  ( 83.27126352523143282, 4.472830434245839371, 4.472830434245842035 ) ) ;
#70180 = AXIS2_PLACEMENT_3D ( 'NONE', #6898, #9026, #32278 ) ;
#70181 = EDGE_LOOP ( 'NONE', ( #141625, #93084, #64569, #79490, #46431, #17492 ) ) ;
#70182 = LINE ( 'NONE', #92570, #63730 ) ;
#70183 = CARTESIAN_POINT ( 'NONE',  ( -23.96628934044694148, -0.2106608083017154909, 4.443784815937080523 ) ) ;
#70184 = EDGE_CURVE ( 'NONE', #107596, #63680, #31160, .T. ) ;
#70185 = DIRECTION ( 'NONE',  ( -0.3543493200069162685, -0.000000000000000000, -0.9351131265310288487 ) ) ;
#70186 = DIRECTION ( 'NONE',  ( -0.7071067811865486830, -0.7071067811865464625, 0.000000000000000000 ) ) ;
#70187 = ORIENTED_EDGE ( 'NONE', *, *, #55010, .F. ) ;
#70188 = CARTESIAN_POINT ( 'NONE',  ( 8.811592354503320124, 9.902892378096218942E-16, 0.000000000000000000 ) ) ;
#70189 = PLANE ( 'NONE',  #83706 ) ;
#70190 = AXIS2_PLACEMENT_3D ( 'NONE', #33851, #11320, #88948 ) ;
#70191 = CARTESIAN_POINT ( 'NONE',  ( 73.70376352523145158, 6.109999999999998543, 1.122388791418548911E-15 ) ) ;
#70192 = ADVANCED_FACE ( 'NONE', ( #132633 ), #21693, .F. ) ;
#70193 = ORIENTED_EDGE ( 'NONE', *, *, #80977, .F. ) ;
#70194 = VECTOR ( 'NONE', #136541, 1000.000000000000000 ) ;
#70195 = CARTESIAN_POINT ( 'NONE',  ( -24.29974487139158867, -27.71228299555223273, 4.000000000000000000 ) ) ;
#70196 = EDGE_CURVE ( 'NONE', #49442, #33856, #140615, .T. ) ;
#70197 = CARTESIAN_POINT ( 'NONE',  ( 15.65467068707222076, 2.499999999999998224, 3.061616997868380183E-16 ) ) ;
#70198 = DIRECTION ( 'NONE',  ( -1.000000000000000000, -1.224606353822377258E-16, -0.000000000000000000 ) ) ;
#70199 = ORIENTED_EDGE ( 'NONE', *, *, #2211, .F. ) ;
#70200 = ORIENTED_EDGE ( 'NONE', *, *, #52155, .T. ) ;
#70201 = EDGE_CURVE ( 'NONE', #34867, #67596, #69149, .T. ) ;
#70202 = CARTESIAN_POINT ( 'NONE',  ( 0.000000000000000000, 0.000000000000000000, 9.119999999999999218 ) ) ;
#70203 = EDGE_CURVE ( 'NONE', #35082, #110223, #34366, .T. ) ;
#70204 = EDGE_CURVE ( 'NONE', #34556, #82308, #132993, .T. ) ;
#70205 = CARTESIAN_POINT ( 'NONE',  ( -33.32816939922329880, 14.25929247661557397, 4.000000000000000000 ) ) ;
#70206 = FACE_OUTER_BOUND ( 'NONE', #94574, .T. ) ;
#70207 = DIRECTION ( 'NONE',  ( 0.7071067811865487940, 0.7071067811865463515, 0.000000000000000000 ) ) ;
#70208 = CYLINDRICAL_SURFACE ( 'NONE', #6324, 5.999999999999998224 ) ;
#70209 = LINE ( 'NONE', #57175, #58075 ) ;
#70211 = ADVANCED_FACE ( 'NONE', ( #123543 ), #143118, .T. ) ;
#70210 = CONICAL_SURFACE ( 'NONE', #44748, 2.055000000000000604, 0.9599310885968764806 ) ;
#70212 = EDGE_CURVE ( 'NONE', #56310, #45046, #1683, .T. ) ;
#70213 = CARTESIAN_POINT ( 'NONE',  ( 47.99451991528749062, 28.92564299267971251, 4.000000000000000000 ) ) ;
#70214 = EDGE_LOOP ( 'NONE', ( #125300, #52163, #141924, #127354, #102470 ) ) ;
#70215 = VERTEX_POINT ( 'NONE', #121355 ) ;
#70217 = ADVANCED_FACE ( 'NONE', ( #22038 ), #66291, .F. ) ;
#70216 = DIRECTION ( 'NONE',  ( 0.7071067811865487940, -0.7071067811865463515, 0.000000000000000000 ) ) ;
#70218 = EDGE_LOOP ( 'NONE', ( #91572, #100424, #80373, #123279 ) ) ;
#70219 = AXIS2_PLACEMENT_3D ( 'NONE', #69294, #67900, #122952 ) ;
#70220 = VECTOR ( 'NONE', #38033, 1000.000000000000227 ) ;
#70221 = ADVANCED_FACE ( 'NONE', ( #72023 ), #70602, .F. ) ;
#70222 = DIRECTION ( 'NONE',  ( -1.000000000000000000, -1.224606353822377258E-16, -0.000000000000000000 ) ) ;
#70223 = ORIENTED_EDGE ( 'NONE', *, *, #46794, .T. ) ;
#70224 = DIRECTION ( 'NONE',  ( 0.6830127018922181881, 0.6830127018922202975, -0.2588190451025214056 ) ) ;
#70225 = DIRECTION ( 'NONE',  ( -0.7071067811865486830, -0.7071067811865464625, 0.000000000000000000 ) ) ;
#70226 = CARTESIAN_POINT ( 'NONE',  ( 0.000000000000000000, 0.000000000000000000, 5.000000000000000000 ) ) ;
#70227 = VECTOR ( 'NONE', #36007, 999.9999999999998863 ) ;
#70228 = CARTESIAN_POINT ( 'NONE',  ( -2.000000000000000000, 2.375000000000000000, 4.319999999999998508 ) ) ;
#70229 = ORIENTED_EDGE ( 'NONE', *, *, #11055, .F. ) ;
#70230 = DIRECTION ( 'NONE',  ( 0.000000000000000000, -1.000000000000000000, 0.000000000000000000 ) ) ;
#70231 = ORIENTED_EDGE ( 'NONE', *, *, #101551, .T. ) ;
#70232 = CARTESIAN_POINT ( 'NONE',  ( -17.51078643762690845, -27.52281430457043143, 5.000000000000000000 ) ) ;
#70233 = EDGE_LOOP ( 'NONE', ( #99446, #38056, #57638, #4487 ) ) ;
#70234 = VERTEX_POINT ( 'NONE', #114056 ) ;
#70235 = PLANE ( 'NONE',  #76037 ) ;
#70236 = EDGE_LOOP ( 'NONE', ( #132102, #131514, #119975, #67110, #16677, #17762 ) ) ;
#70237 = ORIENTED_EDGE ( 'NONE', *, *, #30062, .T. ) ;
#70238 = AXIS2_PLACEMENT_3D ( 'NONE', #15689, #107020, #72315 ) ;
#70239 = LINE ( 'NONE', #32760, #97395 ) ;
#70240 = EDGE_CURVE ( 'NONE', #44417, #114577, #61908, .T. ) ;
#70241 = EDGE_LOOP ( 'NONE', ( #84375, #131574, #94799, #132026 ) ) ;
#70242 = DIRECTION ( 'NONE',  ( 0.7071067811865486830, -0.7071067811865464625, -0.000000000000000000 ) ) ;
#70243 = CARTESIAN_POINT ( 'NONE',  ( 9.183988606268997046, 28.73617430169793607, 5.000000000000000000 ) ) ;
#70244 = CARTESIAN_POINT ( 'NONE',  ( 116.8129301918981184, -1.637169565754159617, -6.110000000000001208 ) ) ;
#70245 = FACE_OUTER_BOUND ( 'NONE', #104598, .T. ) ;
#70246 = DIRECTION ( 'NONE',  ( -0.6830127018922180770, -0.6830127018922204085, -0.2588190451025213501 ) ) ;
#70247 = EDGE_CURVE ( 'NONE', #64709, #109374, #102494, .T. ) ;
#70248 = LINE ( 'NONE', #114408, #23215 ) ;
#70249 = VECTOR ( 'NONE', #84689, 1000.000000000000000 ) ;
#70250 = CARTESIAN_POINT ( 'NONE',  ( 1.828169399223505964, 21.75929247661551358, 4.000000000000000000 ) ) ;
#70251 = VECTOR ( 'NONE', #134951, 1000.000000000000000 ) ;
#70253 = ADVANCED_FACE ( 'NONE', ( #71291 ), #39377, .F. ) ;
#70252 =( NAMED_UNIT ( * ) SI_UNIT ( $, .STERADIAN. ) SOLID_ANGLE_UNIT ( ) );
#70254 = ORIENTED_EDGE ( 'NONE', *, *, #91372, .F. ) ;
#70255 = CARTESIAN_POINT ( 'NONE',  ( -7.499999999999944045, -7.533600742197667621, 5.000000000000000000 ) ) ;
#70256 = CARTESIAN_POINT ( 'NONE',  ( 31.92500000000002203, -21.76999999999999247, -40.00000000000000000 ) ) ;
#70257 = EDGE_LOOP ( 'NONE', ( #106948, #43066, #18254, #108327 ) ) ;
#70258 = EDGE_CURVE ( 'NONE', #132991, #129216, #59023, .T. ) ;
#70259 = VERTEX_POINT ( 'NONE', #17581 ) ;
#70260 = VECTOR ( 'NONE', #3763, 1000.000000000000000 ) ;
#70261 = PRESENTATION_LAYER_ASSIGNMENT (  '', '', ( #35479 ) ) ;
#70262 = CARTESIAN_POINT ( 'NONE',  ( 1.499999999999980460, 19.08746187583906462, 4.000000000000000000 ) ) ;
#70263 = ORIENTED_EDGE ( 'NONE', *, *, #7157, .F. ) ;
#70264 = AXIS2_PLACEMENT_3D ( 'NONE', #115256, #80562, #47261 ) ;
#70265 = EDGE_CURVE ( 'NONE', #72157, #104640, #48105, .T. ) ;
#70266 = DIRECTION ( 'NONE',  ( -0.7071067811865486830, -0.7071067811865464625, -0.000000000000000000 ) ) ;
#70267 = CARTESIAN_POINT ( 'NONE',  ( 34.49999999999976552, -7.420205493532866292, -2.617629953481174887 ) ) ;
#70268 = CARTESIAN_POINT ( 'NONE',  ( 25.17183060077628909, 18.75929247661551713, 4.000000000000000000 ) ) ;
#70269 = CARTESIAN_POINT ( 'NONE',  ( 27.70710678118635428, 14.25929247661557397, 5.000000000000000000 ) ) ;
#70270 = VERTEX_POINT ( 'NONE', #49555 ) ;
#70271 = DIRECTION ( 'NONE',  ( -1.000000000000000000, -0.000000000000000000, -0.000000000000000000 ) ) ;
#70272 = ORIENTED_EDGE ( 'NONE', *, *, #29604, .T. ) ;
#70273 = EDGE_CURVE ( 'NONE', #115863, #83494, #127813, .T. ) ;
#70274 = DIRECTION ( 'NONE',  ( -0.000000000000000000, 0.000000000000000000, 1.000000000000000000 ) ) ;
#70275 = CIRCLE ( 'NONE', #7704, 2.500000000000000444 ) ;
#70276 = CARTESIAN_POINT ( 'NONE',  ( 32.15040314143522693, 7.934999999999989839, -2.126176841940961904 ) ) ;
#70277 = LINE ( 'NONE', #48466, #29740 ) ;
#70278 = EDGE_CURVE ( 'NONE', #37747, #48700, #15420, .T. ) ;
#70279 = DIRECTION ( 'NONE',  ( -0.6830127018922181881, 0.6830127018922202975, -0.2588190451025214056 ) ) ;
#70280 = VERTEX_POINT ( 'NONE', #37214 ) ;
#70281 = VERTEX_POINT ( 'NONE', #137969 ) ;
#70282 = ORIENTED_EDGE ( 'NONE', *, *, #136210, .T. ) ;
#70283 = CARTESIAN_POINT ( 'NONE',  ( 5.292893218813419232, 17.25929247661554911, 5.000000000000000000 ) ) ;
#70284 = DIRECTION ( 'NONE',  ( 0.000000000000000000, 0.000000000000000000, 1.000000000000000000 ) ) ;
#70285 = CARTESIAN_POINT ( 'NONE',  ( 11.20710678118646442, 18.75929247661552068, 5.000000000000000000 ) ) ;
#70286 = DIRECTION ( 'NONE',  ( -0.7071067811865486830, 0.7071067811865464625, 0.000000000000000000 ) ) ;
#70287 = ORIENTED_EDGE ( 'NONE', *, *, #52332, .F. ) ;
#70288 = VECTOR ( 'NONE', #10625, 1000.000000000000000 ) ;
#70289 = LINE ( 'NONE', #5660, #118000 ) ;
#70290 = CARTESIAN_POINT ( 'NONE',  ( 30.29974487139158867, -27.71228299555227537, 4.000000000000000000 ) ) ;
#70291 = AXIS2_PLACEMENT_3D ( 'NONE', #47217, #52553, #142442 ) ;
#70292 = DIRECTION ( 'NONE',  ( 0.7071067811865487940, 0.7071067811865463515, -0.000000000000000000 ) ) ;
#70293 = CARTESIAN_POINT ( 'NONE',  ( 75.29974487139158157, -27.71228299555258445, 4.000000000000000000 ) ) ;
#70294 = ORIENTED_EDGE ( 'NONE', *, *, #131370, .T. ) ;
#70295 = FACE_OUTER_BOUND ( 'NONE', #34818, .T. ) ;
#70296 = ORIENTED_EDGE ( 'NONE', *, *, #95678, .F. ) ;
#70297 = AXIS2_PLACEMENT_3D ( 'NONE', #82363, #126545, #38144 ) ;
#70300 = EDGE_CURVE ( 'NONE', #42962, #92514, #104607, .T. ) ;
#70299 = ORIENTED_EDGE ( 'NONE', *, *, #69670, .T. ) ;
#70298 = DIRECTION ( 'NONE',  ( -0.6830127018922180770, -0.6830127018922204085, -0.2588190451025213501 ) ) ;
#70301 = VERTEX_POINT ( 'NONE', #61166 ) ;
#70302 = DIRECTION ( 'NONE',  ( -1.000000000000000000, -1.224606353822377258E-16, -0.000000000000000000 ) ) ;
#70303 = DIRECTION ( 'NONE',  ( 0.6830127018922180770, -0.6830127018922204085, -0.2588190451025213501 ) ) ;
#70304 = ORIENTED_EDGE ( 'NONE', *, *, #49536, .T. ) ;
#70305 = DIRECTION ( 'NONE',  ( -0.7071067811865486830, -0.7071067811865464625, 0.000000000000000000 ) ) ;
#70306 = VERTEX_POINT ( 'NONE', #80742 ) ;
#70307 = CIRCLE ( 'NONE', #121155, 4.000000000000000000 ) ;
#70308 = LINE ( 'NONE', #59415, #19715 ) ;
#70309 = FACE_OUTER_BOUND ( 'NONE', #102716, .T. ) ;
#70310 = CARTESIAN_POINT ( 'NONE',  ( 31.12043019189811233, 3.055000000000002380, -5.291415217122917625 ) ) ;
#70312 = VECTOR ( 'NONE', #97493, 1000.000000000000000 ) ;
#70311 = LINE ( 'NONE', #36904, #71696 ) ;
#70313 = CARTESIAN_POINT ( 'NONE',  ( 47.47502705046287730, -5.819803920172573086, 5.819803920172573086 ) ) ;
#70314 = CARTESIAN_POINT ( 'NONE',  ( 88.50000000000000000, 0.000000000000000000, -7.950000000000000178 ) ) ;
#70315 = DIRECTION ( 'NONE',  ( -0.000000000000000000, 0.000000000000000000, 1.000000000000000000 ) ) ;
#70316 = DIRECTION ( 'NONE',  ( 1.000000000000000000, 0.000000000000000000, 0.000000000000000000 ) ) ;
#70317 = CARTESIAN_POINT ( 'NONE',  ( 29.29123647476855652, -9.717572351234235426E-16, -7.934999999999990727 ) ) ;
#70318 = CARTESIAN_POINT ( 'NONE',  ( 1.582903141435219485, 3.967499999999992699, -6.871911579029513994 ) ) ;
#70319 = VECTOR ( 'NONE', #3404, 1000.000000000000000 ) ;
#70320 = LINE ( 'NONE', #114468, #43662 ) ;
#70321 = CARTESIAN_POINT ( 'NONE',  ( -32.99999999999976552, -18.41253812416056945, 4.000000000000000000 ) ) ;
#70322 = CARTESIAN_POINT ( 'NONE',  ( 21.48921356237309155, -27.52281430457070499, 5.000000000000000000 ) ) ;
#70323 = VERTEX_POINT ( 'NONE', #124931 ) ;
#70324 = EDGE_CURVE ( 'NONE', #122875, #116985, #125667, .T. ) ;
#70325 = EDGE_LOOP ( 'NONE', ( #86010, #129293, #68279, #97960, #76025, #124585 ) ) ;
#70326 = CARTESIAN_POINT ( 'NONE',  ( 95.93750000000000000, 5.819803920172573974, -5.819803920172572198 ) ) ;
#70327 = EDGE_CURVE ( 'NONE', #34745, #54071, #141089, .T. ) ;
#70328 = ORIENTED_EDGE ( 'NONE', *, *, #90345, .T. ) ;
#70329 = VERTEX_POINT ( 'NONE', #25612 ) ;
#70330 = CARTESIAN_POINT ( 'NONE',  ( 21.48921356237309155, -27.52281430457070499, 5.000000000000000000 ) ) ;
#70331 = CARTESIAN_POINT ( 'NONE',  ( 20.99999999999985434, -13.06887692260767686, 4.000000000000000000 ) ) ;
#70332 = AXIS2_PLACEMENT_3D ( 'NONE', #43137, #141738, #131563 ) ;
#70333 = CARTESIAN_POINT ( 'NONE',  ( 10.61372115956010376, 8.432637487761468265, -4.375000000000002665 ) ) ;
#70334 = ORIENTED_EDGE ( 'NONE', *, *, #30710, .T. ) ;
#70335 = LINE ( 'NONE', #136243, #37031 ) ;
#70336 = CARTESIAN_POINT ( 'NONE',  ( 66.48921356237309510, -27.52281430457101763, 5.000000000000000000 ) ) ;
#70337 = DIRECTION ( 'NONE',  ( -0.7071067811865486830, 0.7071067811865464625, 0.000000000000000000 ) ) ;
#70338 = FACE_OUTER_BOUND ( 'NONE', #15921, .T. ) ;
#70339 = EDGE_CURVE ( 'NONE', #58156, #13978, #83261, .T. ) ;
#70340 = LINE ( 'NONE', #82593, #19251 ) ;
#70342 = VECTOR ( 'NONE', #1097, 1000.000000000000227 ) ;
#70341 = CARTESIAN_POINT ( 'NONE',  ( 28.49999999999980460, 3.052185695429140200, 5.000000000000000000 ) ) ;
#70343 = FACE_OUTER_BOUND ( 'NONE', #119659, .T. ) ;
#70344 = DIRECTION ( 'NONE',  ( 0.6830127018922181881, 0.6830127018922202975, -0.2588190451025214056 ) ) ;
#70345 = LINE ( 'NONE', #25349, #109403 ) ;
#70346 = FACE_OUTER_BOUND ( 'NONE', #112777, .T. ) ;
#70347 = DIRECTION ( 'NONE',  ( -0.000000000000000000, 0.000000000000000000, 1.000000000000000000 ) ) ;
#70348 = CARTESIAN_POINT ( 'NONE',  ( 55.62203754808115264, -51.91654526991819552, 39.52330221398159438 ) ) ;
#70349 = ORIENTED_EDGE ( 'NONE', *, *, #113858, .T. ) ;
#70350 = ORIENTED_EDGE ( 'NONE', *, *, #59603, .T. ) ;
#70351 = CARTESIAN_POINT ( 'NONE',  ( 107.6254301918981042, 5.291415217122919401, 3.055000000000002824 ) ) ;
#70352 = AXIS2_PLACEMENT_3D ( 'NONE', #115080, #17909, #73759 ) ;
#70353 = ORIENTED_EDGE ( 'NONE', *, *, #19468, .T. ) ;
#70354 = DIRECTION ( 'NONE',  ( 0.000000000000000000, -1.000000000000000000, 0.000000000000000000 ) ) ;
#70355 = CARTESIAN_POINT ( 'NONE',  ( 6.938893903907228378E-15, 5.966399257802203593, 5.000000000000000000 ) ) ;
#70356 = EDGE_LOOP ( 'NONE', ( #65803, #29241, #87032 ) ) ;
#70357 = DIRECTION ( 'NONE',  ( -0.6830127018922180770, 0.6830127018922202975, -0.2588190451025213501 ) ) ;
#70359 = AXIS2_PLACEMENT_3D ( 'NONE', #109216, #109928, #117913 ) ;
#70358 = CARTESIAN_POINT ( 'NONE',  ( -39.18398860626899705, 28.73617430169814568, 5.000000000000000000 ) ) ;
#70360 = CARTESIAN_POINT ( 'NONE',  ( 102.5787635252314658, -7.482591942790325086E-16, 6.109999999999998543 ) ) ;
#70361 = VERTEX_POINT ( 'NONE', #82879 ) ;
#70362 = ORIENTED_EDGE ( 'NONE', *, *, #69759, .F. ) ;
#70363 = DIRECTION ( 'NONE',  ( 0.6830127018922181881, 0.6830127018922202975, -0.2588190451025214056 ) ) ;
#70364 = CARTESIAN_POINT ( 'NONE',  ( 30.09667064187387098, -2.240707523384257716, 15.26439735382759544 ) ) ;
#70365 = CARTESIAN_POINT ( 'NONE',  ( -12.48921356237309155, -27.52281430457064104, 5.000000000000000000 ) ) ;
#70366 = FACE_OUTER_BOUND ( 'NONE', #85917, .T. ) ;
#70367 = ORIENTED_EDGE ( 'NONE', *, *, #43700, .F. ) ;
#70368 = ORIENTED_EDGE ( 'NONE', *, *, #83978, .F. ) ;
#70369 = ORIENTED_EDGE ( 'NONE', *, *, #123082, .T. ) ;
#70370 = CARTESIAN_POINT ( 'NONE',  ( 151.4000000000000057, -17.48000000000005016, -12.70000000000043272 ) ) ;
#70371 = ADVANCED_FACE ( 'NONE', ( #127068 ), #27757, .F. ) ;
#70372 = CARTESIAN_POINT ( 'NONE',  ( 2.546236474768552860, -7.934999999999990727, 4.858786175617117713E-16 ) ) ;
#70373 = AXIS2_PLACEMENT_3D ( 'NONE', #58652, #102103, #135454 ) ;
#70374 = ADVANCED_FACE ( 'NONE', ( #140786 ), #87145, .F. ) ;
#70375 = EDGE_CURVE ( 'NONE', #66060, #91002, #29887, .T. ) ;
#70376 = SHAPE_REPRESENTATION_RELATIONSHIP ( 'NONE' , 'NONE' ,  #58954, #70809 ) ;
#70377 = VECTOR ( 'NONE', #107855, 1000.000000000000000 ) ;
#70378 = FILL_AREA_STYLE_COLOUR ( '', #119550 ) ;
#70379 = EDGE_CURVE ( 'NONE', #15864, #76116, #29186, .T. ) ;
#70380 = ORIENTED_EDGE ( 'NONE', *, *, #98175, .F. ) ;
#70381 = EDGE_LOOP ( 'NONE', ( #117167, #83379, #120549, #102167 ) ) ;
#70383 = EDGE_CURVE ( 'NONE', #45317, #100766, #95867, .T. ) ;
#70382 = CARTESIAN_POINT ( 'NONE',  ( 14.74000000000000021, 9.521314400968980422E-16, 0.000000000000000000 ) ) ;
#70384 = VERTEX_POINT ( 'NONE', #141531 ) ;
#70385 = ORIENTED_EDGE ( 'NONE', *, *, #50014, .F. ) ;
#70386 = ADVANCED_FACE ( 'NONE', ( #73427 ), #106296, .T. ) ;
#70387 = VECTOR ( 'NONE', #137981, 1000.000000000000000 ) ;
#70388 = DIRECTION ( 'NONE',  ( 0.7071067811865487940, 0.7071067811865463515, 0.000000000000000000 ) ) ;
#70389 = EDGE_CURVE ( 'NONE', #19080, #14379, #40794, .T. ) ;
#70390 = CARTESIAN_POINT ( 'NONE',  ( -38.01844734635646006, 18.75929247661552424, 20.33588619593452052 ) ) ;
#70391 = ORIENTED_EDGE ( 'NONE', *, *, #93437, .F. ) ;
#70392 = AXIS2_PLACEMENT_3D ( 'NONE', #45825, #121905, #88612 ) ;
#70393 = CARTESIAN_POINT ( 'NONE',  ( 78.29974487139158157, -27.71228299555260577, 4.000000000000000000 ) ) ;
#70394 = PLANE ( 'NONE',  #83064 ) ;
#70395 =( BOUNDED_SURFACE ( )  B_SPLINE_SURFACE ( 3, 2, ( 
 ( #103714, #116030, #104445 ),
 ( #83437, #25454, #50799 ),
 ( #116757, #105857, #16733 ),
 ( #14598, #26897, #6516 ),
 ( #94985, #48663, #39953 ),
 ( #124783, #113906, #37802 ),
 ( #82036, #105167, #5104 ),
 ( #93593, #137822, #38499 ),
 ( #82720, #85541, #130518 ),
 ( #18120, #95719, #42081 ),
 ( #139971, #128370, #107995 ),
 ( #131211, #129775, #84175 ) ),
 .UNSPECIFIED., .F., .F., .T. ) 
 B_SPLINE_SURFACE_WITH_KNOTS ( ( 4, 2, 2, 2, 2, 4 ),
 ( 3, 3 ),
 ( 0.000000000000000000, 0.001647923167088043627, 0.002471884750632065333, 0.003295846334176087255, 0.004943769501264130665, 0.006591692668352174510 ),
 ( 0.000000000000000000, 1.000000000000000000 ),
 .UNSPECIFIED. ) 
 GEOMETRIC_REPRESENTATION_ITEM ( )  RATIONAL_B_SPLINE_SURFACE ( (
 ( 1.000000000000000000, 0.7071067811865443531, 1.000000000000000000),
 ( 1.000000000000000000, 0.7122033721496183745, 1.000000000000000000),
 ( 1.000000000000000000, 0.7158366153106693330, 1.000000000000000000),
 ( 1.000000000000000000, 0.7192720032940053132, 1.000000000000000000),
 ( 1.000000000000000000, 0.7200809050417178447, 1.000000000000000000),
 ( 1.000000000000000000, 0.7210491446665048265, 1.000000000000000000),
 ( 1.000000000000000000, 0.7212054070303647313, 1.000000000000000000),
 ( 1.000000000000000000, 0.7207522793907679137, 1.000000000000000000),
 ( 1.000000000000000000, 0.7192424821649825439, 1.000000000000000000),
 ( 1.000000000000000000, 0.7143802006614192734, 1.000000000000000000),
 ( 1.000000000000000000, 0.7109884861397230971, 1.000000000000000000),
 ( 1.000000000000000000, 0.7071067811865492381, 1.000000000000000000) ) ) 
 REPRESENTATION_ITEM ( '' )  SURFACE ( )  );
#70396 = LINE ( 'NONE', #114548, #2643 ) ;
#70397 = VECTOR ( 'NONE', #64713, 1000.000000000000000 ) ;
#70398 = ADVANCED_FACE ( 'NONE', ( #18278 ), #63972, .T. ) ;
#70399 = CARTESIAN_POINT ( 'NONE',  ( 7.499999999999947597, 18.43112307739200162, 4.000000000000000000 ) ) ;
#70400 = FACE_BOUND ( 'NONE', #31024, .T. ) ;
#70402 = VERTEX_POINT ( 'NONE', #139419 ) ;
#70401 = VECTOR ( 'NONE', #123382, 1000.000000000000000 ) ;
#70403 = EDGE_CURVE ( 'NONE', #4116, #114666, #31344, .T. ) ;
#70404 = LINE ( 'NONE', #5772, #66602 ) ;
#70405 = PLANE ( 'NONE',  #106298 ) ;
#70406 = DIRECTION ( 'NONE',  ( -0.6830127018922181881, 0.6830127018922202975, -0.2588190451025214056 ) ) ;
#70407 = ORIENTED_EDGE ( 'NONE', *, *, #91494, .F. ) ;
#70408 = DIRECTION ( 'NONE',  ( 0.5735764363510453823, -0.8191520442889923537, 1.003171929053525486E-16 ) ) ;
#70409 = VERTEX_POINT ( 'NONE', #118324 ) ;
#70410 = EDGE_LOOP ( 'NONE', ( #68818, #16665, #76833, #14233 ) ) ;
#70411 = AXIS2_PLACEMENT_3D ( 'NONE', #2646, #80256, #34589 ) ;
#70412 = EDGE_CURVE ( 'NONE', #112632, #136524, #86446, .T. ) ;
#70413 = EDGE_LOOP ( 'NONE', ( #67188, #20208 ) ) ;
#70414 = AXIS2_PLACEMENT_3D ( 'NONE', #76817, #110804, #99967 ) ;
#70415 = CARTESIAN_POINT ( 'NONE',  ( 36.07876352523144448, -7.482591942790325086E-16, 6.109999999999998543 ) ) ;
#70417 = ORIENTED_EDGE ( 'NONE', *, *, #73173, .T. ) ;
#70416 = AXIS2_PLACEMENT_3D ( 'NONE', #70434, #5796, #50068 ) ;
#70418 = CARTESIAN_POINT ( 'NONE',  ( 9.183988606268997046, 28.73617430169793607, 5.000000000000000000 ) ) ;
#70419 = CARTESIAN_POINT ( 'NONE',  ( -34.92500000000001137, 13.51246187583936198, 4.000000000000000000 ) ) ;
#70420 = CARTESIAN_POINT ( 'NONE',  ( 0.000000000000000000, 9.735942053221458872E-16, -7.950000000000000178 ) ) ;
#70421 = EDGE_LOOP ( 'NONE', ( #68075, #70076, #51664, #125683 ) ) ;
#70422 = CARTESIAN_POINT ( 'NONE',  ( 48.29974487139158867, -27.71228299555239971, 4.000000000000000000 ) ) ;
#70423 = CIRCLE ( 'NONE', #107409, 17.45000000000002061 ) ;
#70424 = DIRECTION ( 'NONE',  ( 0.6830127018922180770, -0.6830127018922204085, -0.2588190451025213501 ) ) ;
#70425 = DIRECTION ( 'NONE',  ( -0.7071067811865487940, 0.7071067811865463515, -0.000000000000000000 ) ) ;
#70426 = DIRECTION ( 'NONE',  ( 1.000000000000000000, 0.000000000000000000, 0.000000000000000000 ) ) ;
#70427 = CARTESIAN_POINT ( 'NONE',  ( -45.18398860626900415, 28.73617430169818832, 5.000000000000000000 ) ) ;
#70428 = VERTEX_POINT ( 'NONE', #62552 ) ;
#70429 = EDGE_CURVE ( 'NONE', #32288, #48528, #8121, .T. ) ;
#70430 = ORIENTED_EDGE ( 'NONE', *, *, #50144, .F. ) ;
#70432 = VERTEX_POINT ( 'NONE', #51673 ) ;
#70431 = AXIS2_PLACEMENT_3D ( 'NONE', #36870, #85367, #39025 ) ;
#70433 = ORIENTED_EDGE ( 'NONE', *, *, #65135, .T. ) ;
#70434 = CARTESIAN_POINT ( 'NONE',  ( 19.10840764549667270, 9.139736423841732040E-16, 0.000000000000000000 ) ) ;
#70435 = ORIENTED_EDGE ( 'NONE', *, *, #41990, .T. ) ;
#70436 = ORIENTED_EDGE ( 'NONE', *, *, #132035, .F. ) ;
#70437 = LINE ( 'NONE', #58853, #93012 ) ;
#70438 = LINE ( 'NONE', #92838, #78713 ) ;
#70439 = ORIENTED_EDGE ( 'NONE', *, *, #47757, .T. ) ;
#70440 = CYLINDRICAL_SURFACE ( 'NONE', #115888, 2.500000000000000444 ) ;
#70441 = ORIENTED_EDGE ( 'NONE', *, *, #3500, .T. ) ;
#70442 = ADVANCED_FACE ( 'NONE', ( #50957 ), #20434, .F. ) ;
#70443 = DIRECTION ( 'NONE',  ( 0.7071067811865486830, -0.7071067811865464625, -0.000000000000000000 ) ) ;
#70444 = CARTESIAN_POINT ( 'NONE',  ( -75.29974487139158157, -27.71228299555258445, 4.000000000000000000 ) ) ;
#70445 = VECTOR ( 'NONE', #106013, 1000.000000000000000 ) ;
#70446 = VERTEX_POINT ( 'NONE', #64683 ) ;
#70448 = CARTESIAN_POINT ( 'NONE',  ( 6.066782984417857350, 4.584330080086930965E-16, 0.000000000000000000 ) ) ;
#70447 = CARTESIAN_POINT ( 'NONE',  ( 101.8495968585647660, 6.109999999999997655, 1.637169565754163836 ) ) ;
#70450 = EDGE_CURVE ( 'NONE', #30243, #60103, #83367, .T. ) ;
#70449 = DIRECTION ( 'NONE',  ( 0.6830127018922180770, -0.6830127018922204085, -0.2588190451025213501 ) ) ;
#70451 = CARTESIAN_POINT ( 'NONE',  ( 0.000000000000000000, 0.000000000000000000, 5.000000000000000000 ) ) ;
#70452 = ORIENTED_EDGE ( 'NONE', *, *, #24362, .F. ) ;
#70453 = ORIENTED_EDGE ( 'NONE', *, *, #69032, .T. ) ;
#70454 = DIRECTION ( 'NONE',  ( -0.7071067811865486830, -0.7071067811865464625, -0.000000000000000000 ) ) ;
#70455 = ORIENTED_EDGE ( 'NONE', *, *, #117610, .T. ) ;
#70456 = CARTESIAN_POINT ( 'NONE',  ( -9.707106781186478628, 8.259292476615632594, 5.000000000000000000 ) ) ;
#70457 = LINE ( 'NONE', #106564, #85815 ) ;
#70458 = DIRECTION ( 'NONE',  ( -0.7071067811865486830, -0.7071067811865464625, 0.000000000000000000 ) ) ;
#70459 = DIRECTION ( 'NONE',  ( 0.6830127018922180770, -0.6830127018922204085, -0.2588190451025213501 ) ) ;
#70460 = FACE_OUTER_BOUND ( 'NONE', #47544, .T. ) ;
#70462 = VERTEX_POINT ( 'NONE', #84996 ) ;
#70461 = VECTOR ( 'NONE', #18610, 1000.000000000000000 ) ;
#70463 = CARTESIAN_POINT ( 'NONE',  ( 75.48921356237309510, -27.52281430457107803, 5.000000000000000000 ) ) ;
#70464 = EDGE_CURVE ( 'NONE', #23833, #17476, #92547, .T. ) ;
#70465 = DIRECTION ( 'NONE',  ( -0.6830127018922181881, 0.6830127018922202975, -0.2588190451025214056 ) ) ;
#70466 = CARTESIAN_POINT ( 'NONE',  ( 19.49999999999987210, 18.43112307739199451, 4.000000000000000000 ) ) ;
#70467 = ORIENTED_EDGE ( 'NONE', *, *, #6738, .T. ) ;
#70468 = PLANE ( 'NONE',  #120656 ) ;
#70469 = DIRECTION ( 'NONE',  ( 0.7071067811865487940, 0.7071067811865463515, 0.000000000000000000 ) ) ;
#70470 = ORIENTED_EDGE ( 'NONE', *, *, #13089, .F. ) ;
#70473 = ADVANCED_FACE ( 'NONE', ( #52364 ), #142260, .F. ) ;
#70472 = ORIENTED_EDGE ( 'NONE', *, *, #16788, .T. ) ;
#70471 = DIRECTION ( 'NONE',  ( 0.6830127018922180770, -0.6830127018922204085, -0.2588190451025213501 ) ) ;
#70474 = ORIENTED_EDGE ( 'NONE', *, *, #28782, .F. ) ;
#70475 = DIRECTION ( 'NONE',  ( 0.7071067811865486830, -0.7071067811865464625, -0.000000000000000000 ) ) ;
#70476 = DIRECTION ( 'NONE',  ( 0.7071067811865487940, -0.7071067811865463515, 0.000000000000000000 ) ) ;
#70477 = AXIS2_PLACEMENT_3D ( 'NONE', #75893, #123703, #68603 ) ;
#70478 = ORIENTED_EDGE ( 'NONE', *, *, #15017, .T. ) ;
#70479 = CARTESIAN_POINT ( 'NONE',  ( 20.81601139373100295, 28.73617430169773002, 5.000000000000000000 ) ) ;
#70480 = DIRECTION ( 'NONE',  ( -0.7071067811865486830, 0.7071067811865464625, 0.000000000000000000 ) ) ;
#70481 = VECTOR ( 'NONE', #113582, 999.9999999999998863 ) ;
#70482 = EDGE_CURVE ( 'NONE', #65352, #13630, #19733, .T. ) ;
#70483 = VERTEX_POINT ( 'NONE', #10970 ) ;
#70484 = CARTESIAN_POINT ( 'NONE',  ( 12.19999999999999574, -34.51840020119763608, 17.97447928118983640 ) ) ;
#70486 = DIRECTION ( 'NONE',  ( 0.3543493200069162685, -0.000000000000000000, -0.9351131265310288487 ) ) ;
#70485 = VECTOR ( 'NONE', #126587, 1000.000000000000227 ) ;
#70487 = DIRECTION ( 'NONE',  ( 0.7071067811865486830, -0.7071067811865464625, -0.000000000000000000 ) ) ;
#70488 = LINE ( 'NONE', #57442, #33173 ) ;
#70489 = CARTESIAN_POINT ( 'NONE',  ( 126.0561293963919667, -6.895973075043523970, 2.684650104021446992 ) ) ;
#70490 = CARTESIAN_POINT ( 'NONE',  ( -34.92500000000001137, -5.240707523384228850, 4.255531930566255561 ) ) ;
#70491 = FACE_OUTER_BOUND ( 'NONE', #82495, .T. ) ;
#70492 = ORIENTED_EDGE ( 'NONE', *, *, #75185, .F. ) ;
#70493 = ADVANCED_FACE ( 'NONE', ( #89977 ), #819, .F. ) ;
#70494 = ORIENTED_EDGE ( 'NONE', *, *, #97573, .T. ) ;
#70495 = ORIENTED_EDGE ( 'NONE', *, *, #73083, .F. ) ;
#70496 = CARTESIAN_POINT ( 'NONE',  ( 117.6666666666666714, 6.884901960086285300, 3.975000000000003642 ) ) ;
#70497 = EDGE_CURVE ( 'NONE', #30921, #5268, #34198, .T. ) ;
#70498 = VERTEX_POINT ( 'NONE', #134962 ) ;
#70499 = VECTOR ( 'NONE', #79002, 1000.000000000000114 ) ;
#70500 = VERTEX_POINT ( 'NONE', #66126 ) ;
#70501 = CIRCLE ( 'NONE', #121545, 2.500000000000000444 ) ;
#70502 = VERTEX_POINT ( 'NONE', #100173 ) ;
#70503 = LINE ( 'NONE', #114646, #96440 ) ;
#70504 = LINE ( 'NONE', #114647, #124983 ) ;
#70505 = ORIENTED_EDGE ( 'NONE', *, *, #43535, .T. ) ;
#70506 = DIRECTION ( 'NONE',  ( 0.7071067811865487940, 0.7071067811865463515, -0.000000000000000000 ) ) ;
#70507 = CARTESIAN_POINT ( 'NONE',  ( 0.4892135623730947680, -27.52281430457055578, 5.000000000000000000 ) ) ;
#70508 = CONICAL_SURFACE ( 'NONE', #137627, 2.055000000000000604, 0.9599310885968764806 ) ;
#70509 = LINE ( 'NONE', #15322, #86 ) ;
#70510 = CARTESIAN_POINT ( 'NONE',  ( 109.0837635252314470, -6.110000000000001208, -3.741295971395164515E-16 ) ) ;
#70511 = ORIENTED_EDGE ( 'NONE', *, *, #93080, .F. ) ;
#70512 = EDGE_CURVE ( 'NONE', #120212, #128359, #46357, .T. ) ;
#70513 = CARTESIAN_POINT ( 'NONE',  ( -9.183988606268997046, 28.73617430169793607, 5.000000000000000000 ) ) ;
#70514 = LINE ( 'NONE', #114657, #128388 ) ;
#70515 = DIRECTION ( 'NONE',  ( -0.7071067811865486830, -0.7071067811865464625, 0.000000000000000000 ) ) ;
#70516 = SURFACE_STYLE_USAGE ( .BOTH. , #37857 ) ;
#70517 = PLANE ( 'NONE',  #79345 ) ;
#70518 = DIRECTION ( 'NONE',  ( -0.6830127018922181881, 0.6830127018922202975, -0.2588190451025214056 ) ) ;
#70519 = VECTOR ( 'NONE', #84157, 1000.000000000000000 ) ;
#70520 = CARTESIAN_POINT ( 'NONE',  ( 39.60002705046289151, 5.819803920172570422, 5.819803920172574863 ) ) ;
#70521 = DIRECTION ( 'NONE',  ( -0.7071067811865487940, 0.7071067811865463515, -0.000000000000000000 ) ) ;
#70522 = VECTOR ( 'NONE', #104966, 999.9999999999998863 ) ;
#70523 = ORIENTED_EDGE ( 'NONE', *, *, #20731, .T. ) ;
#70524 = ORIENTED_EDGE ( 'NONE', *, *, #139242, .T. ) ;
#70525 = AXIS2_PLACEMENT_3D ( 'NONE', #61696, #105856, #141366 ) ;
#70526 = CARTESIAN_POINT ( 'NONE',  ( 38.18749999999998579, -5.819803920172573086, 5.819803920172572198 ) ) ;
#70527 = ORIENTED_EDGE ( 'NONE', *, *, #45824, .F. ) ;
#70528 = VERTEX_POINT ( 'NONE', #89285 ) ;
#70529 = DIRECTION ( 'NONE',  ( 0.6830127018922180770, 0.6830127018922202975, -0.2588190451025213501 ) ) ;
#70530 = DIRECTION ( 'NONE',  ( -0.7071067811865487940, 0.7071067811865463515, 0.000000000000000000 ) ) ;
#70531 = ORIENTED_EDGE ( 'NONE', *, *, #75296, .F. ) ;
#70532 = PLANE ( 'NONE',  #101283 ) ;
#70533 = CARTESIAN_POINT ( 'NONE',  ( 0.07735809023238571225, 0.3999999999999995781, 2.152165253127958700 ) ) ;
#70534 = DIRECTION ( 'NONE',  ( -0.7071067811865486830, -0.7071067811865464625, -0.000000000000000000 ) ) ;
#70535 = VECTOR ( 'NONE', #119201, 1000.000000000000000 ) ;
#70536 = CARTESIAN_POINT ( 'NONE',  ( 28.43793019189810423, -6.110000000000001208, 1.637169565754158951 ) ) ;
#70537 = ORIENTED_EDGE ( 'NONE', *, *, #15045, .F. ) ;
#70538 = LINE ( 'NONE', #15352, #108095 ) ;
#70539 = ORIENTED_EDGE ( 'NONE', *, *, #125007, .T. ) ;
#70540 = DIRECTION ( 'NONE',  ( -0.7071067811865486830, -0.7071067811865464625, 0.000000000000000000 ) ) ;
#70541 = CARTESIAN_POINT ( 'NONE',  ( 31.49999999999978684, 21.05218569542895679, 5.000000000000000000 ) ) ;
#70542 = DIRECTION ( 'NONE',  ( 1.000000000000000000, 0.000000000000000000, 0.000000000000000000 ) ) ;
#70543 = PLANE ( 'NONE',  #102017 ) ;
#70544 = ORIENTED_EDGE ( 'NONE', *, *, #94707, .T. ) ;
#70545 = ORIENTED_EDGE ( 'NONE', *, *, #23372, .F. ) ;
#70546 = CARTESIAN_POINT ( 'NONE',  ( 31.49999999999977973, -6.839392718269103888, -8.480912228396157104 ) ) ;
#70547 = PLANE ( 'NONE',  #73988 ) ;
#70548 = CARTESIAN_POINT ( 'NONE',  ( -42.29974487139158157, -27.71228299555235708, 4.000000000000000000 ) ) ;
#70549 = EDGE_CURVE ( 'NONE', #47748, #68933, #23283, .T. ) ;
#70550 = CARTESIAN_POINT ( 'NONE',  ( 44.68293019189811588, -1.637169565754158951, -6.109999999999998543 ) ) ;
#70551 = ADVANCED_FACE ( 'NONE', ( #88591 ), #90733, .T. ) ;
#70552 = CARTESIAN_POINT ( 'NONE',  ( 123.6458333333333286, 2.130196079827412436, -7.950000000000009059 ) ) ;
#70554 = EDGE_CURVE ( 'NONE', #63130, #86567, #45803, .T. ) ;
#70553 = DIRECTION ( 'NONE',  ( 0.000000000000000000, 0.000000000000000000, 1.000000000000000000 ) ) ;
#70555 = EDGE_LOOP ( 'NONE', ( #60709, #102768, #70598, #37253, #37095, #112488 ) ) ;
#70556 = ORIENTED_EDGE ( 'NONE', *, *, #55848, .F. ) ;
#70557 = DIRECTION ( 'NONE',  ( 0.7071067811865486830, -0.7071067811865464625, -0.000000000000000000 ) ) ;
#70558 = VERTEX_POINT ( 'NONE', #98715 ) ;
#70559 = EDGE_CURVE ( 'NONE', #106633, #67375, #109600, .T. ) ;
#70560 = VECTOR ( 'NONE', #113133, 1000.000000000000000 ) ;
#70561 = CYLINDRICAL_SURFACE ( 'NONE', #122914, 2.500000000000000444 ) ;
#70562 = ORIENTED_EDGE ( 'NONE', *, *, #48772, .T. ) ;
#70563 = DIRECTION ( 'NONE',  ( 0.7071067811865487940, 0.7071067811865463515, -0.000000000000000000 ) ) ;
#70564 = CARTESIAN_POINT ( 'NONE',  ( -34.49999999999975842, 22.21934299833216997, 4.348028800457638177 ) ) ;
#70565 = ADVANCED_FACE ( 'NONE', ( #44386 ), #57391, .F. ) ;
#70566 = FACE_BOUND ( 'NONE', #89966, .T. ) ;
#70567 = EDGE_CURVE ( 'NONE', #122496, #37221, #67564, .T. ) ;
#70568 = DIRECTION ( 'NONE',  ( -0.7071067811865487940, 0.7071067811865463515, -0.000000000000000000 ) ) ;
#70569 = CARTESIAN_POINT ( 'NONE',  ( 0.7071067811865398012, -18.74070752338409562, 5.000000000000000000 ) ) ;
#70570 = LINE ( 'NONE', #114714, #131936 ) ;
#70571 = PLANE ( 'NONE',  #24903 ) ;
#70573 = EDGE_LOOP ( 'NONE', ( #84408, #71754, #26283, #45702 ) ) ;
#70572 = LINE ( 'NONE', #127778, #80599 ) ;
#70574 = VECTOR ( 'NONE', #42226, 1000.000000000000000 ) ;
#70575 = PLANE ( 'NONE',  #19399 ) ;
#70576 = EDGE_CURVE ( 'NONE', #68975, #93231, #66825, .T. ) ;
#70577 = EDGE_LOOP ( 'NONE', ( #8838, #52299, #96414, #64886, #76615 ) ) ;
#70578 = ORIENTED_EDGE ( 'NONE', *, *, #53115, .F. ) ;
#70579 = CARTESIAN_POINT ( 'NONE',  ( 70.49543019189810877, 5.291415217122916737, 3.055000000000001936 ) ) ;
#70580 = VERTEX_POINT ( 'NONE', #101568 ) ;
#70581 = PLANE ( 'NONE',  #102239 ) ;
#70582 = VECTOR ( 'NONE', #59773, 1000.000000000000000 ) ;
#70583 = DIRECTION ( 'NONE',  ( 0.7071067811865486830, -0.7071067811865464625, -0.000000000000000000 ) ) ;
#70584 = ORIENTED_EDGE ( 'NONE', *, *, #139680, .T. ) ;
#70585 = DIRECTION ( 'NONE',  ( -0.6830127018922180770, -0.6830127018922204085, -0.2588190451025213501 ) ) ;
#70586 = EDGE_CURVE ( 'NONE', #58831, #119104, #132095, .T. ) ;
#70587 = CARTESIAN_POINT ( 'NONE',  ( -3.707106781186514599, -3.740707523384248390, 5.000000000000000000 ) ) ;
#70588 = AXIS2_PLACEMENT_3D ( 'NONE', #99087, #143332, #132506 ) ;
#70589 = CARTESIAN_POINT ( 'NONE',  ( -31.49999999999977973, 18.43112307739199451, 4.000000000000000000 ) ) ;
#70590 = DIRECTION ( 'NONE',  ( -1.000000000000000000, -0.000000000000000000, -0.000000000000000000 ) ) ;
#70591 = DIRECTION ( 'NONE',  ( -0.000000000000000000, 0.000000000000000000, 1.000000000000000000 ) ) ;
#70592 = DIRECTION ( 'NONE',  ( -0.7071067811865487940, 0.7071067811865463515, 0.000000000000000000 ) ) ;
#70593 = VERTEX_POINT ( 'NONE', #78414 ) ;
#70594 = EDGE_CURVE ( 'NONE', #16291, #61647, #35655, .T. ) ;
#70595 = ORIENTED_EDGE ( 'NONE', *, *, #92510, .T. ) ;
#70596 = DIRECTION ( 'NONE',  ( 0.7071067811865486830, -0.7071067811865464625, -0.000000000000000000 ) ) ;
#70597 = CARTESIAN_POINT ( 'NONE',  ( -33.48921356237309510, -27.52281430457078670, 5.000000000000000000 ) ) ;
#70598 = ORIENTED_EDGE ( 'NONE', *, *, #79415, .T. ) ;
#70599 = EDGE_LOOP ( 'NONE', ( #133360, #132772, #11307, #41000 ) ) ;
#70600 = ORIENTED_EDGE ( 'NONE', *, *, #22668, .T. ) ;
#70601 = DIRECTION ( 'NONE',  ( 0.000000000000000000, -1.000000000000000000, 0.000000000000000000 ) ) ;
#70602 = PLANE ( 'NONE',  #48484 ) ;
#70603 = EDGE_LOOP ( 'NONE', ( #63640, #56155, #129349, #133677 ) ) ;
#70604 = CARTESIAN_POINT ( 'NONE',  ( 0.000000000000000000, 0.000000000000000000, 5.000000000000000000 ) ) ;
#70605 = EDGE_CURVE ( 'NONE', #96290, #23136, #121884, .T. ) ;
#70606 = VECTOR ( 'NONE', #82259, 1000.000000000000000 ) ;
#70607 = DIRECTION ( 'NONE',  ( -0.000000000000000000, -0.3543493200069152693, 0.9351131265310292928 ) ) ;
#70608 = AXIS2_PLACEMENT_3D ( 'NONE', #16730, #14596, #92135 ) ;
#70609 = CARTESIAN_POINT ( 'NONE',  ( 10.85873647476855197, 5.808823158059031044, -5.808823158059038150 ) ) ;
#70610 = AXIS2_PLACEMENT_3D ( 'NONE', #45661, #10135, #123210 ) ;
#70611 = CARTESIAN_POINT ( 'NONE',  ( 0.000000000000000000, 0.000000000000000000, 5.000000000000000000 ) ) ;
#70612 = ORIENTED_EDGE ( 'NONE', *, *, #113857, .F. ) ;
#70613 = MECHANICAL_DESIGN_GEOMETRIC_PRESENTATION_REPRESENTATION (  '', ( #10322 ), #8045 ) ;
#70614 = CARTESIAN_POINT ( 'NONE',  ( -8.700255128608413102, -27.71228299555199825, 4.000000000000000000 ) ) ;
#70615 = EDGE_CURVE ( 'NONE', #128260, #44264, #120364, .T. ) ;
#70616 = CARTESIAN_POINT ( 'NONE',  ( 25.08333333333333570, -5.278424836066144543, 3.047499999999995879 ) ) ;
#70618 = ORIENTED_EDGE ( 'NONE', *, *, #129527, .T. ) ;
#70617 = PLANE ( 'NONE',  #7803 ) ;
#70619 = DIRECTION ( 'NONE',  ( -0.7071067811865486830, 0.7071067811865464625, 0.000000000000000000 ) ) ;
#70620 = VERTEX_POINT ( 'NONE', #65424 ) ;
#70621 = CARTESIAN_POINT ( 'NONE',  ( 23.03315071937583980, 7.620612595215163765, 4.000000000000000000 ) ) ;
#70622 = DIRECTION ( 'NONE',  ( -0.3543493200069162685, -0.000000000000000000, -0.9351131265310288487 ) ) ;
#70623 = DIRECTION ( 'NONE',  ( 0.000000000000000000, 0.000000000000000000, 1.000000000000000000 ) ) ;
#70624 = ORIENTED_EDGE ( 'NONE', *, *, #66782, .F. ) ;
#70625 = DIRECTION ( 'NONE',  ( -0.000000000000000000, 0.000000000000000000, 1.000000000000000000 ) ) ;
#70626 = EDGE_CURVE ( 'NONE', #53240, #18032, #10277, .T. ) ;
#70627 = PLANE ( 'NONE',  #35644 ) ;
#70628 = DIRECTION ( 'NONE',  ( 0.7071067811865487940, 0.7071067811865463515, 0.000000000000000000 ) ) ;
#70629 = CARTESIAN_POINT ( 'NONE',  ( -57.48921356237308800, -27.52281430457095368, 5.000000000000000000 ) ) ;
#70630 = ORIENTED_EDGE ( 'NONE', *, *, #132798, .F. ) ;
#70631 = CARTESIAN_POINT ( 'NONE',  ( -34.47516574401893052, 0.02806734111581892996, 4.998110765256835286 ) ) ;
#70632 = LINE ( 'NONE', #90937, #100259 ) ;
#70633 = CARTESIAN_POINT ( 'NONE',  ( 7.629139616203772789, 5.278424836066147208, 3.047499999999990550 ) ) ;
#70634 = CARTESIAN_POINT ( 'NONE',  ( 8.292893218813393474, 20.25929247661551713, 5.000000000000000000 ) ) ;
#70635 = DIRECTION ( 'NONE',  ( -0.000000000000000000, -0.3543493200069152693, 0.9351131265310292928 ) ) ;
#70637 = EDGE_CURVE ( 'NONE', #133903, #139608, #21876, .T. ) ;
#70636 = EDGE_LOOP ( 'NONE', ( #103593, #94821, #33096, #137641 ) ) ;
#70638 = EDGE_LOOP ( 'NONE', ( #62357, #119145, #29490, #83870 ) ) ;
#70639 = LINE ( 'NONE', #128550, #28668 ) ;
#70640 = DIRECTION ( 'NONE',  ( -1.000000000000000000, -1.224606353822377258E-16, -0.000000000000000000 ) ) ;
#70641 = CARTESIAN_POINT ( 'NONE',  ( 7.999569808101885116, -3.967499999999998028, -6.871911579029511330 ) ) ;
#70642 = DIRECTION ( 'NONE',  ( -0.7071067811865486830, 0.7071067811865464625, 0.000000000000000000 ) ) ;
#70643 = DIRECTION ( 'NONE',  ( 0.000000000000000000, -1.000000000000000000, 0.000000000000000000 ) ) ;
#70644 = CARTESIAN_POINT ( 'NONE',  ( -50.99451991528749062, 28.92564299267973738, 4.000000000000000000 ) ) ;
#70645 = CARTESIAN_POINT ( 'NONE',  ( -11.67183060077638856, -0.7407075233842701500, 4.000000000000000000 ) ) ;
#70646 = ORIENTED_EDGE ( 'NONE', *, *, #62518, .T. ) ;
#70647 = DIRECTION ( 'NONE',  ( -0.3543493200069162685, -0.000000000000000000, -0.9351131265310288487 ) ) ;
#70648 = FILL_AREA_STYLE ('',( #80784 ) ) ;
#70649 = CARTESIAN_POINT ( 'NONE',  ( 45.84959685856478018, 6.109999999999997655, 1.637169565754163836 ) ) ;
#70650 = CARTESIAN_POINT ( 'NONE',  ( 62.99451991528749772, 28.92564299267982264, 4.000000000000000000 ) ) ;
#70651 = EDGE_CURVE ( 'NONE', #12281, #61250, #55973, .T. ) ;
#70652 = ORIENTED_EDGE ( 'NONE', *, *, #105102, .T. ) ;
#70653 = EDGE_CURVE ( 'NONE', #129678, #85221, #50074, .T. ) ;
#70654 = EDGE_LOOP ( 'NONE', ( #131692, #91080, #138141, #106583 ) ) ;
#70655 = DIRECTION ( 'NONE',  ( 0.7071067811865487940, 0.7071067811865463515, 0.000000000000000000 ) ) ;
#70656 = ORIENTED_EDGE ( 'NONE', *, *, #16711, .F. ) ;
#70657 = DIRECTION ( 'NONE',  ( -0.7071067811865486830, -0.7071067811865464625, 0.000000000000000000 ) ) ;
#70658 = LINE ( 'NONE', #27103, #36823 ) ;
#70659 = PLANE ( 'NONE',  #62790 ) ;
#70660 = CARTESIAN_POINT ( 'NONE',  ( 24.29974487139158867, -27.71228299555223273, 4.000000000000000000 ) ) ;
#70661 = ADVANCED_FACE ( 'NONE', ( #58125 ), #13829, .F. ) ;
#70662 = CARTESIAN_POINT ( 'NONE',  ( 0.000000000000000000, 0.000000000000000000, 5.000000000000000000 ) ) ;
#70663 = DIRECTION ( 'NONE',  ( -0.6830127018922181881, 0.6830127018922202975, -0.2588190451025214056 ) ) ;
#70664 = ORIENTED_EDGE ( 'NONE', *, *, #40922, .F. ) ;
#70665 = EDGE_CURVE ( 'NONE', #9428, #71344, #103691, .T. ) ;
#70666 = CARTESIAN_POINT ( 'NONE',  ( 50.99451991528749062, 28.92564299267973738, 4.000000000000000000 ) ) ;
#70667 = CARTESIAN_POINT ( 'NONE',  ( -34.92500000000001137, -1.298069433178978382, 4.500000000000000888 ) ) ;
#70668 = CARTESIAN_POINT ( 'NONE',  ( 30.18398860626900060, 28.73617430169808173, 5.000000000000000000 ) ) ;
#70669 = DIRECTION ( 'NONE',  ( 0.7071067811865486830, -0.7071067811865463515, 0.000000000000000000 ) ) ;
#70670 = CARTESIAN_POINT ( 'NONE',  ( 69.78752705046289861, 0.000000000000000000, -7.949999999999998401 ) ) ;
#70671 = VECTOR ( 'NONE', #44849, 1000.000000000000227 ) ;
#70672 = DIRECTION ( 'NONE',  ( 0.7071067811865487940, 0.7071067811865463515, -0.000000000000000000 ) ) ;
#70673 = VERTEX_POINT ( 'NONE', #39191 ) ;
#70674 = ORIENTED_EDGE ( 'NONE', *, *, #126459, .F. ) ;
#70675 = CARTESIAN_POINT ( 'NONE',  ( 60.50000000000000000, 0.000000000000000000, -7.950000000000000178 ) ) ;
#70676 = CARTESIAN_POINT ( 'NONE',  ( -0.4116149059483131256, 22.22500000000000142, 4.777194822843814137 ) ) ;
#70677 = VECTOR ( 'NONE', #114659, 999.9999999999998863 ) ;
#70678 = DIRECTION ( 'NONE',  ( -0.000000000000000000, 0.000000000000000000, 1.000000000000000000 ) ) ;
#70679 = CARTESIAN_POINT ( 'NONE',  ( -32.99999999999976552, 5.966399257802205369, 5.000000000000000000 ) ) ;
#70680 = VERTEX_POINT ( 'NONE', #116006 ) ;
#70681 = EDGE_CURVE ( 'NONE', #20616, #69496, #137075, .T. ) ;
#70682 = DIRECTION ( 'NONE',  ( 0.000000000000000000, -1.000000000000000000, 0.000000000000000000 ) ) ;
#70683 = VECTOR ( 'NONE', #139283, 1000.000000000000000 ) ;
#70684 = DIRECTION ( 'NONE',  ( 0.000000000000000000, -1.000000000000000000, 0.000000000000000000 ) ) ;
#70685 = CARTESIAN_POINT ( 'NONE',  ( 56.43793019189809712, -6.110000000000001208, 1.637169565754158951 ) ) ;
#70686 = CARTESIAN_POINT ( 'NONE',  ( 33.48921356237309510, -27.52281430457078670, 5.000000000000000000 ) ) ;
#70687 = ORIENTED_EDGE ( 'NONE', *, *, #101732, .F. ) ;
#70688 = EDGE_LOOP ( 'NONE', ( #75426, #96147, #61579, #80966 ) ) ;
#70689 = PLANE ( 'NONE',  #58234 ) ;
#70690 = LINE ( 'NONE', #80838, #133296 ) ;
#70691 = DIRECTION ( 'NONE',  ( 1.000000000000000000, 0.000000000000000000, 0.000000000000000000 ) ) ;
#70692 = LINE ( 'NONE', #4610, #9243 ) ;
#70693 = DIRECTION ( 'NONE',  ( -0.7071067811865487940, 0.7071067811865463515, 0.000000000000000000 ) ) ;
#70695 = ORIENTED_EDGE ( 'NONE', *, *, #133193, .F. ) ;
#70694 = CARTESIAN_POINT ( 'NONE',  ( 2.999999999999999112, 1.399999999999987699, -20.40202195861970580 ) ) ;
#70696 = DIRECTION ( 'NONE',  ( -0.000000000000000000, 0.3543493200069153248, 0.9351131265310292928 ) ) ;
#70697 = LINE ( 'NONE', #3924, #57033 ) ;
#70698 = CARTESIAN_POINT ( 'NONE',  ( -9.826759492923502037, -22.22500000000000142, 14.51066154962963139 ) ) ;
#70699 = DIRECTION ( 'NONE',  ( 0.6830127018922180770, -0.6830127018922204085, -0.2588190451025213501 ) ) ;
#70700 = VECTOR ( 'NONE', #44100, 1000.000000000000000 ) ;
#70701 = VERTEX_POINT ( 'NONE', #24728 ) ;
#70702 = VECTOR ( 'NONE', #133004, 1000.000000000000000 ) ;
#70704 = EDGE_CURVE ( 'NONE', #132568, #70259, #138503, .T. ) ;
#70703 = VECTOR ( 'NONE', #73768, 1000.000000000000000 ) ;
#70705 = VERTEX_POINT ( 'NONE', #36338 ) ;
#70706 = VECTOR ( 'NONE', #64626, 1000.000000000000000 ) ;
#70707 = CARTESIAN_POINT ( 'NONE',  ( -34.42500000000001137, 0.000000000000000000, 4.500000000000000888 ) ) ;
#70708 = EDGE_CURVE ( 'NONE', #129051, #138298, #37774, .T. ) ;
#70709 = LINE ( 'NONE', #93140, #95028 ) ;
#70710 = CARTESIAN_POINT ( 'NONE',  ( 110.3291937171295700, -3.975000000000001865, 6.884901960086284411 ) ) ;
#70711 = DIRECTION ( 'NONE',  ( 0.7071067811865486830, -0.7071067811865464625, -0.000000000000000000 ) ) ;
#70712 = ORIENTED_EDGE ( 'NONE', *, *, #23525, .T. ) ;
#70713 = EDGE_LOOP ( 'NONE', ( #120593, #37317, #44882, #28797 ) ) ;
#70714 = DIRECTION ( 'NONE',  ( -0.000000000000000000, -0.3543493200069152693, 0.9351131265310292928 ) ) ;
#70715 = CARTESIAN_POINT ( 'NONE',  ( 45.29974487139158867, -27.71228299555237840, 4.000000000000000000 ) ) ;
#70716 = EDGE_CURVE ( 'NONE', #139251, #132813, #124761, .T. ) ;
#70717 = EDGE_CURVE ( 'NONE', #69036, #5408, #47266, .T. ) ;
#70718 = ORIENTED_EDGE ( 'NONE', *, *, #37918, .T. ) ;
#70719 = CARTESIAN_POINT ( 'NONE',  ( -34.92500000000001137, 6.662461875838927128, 4.000000000000000000 ) ) ;
#70720 = EDGE_LOOP ( 'NONE', ( #141333, #140097, #13115, #50361, #125949 ) ) ;
#70721 = CARTESIAN_POINT ( 'NONE',  ( 61.47502705046287730, -5.819803920172573086, 5.819803920172573086 ) ) ;
#70722 = CARTESIAN_POINT ( 'NONE',  ( -36.48921356237310221, -27.52281430457080802, 5.000000000000000000 ) ) ;
#70723 = EDGE_CURVE ( 'NONE', #141627, #95547, #126196, .T. ) ;
#70724 = FACE_BOUND ( 'NONE', #8476, .T. ) ;
#70725 = ADVANCED_FACE ( 'NONE', ( #113155 ), #41650, .T. ) ;
#70726 = CARTESIAN_POINT ( 'NONE',  ( 21.32816939922336985, -18.74070752338409207, 4.000000000000000000 ) ) ;
#70727 = CARTESIAN_POINT ( 'NONE',  ( -27.70679250724057852, 20.25929247661551358, 20.83292124670821366 ) ) ;
#70728 = CARTESIAN_POINT ( 'NONE',  ( -63.48921356237309510, -27.52281430457099631, 5.000000000000000000 ) ) ;
#70729 = DIRECTION ( 'NONE',  ( -0.000000000000000000, 0.3543493200069153248, 0.9351131265310292928 ) ) ;
#70730 = DIRECTION ( 'NONE',  ( 0.000000000000000000, -1.000000000000000000, 0.000000000000000000 ) ) ;
#70732 = EDGE_CURVE ( 'NONE', #51437, #94410, #26175, .T. ) ;
#70731 = APPLICATION_PROTOCOL_DEFINITION ( 'draft international standard', 'automotive_design', 1998, #30025 ) ;
#70733 = ORIENTED_EDGE ( 'NONE', *, *, #11055, .T. ) ;
#70734 = ORIENTED_EDGE ( 'NONE', *, *, #134822, .F. ) ;
#70735 = CARTESIAN_POINT ( 'NONE',  ( 93.09959685856478018, -6.109999999999997655, -1.637169565754160283 ) ) ;
#70736 = EDGE_LOOP ( 'NONE', ( #111085, #8786, #68039, #120361 ) ) ;
#70737 = DIRECTION ( 'NONE',  ( -0.7071067811865486830, 0.7071067811865464625, 0.000000000000000000 ) ) ;
#70738 = LINE ( 'NONE', #103310, #14589 ) ;
#70739 = EDGE_CURVE ( 'NONE', #15691, #71257, #70438, .T. ) ;
#70740 = DIRECTION ( 'NONE',  ( 0.000000000000000000, 0.000000000000000000, 1.000000000000000000 ) ) ;
#70741 = ORIENTED_EDGE ( 'NONE', *, *, #83327, .F. ) ;
#70742 = CARTESIAN_POINT ( 'NONE',  ( -21.70710678118638981, -9.740707523384184441, 5.000000000000000000 ) ) ;
#70743 = PLANE ( 'NONE',  #77875 ) ;
#70744 = CARTESIAN_POINT ( 'NONE',  ( 21.70701326429288613, -21.74070752338406365, 4.999753212805217117 ) ) ;
#70746 = CARTESIAN_POINT ( 'NONE',  ( 3.183988606268992161, 28.73617430169789699, 5.000000000000000000 ) ) ;
#70745 = CARTESIAN_POINT ( 'NONE',  ( 32.99999999999977263, -12.03360074219761700, 5.000000000000000000 ) ) ;
#70747 = DIRECTION ( 'NONE',  ( -0.000000000000000000, -0.3543493200069152693, 0.9351131265310292928 ) ) ;
#70748 = EDGE_CURVE ( 'NONE', #55182, #33283, #135648, .T. ) ;
#70749 = FACE_OUTER_BOUND ( 'NONE', #108140, .T. ) ;
#70750 = ORIENTED_EDGE ( 'NONE', *, *, #24566, .T. ) ;
#70751 = CARTESIAN_POINT ( 'NONE',  ( 34.45011844616451668, -1.483719188362489172, 5.000000000000000000 ) ) ;
#70752 = DIRECTION ( 'NONE',  ( -1.000000000000000000, -0.000000000000000000, 0.000000000000000000 ) ) ;
#70753 = ORIENTED_EDGE ( 'NONE', *, *, #100899, .F. ) ;
#70754 = EDGE_LOOP ( 'NONE', ( #74337, #101501, #127327, #51467 ) ) ;
#70755 = EDGE_LOOP ( 'NONE', ( #124930, #123794, #140751, #94621 ) ) ;
#70756 = ADVANCED_FACE ( 'NONE', ( #15252 ), #69701, .F. ) ;
#70757 = CARTESIAN_POINT ( 'NONE',  ( 49.14626352523143282, -4.472830434245840259, 4.472830434245838482 ) ) ;
#70758 = ADVANCED_FACE ( 'NONE', ( #105149 ), #80566, .T. ) ;
#70759 = EDGE_LOOP ( 'NONE', ( #95004, #42605, #77725, #93967, #89732 ) ) ;
#70760 = EDGE_CURVE ( 'NONE', #137485, #121162, #48638, .T. ) ;
#70761 = AXIS2_PLACEMENT_3D ( 'NONE', #142357, #43047, #24657 ) ;
#70762 = CARTESIAN_POINT ( 'NONE',  ( 13.02497294953710849, -4.461849672132299993, -4.461849672132299105 ) ) ;
#70763 = ORIENTED_EDGE ( 'NONE', *, *, #138137, .T. ) ;
#70764 = PLANE ( 'NONE',  #64180 ) ;
#70765 = ORIENTED_EDGE ( 'NONE', *, *, #128418, .F. ) ;
#70766 = DIRECTION ( 'NONE',  ( 0.3543493200069162685, -0.000000000000000000, -0.9351131265310288487 ) ) ;
#70767 = CARTESIAN_POINT ( 'NONE',  ( -54.48921356237310221, -27.52281430457093236, 5.000000000000000000 ) ) ;
#70769 = ORIENTED_EDGE ( 'NONE', *, *, #140432, .T. ) ;
#70768 = DIRECTION ( 'NONE',  ( 1.000000000000000000, 0.000000000000000000, 0.000000000000000000 ) ) ;
#70770 = ORIENTED_EDGE ( 'NONE', *, *, #141728, .T. ) ;
#70771 =( BOUNDED_CURVE ( )  B_SPLINE_CURVE ( 3, ( #17783, #73628, #137462, #95365 ),
 .UNSPECIFIED., .F., .F. ) 
 B_SPLINE_CURVE_WITH_KNOTS ( ( 4, 4 ),
 ( 5.143245962375951663, 6.645403452391247079 ),
 .UNSPECIFIED. ) 
 CURVE ( )  GEOMETRIC_REPRESENTATION_ITEM ( )  RATIONAL_B_SPLINE_CURVE ( ( 1.000000000000000000, 0.8206354192515209478, 0.8206354192515209478, 1.000000000000000000 ) ) 
 REPRESENTATION_ITEM ( '' )  );
#70772 = CARTESIAN_POINT ( 'NONE',  ( -34.42500000000001137, -13.45860074219784863, 5.000000000000000000 ) ) ;
#70773 = CARTESIAN_POINT ( 'NONE',  ( 48.18398860626899705, 28.73617430169820608, 5.000000000000000000 ) ) ;
#70774 = VERTEX_POINT ( 'NONE', #60247 ) ;
#70775 = CARTESIAN_POINT ( 'NONE',  ( 5.999999999999955591, -18.41253812416056945, 4.000000000000000000 ) ) ;
#70776 = ORIENTED_EDGE ( 'NONE', *, *, #118380, .F. ) ;
#70777 = AXIS2_PLACEMENT_3D ( 'NONE', #8358, #41028, #141791 ) ;
#70778 = EDGE_LOOP ( 'NONE', ( #92904, #64155, #138921, #94054 ) ) ;
#70779 = VERTEX_POINT ( 'NONE', #137800 ) ;
#70780 = ORIENTED_EDGE ( 'NONE', *, *, #7979, .F. ) ;
#70781 = LINE ( 'NONE', #128701, #88824 ) ;
#70782 = CARTESIAN_POINT ( 'NONE',  ( 25.39999999999999858, -57.15000000000003411, -15.92500000000064730 ) ) ;
#70783 = CARTESIAN_POINT ( 'NONE',  ( 12.69999999999999574, -22.26999999999999247, -39.79289321881344677 ) ) ;
#70784 = DIRECTION ( 'NONE',  ( -0.000000000000000000, -0.3543493200069152693, 0.9351131265310292928 ) ) ;
#70785 = PLANE ( 'NONE',  #118278 ) ;
#70786 = ORIENTED_EDGE ( 'NONE', *, *, #97226, .F. ) ;
#70787 = CARTESIAN_POINT ( 'NONE',  ( 0.000000000000000000, 0.000000000000000000, 0.000000000000000000 ) ) ;
#70788 = VECTOR ( 'NONE', #54808, 999.9999999999998863 ) ;
#70789 = CARTESIAN_POINT ( 'NONE',  ( 24.47873647476856007, -5.808823158059033709, 5.808823158059035485 ) ) ;
#70790 = DIRECTION ( 'NONE',  ( -1.000000000000000000, -1.224606353822377258E-16, -0.000000000000000000 ) ) ;
#70791 = VECTOR ( 'NONE', #112033, 999.9999999999998863 ) ;
#70792 = CARTESIAN_POINT ( 'NONE',  ( 95.93750000000000000, 5.819803920172574863, -5.819803920172573086 ) ) ;
#70793 = AXIS2_PLACEMENT_3D ( 'NONE', #92126, #114593, #59546 ) ;
#70794 = CARTESIAN_POINT ( 'NONE',  ( 8.423184310185783730, 2.500000000000000888, 0.000000000000000000 ) ) ;
#70795 = EDGE_LOOP ( 'NONE', ( #40368, #15601, #84096, #123352 ) ) ;
#70796 = ORIENTED_EDGE ( 'NONE', *, *, #19804, .F. ) ;
#70797 = ORIENTED_EDGE ( 'NONE', *, *, #17314, .T. ) ;
#70798 = FACE_OUTER_BOUND ( 'NONE', #55826, .T. ) ;
#70799 = DIRECTION ( 'NONE',  ( 0.000000000000000000, 0.000000000000000000, -1.000000000000000000 ) ) ;
#70800 = UNCERTAINTY_MEASURE_WITH_UNIT (LENGTH_MEASURE( 1.000000000000000082E-05 ), #102105, 'distance_accuracy_value', 'NONE');
#70801 = LINE ( 'NONE', #27251, #124031 ) ;
#70802 = VECTOR ( 'NONE', #24422, 1000.000000000000000 ) ;
#70803 = CARTESIAN_POINT ( 'NONE',  ( -18.70612307739182967, 22.22500000000000142, 4.000000000000000000 ) ) ;
#70804 = FACE_OUTER_BOUND ( 'NONE', #115293, .T. ) ;
#70805 = CARTESIAN_POINT ( 'NONE',  ( 74.14126352523146579, 4.472830434245837594, 4.472830434245841147 ) ) ;
#70806 = CARTESIAN_POINT ( 'NONE',  ( 73.87086038379622721, 6.884901960086289741, -3.974999999999993427 ) ) ;
#70807 = DIRECTION ( 'NONE',  ( -0.7071067811865486830, -0.7071067811865464625, 0.000000000000000000 ) ) ;
#70808 = DIRECTION ( 'NONE',  ( -1.000000000000000000, -0.000000000000000000, -0.000000000000000000 ) ) ;
#70809 = ADVANCED_BREP_SHAPE_REPRESENTATION ( '', ( #142006, #127880 ), #12041 ) ;
#70810 = PLANE ( 'NONE',  #44372 ) ;
#70811 = LINE ( 'NONE', #93957, #34975 ) ;
#70812 = ORIENTED_EDGE ( 'NONE', *, *, #47160, .F. ) ;
#70813 = DIRECTION ( 'NONE',  ( -1.000000000000000000, -1.369518533665899572E-16, 0.000000000000000000 ) ) ;
#70814 = ORIENTED_EDGE ( 'NONE', *, *, #131884, .F. ) ;
#70815 = DIRECTION ( 'NONE',  ( -0.3543493200069162685, -0.000000000000000000, -0.9351131265310288487 ) ) ;
#70817 = ORIENTED_EDGE ( 'NONE', *, *, #20748, .F. ) ;
#70816 = FACE_OUTER_BOUND ( 'NONE', #97147, .T. ) ;
#70818 = EDGE_CURVE ( 'NONE', #56703, #71811, #5801, .T. ) ;
#70819 = DIRECTION ( 'NONE',  ( -0.7071067811865486830, 0.7071067811865464625, -0.000000000000000000 ) ) ;
#70820 = DIRECTION ( 'NONE',  ( -0.000000000000000000, -0.3543493200069152693, 0.9351131265310292928 ) ) ;
#70821 = ORIENTED_EDGE ( 'NONE', *, *, #123500, .T. ) ;
#70822 = ADVANCED_FACE ( 'NONE', ( #83414 ), #95695, .F. ) ;
#70823 = DIRECTION ( 'NONE',  ( -0.6830127018922180770, -0.6830127018922204085, -0.2588190451025213501 ) ) ;
#70824 = ORIENTED_EDGE ( 'NONE', *, *, #62250, .T. ) ;
#70825 = CARTESIAN_POINT ( 'NONE',  ( 120.5375270504628844, -9.735942053221456900E-16, 7.949999999999998401 ) ) ;
#70826 = ORIENTED_EDGE ( 'NONE', *, *, #31453, .F. ) ;
#70827 = LINE ( 'NONE', #136758, #29046 ) ;
#70828 = CARTESIAN_POINT ( 'NONE',  ( 103.9125270504628844, -7.949999999999998401, -4.867971026610728450E-16 ) ) ;
#70829 = FACE_OUTER_BOUND ( 'NONE', #124894, .T. ) ;
#70830 = DIRECTION ( 'NONE',  ( 1.049727191138614875E-16, -0.5150380749100594846, 0.8571673007021091140 ) ) ;
#70831 = VERTEX_POINT ( 'NONE', #129036 ) ;
#70832 = EDGE_CURVE ( 'NONE', #85690, #28808, #52882, .T. ) ;
#70833 = CARTESIAN_POINT ( 'NONE',  ( 34.92499999999998295, -18.18334561358936341, 4.500000000000000888 ) ) ;
#70834 = FACE_OUTER_BOUND ( 'NONE', #6440, .T. ) ;
#70835 = LINE ( 'NONE', #128755, #55385 ) ;
#70836 = CARTESIAN_POINT ( 'NONE',  ( 22.75000000000000355, -7.464222240803106570E-16, -6.094999999999989981 ) ) ;
#70837 = PLANE ( 'NONE',  #72314 ) ;
#70838 = CARTESIAN_POINT ( 'NONE',  ( 5.999999999999950262, -13.39766691384882513, -10.96608748226467256 ) ) ;
#70839 = ORIENTED_EDGE ( 'NONE', *, *, #124872, .T. ) ;
#70840 = B_SPLINE_CURVE_WITH_KNOTS ( 'NONE', 3,
 ( #44330, #133462, #77662, #123317 ),
 .UNSPECIFIED., .F., .F.,
 ( 4, 4 ),
 ( 0.008851590069444708123, 0.009100162336955338813 ),
 .UNSPECIFIED. ) ;
#70841 = EDGE_CURVE ( 'NONE', #3523, #90074, #18840, .T. ) ;
#70842 = LINE ( 'NONE', #101297, #9767 ) ;
#70843 = ORIENTED_EDGE ( 'NONE', *, *, #34108, .F. ) ;
#70844 = CARTESIAN_POINT ( 'NONE',  ( 89.10459685856477563, 1.637169565754164946, -6.109999999999999432 ) ) ;
#70845 = LINE ( 'NONE', #49814, #89430 ) ;
#70846 = DIRECTION ( 'NONE',  ( 0.000000000000000000, -1.000000000000000000, 0.000000000000000000 ) ) ;
#70847 = PLANE ( 'NONE',  #115017 ) ;
#70848 = EDGE_LOOP ( 'NONE', ( #99356, #19555, #41476, #141819, #71015 ) ) ;
#70849 = EDGE_CURVE ( 'NONE', #36287, #60685, #142090, .T. ) ;
#70850 = CARTESIAN_POINT ( 'NONE',  ( -26.99999999999981526, -18.03360074219755660, 5.000000000000000000 ) ) ;
#70851 = DIRECTION ( 'NONE',  ( -0.6830127018922180770, -0.6830127018922204085, -0.2588190451025213501 ) ) ;
#70852 = DIRECTION ( 'NONE',  ( 0.7071067811865487940, 0.7071067811865463515, 0.000000000000000000 ) ) ;
#70853 = CARTESIAN_POINT ( 'NONE',  ( 0.000000000000000000, 0.000000000000000000, 7.950000000000000178 ) ) ;
#70855 = ORIENTED_EDGE ( 'NONE', *, *, #127279, .F. ) ;
#70854 = FACE_OUTER_BOUND ( 'NONE', #35277, .T. ) ;
#70856 = SPHERICAL_SURFACE ( 'NONE', #41473, 0.5000000000000000000 ) ;
#70857 = EDGE_CURVE ( 'NONE', #127030, #122448, #29709, .T. ) ;
#70858 = CARTESIAN_POINT ( 'NONE',  ( 15.49238828748955576, 3.061616997868383634E-16, -2.500000000000000444 ) ) ;
#70859 = SURFACE_STYLE_FILL_AREA ( #125942 ) ;
#70860 = SURFACE_STYLE_USAGE ( .BOTH. , #114335 ) ;
#70861 = ORIENTED_EDGE ( 'NONE', *, *, #76881, .T. ) ;
#70862 = AXIS2_PLACEMENT_3D ( 'NONE', #129708, #99765, #106506 ) ;
#70863 = ORIENTED_EDGE ( 'NONE', *, *, #125748, .F. ) ;
#70864 = VERTEX_POINT ( 'NONE', #73957 ) ;
#70865 = CARTESIAN_POINT ( 'NONE',  ( 82.25043019189810423, 3.055000000000002824, -5.291415217122919401 ) ) ;
#70866 = ORIENTED_EDGE ( 'NONE', *, *, #36012, .T. ) ;
#70867 = VECTOR ( 'NONE', #60179, 1000.000000000000227 ) ;
#70868 = PLANE ( 'NONE',  #112346 ) ;
#70869 = ADVANCED_FACE ( 'NONE', ( #19564 ), #7230, .F. ) ;
#70870 = CARTESIAN_POINT ( 'NONE',  ( -42.48921356237308800, -27.52281430457085065, 5.000000000000000000 ) ) ;
#70871 = DIRECTION ( 'NONE',  ( 0.7071067811865486830, -0.7071067811865464625, -0.000000000000000000 ) ) ;
#70872 = CARTESIAN_POINT ( 'NONE',  ( 56.99451991528749062, 28.92564299267978001, 4.000000000000000000 ) ) ;
#70873 = ORIENTED_EDGE ( 'NONE', *, *, #110596, .T. ) ;
#70874 = LINE ( 'NONE', #47019, #95411 ) ;
#70875 = DIRECTION ( 'NONE',  ( 0.7071067811865486830, -0.7071067811865464625, -0.000000000000000000 ) ) ;
#70876 = EDGE_CURVE ( 'NONE', #127957, #11859, #63808, .T. ) ;
#70877 = EDGE_CURVE ( 'NONE', #136293, #20115, #107281, .T. ) ;
#70878 = CARTESIAN_POINT ( 'NONE',  ( 72.53709685856478018, -3.054999999999998828, -5.291415217122919401 ) ) ;
#70879 = ORIENTED_EDGE ( 'NONE', *, *, #64941, .T. ) ;
#70880 = VECTOR ( 'NONE', #74199, 1000.000000000000000 ) ;
#70881 = DIRECTION ( 'NONE',  ( 0.3543493200069162685, -0.000000000000000000, -0.9351131265310288487 ) ) ;
#70882 = DIRECTION ( 'NONE',  ( -1.000000000000000000, -0.000000000000000000, -0.000000000000000000 ) ) ;
#70883 = CARTESIAN_POINT ( 'NONE',  ( 12.19999999999999574, -25.83999999999998565, 2.999999999999999112 ) ) ;
#70884 = EDGE_CURVE ( 'NONE', #75249, #71697, #52193, .T. ) ;
#70885 = VERTEX_POINT ( 'NONE', #141343 ) ;
#70886 = ORIENTED_EDGE ( 'NONE', *, *, #77335, .T. ) ;
#70887 = CARTESIAN_POINT ( 'NONE',  ( 24.71757738642550351, -21.73023691814493219, 5.000000000000000888 ) ) ;
#70888 = EDGE_CURVE ( 'NONE', #90217, #101026, #119562, .T. ) ;
#70889 = ADVANCED_FACE ( 'NONE', ( #96378 ), #140620, .T. ) ;
#70890 = CARTESIAN_POINT ( 'NONE',  ( 11.15159235450332176, 9.902892378096218942E-16, 0.000000000000000000 ) ) ;
#70891 = CARTESIAN_POINT ( 'NONE',  ( 25.40000000000000568, -6.165261453458376728, -3.761236098458531796 ) ) ;
#70892 = AXIS2_PLACEMENT_3D ( 'NONE', #112572, #109713, #4450 ) ;
#70893 = FACE_OUTER_BOUND ( 'NONE', #92538, .T. ) ;
#70894 = LINE ( 'NONE', #92600, #67391 ) ;
#70895 = VECTOR ( 'NONE', #14682, 1000.000000000000000 ) ;
#70896 = ORIENTED_EDGE ( 'NONE', *, *, #10457, .T. ) ;
#70897 = ORIENTED_EDGE ( 'NONE', *, *, #101361, .F. ) ;
#70898 = EDGE_CURVE ( 'NONE', #30958, #42096, #107967, .T. ) ;
#70899 = VECTOR ( 'NONE', #68893, 1000.000000000000227 ) ;
#70900 = LINE ( 'NONE', #68073, #80406 ) ;
#70901 = VERTEX_POINT ( 'NONE', #64501 ) ;
#70902 = AXIS2_PLACEMENT_3D ( 'NONE', #55476, #137857, #82753 ) ;
#70903 = ADVANCED_FACE ( 'NONE', ( #72579 ), #69415, .T. ) ;
#70904 = CARTESIAN_POINT ( 'NONE',  ( 68.03752705046289861, -9.735942053221456900E-16, 7.949999999999998401 ) ) ;
#70905 = SURFACE_SIDE_STYLE ('',( #17211 ) ) ;
#70906 = EDGE_LOOP ( 'NONE', ( #61741, #1680, #26980, #25441, #52784, #114396, #101745 ) ) ;
#70907 = DIRECTION ( 'NONE',  ( -0.000000000000000000, 0.3543493200069153248, 0.9351131265310292928 ) ) ;
#70908 = DIRECTION ( 'NONE',  ( 0.7071067811865486830, -0.7071067811865464625, -0.000000000000000000 ) ) ;
#70909 = CARTESIAN_POINT ( 'NONE',  ( 34.92499999999998295, -7.199905483972748321, 4.759050581649326261 ) ) ;
#70910 = CARTESIAN_POINT ( 'NONE',  ( 0.000000000000000000, 0.000000000000000000, 9.500000000000001776 ) ) ;
#70911 = LINE ( 'NONE', #115062, #100057 ) ;
#70912 = VERTEX_POINT ( 'NONE', #61674 ) ;
#70913 = CARTESIAN_POINT ( 'NONE',  ( 0.000000000000000000, 0.000000000000000000, 5.000000000000000000 ) ) ;
#70914 = CARTESIAN_POINT ( 'NONE',  ( 5.878526836628497065, -20.24070752338406720, 7.412974875817778475 ) ) ;
#70915 = ORIENTED_EDGE ( 'NONE', *, *, #43594, .F. ) ;
#70916 = DIRECTION ( 'NONE',  ( -0.3543493200069163240, -0.000000000000000000, 0.9351131265310288487 ) ) ;
#70917 = VERTEX_POINT ( 'NONE', #105835 ) ;
#70918 = ORIENTED_EDGE ( 'NONE', *, *, #42033, .F. ) ;
#70919 = DIRECTION ( 'NONE',  ( 0.7071067811865486830, -0.7071067811865464625, -0.000000000000000000 ) ) ;
#70920 = ORIENTED_EDGE ( 'NONE', *, *, #25216, .T. ) ;
#70921 = ORIENTED_EDGE ( 'NONE', *, *, #100632, .F. ) ;
#70922 = CARTESIAN_POINT ( 'NONE',  ( 77.43793019189809002, -6.110000000000001208, 1.637169565754158951 ) ) ;
#70923 = ORIENTED_EDGE ( 'NONE', *, *, #27284, .T. ) ;
#70924 = EDGE_CURVE ( 'NONE', #4056, #109940, #6496, .T. ) ;
#70925 = FILL_AREA_STYLE_COLOUR ( '', #28035 ) ;
#70926 = ADVANCED_FACE ( 'NONE', ( #139236 ), #39932, .F. ) ;
#70927 = DIRECTION ( 'NONE',  ( 0.7071067811865487940, 0.7071067811865463515, 0.000000000000000000 ) ) ;
#70929 =( BOUNDED_CURVE ( )  B_SPLINE_CURVE ( 3, ( #17751, #96725, #117765, #62025 ),
 .UNSPECIFIED., .F., .T. ) 
 B_SPLINE_CURVE_WITH_KNOTS ( ( 4, 4 ),
 ( 2.228251278275058755, 2.286295730127291037 ),
 .UNSPECIFIED. ) 
 CURVE ( )  GEOMETRIC_REPRESENTATION_ITEM ( )  RATIONAL_B_SPLINE_CURVE ( ( 1.000000000000000000, 0.9997192565072046122, 0.9997192565072046122, 1.000000000000000000 ) ) 
 REPRESENTATION_ITEM ( '' )  );
#70928 = CARTESIAN_POINT ( 'NONE',  ( 107.1879301918980900, 6.110000000000002984, -1.637169565754156730 ) ) ;
#70930 = DIRECTION ( 'NONE',  ( 0.000000000000000000, -1.000000000000000000, 0.000000000000000000 ) ) ;
#70931 = CARTESIAN_POINT ( 'NONE',  ( 3.183988606268992161, 28.73617430169789699, 5.000000000000000000 ) ) ;
#70932 = CARTESIAN_POINT ( 'NONE',  ( 6.707106781186498168, -6.740707523384214639, 5.000000000000000000 ) ) ;
#70933 = CARTESIAN_POINT ( 'NONE',  ( -33.48921356237309510, -27.52281430457078670, 5.000000000000000000 ) ) ;
#70934 = PLANE ( 'NONE',  #80028 ) ;
#70935 = VECTOR ( 'NONE', #19988, 999.9999999999998863 ) ;
#70936 = CARTESIAN_POINT ( 'NONE',  ( 33.70710678118631165, 14.25929247661557042, 5.000000000000000000 ) ) ;
#70937 = SURFACE_SIDE_STYLE ('',( #15083 ) ) ;
#70938 = CARTESIAN_POINT ( 'NONE',  ( 34.45011844616451668, 4.516280811637454207, 5.000000000000000000 ) ) ;
#70939 = ORIENTED_EDGE ( 'NONE', *, *, #99006, .F. ) ;
#70940 = ORIENTED_EDGE ( 'NONE', *, *, #115269, .T. ) ;
#70941 = ORIENTED_EDGE ( 'NONE', *, *, #39503, .F. ) ;
#70942 = DIRECTION ( 'NONE',  ( 0.3543493200069162685, -0.000000000000000000, -0.9351131265310288487 ) ) ;
#70943 = VERTEX_POINT ( 'NONE', #106546 ) ;
#70944 = PLANE ( 'NONE',  #67702 ) ;
#70945 = PLANE ( 'NONE',  #84869 ) ;
#70946 = DIRECTION ( 'NONE',  ( 0.7071067811865487940, 0.7071067811865463515, 0.000000000000000000 ) ) ;
#70947 = LINE ( 'NONE', #125314, #23209 ) ;
#70948 = EDGE_LOOP ( 'NONE', ( #131354, #11846, #30831, #115579 ) ) ;
#70949 = PLANE ( 'NONE',  #115996 ) ;
#70950 = VERTEX_POINT ( 'NONE', #40624 ) ;
#70951 =( BOUNDED_CURVE ( )  B_SPLINE_CURVE ( 3, ( #111416, #136738, #112845, #102707 ),
 .UNSPECIFIED., .F., .F. ) 
 B_SPLINE_CURVE_WITH_KNOTS ( ( 4, 4 ),
 ( 1.864375635226930505, 1.933014472006549189 ),
 .UNSPECIFIED. ) 
 CURVE ( )  GEOMETRIC_REPRESENTATION_ITEM ( )  RATIONAL_B_SPLINE_CURVE ( ( 1.000000000000000000, 0.9996074310407763175, 0.9996074310407763175, 1.000000000000000000 ) ) 
 REPRESENTATION_ITEM ( '' )  );
#70952 = DIRECTION ( 'NONE',  ( 0.6830127018922180770, -0.6830127018922204085, -0.2588190451025213501 ) ) ;
#70953 = VECTOR ( 'NONE', #56320, 1000.000000000000000 ) ;
#70954 = CARTESIAN_POINT ( 'NONE',  ( 26.02540314143521982, 2.126176841940962348, 7.934999999999989839 ) ) ;
#70955 = DIRECTION ( 'NONE',  ( -0.7071067811865487940, 0.7071067811865463515, -0.000000000000000000 ) ) ;
#70956 = CARTESIAN_POINT ( 'NONE',  ( 31.49999999999977973, -5.568876922607759461, 4.000000000000000000 ) ) ;
#70957 = AXIS2_PLACEMENT_3D ( 'NONE', #31648, #65008, #130260 ) ;
#70958 = CARTESIAN_POINT ( 'NONE',  ( 14.67146529891954110, -9.486753853592309937, 0.5779121670573046377 ) ) ;
#70959 = ORIENTED_EDGE ( 'NONE', *, *, #93459, .T. ) ;
#70960 = ORIENTED_EDGE ( 'NONE', *, *, #97500, .T. ) ;
#70961 = VERTEX_POINT ( 'NONE', #10113 ) ;
#70962 = DIRECTION ( 'NONE',  ( -0.7071067811865486830, -0.7071067811865464625, 0.000000000000000000 ) ) ;
#70963 = CARTESIAN_POINT ( 'NONE',  ( -19.49999999999986500, 8.319652575858361487, -8.582050562765870083 ) ) ;
#70964 = DIRECTION ( 'NONE',  ( 0.6830127018922180770, -0.6830127018922204085, -0.2588190451025213501 ) ) ;
#70965 = DIRECTION ( 'NONE',  ( -1.000000000000000000, -1.224606353822377258E-16, -0.000000000000000000 ) ) ;
#70966 = EDGE_LOOP ( 'NONE', ( #34985, #126800, #78994, #125272 ) ) ;
#70967 = PLANE ( 'NONE',  #110976 ) ;
#70968 = LINE ( 'NONE', #105683, #110503 ) ;
#70969 = DIRECTION ( 'NONE',  ( 0.7071067811865487940, 0.7071067811865463515, -0.000000000000000000 ) ) ;
#70970 = CIRCLE ( 'NONE', #8402, 2.552699999999994418 ) ;
#70971 = CARTESIAN_POINT ( 'NONE',  ( 17.07999999999999829, -2.055000000000000160, 0.000000000000000000 ) ) ;
#70972 = CARTESIAN_POINT ( 'NONE',  ( 34.49999999999975842, -8.945670655168960650, 4.994342998332163219 ) ) ;
#70973 = VERTEX_POINT ( 'NONE', #76098 ) ;
#70974 = FACE_OUTER_BOUND ( 'NONE', #61861, .T. ) ;
#70975 = LINE ( 'NONE', #73813, #107231 ) ;
#70976 = VERTEX_POINT ( 'NONE', #121717 ) ;
#70977 = EDGE_CURVE ( 'NONE', #103327, #121984, #87681, .T. ) ;
#70978 = DIRECTION ( 'NONE',  ( -0.000000000000000000, 0.3543493200069153248, 0.9351131265310292928 ) ) ;
#70980 = ORIENTED_EDGE ( 'NONE', *, *, #72057, .F. ) ;
#70979 = SURFACE_STYLE_FILL_AREA ( #37638 ) ;
#70981 = CIRCLE ( 'NONE', #117290, 2.055000000000000604 ) ;
#70982 = EDGE_LOOP ( 'NONE', ( #67420, #141268, #121664, #52894 ) ) ;
#70983 = EDGE_CURVE ( 'NONE', #115520, #63418, #141297, .T. ) ;
#70984 = EDGE_CURVE ( 'NONE', #138636, #86181, #45637, .T. ) ;
#70985 = DIRECTION ( 'NONE',  ( -0.7071067811865487940, 0.7071067811865463515, -0.000000000000000000 ) ) ;
#70986 = DIRECTION ( 'NONE',  ( 0.7071067811865487940, 0.7071067811865463515, 0.000000000000000000 ) ) ;
#70987 = LINE ( 'NONE', #4203, #46066 ) ;
#70988 = VERTEX_POINT ( 'NONE', #110127 ) ;
#70989 = CARTESIAN_POINT ( 'NONE',  ( 0.000000000000000000, 0.000000000000000000, 5.000000000000000000 ) ) ;
#70990 = UNCERTAINTY_MEASURE_WITH_UNIT (LENGTH_MEASURE( 1.000000000000000082E-05 ), #98940, 'distance_accuracy_value', 'NONE');
#70991 = AXIS2_PLACEMENT_3D ( 'NONE', #43944, #31641, #96847 ) ;
#70993 = EDGE_CURVE ( 'NONE', #117128, #60304, #121017, .T. ) ;
#70992 = VECTOR ( 'NONE', #37341, 999.9999999999998863 ) ;
#70994 = ADVANCED_FACE ( 'NONE', ( #78981 ), #21713, .F. ) ;
#70995 = FACE_OUTER_BOUND ( 'NONE', #126455, .T. ) ;
#70996 = CARTESIAN_POINT ( 'NONE',  ( 15.29974487139158867, -27.71228299555216879, 4.000000000000000000 ) ) ;
#70998 = CARTESIAN_POINT ( 'NONE',  ( 28.49543019189811233, 5.291415217122917625, 3.055000000000002380 ) ) ;
#70997 = VECTOR ( 'NONE', #100562, 1000.000000000000000 ) ;
#70999 = PLANE ( 'NONE',  #106402 ) ;
#71000 = EDGE_CURVE ( 'NONE', #65622, #43439, #78253, .T. ) ;
#71001 = FACE_OUTER_BOUND ( 'NONE', #42815, .T. ) ;
#71002 = DIRECTION ( 'NONE',  ( 0.7071067811865486830, -0.7071067811865464625, -0.000000000000000000 ) ) ;
#71003 = FACE_OUTER_BOUND ( 'NONE', #114097, .T. ) ;
#71004 = CARTESIAN_POINT ( 'NONE',  ( 27.83290314143522437, -3.967499999999994476, 6.871911579029513106 ) ) ;
#71005 = CARTESIAN_POINT ( 'NONE',  ( 4.791236474768552966, -9.717572351234235426E-16, -7.934999999999990727 ) ) ;
#71006 = DIRECTION ( 'NONE',  ( -0.7071067811865486830, -0.7071067811865464625, 0.000000000000000000 ) ) ;
#71007 = AXIS2_PLACEMENT_3D ( 'NONE', #122308, #99870, #110709 ) ;
#71008 = DIRECTION ( 'NONE',  ( -0.7071067811865486830, -0.7071067811865464625, 0.000000000000000000 ) ) ;
#71009 = CARTESIAN_POINT ( 'NONE',  ( -34.42499999999997584, -21.76999999999999247, -0.5000000000000000000 ) ) ;
#71010 = EDGE_LOOP ( 'NONE', ( #121546, #3141, #8668, #70367, #15579 ) ) ;
#71011 = ORIENTED_EDGE ( 'NONE', *, *, #121223, .T. ) ;
#71013 = EDGE_CURVE ( 'NONE', #8528, #19998, #32608, .T. ) ;
#71012 = CARTESIAN_POINT ( 'NONE',  ( 89.81250000000000000, 5.819803920172571310, 5.819803920172575751 ) ) ;
#71014 = EDGE_LOOP ( 'NONE', ( #38138, #106331, #80689, #133823 ) ) ;
#71015 = ORIENTED_EDGE ( 'NONE', *, *, #58721, .F. ) ;
#71017 = EDGE_CURVE ( 'NONE', #36186, #127483, #12254, .T. ) ;
#71016 = CARTESIAN_POINT ( 'NONE',  ( 19.93618820137057668, -6.269999999999996021, -37.00000000000000000 ) ) ;
#71018 = LINE ( 'NONE', #83302, #13924 ) ;
#71019 = FACE_OUTER_BOUND ( 'NONE', #73814, .T. ) ;
#71020 = EDGE_LOOP ( 'NONE', ( #92490, #101557, #61652, #34703, #81423, #7720 ) ) ;
#71021 = EDGE_CURVE ( 'NONE', #134912, #142570, #65970, .T. ) ;
#71022 = DIRECTION ( 'NONE',  ( -0.7071067811865486830, -0.7071067811865464625, 0.000000000000000000 ) ) ;
#71023 = DIRECTION ( 'NONE',  ( 0.6830127018922181881, 0.6830127018922202975, -0.2588190451025214056 ) ) ;
#71024 = CARTESIAN_POINT ( 'NONE',  ( 3.489213562373097322, -27.52281430457057709, 5.000000000000000000 ) ) ;
#71025 = CARTESIAN_POINT ( 'NONE',  ( 126.2730375289500557, 6.754077994965395959, -2.478850524292684376 ) ) ;
#71026 = CARTESIAN_POINT ( 'NONE',  ( -12.00548008471251293, 28.92564299267929684, 4.000000000000000000 ) ) ;
#71027 = CARTESIAN_POINT ( 'NONE',  ( 12.29974487139158512, -27.71228299555214747, 4.000000000000000000 ) ) ;
#71028 = DIRECTION ( 'NONE',  ( -1.000000000000000000, 0.000000000000000000, -0.000000000000000000 ) ) ;
#71029 = EDGE_CURVE ( 'NONE', #131632, #67882, #120265, .T. ) ;
#71030 = CARTESIAN_POINT ( 'NONE',  ( 27.48921356237309155, -27.52281430457074762, 5.000000000000000000 ) ) ;
#71031 = CARTESIAN_POINT ( 'NONE',  ( -26.20710678118635428, -8.240707523384200428, 5.000000000000000000 ) ) ;
#71032 = CARTESIAN_POINT ( 'NONE',  ( 0.000000000000000000, -4.600000000000013856, 20.40202195861967382 ) ) ;
#71033 = CARTESIAN_POINT ( 'NONE',  ( -0.7928932188134476533, -8.240707523384200428, 5.000000000000000000 ) ) ;
#71034 = CARTESIAN_POINT ( 'NONE',  ( 52.83697049268917567, -48.90295371244932454, 39.18578444878559708 ) ) ;
#71035 = ORIENTED_EDGE ( 'NONE', *, *, #109752, .T. ) ;
#71036 = ORIENTED_EDGE ( 'NONE', *, *, #77234, .T. ) ;
#71037 = CARTESIAN_POINT ( 'NONE',  ( 113.7504301918981042, 3.055000000000002824, -5.291415217122919401 ) ) ;
#71038 = ORIENTED_EDGE ( 'NONE', *, *, #46335, .F. ) ;
#71039 = EDGE_CURVE ( 'NONE', #53276, #16457, #99239, .T. ) ;
#71040 = LINE ( 'NONE', #136264, #1536 ) ;
#71041 = VECTOR ( 'NONE', #71213, 1000.000000000000000 ) ;
#71042 = EDGE_LOOP ( 'NONE', ( #77908, #123256, #100817, #128719 ) ) ;
#71043 = CARTESIAN_POINT ( 'NONE',  ( -19.17183060077633172, -17.24070752338410273, 4.000000000000000000 ) ) ;
#71044 = LINE ( 'NONE', #7141, #60524 ) ;
#71045 = EDGE_CURVE ( 'NONE', #141546, #142614, #65247, .T. ) ;
#71046 = CARTESIAN_POINT ( 'NONE',  ( 100.5370968585647802, -3.054999999999998828, -5.291415217122919401 ) ) ;
#71047 = EDGE_LOOP ( 'NONE', ( #6086, #129785, #24878, #69316 ) ) ;
#71048 = EDGE_CURVE ( 'NONE', #64057, #120574, #143481, .T. ) ;
#71049 = ORIENTED_EDGE ( 'NONE', *, *, #119531, .F. ) ;
#71050 = LINE ( 'NONE', #63741, #10578 ) ;
#71051 = CIRCLE ( 'NONE', #131254, 2.500000000000000444 ) ;
#71052 = CARTESIAN_POINT ( 'NONE',  ( -34.42500000000001137, -21.02281430457035682, 5.000000000000000000 ) ) ;
#71053 = DIRECTION ( 'NONE',  ( 1.000000000000000000, 0.000000000000000000, 0.000000000000000000 ) ) ;
#71054 = ADVANCED_FACE ( 'NONE', ( #44202 ), #23101, .F. ) ;
#71055 = EDGE_LOOP ( 'NONE', ( #134754, #78731, #117952, #60918 ) ) ;
#71056 = EDGE_LOOP ( 'NONE', ( #993, #135038, #5180, #86442 ) ) ;
#71057 = VECTOR ( 'NONE', #131868, 1000.000000000000000 ) ;
#71058 = EDGE_LOOP ( 'NONE', ( #5012, #132653, #97119, #92106 ) ) ;
#71059 = LINE ( 'NONE', #95630, #532 ) ;
#71060 = CARTESIAN_POINT ( 'NONE',  ( 4.733736474768551972, 5.808823158059035485, 5.808823158059032821 ) ) ;
#71061 = DIRECTION ( 'NONE',  ( -1.000000000000000000, -1.224606353822377258E-16, -0.000000000000000000 ) ) ;
#71062 = AXIS2_PLACEMENT_3D ( 'NONE', #111739, #804, #89268 ) ;
#71063 =( NAMED_UNIT ( * ) PLANE_ANGLE_UNIT ( ) SI_UNIT ( $, .RADIAN. ) );
#71064 = CARTESIAN_POINT ( 'NONE',  ( -57.48921356237308800, -27.52281430457095368, 5.000000000000000000 ) ) ;
#71065 = ORIENTED_EDGE ( 'NONE', *, *, #71247, .T. ) ;
#71066 = VECTOR ( 'NONE', #131505, 1000.000000000000227 ) ;
#71067 = VERTEX_POINT ( 'NONE', #33349 ) ;
#71068 = EDGE_CURVE ( 'NONE', #36186, #72918, #11511, .T. ) ;
#71069 = LINE ( 'NONE', #7901, #34041 ) ;
#71070 = ORIENTED_EDGE ( 'NONE', *, *, #80668, .F. ) ;
#71071 = AXIS2_PLACEMENT_3D ( 'NONE', #85778, #66896, #10349 ) ;
#71072 = ORIENTED_EDGE ( 'NONE', *, *, #94822, .F. ) ;
#71073 = ADVANCED_FACE ( 'NONE', ( #100713 ), #99996, .F. ) ;
#71074 = DIRECTION ( 'NONE',  ( -0.7071067811865486830, 0.7071067811865464625, 0.000000000000000000 ) ) ;
#71075 = LINE ( 'NONE', #70390, #46703 ) ;
#71076 = VERTEX_POINT ( 'NONE', #133345 ) ;
#71077 = DIRECTION ( 'NONE',  ( -0.7071067811865486830, -0.7071067811865464625, 0.000000000000000000 ) ) ;
#71078 = CARTESIAN_POINT ( 'NONE',  ( 34.17183060077623225, 21.75929247661550292, 4.000000000000000000 ) ) ;
#71079 = CARTESIAN_POINT ( 'NONE',  ( 25.39999999999999858, -5.520864266206504263E-14, 0.000000000000000000 ) ) ;
#71080 = LINE ( 'NONE', #82659, #99691 ) ;
#71081 = EDGE_CURVE ( 'NONE', #45528, #119529, #67384, .T. ) ;
#71083 = FACE_BOUND ( 'NONE', #74374, .T. ) ;
#71082 = AXIS2_PLACEMENT_3D ( 'NONE', #61622, #141276, #39133 ) ;
#71084 = VERTEX_POINT ( 'NONE', #12954 ) ;
#71085 = PLANE ( 'NONE',  #129079 ) ;
#71086 = LINE ( 'NONE', #28282, #80505 ) ;
#71087 = CARTESIAN_POINT ( 'NONE',  ( -17.67183060077634593, -3.740707523384244837, 4.000000000000000000 ) ) ;
#71088 = EDGE_LOOP ( 'NONE', ( #48768, #5129, #124222, #92411 ) ) ;
#71089 = DIRECTION ( 'NONE',  ( 1.000000000000000000, -0.000000000000000000, -0.000000000000000000 ) ) ;
#71090 = ORIENTED_EDGE ( 'NONE', *, *, #59254, .F. ) ;
#71091 = ORIENTED_EDGE ( 'NONE', *, *, #135977, .T. ) ;
#71092 = AXIS2_PLACEMENT_3D ( 'NONE', #27168, #71411, #60562 ) ;
#71093 = VERTEX_POINT ( 'NONE', #47787 ) ;
#71094 = AXIS2_PLACEMENT_3D ( 'NONE', #121128, #132770, #34147 ) ;
#71095 = AXIS2_PLACEMENT_3D ( 'NONE', #43031, #133607, #34282 ) ;
#71096 = CARTESIAN_POINT ( 'NONE',  ( 39.43293019189811588, 1.637169565754156508, 6.110000000000000320 ) ) ;
#71097 = EDGE_LOOP ( 'NONE', ( #113650, #28644, #127996, #89495 ) ) ;
#71098 = CARTESIAN_POINT ( 'NONE',  ( -14.99999999999989164, -21.41253812416053748, 4.000000000000000000 ) ) ;
#71099 = DIRECTION ( 'NONE',  ( 0.7071067811865486830, -0.7071067811865464625, -0.000000000000000000 ) ) ;
#71100 = LINE ( 'NONE', #115242, #45094 ) ;
#71101 = AXIS2_PLACEMENT_3D ( 'NONE', #52104, #41220, #86172 ) ;
#71102 = ORIENTED_EDGE ( 'NONE', *, *, #90641, .F. ) ;
#71103 = FACE_OUTER_BOUND ( 'NONE', #46394, .T. ) ;
#71104 = CARTESIAN_POINT ( 'NONE',  ( 156.1499999999997783, -57.14999999999999147, 34.92500000000004690 ) ) ;
#71105 = AXIS2_PLACEMENT_3D ( 'NONE', #92214, #91533, #92947 ) ;
#71106 = EDGE_CURVE ( 'NONE', #74147, #69156, #55639, .T. ) ;
#71107 = CARTESIAN_POINT ( 'NONE',  ( 39.48921356237310221, -27.52281430457082934, 5.000000000000000000 ) ) ;
#71108 = EDGE_CURVE ( 'NONE', #95610, #63299, #38307, .T. ) ;
#71109 = CARTESIAN_POINT ( 'NONE',  ( 22.49999999999984723, 10.94296225409028089, -9.576120664313204855 ) ) ;
#71110 = CARTESIAN_POINT ( 'NONE',  ( -36.48921356237310221, -27.52281430457080802, 5.000000000000000000 ) ) ;
#71111 = CARTESIAN_POINT ( 'NONE',  ( 34.92499999999998295, 5.087954687542306509, -1.493867085284230400 ) ) ;
#71112 = ORIENTED_EDGE ( 'NONE', *, *, #605, .T. ) ;
#71113 = VERTEX_POINT ( 'NONE', #90552 ) ;
#71114 = ORIENTED_EDGE ( 'NONE', *, *, #86497, .T. ) ;
#71115 = ORIENTED_EDGE ( 'NONE', *, *, #86875, .F. ) ;
#71116 = CARTESIAN_POINT ( 'NONE',  ( 0.000000000000000000, 0.000000000000000000, 5.000000000000000000 ) ) ;
#71117 = VERTEX_POINT ( 'NONE', #80400 ) ;
#71118 = VERTEX_POINT ( 'NONE', #92660 ) ;
#71119 = DIRECTION ( 'NONE',  ( -0.000000000000000000, 0.3543493200069153248, 0.9351131265310292928 ) ) ;
#71120 = EDGE_CURVE ( 'NONE', #288, #112494, #36888, .T. ) ;
#71121 = DIRECTION ( 'NONE',  ( 0.7071067811865487940, -0.7071067811865463515, 0.000000000000000000 ) ) ;
#71122 = ORIENTED_EDGE ( 'NONE', *, *, #12234, .T. ) ;
#71123 = DIRECTION ( 'NONE',  ( -0.6830127018922180770, -0.6830127018922204085, -0.2588190451025213501 ) ) ;
#71124 = EDGE_LOOP ( 'NONE', ( #93921, #3679, #132291, #91979 ) ) ;
#71125 = LINE ( 'NONE', #15960, #35152 ) ;
#71126 = CARTESIAN_POINT ( 'NONE',  ( -10.49999999999993250, -12.08601207473291161, -10.46905243149092257 ) ) ;
#71127 = VECTOR ( 'NONE', #1015, 1000.000000000000000 ) ;
#71128 = ORIENTED_EDGE ( 'NONE', *, *, #7143, .F. ) ;
#71130 = DIRECTION ( 'NONE',  ( 0.7071067811865487940, 0.7071067811865463515, 0.000000000000000000 ) ) ;
#71129 = CARTESIAN_POINT ( 'NONE',  ( 98.34959685856479439, 6.109999999999997655, 1.637169565754163836 ) ) ;
#71131 = CARTESIAN_POINT ( 'NONE',  ( 52.60764783923754351, -49.05583548141699168, -39.86617647058817937 ) ) ;
#71132 = DIRECTION ( 'NONE',  ( 1.000000000000000000, 3.469446951953611428E-15, -9.465303761398244822E-16 ) ) ;
#71133 = ORIENTED_EDGE ( 'NONE', *, *, #133187, .T. ) ;
#71134 = EDGE_LOOP ( 'NONE', ( #104484, #136390, #37192, #130791 ) ) ;
#71135 = DIRECTION ( 'NONE',  ( 0.6830127018922180770, -0.6830127018922204085, -0.2588190451025213501 ) ) ;
#71136 = ORIENTED_EDGE ( 'NONE', *, *, #108740, .F. ) ;
#71137 =( LENGTH_UNIT ( ) NAMED_UNIT ( * ) SI_UNIT ( .MILLI., .METRE. ) );
#71138 = PLANE ( 'NONE',  #127412 ) ;
#71139 = CARTESIAN_POINT ( 'NONE',  ( 66.48921356237309510, -27.52281430457101763, 5.000000000000000000 ) ) ;
#71140 = LINE ( 'NONE', #124081, #2921 ) ;
#71141 = DIRECTION ( 'NONE',  ( -0.000000000000000000, 0.3543493200069153248, 0.9351131265310292928 ) ) ;
#71142 = VERTEX_POINT ( 'NONE', #68815 ) ;
#71143 = CARTESIAN_POINT ( 'NONE',  ( 34.42499999999998295, 22.22500000000000142, 5.000000000000000000 ) ) ;
#71144 = CARTESIAN_POINT ( 'NONE',  ( 34.92499999999998295, 21.72500000000000142, 5.000000000000000000 ) ) ;
#71145 = CARTESIAN_POINT ( 'NONE',  ( 36.48921356237310221, -27.52281430457080802, 5.000000000000000000 ) ) ;
#71146 = ADVANCED_FACE ( 'NONE', ( #81845 ), #134791, .F. ) ;
#71147 = PRESENTATION_LAYER_ASSIGNMENT (  '', '', ( #20183 ) ) ;
#71148 = EDGE_LOOP ( 'NONE', ( #132628, #6132, #12652, #131744 ) ) ;
#71149 = DIRECTION ( 'NONE',  ( 0.7071067811865487940, 0.7071067811865463515, 0.000000000000000000 ) ) ;
#71150 = LINE ( 'NONE', #15279, #65471 ) ;
#71151 = ORIENTED_EDGE ( 'NONE', *, *, #12893, .T. ) ;
#71153 = EDGE_LOOP ( 'NONE', ( #114639, #17005, #88504, #128675 ) ) ;
#71152 = CARTESIAN_POINT ( 'NONE',  ( -17.14994871458964809, -8.240707523384200428, 17.25253755692235558 ) ) ;
#71154 = EDGE_CURVE ( 'NONE', #97256, #104186, #115818, .T. ) ;
#71155 = EDGE_CURVE ( 'NONE', #51943, #19705, #70947, .T. ) ;
#71156 = VERTEX_POINT ( 'NONE', #60070 ) ;
#71157 = CARTESIAN_POINT ( 'NONE',  ( -1.089366964280113814, 13.74372519030773532, -24.36966481856508437 ) ) ;
#71158 = FACE_OUTER_BOUND ( 'NONE', #40052, .T. ) ;
#71159 = ORIENTED_EDGE ( 'NONE', *, *, #31470, .T. ) ;
#71160 = CARTESIAN_POINT ( 'NONE',  ( 48.18398860626899705, 28.73617430169820608, 5.000000000000000000 ) ) ;
#71161 = EDGE_CURVE ( 'NONE', #108305, #128690, #3494, .T. ) ;
#71162 = EDGE_CURVE ( 'NONE', #102314, #58699, #110696, .T. ) ;
#71163 = LINE ( 'NONE', #72619, #59009 ) ;
#71164 = CARTESIAN_POINT ( 'NONE',  ( -11.99451991528749417, 28.92564299267946382, 4.000000000000000000 ) ) ;
#71165 = EDGE_CURVE ( 'NONE', #47662, #14571, #69527, .T. ) ;
#71166 = AXIS2_PLACEMENT_3D ( 'NONE', #18992, #139386, #86411 ) ;
#71167 = VERTEX_POINT ( 'NONE', #93390 ) ;
#71168 = PLANE ( 'NONE',  #73991 ) ;
#71169 = DIRECTION ( 'NONE',  ( -0.7071067811865486830, 0.7071067811865464625, 0.000000000000000000 ) ) ;
#71170 = EDGE_CURVE ( 'NONE', #49544, #75615, #79721, .T. ) ;
#71171 = DIRECTION ( 'NONE',  ( -1.000000000000000000, 0.000000000000000000, 0.000000000000000000 ) ) ;
#71172 = CARTESIAN_POINT ( 'NONE',  ( -1.433128002487412678, -21.74070752338405654, 6.915939825044077338 ) ) ;
#71173 = DIRECTION ( 'NONE',  ( 0.3543493200069162685, -0.000000000000000000, -0.9351131265310288487 ) ) ;
#71174 = PLANE ( 'NONE',  #138676 ) ;
#71175 = EDGE_CURVE ( 'NONE', #124559, #17742, #2801, .T. ) ;
#71176 = CARTESIAN_POINT ( 'NONE',  ( -34.75611968250420603, 4.705650698524018516, 4.955485411084897152 ) ) ;
#71177 = VERTEX_POINT ( 'NONE', #70269 ) ;
#71178 = ORIENTED_EDGE ( 'NONE', *, *, #70278, .T. ) ;
#71179 = ORIENTED_EDGE ( 'NONE', *, *, #112399, .F. ) ;
#71181 = EDGE_CURVE ( 'NONE', #9860, #15339, #91283, .T. ) ;
#71180 = CARTESIAN_POINT ( 'NONE',  ( 122.4791666666666714, -7.950000000000001066, 2.130196079827424427 ) ) ;
#71182 = EDGE_LOOP ( 'NONE', ( #105379, #46401, #86526, #118960, #25619, #29182 ) ) ;
#71183 = VERTEX_POINT ( 'NONE', #82522 ) ;
#71184 = VERTEX_POINT ( 'NONE', #58687 ) ;
#71185 = LINE ( 'NONE', #73323, #53249 ) ;
#71186 = ORIENTED_EDGE ( 'NONE', *, *, #4994, .F. ) ;
#71187 = FACE_OUTER_BOUND ( 'NONE', #14680, .T. ) ;
#71188 = ADVANCED_FACE ( 'NONE', ( #126710 ), #123904, .F. ) ;
#71189 = PLANE ( 'NONE',  #25448 ) ;
#71190 = VECTOR ( 'NONE', #104916, 1000.000000000000227 ) ;
#71191 = CARTESIAN_POINT ( 'NONE',  ( -17.99999999999986500, 14.96639925780211122, 5.000000000000000000 ) ) ;
#71192 = CARTESIAN_POINT ( 'NONE',  ( 110.9795968585647756, 6.109999999999999432, 1.637169565754164280 ) ) ;
#71193 = EDGE_LOOP ( 'NONE', ( #126853, #67385, #31275, #138416, #10208 ) ) ;
#71194 = DIRECTION ( 'NONE',  ( 0.000000000000000000, -1.000000000000000000, 0.000000000000000000 ) ) ;
#71195 = CARTESIAN_POINT ( 'NONE',  ( 105.3708603837962272, 6.884901960086289741, -3.974999999999993427 ) ) ;
#71196 = CARTESIAN_POINT ( 'NONE',  ( 2.901564193917615331, 11.25929247661561305, 10.79108189686407471 ) ) ;
#71197 = CARTESIAN_POINT ( 'NONE',  ( 83.35002705046287019, -5.819803920172573086, -5.819803920172573086 ) ) ;
#71198 = DIRECTION ( 'NONE',  ( -0.3543493200069162685, -0.000000000000000000, -0.9351131265310288487 ) ) ;
#71199 = EDGE_CURVE ( 'NONE', #30921, #47131, #16523, .T. ) ;
#71200 = AXIS2_PLACEMENT_3D ( 'NONE', #73223, #95657, #139914 ) ;
#71201 = CARTESIAN_POINT ( 'NONE',  ( 17.20666063542140733, 21.75929247661550292, 4.998822639870701856 ) ) ;
#71202 =( LENGTH_UNIT ( ) NAMED_UNIT ( * ) SI_UNIT ( .MILLI., .METRE. ) );
#71203 = AXIS2_PLACEMENT_3D ( 'NONE', #46693, #79312, #122755 ) ;
#71204 = CARTESIAN_POINT ( 'NONE',  ( 36.53752705046288440, -9.735942053221456900E-16, 7.949999999999998401 ) ) ;
#71205 = CARTESIAN_POINT ( 'NONE',  ( -16.49999999999988276, -17.91344420646044000, 1.358650452708426659 ) ) ;
#71206 = DIRECTION ( 'NONE',  ( 0.000000000000000000, 5.075120898959323014E-15, 1.000000000000000000 ) ) ;
#71207 = ORIENTED_EDGE ( 'NONE', *, *, #91985, .T. ) ;
#71208 = ORIENTED_EDGE ( 'NONE', *, *, #111613, .F. ) ;
#71209 = CARTESIAN_POINT ( 'NONE',  ( 34.97916666666664298, -7.950000000000001066, 2.130196079827424427 ) ) ;
#71210 = ORIENTED_EDGE ( 'NONE', *, *, #26036, .F. ) ;
#71211 = ORIENTED_EDGE ( 'NONE', *, *, #40207, .T. ) ;
#71212 = LINE ( 'NONE', #16803, #78761 ) ;
#71213 = DIRECTION ( 'NONE',  ( 0.7071067811865486830, -0.7071067811865464625, -0.000000000000000000 ) ) ;
#71214 = ORIENTED_EDGE ( 'NONE', *, *, #127537, .T. ) ;
#71215 = DIRECTION ( 'NONE',  ( 0.7071067811865486830, -0.7071067811865464625, -0.000000000000000000 ) ) ;
#71216 = CARTESIAN_POINT ( 'NONE',  ( 2.510786437626908008, -27.52281430457053446, 5.000000000000000000 ) ) ;
#71217 = FACE_OUTER_BOUND ( 'NONE', #42243, .T. ) ;
#71218 = ADVANCED_FACE ( 'NONE', ( #114426 ), #15095, .T. ) ;
#71219 = CARTESIAN_POINT ( 'NONE',  ( 28.58376352523143993, -6.110000000000001208, -3.741295971395164515E-16 ) ) ;
#71220 = ORIENTED_EDGE ( 'NONE', *, *, #49382, .F. ) ;
#71221 = EDGE_CURVE ( 'NONE', #74158, #17485, #139049, .T. ) ;
#71222 = CARTESIAN_POINT ( 'NONE',  ( 33.18398860626899705, 28.73617430169810305, 5.000000000000000000 ) ) ;
#71223 = VERTEX_POINT ( 'NONE', #128866 ) ;
#71224 = FACE_OUTER_BOUND ( 'NONE', #100072, .T. ) ;
#71225 = CARTESIAN_POINT ( 'NONE',  ( -17.29298673570684386, -21.74070752338406720, 4.999753212805220670 ) ) ;
#71227 = ADVANCED_FACE ( 'NONE', ( #5637 ), #143143, .T. ) ;
#71226 =( BOUNDED_CURVE ( )  B_SPLINE_CURVE ( 3, ( #70744, #27919, #92433, #127217 ),
 .UNSPECIFIED., .F., .T. ) 
 B_SPLINE_CURVE_WITH_KNOTS ( ( 4, 4 ),
 ( 1.901594255663603183, 1.933014472006550966 ),
 .UNSPECIFIED. ) 
 CURVE ( )  GEOMETRIC_REPRESENTATION_ITEM ( )  RATIONAL_B_SPLINE_CURVE ( ( 1.000000000000000000, 0.9999177325257868620, 0.9999177325257868620, 1.000000000000000000 ) ) 
 REPRESENTATION_ITEM ( '' )  );
#71228 = CARTESIAN_POINT ( 'NONE',  ( -6.707106781186487510, -15.74070752338412760, 5.000000000000000000 ) ) ;
#71229 = ORIENTED_EDGE ( 'NONE', *, *, #134586, .F. ) ;
#71230 = ORIENTED_EDGE ( 'NONE', *, *, #115544, .F. ) ;
#71231 = FACE_OUTER_BOUND ( 'NONE', #78153, .T. ) ;
#71232 = DIRECTION ( 'NONE',  ( 0.3543493200069162685, -0.000000000000000000, -0.9351131265310288487 ) ) ;
#71233 = CARTESIAN_POINT ( 'NONE',  ( -20.48334561358941386, 22.22500000000000142, 4.500000000000000888 ) ) ;
#71234 = AXIS2_PLACEMENT_3D ( 'NONE', #55574, #97614, #141877 ) ;
#71235 = EDGE_CURVE ( 'NONE', #33799, #46517, #29000, .T. ) ;
#71236 = CIRCLE ( 'NONE', #131448, 2.500000000000000888 ) ;
#71237 = CARTESIAN_POINT ( 'NONE',  ( 52.99543019189811588, 5.291415217122916737, 3.055000000000001936 ) ) ;
#71238 = ORIENTED_EDGE ( 'NONE', *, *, #127197, .T. ) ;
#71239 = DIRECTION ( 'NONE',  ( -0.000000000000000000, 0.3543493200069153248, 0.9351131265310292928 ) ) ;
#71240 = EDGE_CURVE ( 'NONE', #126185, #25402, #54033, .T. ) ;
#71241 = CARTESIAN_POINT ( 'NONE',  ( 0.4000000000000001887, 0.000000000000000000, 0.000000000000000000 ) ) ;
#71242 = VERTEX_POINT ( 'NONE', #105666 ) ;
#71243 = ORIENTED_EDGE ( 'NONE', *, *, #63195, .F. ) ;
#71244 = CARTESIAN_POINT ( 'NONE',  ( 34.42499999999998295, -16.45860074219779889, 5.000000000000000000 ) ) ;
#71245 = ORIENTED_EDGE ( 'NONE', *, *, #43618, .F. ) ;
#71246 = CARTESIAN_POINT ( 'NONE',  ( -60.18398860626900415, 28.73617430169829490, 5.000000000000000000 ) ) ;
#71247 = EDGE_CURVE ( 'NONE', #119622, #118275, #17932, .T. ) ;
#71248 = ORIENTED_EDGE ( 'NONE', *, *, #98175, .T. ) ;
#71249 = CARTESIAN_POINT ( 'NONE',  ( -15.18398860626900237, 28.73617430169797871, 5.000000000000000000 ) ) ;
#71250 = DIRECTION ( 'NONE',  ( -0.7071067811865486830, -0.7071067811865464625, -0.000000000000000000 ) ) ;
#71251 = LINE ( 'NONE', #135779, #62821 ) ;
#71252 = EDGE_CURVE ( 'NONE', #110396, #140292, #10469, .T. ) ;
#71253 = FACE_BOUND ( 'NONE', #85009, .T. ) ;
#71254 = DIRECTION ( 'NONE',  ( -0.000000000000000000, -0.3543493200069152693, 0.9351131265310292928 ) ) ;
#71255 = CARTESIAN_POINT ( 'NONE',  ( 2.999999999999981792, 14.96639925780211122, 5.000000000000000000 ) ) ;
#71256 = EDGE_CURVE ( 'NONE', #81146, #79854, #65461, .T. ) ;
#71257 = VERTEX_POINT ( 'NONE', #6326 ) ;
#71258 = DIRECTION ( 'NONE',  ( 0.7071067811865487940, 0.7071067811865463515, 0.000000000000000000 ) ) ;
#71260 = ORIENTED_EDGE ( 'NONE', *, *, #87012, .T. ) ;
#71259 = CARTESIAN_POINT ( 'NONE',  ( -19.28515664589289003, 1.963325189347658428, -33.49048331797055766 ) ) ;
#71261 = LINE ( 'NONE', #125639, #4591 ) ;
#71262 = VERTEX_POINT ( 'NONE', #75764 ) ;
#71263 = EDGE_CURVE ( 'NONE', #6488, #136798, #119929, .T. ) ;
#71264 = EDGE_LOOP ( 'NONE', ( #14925, #32439, #56695, #128784, #129812, #60160 ) ) ;
#71265 = CARTESIAN_POINT ( 'NONE',  ( 65.53709685856478018, -3.054999999999998828, -5.291415217122919401 ) ) ;
#71266 = VERTEX_POINT ( 'NONE', #22061 ) ;
#71267 = VECTOR ( 'NONE', #28989, 999.9999999999998863 ) ;
#71268 = FACE_OUTER_BOUND ( 'NONE', #1249, .T. ) ;
#71269 = CARTESIAN_POINT ( 'NONE',  ( -34.42500000000001137, 20.97718569542920264, 5.000000000000000000 ) ) ;
#71270 = VERTEX_POINT ( 'NONE', #87348 ) ;
#71271 = CARTESIAN_POINT ( 'NONE',  ( 17.99999999999987566, 17.96639925780207747, 5.000000000000000000 ) ) ;
#71272 = EDGE_CURVE ( 'NONE', #118457, #72919, #94090, .T. ) ;
#71273 = VECTOR ( 'NONE', #28570, 1000.000000000000227 ) ;
#71274 = EDGE_CURVE ( 'NONE', #86982, #69962, #51329, .T. ) ;
#71275 = CARTESIAN_POINT ( 'NONE',  ( 14.29289321881336150, -12.74070752338415780, 5.000000000000000000 ) ) ;
#71276 = CARTESIAN_POINT ( 'NONE',  ( 101.0416666666666714, -3.975000000000002753, 6.884901960086286188 ) ) ;
#71277 = CARTESIAN_POINT ( 'NONE',  ( 18.18398860626898994, 28.73617430169800002, 5.000000000000000000 ) ) ;
#71278 = CARTESIAN_POINT ( 'NONE',  ( 17.20833333333333570, 3.047499999999997655, 5.278424836066143655 ) ) ;
#71279 = DIRECTION ( 'NONE',  ( 0.6830127018922180770, -0.6830127018922204085, -0.2588190451025213501 ) ) ;
#71280 = ORIENTED_EDGE ( 'NONE', *, *, #85187, .T. ) ;
#71281 = VERTEX_POINT ( 'NONE', #20634 ) ;
#71282 = PLANE ( 'NONE',  #12562 ) ;
#71284 = PLANE ( 'NONE',  #76761 ) ;
#71283 = VECTOR ( 'NONE', #1864, 999.9999999999998863 ) ;
#71285 = VERTEX_POINT ( 'NONE', #95518 ) ;
#71286 = VERTEX_POINT ( 'NONE', #88058 ) ;
#71288 = ORIENTED_EDGE ( 'NONE', *, *, #27824, .F. ) ;
#71287 = VECTOR ( 'NONE', #101722, 1000.000000000000000 ) ;
#71289 = CARTESIAN_POINT ( 'NONE',  ( 0.000000000000000000, 0.000000000000000000, 5.000000000000000000 ) ) ;
#71290 = EDGE_CURVE ( 'NONE', #66060, #58311, #131564, .T. ) ;
#71291 = FACE_OUTER_BOUND ( 'NONE', #81457, .T. ) ;
#71292 = ORIENTED_EDGE ( 'NONE', *, *, #123182, .F. ) ;
#71293 = LINE ( 'NONE', #103180, #18512 ) ;
#71294 = VECTOR ( 'NONE', #52850, 1000.000000000000000 ) ;
#71295 = AXIS2_PLACEMENT_3D ( 'NONE', #92253, #104578, #39345 ) ;
#71296 =( LENGTH_UNIT ( ) NAMED_UNIT ( * ) SI_UNIT ( .MILLI., .METRE. ) );
#71297 = CARTESIAN_POINT ( 'NONE',  ( 6.629569808101885897, -3.967499999999998028, -6.871911579029511330 ) ) ;
#71298 = LINE ( 'NONE', #48828, #98142 ) ;
#71299 = ORIENTED_EDGE ( 'NONE', *, *, #111397, .T. ) ;
#71300 = CARTESIAN_POINT ( 'NONE',  ( -14.99999999999988809, -10.06887692260770528, 4.000000000000000000 ) ) ;
#71301 = DIRECTION ( 'NONE',  ( -0.7071067811865487940, 0.7071067811865463515, 0.000000000000000000 ) ) ;
#71302 = PLANE ( 'NONE',  #105321 ) ;
#71304 = ORIENTED_EDGE ( 'NONE', *, *, #27339, .T. ) ;
#71303 = CARTESIAN_POINT ( 'NONE',  ( -34.17183060077623225, -20.24070752338407786, 4.000000000000000000 ) ) ;
#71305 = LINE ( 'NONE', #81480, #98052 ) ;
#71306 = EDGE_LOOP ( 'NONE', ( #114471, #19683, #108542, #26304 ) ) ;
#71307 = DIRECTION ( 'NONE',  ( 1.000000000000000000, 0.000000000000000000, 0.000000000000000000 ) ) ;
#71308 = CARTESIAN_POINT ( 'NONE',  ( 23.99999999999984013, 14.87792677143811026, -11.06722581663434646 ) ) ;
#71309 = CARTESIAN_POINT ( 'NONE',  ( 8.207106781186494615, 3.759292476615680112, 5.000000000000000000 ) ) ;
#71310 = ORIENTED_EDGE ( 'NONE', *, *, #98636, .F. ) ;
#71311 = FACE_OUTER_BOUND ( 'NONE', #35959, .T. ) ;
#71312 = CARTESIAN_POINT ( 'NONE',  ( -24.29974487139158867, -27.71228299555223273, 4.000000000000000000 ) ) ;
#71313 = CARTESIAN_POINT ( 'NONE',  ( -26.29289321881326913, 11.25929247661560240, 5.000000000000000000 ) ) ;
#71314 = EDGE_LOOP ( 'NONE', ( #106236, #137835, #14739, #111775 ) ) ;
#71315 = FACE_OUTER_BOUND ( 'NONE', #104514, .T. ) ;
#71316 = CARTESIAN_POINT ( 'NONE',  ( 1.499999999999987566, -10.04351517176478303, -1.623559851933819687 ) ) ;
#71317 = CARTESIAN_POINT ( 'NONE',  ( 21.46453280170069888, 2.055000000000001048, 2.516649172247811554E-16 ) ) ;
#71318 = DIRECTION ( 'NONE',  ( 0.7071067811865487940, -0.7071067811865463515, 0.000000000000000000 ) ) ;
#71319 = PRESENTATION_STYLE_ASSIGNMENT (( #27075 ) ) ;
#71320 = VERTEX_POINT ( 'NONE', #54729 ) ;
#71321 = ORIENTED_EDGE ( 'NONE', *, *, #110091, .F. ) ;
#71322 = VECTOR ( 'NONE', #95675, 1000.000000000000000 ) ;
#71323 = CARTESIAN_POINT ( 'NONE',  ( 9.994118527364397764, 4.584330080086930965E-16, 0.000000000000000000 ) ) ;
#71324 = CARTESIAN_POINT ( 'NONE',  ( 9.603736474768549414, 5.808823158059036373, 5.808823158059032821 ) ) ;
#71325 = DIRECTION ( 'NONE',  ( -0.000000000000000000, 0.3543493200069152138, -0.9351131265310292928 ) ) ;
#71326 = EDGE_CURVE ( 'NONE', #38058, #42501, #128182, .T. ) ;
#71327 = LINE ( 'NONE', #115484, #96980 ) ;
#71328 = LINE ( 'NONE', #16936, #78417 ) ;
#71329 = CARTESIAN_POINT ( 'NONE',  ( 25.97159235450331849, 9.902892378096218942E-16, 0.000000000000000000 ) ) ;
#71330 = EDGE_CURVE ( 'NONE', #79114, #89628, #32997, .T. ) ;
#71331 = EDGE_LOOP ( 'NONE', ( #96922, #4862, #129747, #141517 ) ) ;
#71332 = DIRECTION ( 'NONE',  ( -0.7071067811865486830, -0.7071067811865464625, -0.000000000000000000 ) ) ;
#71333 = ADVANCED_FACE ( 'NONE', ( #138329 ), #76487, .T. ) ;
#71334 = FACE_OUTER_BOUND ( 'NONE', #53426, .T. ) ;
#71335 = CARTESIAN_POINT ( 'NONE',  ( 11.25346039003969523, 4.202752102959690472E-16, 0.000000000000000000 ) ) ;
#71336 = EDGE_CURVE ( 'NONE', #107847, #125874, #116571, .T. ) ;
#71337 = CARTESIAN_POINT ( 'NONE',  ( 48.76626352523144448, 4.472830434245839371, -4.472830434245839371 ) ) ;
#71338 = DIRECTION ( 'NONE',  ( -0.6830127018922181881, 0.6830127018922202975, -0.2588190451025214056 ) ) ;
#71339 = PRESENTATION_LAYER_ASSIGNMENT (  '', '', ( #75983 ) ) ;
#71340 = ORIENTED_EDGE ( 'NONE', *, *, #87367, .F. ) ;
#71341 = DIRECTION ( 'NONE',  ( -1.000000000000000000, 0.000000000000000000, -0.000000000000000000 ) ) ;
#71342 = ORIENTED_EDGE ( 'NONE', *, *, #13209, .T. ) ;
#71343 = EDGE_CURVE ( 'NONE', #100429, #113476, #28143, .T. ) ;
#71344 = VERTEX_POINT ( 'NONE', #135843 ) ;
#71345 = CARTESIAN_POINT ( 'NONE',  ( 28.49999999999979750, 7.087461875839178305, 4.000000000000000000 ) ) ;
#71346 = CARTESIAN_POINT ( 'NONE',  ( -39.18398860626899705, 28.73617430169814568, 5.000000000000000000 ) ) ;
#71347 = DIRECTION ( 'NONE',  ( -0.000000000000000000, -0.3543493200069152693, 0.9351131265310292928 ) ) ;
#71348 = ADVANCED_FACE ( 'NONE', ( #101052 ), #35127, .F. ) ;
#71349 = DIRECTION ( 'NONE',  ( -0.000000000000000000, -0.3543493200069152693, 0.9351131265310292928 ) ) ;
#71350 = EDGE_CURVE ( 'NONE', #106603, #65916, #295, .T. ) ;
#71351 = DIRECTION ( 'NONE',  ( 0.3543493200069162685, -0.000000000000000000, -0.9351131265310288487 ) ) ;
#71352 = CARTESIAN_POINT ( 'NONE',  ( 11.08333333333333393, -5.278424836066144543, 3.047499999999995879 ) ) ;
#71353 = ORIENTED_EDGE ( 'NONE', *, *, #17062, .F. ) ;
#71354 = CARTESIAN_POINT ( 'NONE',  ( 3.872664058232598183, 3.821174125832445049E-16, 0.000000000000000000 ) ) ;
#71355 = DIRECTION ( 'NONE',  ( -0.7071067811865486830, -0.7071067811865464625, 0.000000000000000000 ) ) ;
#71356 = DIRECTION ( 'NONE',  ( -0.000000000000000000, -1.000000000000000000, -0.000000000000000000 ) ) ;
#71357 = DIRECTION ( 'NONE',  ( 0.7071067811865487940, 0.7071067811865463515, 0.000000000000000000 ) ) ;
#71358 = EDGE_CURVE ( 'NONE', #82218, #102711, #45299, .T. ) ;
#71359 = CARTESIAN_POINT ( 'NONE',  ( 116.9375000000000000, 5.819803920172574863, -5.819803920172573086 ) ) ;
#71360 = CARTESIAN_POINT ( 'NONE',  ( 63.66252705046289151, 7.949999999999998401, 1.460391307983218338E-15 ) ) ;
#71361 = LINE ( 'NONE', #127143, #29772 ) ;
#71362 = ORIENTED_EDGE ( 'NONE', *, *, #91690, .F. ) ;
#71363 = EDGE_LOOP ( 'NONE', ( #113774, #66771, #5402, #27427 ) ) ;
#71364 = AXIS2_PLACEMENT_3D ( 'NONE', #16121, #103848, #114042 ) ;
#71365 = CARTESIAN_POINT ( 'NONE',  ( 62.97916666666667140, -7.950000000000001066, 2.130196079827424427 ) ) ;
#71366 = DIRECTION ( 'NONE',  ( 0.000000000000000000, 0.000000000000000000, 1.000000000000000000 ) ) ;
#71367 = FACE_OUTER_BOUND ( 'NONE', #21872, .T. ) ;
#71368 = DIRECTION ( 'NONE',  ( -0.7071067811865486830, 0.7071067811865464625, 0.000000000000000000 ) ) ;
#71369 = ORIENTED_EDGE ( 'NONE', *, *, #80924, .F. ) ;
#71370 = CARTESIAN_POINT ( 'NONE',  ( 32.64583333333332860, 2.130196079827356037, -7.950000000000043698 ) ) ;
#71371 = DIRECTION ( 'NONE',  ( 0.7071067811865486830, -0.7071067811865464625, -0.000000000000000000 ) ) ;
#71372 = CARTESIAN_POINT ( 'NONE',  ( 60.66709685856477563, -3.055000000000000160, -5.291415217122921177 ) ) ;
#71373 = EDGE_CURVE ( 'NONE', #128811, #31148, #80764, .T. ) ;
#71374 = DIRECTION ( 'NONE',  ( 0.000000000000000000, 0.000000000000000000, 1.000000000000000000 ) ) ;
#71375 = ORIENTED_EDGE ( 'NONE', *, *, #93325, .T. ) ;
#71376 = ORIENTED_EDGE ( 'NONE', *, *, #59328, .F. ) ;
#71377 = CARTESIAN_POINT ( 'NONE',  ( 8.999999999999937828, -21.03360074219752462, 5.000000000000000000 ) ) ;
#71378 = FILL_AREA_STYLE_COLOUR ( '', #93935 ) ;
#71379 = DIRECTION ( 'NONE',  ( 0.000000000000000000, 1.000000000000000000, 0.000000000000000000 ) ) ;
#71380 = CIRCLE ( 'NONE', #6427, 8.094999999999991758 ) ;
#71381 = LINE ( 'NONE', #30743, #32487 ) ;
#71382 = DIRECTION ( 'NONE',  ( -0.000000000000000000, 0.3543493200069153248, 0.9351131265310292928 ) ) ;
#71384 = ORIENTED_EDGE ( 'NONE', *, *, #65477, .F. ) ;
#71383 = LINE ( 'NONE', #140207, #52198 ) ;
#71385 = CARTESIAN_POINT ( 'NONE',  ( -14.08979869950237074, -1.618973607074043475, -36.99999999997771738 ) ) ;
#71386 = CYLINDRICAL_SURFACE ( 'NONE', #66333, 2.500000000000000444 ) ;
#71387 = CARTESIAN_POINT ( 'NONE',  ( -24.51665438641027706, 22.22500000000000142, 4.500000000000000888 ) ) ;
#71388 = VECTOR ( 'NONE', #70916, 1000.000000000000227 ) ;
#71389 = DIRECTION ( 'NONE',  ( 0.7071067811865486830, -0.7071067811865464625, -0.000000000000000000 ) ) ;
#71391 = VECTOR ( 'NONE', #3049, 999.9999999999998863 ) ;
#71390 = VECTOR ( 'NONE', #53612, 1000.000000000000000 ) ;
#71392 = EDGE_CURVE ( 'NONE', #68809, #141475, #58337, .T. ) ;
#71393 = VERTEX_POINT ( 'NONE', #122089 ) ;
#71394 = VERTEX_POINT ( 'NONE', #23501 ) ;
#71395 = CARTESIAN_POINT ( 'NONE',  ( 0.000000000000000000, 0.000000000000000000, 5.000000000000000000 ) ) ;
#71396 = PLANE ( 'NONE',  #62676 ) ;
#71397 = DIRECTION ( 'NONE',  ( 0.000000000000000000, -1.000000000000000000, 0.000000000000000000 ) ) ;
#71398 = ADVANCED_FACE ( 'NONE', ( #112657 ), #79369, .F. ) ;
#71399 = LINE ( 'NONE', #61282, #54741 ) ;
#71400 = SURFACE_STYLE_FILL_AREA ( #27158 ) ;
#71401 = ORIENTED_EDGE ( 'NONE', *, *, #51275, .T. ) ;
#71402 = ORIENTED_EDGE ( 'NONE', *, *, #16097, .T. ) ;
#71403 = VECTOR ( 'NONE', #135689, 1000.000000000000000 ) ;
#71404 = CARTESIAN_POINT ( 'NONE',  ( 30.71230993966007361, -21.73547319004781286, 4.999917730833663754 ) ) ;
#71405 = DIRECTION ( 'NONE',  ( -1.000000000000000000, -0.000000000000000000, -0.000000000000000000 ) ) ;
#71406 = EDGE_LOOP ( 'NONE', ( #9936, #79494, #99155, #133640 ) ) ;
#71407 = VERTEX_POINT ( 'NONE', #3167 ) ;
#71408 = EDGE_CURVE ( 'NONE', #114577, #108642, #125576, .T. ) ;
#71409 = CARTESIAN_POINT ( 'NONE',  ( 0.000000000000000000, 0.000000000000000000, 5.000000000000000000 ) ) ;
#71410 = VERTEX_POINT ( 'NONE', #55433 ) ;
#71411 = DIRECTION ( 'NONE',  ( -0.000000000000000000, 0.000000000000000000, 1.000000000000000000 ) ) ;
#71412 = PLANE ( 'NONE',  #12319 ) ;
#71413 = VECTOR ( 'NONE', #61567, 1000.000000000000000 ) ;
#71414 = VECTOR ( 'NONE', #79383, 1000.000000000000000 ) ;
#71415 = VECTOR ( 'NONE', #89114, 1000.000000000000000 ) ;
#71416 = EDGE_CURVE ( 'NONE', #139679, #100881, #96151, .T. ) ;
#71417 = FACE_BOUND ( 'NONE', #92882, .T. ) ;
#71418 = LINE ( 'NONE', #115573, #142756 ) ;
#71419 = DIRECTION ( 'NONE',  ( -0.7071067811865486830, -0.7071067811865464625, -0.000000000000000000 ) ) ;
#71420 = CARTESIAN_POINT ( 'NONE',  ( 14.39532882439692862, 2.055000000000001048, 2.516649172247811554E-16 ) ) ;
#71421 = LINE ( 'NONE', #6815, #1777 ) ;
#71422 =( NAMED_UNIT ( * ) PLANE_ANGLE_UNIT ( ) SI_UNIT ( $, .RADIAN. ) );
#71423 = PRODUCT_CONTEXT ( 'NONE', #106872, 'mechanical' ) ;
#71424 = ORIENTED_EDGE ( 'NONE', *, *, #105476, .T. ) ;
#71425 = ORIENTED_EDGE ( 'NONE', *, *, #4681, .T. ) ;
#71426 = CARTESIAN_POINT ( 'NONE',  ( 96.30793019189810877, -6.109999999999998543, 1.637169565754158507 ) ) ;
#71427 = ORIENTED_EDGE ( 'NONE', *, *, #117774, .T. ) ;
#71428 = DIRECTION ( 'NONE',  ( 2.781805975412905274E-17, -0.3543493200069152138, 0.9351131265310292928 ) ) ;
#71429 = DIRECTION ( 'NONE',  ( -0.7071067811865487940, 0.7071067811865463515, 0.000000000000000000 ) ) ;
#71430 = AXIS2_PLACEMENT_3D ( 'NONE', #30434, #72560, #39908 ) ;
#71431 = VECTOR ( 'NONE', #139474, 1000.000000000000000 ) ;
#71432 = CARTESIAN_POINT ( 'NONE',  ( 55.24999999999999289, -9.735942053221458872E-16, 7.950000000000000178 ) ) ;
#71433 = ORIENTED_EDGE ( 'NONE', *, *, #131837, .F. ) ;
#71434 = CARTESIAN_POINT ( 'NONE',  ( 156.1499999999997783, -49.14999999999999147, 34.92500000000004690 ) ) ;
#71435 = EDGE_CURVE ( 'NONE', #49146, #74280, #7224, .T. ) ;
#71436 = DIRECTION ( 'NONE',  ( 0.7071067811865486830, -0.7071067811865464625, -0.000000000000000000 ) ) ;
#71437 = FACE_OUTER_BOUND ( 'NONE', #108944, .T. ) ;
#71438 = ADVANCED_FACE ( 'NONE', ( #15441 ), #50978, .F. ) ;
#71440 = DIRECTION ( 'NONE',  ( 0.7071067811865487940, 0.7071067811865463515, 0.000000000000000000 ) ) ;
#71439 = CARTESIAN_POINT ( 'NONE',  ( 5.510786437626906675, -27.52281430457051314, 5.000000000000000000 ) ) ;
#71441 = FACE_OUTER_BOUND ( 'NONE', #43383, .T. ) ;
#71442 = CARTESIAN_POINT ( 'NONE',  ( -13.49999999999990763, -8.568876922607724822, 4.000000000000000000 ) ) ;
#71443 = CARTESIAN_POINT ( 'NONE',  ( -34.75611968250421313, -9.187065745292532171, 4.955485411084894487 ) ) ;
#71444 = ORIENTED_EDGE ( 'NONE', *, *, #130980, .T. ) ;
#71445 = DIRECTION ( 'NONE',  ( 0.000000000000000000, -1.000000000000000000, 0.000000000000000000 ) ) ;
#71446 = FACE_OUTER_BOUND ( 'NONE', #43441, .T. ) ;
#71447 = VERTEX_POINT ( 'NONE', #60453 ) ;
#71448 = EDGE_CURVE ( 'NONE', #134235, #16391, #84346, .T. ) ;
#71449 = ORIENTED_EDGE ( 'NONE', *, *, #86580, .T. ) ;
#71450 = EDGE_CURVE ( 'NONE', #64832, #52944, #61189, .T. ) ;
#71451 = ORIENTED_EDGE ( 'NONE', *, *, #48426, .T. ) ;
#71452 = CARTESIAN_POINT ( 'NONE',  ( 46.22959685856476852, -6.110000000000000320, -1.637169565754161393 ) ) ;
#71453 = ORIENTED_EDGE ( 'NONE', *, *, #87413, .F. ) ;
#71454 = CARTESIAN_POINT ( 'NONE',  ( 17.10830628287044064, 1.633150327867687324, -6.094999999999991758 ) ) ;
#71455 = CARTESIAN_POINT ( 'NONE',  ( -9.853871626853138110, 9.550302695096817729, -29.19944056394587761 ) ) ;
#71456 = VERTEX_POINT ( 'NONE', #95175 ) ;
#71457 = DIRECTION ( 'NONE',  ( 0.6830127018922181881, 0.6830127018922202975, -0.2588190451025214056 ) ) ;
#71458 = EDGE_LOOP ( 'NONE', ( #10059, #26210, #45629, #19094, #78076 ) ) ;
#71459 = SURFACE_STYLE_USAGE ( .BOTH. , #91089 ) ;
#71460 = CARTESIAN_POINT ( 'NONE',  ( -63.29974487139158867, -27.71228299555250274, 4.000000000000000000 ) ) ;
#71462 = ORIENTED_EDGE ( 'NONE', *, *, #132635, .T. ) ;
#71461 = CARTESIAN_POINT ( 'NONE',  ( 15.48921356237309510, -27.52281430457066236, 5.000000000000000000 ) ) ;
#71463 = EDGE_LOOP ( 'NONE', ( #85940, #137103, #123232, #74188 ) ) ;
#71464 = EDGE_CURVE ( 'NONE', #115745, #118674, #40132, .T. ) ;
#71465 = CARTESIAN_POINT ( 'NONE',  ( 22.49999999999985079, -20.94781430457061333, 5.000000000000000000 ) ) ;
#71466 = CARTESIAN_POINT ( 'NONE',  ( 0.000000000000000000, 0.000000000000000000, 0.000000000000000000 ) ) ;
#71467 = VERTEX_POINT ( 'NONE', #137990 ) ;
#71468 = DIRECTION ( 'NONE',  ( 0.7071067811865487940, 0.7071067811865463515, -0.000000000000000000 ) ) ;
#71469 = ORIENTED_EDGE ( 'NONE', *, *, #8506, .F. ) ;
#71470 = ORIENTED_EDGE ( 'NONE', *, *, #108525, .T. ) ;
#71471 = EDGE_LOOP ( 'NONE', ( #119625, #61117, #99602, #55081 ) ) ;
#71472 = VERTEX_POINT ( 'NONE', #92310 ) ;
#71473 = LINE ( 'NONE', #126543, #49519 ) ;
#71474 = VECTOR ( 'NONE', #36133, 999.9999999999998863 ) ;
#71475 = VECTOR ( 'NONE', #25099, 1000.000000000000000 ) ;
#71476 = AXIS2_PLACEMENT_3D ( 'NONE', #129889, #110951, #20386 ) ;
#71477 = CARTESIAN_POINT ( 'NONE',  ( -27.18398860626900060, 28.73617430169806042, 5.000000000000000000 ) ) ;
#71478 = VECTOR ( 'NONE', #130975, 1000.000000000000000 ) ;
#71479 = CARTESIAN_POINT ( 'NONE',  ( 34.92499999999998295, -7.298069433178939747, 4.500000000000000888 ) ) ;
#71480 = CARTESIAN_POINT ( 'NONE',  ( -13.20450575203696886, 4.382956123802139281, 4.000000000000000000 ) ) ;
#71481 = CARTESIAN_POINT ( 'NONE',  ( -60.29974487139158867, -27.71228299555248142, 4.000000000000000000 ) ) ;
#71482 = ORIENTED_EDGE ( 'NONE', *, *, #111280, .T. ) ;
#71483 = VECTOR ( 'NONE', #85500, 1000.000000000000000 ) ;
#71484 = VECTOR ( 'NONE', #43680, 1000.000000000000000 ) ;
#71485 = CARTESIAN_POINT ( 'NONE',  ( 12.18398860626900060, 28.73617430169795739, 5.000000000000000000 ) ) ;
#71486 = CARTESIAN_POINT ( 'NONE',  ( 26.12840764549667583, 2.499999999999998224, 3.061616997868380183E-16 ) ) ;
#71487 = CARTESIAN_POINT ( 'NONE',  ( 18.29974487139159223, -27.71228299555219010, 4.000000000000000000 ) ) ;
#71488 = ADVANCED_FACE ( 'NONE', ( #136533 ), #5296, .F. ) ;
#71489 = CARTESIAN_POINT ( 'NONE',  ( 96.52083333333332860, 7.949999999999998401, 2.130196079827431532 ) ) ;
#71490 = CARTESIAN_POINT ( 'NONE',  ( -34.64589307847458599, 22.27000000000001023, -11.14749280822901767 ) ) ;
#71491 = ORIENTED_EDGE ( 'NONE', *, *, #122579, .F. ) ;
#71492 = EDGE_CURVE ( 'NONE', #45317, #40492, #37242, .T. ) ;
#71493 = ORIENTED_EDGE ( 'NONE', *, *, #110930, .T. ) ;
#71494 = ORIENTED_EDGE ( 'NONE', *, *, #65668, .F. ) ;
#71495 = PLANE ( 'NONE',  #88067 ) ;
#71496 = LINE ( 'NONE', #37443, #21051 ) ;
#71497 = DIRECTION ( 'NONE',  ( 0.6830127018922181881, 0.6830127018922202975, -0.2588190451025214056 ) ) ;
#71498 = AXIS2_PLACEMENT_3D ( 'NONE', #103568, #37644, #93433 ) ;
#71499 = CARTESIAN_POINT ( 'NONE',  ( -11.99999999999992006, 12.83542986846996214, -1.025386466790342066 ) ) ;
#71500 = CARTESIAN_POINT ( 'NONE',  ( -33.18398860626899705, 28.73617430169810305, 5.000000000000000000 ) ) ;
#71501 = ADVANCED_FACE ( 'NONE', ( #139447 ), #3845, .F. ) ;
#71503 = ADVANCED_FACE ( 'NONE', ( #115468 ), #14770, .F. ) ;
#71502 = CARTESIAN_POINT ( 'NONE',  ( 76.18293019189810877, -1.637169565754159173, -6.109999999999999432 ) ) ;
#71504 = CARTESIAN_POINT ( 'NONE',  ( 79.74999999999998579, -9.735942053221458872E-16, 7.950000000000000178 ) ) ;
#71506 = FACE_OUTER_BOUND ( 'NONE', #120349, .T. ) ;
#71505 = VECTOR ( 'NONE', #63540, 1000.000000000000227 ) ;
#71507 = FACE_OUTER_BOUND ( 'NONE', #143520, .T. ) ;
#71508 = LINE ( 'NONE', #69374, #78807 ) ;
#71509 = CARTESIAN_POINT ( 'NONE',  ( -3.792893218813431222, -8.240707523384200428, 5.000000000000000000 ) ) ;
#71510 = ORIENTED_EDGE ( 'NONE', *, *, #108159, .F. ) ;
#71511 = VECTOR ( 'NONE', #143541, 1000.000000000000000 ) ;
#71512 = LINE ( 'NONE', #18514, #114732 ) ;
#71513 = ORIENTED_EDGE ( 'NONE', *, *, #60900, .T. ) ;
#71514 = AXIS2_PLACEMENT_3D ( 'NONE', #119652, #20348, #97175 ) ;
#71515 = VECTOR ( 'NONE', #94819, 1000.000000000000000 ) ;
#71516 = AXIS2_PLACEMENT_3D ( 'NONE', #30296, #42633, #109283 ) ;
#71517 = DIRECTION ( 'NONE',  ( -0.6830127018922181881, 0.6830127018922202975, -0.2588190451025214056 ) ) ;
#71519 = ORIENTED_EDGE ( 'NONE', *, *, #20245, .T. ) ;
#71518 = DIRECTION ( 'NONE',  ( -0.6830127018922181881, 0.6830127018922202975, -0.2588190451025214056 ) ) ;
#71520 = EDGE_CURVE ( 'NONE', #75908, #13355, #105339, .T. ) ;
#71521 = EDGE_CURVE ( 'NONE', #73032, #137982, #26374, .T. ) ;
#71522 = DIRECTION ( 'NONE',  ( -0.7071067811865487940, 0.7071067811865463515, 0.000000000000000000 ) ) ;
#71523 = FACE_OUTER_BOUND ( 'NONE', #79804, .T. ) ;
#71524 = VERTEX_POINT ( 'NONE', #59047 ) ;
#71525 = DIRECTION ( 'NONE',  ( -0.7071067811865487940, 0.7071067811865463515, -0.000000000000000000 ) ) ;
#71526 = ORIENTED_EDGE ( 'NONE', *, *, #35692, .T. ) ;
#71527 = CARTESIAN_POINT ( 'NONE',  ( 121.8500270504628844, -5.819803920172573086, -5.819803920172573086 ) ) ;
#71528 = VERTEX_POINT ( 'NONE', #5994 ) ;
#71529 = AXIS2_PLACEMENT_3D ( 'NONE', #66014, #110877, #109485 ) ;
#71530 = VECTOR ( 'NONE', #7933, 1000.000000000000000 ) ;
#71531 = CARTESIAN_POINT ( 'NONE',  ( 14.99999999999989342, -21.84840872380823384, 2.849755605029642869 ) ) ;
#71532 = ADVANCED_FACE ( 'NONE', ( #37975 ), #65065, .T. ) ;
#71533 = CARTESIAN_POINT ( 'NONE',  ( 90.49586038379622721, -3.974999999999998312, -6.884901960086286188 ) ) ;
#71534 = CARTESIAN_POINT ( 'NONE',  ( 72.45833333333332860, 3.974999999999997424, 6.884901960086288852 ) ) ;
#71535 = FACE_OUTER_BOUND ( 'NONE', #116125, .T. ) ;
#71536 = ORIENTED_EDGE ( 'NONE', *, *, #48253, .F. ) ;
#71537 = FACE_OUTER_BOUND ( 'NONE', #17455, .T. ) ;
#71538 = DIRECTION ( 'NONE',  ( 0.6830127018922181881, 0.6830127018922202975, -0.2588190451025214056 ) ) ;
#71539 = CARTESIAN_POINT ( 'NONE',  ( 22.45833333333333215, -3.047499999999997211, -5.278424836066143655 ) ) ;
#71540 = DIRECTION ( 'NONE',  ( 0.7071067811865487940, -0.7071067811865463515, 0.000000000000000000 ) ) ;
#71541 = ADVANCED_FACE ( 'NONE', ( #82902, #127089 ), #17602, .T. ) ;
#71542 = CIRCLE ( 'NONE', #8959, 2.500000000000000888 ) ;
#71543 = LINE ( 'NONE', #41041, #79191 ) ;
#71544 = ORIENTED_EDGE ( 'NONE', *, *, #8418, .T. ) ;
#71545 = CARTESIAN_POINT ( 'NONE',  ( 22.45764329680116234, -1.725981765586488192, 4.380536896699297245 ) ) ;
#71546 = ORIENTED_EDGE ( 'NONE', *, *, #107482, .F. ) ;
#71547 = CARTESIAN_POINT ( 'NONE',  ( 80.20876352523143282, -7.482591942790329030E-16, 6.110000000000001208 ) ) ;
#71548 = DIRECTION ( 'NONE',  ( -0.000000000000000000, 0.000000000000000000, 1.000000000000000000 ) ) ;
#71549 = ADVANCED_FACE ( 'NONE', ( #127839 ), #72780, .F. ) ;
#71550 = LINE ( 'NONE', #114996, #56293 ) ;
#71551 = DIRECTION ( 'NONE',  ( 0.6830127018922181881, 0.6830127018922202975, -0.2588190451025214056 ) ) ;
#71552 = EDGE_LOOP ( 'NONE', ( #122186, #75039, #31823, #40239 ) ) ;
#71553 = CARTESIAN_POINT ( 'NONE',  ( 54.48921356237310221, -27.52281430457093236, 5.000000000000000000 ) ) ;
#71554 = CARTESIAN_POINT ( 'NONE',  ( -16.49999999999988276, -10.04351517176479192, -1.623559851933863873 ) ) ;
#71555 = CARTESIAN_POINT ( 'NONE',  ( -27.29974487139158512, -27.71228299555225405, 4.000000000000000000 ) ) ;
#71556 = CARTESIAN_POINT ( 'NONE',  ( -21.79289321881330466, -11.24070752338416312, 5.000000000000000000 ) ) ;
#71559 = EDGE_CURVE ( 'NONE', #87588, #88391, #97285, .T. ) ;
#71558 = ORIENTED_EDGE ( 'NONE', *, *, #71689, .F. ) ;
#71557 = CARTESIAN_POINT ( 'NONE',  ( -34.92500000000001137, -1.199905483972785181, 4.759050581649336031 ) ) ;
#71560 = LINE ( 'NONE', #140366, #103962 ) ;
#71561 = CARTESIAN_POINT ( 'NONE',  ( -19.99806943317887331, -22.22500000000000142, 4.500000000000000888 ) ) ;
#71562 = CARTESIAN_POINT ( 'NONE',  ( 1.470220343760034742, -1.488543484705065811, 6.466294286230377608 ) ) ;
#71563 = ORIENTED_EDGE ( 'NONE', *, *, #112816, .F. ) ;
#71564 = EDGE_CURVE ( 'NONE', #93164, #92088, #86469, .T. ) ;
#71565 = ORIENTED_EDGE ( 'NONE', *, *, #48619, .F. ) ;
#71566 = ORIENTED_EDGE ( 'NONE', *, *, #82466, .T. ) ;
#71567 = CARTESIAN_POINT ( 'NONE',  ( 73.64626352523141861, -4.472830434245840259, 4.472830434245839371 ) ) ;
#71568 = VERTEX_POINT ( 'NONE', #87164 ) ;
#71569 = DIRECTION ( 'NONE',  ( 0.000000000000000000, -1.000000000000000000, 0.000000000000000000 ) ) ;
#71570 = DIRECTION ( 'NONE',  ( 0.7071067811865487940, 0.7071067811865463515, 0.000000000000000000 ) ) ;
#71571 = CARTESIAN_POINT ( 'NONE',  ( -24.72281430457042717, -21.72500000000000142, 5.000000000000000000 ) ) ;
#71572 = DIRECTION ( 'NONE',  ( -1.000000000000000000, -1.224606353822377258E-16, -0.000000000000000000 ) ) ;
#71573 = VERTEX_POINT ( 'NONE', #119760 ) ;
#71574 = CARTESIAN_POINT ( 'NONE',  ( 5.999999999999963585, 1.761378380278687983, -6.096875308897241830 ) ) ;
#71575 = CARTESIAN_POINT ( 'NONE',  ( 39.48921356237310221, -27.52281430457082934, 5.000000000000000000 ) ) ;
#71576 = EDGE_LOOP ( 'NONE', ( #77514, #95367, #110543, #69878 ) ) ;
#71577 = CARTESIAN_POINT ( 'NONE',  ( 1.320799999999990870, 1.617513596018363294E-16, 3.775643966265890494 ) ) ;
#71578 = PLANE ( 'NONE',  #29348 ) ;
#71579 = CARTESIAN_POINT ( 'NONE',  ( -34.92500000000001137, -14.33753812416085971, 4.000000000000000000 ) ) ;
#71580 = AXIS2_PLACEMENT_3D ( 'NONE', #44550, #15233, #92816 ) ;
#71581 = AXIS2_PLACEMENT_3D ( 'NONE', #104645, #116244, #105354 ) ;
#71582 = VECTOR ( 'NONE', #2521, 1000.000000000000227 ) ;
#71583 = VERTEX_POINT ( 'NONE', #30664 ) ;
#71584 = VERTEX_POINT ( 'NONE', #21190 ) ;
#71585 = MECHANICAL_DESIGN_GEOMETRIC_PRESENTATION_REPRESENTATION (  '', ( #103822 ), #36797 ) ;
#71586 = DIRECTION ( 'NONE',  ( 0.3543493200069163240, -0.000000000000000000, -0.9351131265310288487 ) ) ;
#71587 = EDGE_CURVE ( 'NONE', #75086, #2249, #10301, .T. ) ;
#71588 = DIRECTION ( 'NONE',  ( -0.7071067811865486830, -0.7071067811865464625, 0.000000000000000000 ) ) ;
#71589 = PLANE ( 'NONE',  #39298 ) ;
#71590 = CARTESIAN_POINT ( 'NONE',  ( -18.28838880452753202, -2.745211937670052560, 5.000000000000000000 ) ) ;
#71591 = LINE ( 'NONE', #115753, #104570 ) ;
#71592 = PRESENTATION_LAYER_ASSIGNMENT (  '', '', ( #134096 ) ) ;
#71593 = LINE ( 'NONE', #51982, #71190 ) ;
#71594 = DIRECTION ( 'NONE',  ( -0.7071067811865487940, 0.7071067811865463515, 0.000000000000000000 ) ) ;
#71595 =( NAMED_UNIT ( * ) PLANE_ANGLE_UNIT ( ) SI_UNIT ( $, .RADIAN. ) );
#71596 = EDGE_LOOP ( 'NONE', ( #21014, #112264, #133219, #42426 ) ) ;
#71597 = ORIENTED_EDGE ( 'NONE', *, *, #60095, .T. ) ;
#71598 = ORIENTED_EDGE ( 'NONE', *, *, #116488, .T. ) ;
#71599 = ORIENTED_EDGE ( 'NONE', *, *, #80379, .F. ) ;
#71600 = VECTOR ( 'NONE', #62971, 1000.000000000000000 ) ;
#71601 =( BOUNDED_CURVE ( )  B_SPLINE_CURVE ( 3, ( #109178, #129491, #17857, #30185 ),
 .UNSPECIFIED., .F., .F. ) 
 B_SPLINE_CURVE_WITH_KNOTS ( ( 4, 4 ),
 ( 5.772031613926481342, 5.830584196225662375 ),
 .UNSPECIFIED. ) 
 CURVE ( )  GEOMETRIC_REPRESENTATION_ITEM ( )  RATIONAL_B_SPLINE_CURVE ( ( 1.000000000000000000, 0.9997143199977724937, 0.9997143199977724937, 1.000000000000000000 ) ) 
 REPRESENTATION_ITEM ( '' )  );
#71602 = CARTESIAN_POINT ( 'NONE',  ( 51.18398860626899705, 28.73617430169823095, 5.000000000000000000 ) ) ;
#71603 = VECTOR ( 'NONE', #28401, 1000.000000000000227 ) ;
#71604 = ORIENTED_EDGE ( 'NONE', *, *, #22168, .T. ) ;
#71605 = CARTESIAN_POINT ( 'NONE',  ( -34.92500000000001137, 13.70115479773740752, 1.769996414796630058 ) ) ;
#71606 = DIRECTION ( 'NONE',  ( 0.6830127018922180770, -0.6830127018922204085, -0.2588190451025213501 ) ) ;
#71607 = LINE ( 'NONE', #27352, #59568 ) ;
#71608 = CARTESIAN_POINT ( 'NONE',  ( -63.18398860626900415, 28.73617430169831621, 5.000000000000000000 ) ) ;
#71609 = AXIS2_PLACEMENT_3D ( 'NONE', #112040, #78686, #122904 ) ;
#71610 = LINE ( 'NONE', #94053, #118554 ) ;
#71611 = VERTEX_POINT ( 'NONE', #62573 ) ;
#71612 = VECTOR ( 'NONE', #11200, 999.9999999999998863 ) ;
#71613 = CARTESIAN_POINT ( 'NONE',  ( 0.000000000000000000, 0.000000000000000000, 7.950000000000000178 ) ) ;
#71614 = CARTESIAN_POINT ( 'NONE',  ( -15.70710678118643422, -18.74070752338409562, 5.000000000000000000 ) ) ;
#71615 = VECTOR ( 'NONE', #18893, 1000.000000000000227 ) ;
#71616 = ORIENTED_EDGE ( 'NONE', *, *, #45790, .T. ) ;
#71617 = EDGE_CURVE ( 'NONE', #80430, #121119, #99699, .T. ) ;
#71618 = CARTESIAN_POINT ( 'NONE',  ( 0.4892135623730947680, -27.52281430457055578, 5.000000000000000000 ) ) ;
#71619 = ORIENTED_EDGE ( 'NONE', *, *, #131282, .F. ) ;
#71620 = ORIENTED_EDGE ( 'NONE', *, *, #37649, .T. ) ;
#71622 = EDGE_CURVE ( 'NONE', #12905, #73407, #55744, .T. ) ;
#71621 = CARTESIAN_POINT ( 'NONE',  ( 12.44163961620377101, -6.094999999999989093, 1.633150327867691542 ) ) ;
#71623 = ORIENTED_EDGE ( 'NONE', *, *, #118284, .F. ) ;
#71624 = ORIENTED_EDGE ( 'NONE', *, *, #8560, .F. ) ;
#71626 = VECTOR ( 'NONE', #121445, 1000.000000000000227 ) ;
#71625 = CARTESIAN_POINT ( 'NONE',  ( 73.35459685856476142, -1.637169565754161615, 6.110000000000000320 ) ) ;
#71627 = ORIENTED_EDGE ( 'NONE', *, *, #40117, .F. ) ;
#71628 = VECTOR ( 'NONE', #38835, 999.9999999999998863 ) ;
#71629 = SURFACE_STYLE_USAGE ( .BOTH. , #27370 ) ;
#71630 = DIRECTION ( 'NONE',  ( 0.7071067811865487940, -0.7071067811865463515, 0.000000000000000000 ) ) ;
#71631 = CARTESIAN_POINT ( 'NONE',  ( 107.0420968585647756, 5.291415217122923842, -3.054999999999996163 ) ) ;
#71632 = LINE ( 'NONE', #136872, #132829 ) ;
#71633 = ADVANCED_FACE ( 'NONE', ( #53087 ), #118350, .T. ) ;
#71634 = FACE_OUTER_BOUND ( 'NONE', #2413, .T. ) ;
#71635 = PLANE ( 'NONE',  #39780 ) ;
#71636 = SURFACE_SIDE_STYLE ('',( #55956 ) ) ;
#71637 = VECTOR ( 'NONE', #34959, 1000.000000000000000 ) ;
#71638 = FACE_OUTER_BOUND ( 'NONE', #3840, .T. ) ;
#71639 = CARTESIAN_POINT ( 'NONE',  ( -39.48921356237310221, -27.52281430457082934, 5.000000000000000000 ) ) ;
#71640 = EDGE_CURVE ( 'NONE', #116493, #95953, #20457, .T. ) ;
#71641 = CARTESIAN_POINT ( 'NONE',  ( -4.499999999999968914, -1.592773361805379428, -6.492772025301219330 ) ) ;
#71642 = FACE_OUTER_BOUND ( 'NONE', #141409, .T. ) ;
#71643 = ORIENTED_EDGE ( 'NONE', *, *, #111996, .T. ) ;
#71644 = PLANE ( 'NONE',  #138654 ) ;
#71645 = DIRECTION ( 'NONE',  ( -0.000000000000000000, 0.3543493200069153248, 0.9351131265310292928 ) ) ;
#71646 = ORIENTED_EDGE ( 'NONE', *, *, #87129, .F. ) ;
#71647 = VERTEX_POINT ( 'NONE', #43659 ) ;
#71648 = FACE_OUTER_BOUND ( 'NONE', #93628, .T. ) ;
#71649 = EDGE_CURVE ( 'NONE', #98924, #95164, #54561, .T. ) ;
#71650 = ORIENTED_EDGE ( 'NONE', *, *, #49564, .T. ) ;
#71651 = CARTESIAN_POINT ( 'NONE',  ( -20.51078643762690490, -27.52281430457041012, 5.000000000000000000 ) ) ;
#71652 = DIRECTION ( 'NONE',  ( -1.000000000000000000, -1.224606353822377258E-16, -0.000000000000000000 ) ) ;
#71653 = DIRECTION ( 'NONE',  ( -0.000000000000000000, 0.000000000000000000, 1.000000000000000000 ) ) ;
#71654 = CARTESIAN_POINT ( 'NONE',  ( -15.19713381108422290, 7.733989266307781385, 4.000000000000000000 ) ) ;
#71655 = ORIENTED_EDGE ( 'NONE', *, *, #43820, .F. ) ;
#71656 = DIRECTION ( 'NONE',  ( -0.7071067811865487940, 0.7071067811865463515, -0.000000000000000000 ) ) ;
#71657 = ORIENTED_EDGE ( 'NONE', *, *, #121954, .T. ) ;
#71658 = CARTESIAN_POINT ( 'NONE',  ( 31.12956980810189478, -3.967499999999998028, -6.871911579029511330 ) ) ;
#71659 = CARTESIAN_POINT ( 'NONE',  ( -11.47599861414542133, 22.03583458319438293, 4.979811245910087614 ) ) ;
#71660 = LINE ( 'NONE', #61526, #129297 ) ;
#71661 = FACE_OUTER_BOUND ( 'NONE', #127213, .T. ) ;
#71662 = ORIENTED_EDGE ( 'NONE', *, *, #113926, .F. ) ;
#71663 = ADVANCED_FACE ( 'NONE', ( #131392 ), #107484, .F. ) ;
#71664 = ORIENTED_EDGE ( 'NONE', *, *, #65826, .F. ) ;
#71665 = ORIENTED_EDGE ( 'NONE', *, *, #309, .T. ) ;
#71666 = CARTESIAN_POINT ( 'NONE',  ( 1.566871997512565562, -21.74070752338405654, 6.915939825044070233 ) ) ;
#71667 = CARTESIAN_POINT ( 'NONE',  ( 3.183988606268992161, 28.73617430169789699, 5.000000000000000000 ) ) ;
#71668 = LINE ( 'NONE', #28159, #26485 ) ;
#71669 = DIRECTION ( 'NONE',  ( -0.000000000000000000, 0.000000000000000000, 1.000000000000000000 ) ) ;
#71670 = CARTESIAN_POINT ( 'NONE',  ( -6.475126127850423963, 14.25929247661557220, 9.797011795316622695 ) ) ;
#71671 = EDGE_CURVE ( 'NONE', #75064, #100892, #95895, .T. ) ;
#71672 = EDGE_CURVE ( 'NONE', #31910, #27663, #117614, .T. ) ;
#71673 = CARTESIAN_POINT ( 'NONE',  ( 36.48921356237310221, -27.52281430457080802, 5.000000000000000000 ) ) ;
#71674 = PLANE ( 'NONE',  #67164 ) ;
#71675 = LINE ( 'NONE', #80426, #127660 ) ;
#71676 = CARTESIAN_POINT ( 'NONE',  ( 26.99999999999981526, 8.966399257802175171, 5.000000000000000000 ) ) ;
#71677 = EDGE_LOOP ( 'NONE', ( #29978, #104959, #82644, #20092, #104963 ) ) ;
#71678 = CARTESIAN_POINT ( 'NONE',  ( -3.183988606268992161, 28.73617430169789699, 5.000000000000000000 ) ) ;
#71679 = VECTOR ( 'NONE', #108858, 1000.000000000000000 ) ;
#71680 = AXIS2_PLACEMENT_3D ( 'NONE', #95362, #6888, #39586 ) ;
#71681 = VECTOR ( 'NONE', #47380, 1000.000000000000000 ) ;
#71683 = ADVANCED_FACE ( 'NONE', ( #51701 ), #29207, .F. ) ;
#71682 = LINE ( 'NONE', #7816, #118823 ) ;
#71684 = ORIENTED_EDGE ( 'NONE', *, *, #3659, .T. ) ;
#71685 = AXIS2_PLACEMENT_3D ( 'NONE', #92437, #116364, #106164 ) ;
#71686 = CARTESIAN_POINT ( 'NONE',  ( 18.61838490601984830, -2.240707523384257716, 13.37739548510235110 ) ) ;
#71688 = EDGE_LOOP ( 'NONE', ( #125035, #90623, #130622, #126129 ) ) ;
#71687 = CARTESIAN_POINT ( 'NONE',  ( 9.489213562373095101, -27.52281430457062328, 5.000000000000000000 ) ) ;
#71690 = VERTEX_POINT ( 'NONE', #41507 ) ;
#71689 = EDGE_CURVE ( 'NONE', #123220, #117459, #142966, .T. ) ;
#71691 = EDGE_CURVE ( 'NONE', #20060, #55296, #73450, .T. ) ;
#71692 = CARTESIAN_POINT ( 'NONE',  ( 30.29974487139158867, -27.71228299555227537, 4.000000000000000000 ) ) ;
#71693 = FACE_OUTER_BOUND ( 'NONE', #113364, .T. ) ;
#71694 = VERTEX_POINT ( 'NONE', #74895 ) ;
#71695 = DIRECTION ( 'NONE',  ( -1.000000000000000000, -0.000000000000000000, -0.000000000000000000 ) ) ;
#71696 = VECTOR ( 'NONE', #59419, 1000.000000000000000 ) ;
#71697 = VERTEX_POINT ( 'NONE', #140140 ) ;
#71698 = CARTESIAN_POINT ( 'NONE',  ( 69.18398860626899705, 28.73617430169835529, 5.000000000000000000 ) ) ;
#71699 = CARTESIAN_POINT ( 'NONE',  ( 106.0000000000000000, 0.000000000000000000, -7.950000000000000178 ) ) ;
#71700 = CARTESIAN_POINT ( 'NONE',  ( 126.0791937171295558, 3.975000000000002753, -6.884901960086283523 ) ) ;
#71701 = ADVANCED_FACE ( 'NONE', ( #85017 ), #129225, .F. ) ;
#71702 = DIRECTION ( 'NONE',  ( -0.7071067811865486830, 0.7071067811865464625, 0.000000000000000000 ) ) ;
#71703 = ADVANCED_FACE ( 'NONE', ( #119068 ), #79911, .T. ) ;
#71704 = CARTESIAN_POINT ( 'NONE',  ( 83.78752705046288440, 0.000000000000000000, -7.949999999999998401 ) ) ;
#71705 = CARTESIAN_POINT ( 'NONE',  ( 21.44840764549667611, 9.139736423841732040E-16, 0.000000000000000000 ) ) ;
#71706 = CARTESIAN_POINT ( 'NONE',  ( -35.99451991528749772, 28.92564299267963079, 4.000000000000000000 ) ) ;
#71707 = LINE ( 'NONE', #93447, #106140 ) ;
#71708 = CARTESIAN_POINT ( 'NONE',  ( 34.39540314143521016, 2.126176841940962348, 7.934999999999989839 ) ) ;
#71710 = VECTOR ( 'NONE', #85589, 1000.000000000000000 ) ;
#71709 = CARTESIAN_POINT ( 'NONE',  ( 3.770403141435219485, -7.934999999999988951, 2.126176841940957907 ) ) ;
#71711 = DIRECTION ( 'NONE',  ( 0.7071067811865487940, 0.7071067811865463515, -0.000000000000000000 ) ) ;
#71712 = AXIS2_PLACEMENT_3D ( 'NONE', #122573, #13087, #57362 ) ;
#71713 = EDGE_CURVE ( 'NONE', #44351, #93058, #77734, .T. ) ;
#71714 = CARTESIAN_POINT ( 'NONE',  ( 60.18398860626900415, 28.73617430169829490, 5.000000000000000000 ) ) ;
#71715 = DIRECTION ( 'NONE',  ( -1.000000000000000000, -0.000000000000000000, -0.000000000000000000 ) ) ;
#71716 = ORIENTED_EDGE ( 'NONE', *, *, #41785, .F. ) ;
#71717 = EDGE_LOOP ( 'NONE', ( #40934, #29888, #74840, #73421, #7734 ) ) ;
#71718 = CARTESIAN_POINT ( 'NONE',  ( 86.16666666666667140, 6.884901960086285300, 3.975000000000003642 ) ) ;
#71719 = AXIS2_PLACEMENT_3D ( 'NONE', #33251, #50862, #22287 ) ;
#71721 = VERTEX_POINT ( 'NONE', #124084 ) ;
#71720 = CARTESIAN_POINT ( 'NONE',  ( 25.39999999999998792, 6.130634315452725858, 3.678650144044258941 ) ) ;
#71722 = ORIENTED_EDGE ( 'NONE', *, *, #5900, .F. ) ;
#71723 = FACE_OUTER_BOUND ( 'NONE', #86475, .T. ) ;
#71724 = CARTESIAN_POINT ( 'NONE',  ( 22.79580628287044064, -5.278424836066144543, 3.047499999999995879 ) ) ;
#71725 = EDGE_CURVE ( 'NONE', #22559, #50033, #133536, .T. ) ;
#71726 = CARTESIAN_POINT ( 'NONE',  ( -8.999999999999944933, 11.58746187583914100, 4.000000000000000000 ) ) ;
#71727 = VERTEX_POINT ( 'NONE', #13856 ) ;
#71728 = VECTOR ( 'NONE', #32903, 999.9999999999998863 ) ;
#71729 = DIRECTION ( 'NONE',  ( -0.7071067811865486830, -0.7071067811865464625, 0.000000000000000000 ) ) ;
#71730 = VECTOR ( 'NONE', #45170, 999.9999999999998863 ) ;
#71731 = LINE ( 'NONE', #17320, #85791 ) ;
#71732 = VECTOR ( 'NONE', #65119, 1000.000000000000000 ) ;
#71733 = DIRECTION ( 'NONE',  ( -0.000000000000000000, 0.3543493200069153248, 0.9351131265310292928 ) ) ;
#71734 = CARTESIAN_POINT ( 'NONE',  ( 126.6594863501952801, 5.928045853110953445, 3.350272726927312483 ) ) ;
#71735 = VECTOR ( 'NONE', #136918, 1000.000000000000000 ) ;
#71736 = CARTESIAN_POINT ( 'NONE',  ( 12.69999999999999574, -22.26999999999999247, -0.5000000000000004441 ) ) ;
#71737 = CARTESIAN_POINT ( 'NONE',  ( 18.63999999999999702, 2.055000000000001492, 2.516649172247811554E-16 ) ) ;
#71738 = CARTESIAN_POINT ( 'NONE',  ( -30.18398860626900060, 28.73617430169808173, 5.000000000000000000 ) ) ;
#71739 = AXIS2_PLACEMENT_3D ( 'NONE', #117673, #53150, #130758 ) ;
#71740 = CARTESIAN_POINT ( 'NONE',  ( 79.74999999999998579, -9.735942053221458872E-16, 7.950000000000000178 ) ) ;
#71741 = CARTESIAN_POINT ( 'NONE',  ( -3.183988606268992161, 28.73617430169789699, 5.000000000000000000 ) ) ;
#71742 = CARTESIAN_POINT ( 'NONE',  ( 12.98911971346042549, -22.02621442084248216, 4.990779571109223767 ) ) ;
#71743 = CARTESIAN_POINT ( 'NONE',  ( -22.49999999999983658, -8.947814304570739452, 5.000000000000000000 ) ) ;
#71744 = DIRECTION ( 'NONE',  ( 0.7071067811865487940, -0.7071067811865463515, 0.000000000000000000 ) ) ;
#71745 = EDGE_CURVE ( 'NONE', #4118, #123737, #53448, .T. ) ;
#71746 = EDGE_CURVE ( 'NONE', #138298, #103133, #111781, .T. ) ;
#71747 = ORIENTED_EDGE ( 'NONE', *, *, #48938, .T. ) ;
#71748 = ORIENTED_EDGE ( 'NONE', *, *, #82483, .F. ) ;
#71749 = CARTESIAN_POINT ( 'NONE',  ( 111.7087635252314470, -7.482591942790329030E-16, 6.110000000000001208 ) ) ;
#71750 = ORIENTED_EDGE ( 'NONE', *, *, #82652, .F. ) ;
#71751 = LINE ( 'NONE', #36950, #45592 ) ;
#71752 = VECTOR ( 'NONE', #118570, 1000.000000000000000 ) ;
#71753 = CARTESIAN_POINT ( 'NONE',  ( 7.437500000000000000, -4.461849672132299105, 4.461849672132299993 ) ) ;
#71754 = ORIENTED_EDGE ( 'NONE', *, *, #16731, .T. ) ;
#71755 = EDGE_CURVE ( 'NONE', #75268, #70831, #24759, .T. ) ;
#71756 = CARTESIAN_POINT ( 'NONE',  ( -21.79289321881330110, 9.759292476615616607, 5.000000000000000000 ) ) ;
#71757 = CARTESIAN_POINT ( 'NONE',  ( 12.18398860626900060, 28.73617430169795739, 5.000000000000000000 ) ) ;
#71758 = CARTESIAN_POINT ( 'NONE',  ( 101.5579301918981088, 6.110000000000000320, -1.637169565754156064 ) ) ;
#71759 = ORIENTED_EDGE ( 'NONE', *, *, #75394, .T. ) ;
#71760 = DIRECTION ( 'NONE',  ( 0.3543493200069162685, -0.000000000000000000, -0.9351131265310288487 ) ) ;
#71761 = ORIENTED_EDGE ( 'NONE', *, *, #47991, .T. ) ;
#71762 = CARTESIAN_POINT ( 'NONE',  ( -39.18398860626899705, 28.73617430169814568, 5.000000000000000000 ) ) ;
#71763 = FACE_OUTER_BOUND ( 'NONE', #109951, .T. ) ;
#71764 = VECTOR ( 'NONE', #79347, 999.9999999999998863 ) ;
#71765 = DIRECTION ( 'NONE',  ( 0.7071067811865487940, 0.7071067811865463515, -0.000000000000000000 ) ) ;
#71766 = DIRECTION ( 'NONE',  ( -0.7071067811865487940, 0.7071067811865463515, 0.000000000000000000 ) ) ;
#71767 = VERTEX_POINT ( 'NONE', #844 ) ;
#71768 = EDGE_LOOP ( 'NONE', ( #70087, #46381 ) ) ;
#71769 = ORIENTED_EDGE ( 'NONE', *, *, #100267, .F. ) ;
#71770 = CARTESIAN_POINT ( 'NONE',  ( 156.1500000000000057, -49.14999999999999147, -49.92499999999968452 ) ) ;
#71771 = FACE_OUTER_BOUND ( 'NONE', #19174, .T. ) ;
#71772 = CARTESIAN_POINT ( 'NONE',  ( 8.671236474768553748, 0.000000000000000000, 7.934999999999990727 ) ) ;
#71773 = DIRECTION ( 'NONE',  ( 0.000000000000000000, -1.000000000000000000, 0.000000000000000000 ) ) ;
#71774 = CARTESIAN_POINT ( 'NONE',  ( 32.99999999999977973, -6.033600742197672950, 5.000000000000000000 ) ) ;
#71775 = ORIENTED_EDGE ( 'NONE', *, *, #19114, .F. ) ;
#71776 = ORIENTED_EDGE ( 'NONE', *, *, #135256, .F. ) ;
#71777 = LINE ( 'NONE', #52831, #52538 ) ;
#71779 = EDGE_CURVE ( 'NONE', #50892, #114341, #69004, .T. ) ;
#71778 = ORIENTED_EDGE ( 'NONE', *, *, #32080, .F. ) ;
#71780 = ORIENTED_EDGE ( 'NONE', *, *, #66011, .F. ) ;
#71781 = CARTESIAN_POINT ( 'NONE',  ( 112.0579301918981230, 6.110000000000000320, -1.637169565754156064 ) ) ;
#71782 = VECTOR ( 'NONE', #138888, 1000.000000000000000 ) ;
#71783 = DIRECTION ( 'NONE',  ( 0.7071067811865486830, -0.7071067811865464625, -0.000000000000000000 ) ) ;
#71784 = DIRECTION ( 'NONE',  ( -0.3543493200069162685, -0.000000000000000000, -0.9351131265310288487 ) ) ;
#71785 = VERTEX_POINT ( 'NONE', #3000 ) ;
#71786 = CARTESIAN_POINT ( 'NONE',  ( 6.708333333333333925, 3.047499999999997655, 5.278424836066143655 ) ) ;
#71787 = LINE ( 'NONE', #28272, #40924 ) ;
#71788 = PLANE ( 'NONE',  #6632 ) ;
#71789 = AXIS2_PLACEMENT_3D ( 'NONE', #42059, #28323, #63110 ) ;
#71790 = VECTOR ( 'NONE', #84185, 1000.000000000000000 ) ;
#71791 = VECTOR ( 'NONE', #88435, 1000.000000000000227 ) ;
#71792 = DIRECTION ( 'NONE',  ( -0.7071067811865487940, 0.7071067811865463515, -0.000000000000000000 ) ) ;
#71793 = VERTEX_POINT ( 'NONE', #134252 ) ;
#71794 = EDGE_CURVE ( 'NONE', #39262, #64959, #57417, .T. ) ;
#71795 = CARTESIAN_POINT ( 'NONE',  ( -19.72673754300674531, 9.106605730562614909, 4.258036837949483733 ) ) ;
#71796 = FACE_BOUND ( 'NONE', #140311, .T. ) ;
#71797 = ORIENTED_EDGE ( 'NONE', *, *, #74583, .F. ) ;
#71798 = CARTESIAN_POINT ( 'NONE',  ( 36.18398860626899705, 28.73617430169812437, 5.000000000000000000 ) ) ;
#71799 = EDGE_CURVE ( 'NONE', #77043, #136204, #45133, .T. ) ;
#71800 = CARTESIAN_POINT ( 'NONE',  ( 31.49999999999978684, 16.77039438581781994, 0.4657186855307002826 ) ) ;
#71801 = ORIENTED_EDGE ( 'NONE', *, *, #130756, .T. ) ;
#71802 = DIRECTION ( 'NONE',  ( 0.3543493200069162685, -0.000000000000000000, -0.9351131265310288487 ) ) ;
#71803 = VERTEX_POINT ( 'NONE', #2256 ) ;
#71804 = EDGE_LOOP ( 'NONE', ( #44421, #4961, #111358, #112505, #20757 ) ) ;
#71805 = VECTOR ( 'NONE', #24967, 1000.000000000000000 ) ;
#71806 =( BOUNDED_CURVE ( )  B_SPLINE_CURVE ( 3, ( #19582, #140639, #121033, #42076 ),
 .UNSPECIFIED., .F., .T. ) 
 B_SPLINE_CURVE_WITH_KNOTS ( ( 4, 4 ),
 ( 1.901594255663606736, 1.933014472006568507 ),
 .UNSPECIFIED. ) 
 CURVE ( )  GEOMETRIC_REPRESENTATION_ITEM ( )  RATIONAL_B_SPLINE_CURVE ( ( 1.000000000000000000, 0.9999177325257867510, 0.9999177325257867510, 1.000000000000000000 ) ) 
 REPRESENTATION_ITEM ( '' )  );
#71807 = ORIENTED_EDGE ( 'NONE', *, *, #108085, .T. ) ;
#71808 = EDGE_CURVE ( 'NONE', #107846, #129409, #32812, .T. ) ;
#71809 = ADVANCED_FACE ( 'NONE', ( #112490 ), #46572, .F. ) ;
#71810 = CARTESIAN_POINT ( 'NONE',  ( 33.74543019189811588, -5.291415217122918513, -3.055000000000000160 ) ) ;
#71811 = VERTEX_POINT ( 'NONE', #35687 ) ;
#71812 = FACE_OUTER_BOUND ( 'NONE', #51148, .T. ) ;
#71813 = CARTESIAN_POINT ( 'NONE',  ( 27.99999999999996803, -49.14999999999999147, 49.92499999999997584 ) ) ;
#71814 = CARTESIAN_POINT ( 'NONE',  ( -29.99999999999979039, 1.931123077392163712, 4.000000000000000000 ) ) ;
#71815 = EDGE_CURVE ( 'NONE', #79053, #51562, #107, .T. ) ;
#71816 = CARTESIAN_POINT ( 'NONE',  ( 12.86840764549667604, 3.061616997868380183E-16, -2.500000000000001332 ) ) ;
#71817 = VECTOR ( 'NONE', #94333, 1000.000000000000000 ) ;
#71818 = VECTOR ( 'NONE', #22990, 1000.000000000000227 ) ;
#71819 = LINE ( 'NONE', #124744, #90861 ) ;
#71820 = EDGE_CURVE ( 'NONE', #55207, #94043, #21901, .T. ) ;
#71821 = VECTOR ( 'NONE', #49654, 1000.000000000000000 ) ;
#71822 = CARTESIAN_POINT ( 'NONE',  ( 2.700255128608413990, -27.71228299555204089, 4.000000000000000000 ) ) ;
#71823 = DIRECTION ( 'NONE',  ( -0.7071067811865486830, -0.7071067811865464625, 0.000000000000000000 ) ) ;
#71824 = DIRECTION ( 'NONE',  ( 0.7071067811865486830, -0.7071067811865464625, -0.000000000000000000 ) ) ;
#71825 = PLANE ( 'NONE',  #3028 ) ;
#71826 = EDGE_LOOP ( 'NONE', ( #51127, #94764, #81363, #87472 ) ) ;
#71827 = AXIS2_PLACEMENT_3D ( 'NONE', #109847, #64218, #141788 ) ;
#71828 = ORIENTED_EDGE ( 'NONE', *, *, #65072, .T. ) ;
#71829 = ORIENTED_EDGE ( 'NONE', *, *, #124388, .F. ) ;
#71830 = VERTEX_POINT ( 'NONE', #66149 ) ;
#71831 = CARTESIAN_POINT ( 'NONE',  ( 60.18398860626900415, 28.73617430169829490, 5.000000000000000000 ) ) ;
#71832 = EDGE_CURVE ( 'NONE', #83942, #123983, #74266, .T. ) ;
#71833 = VERTEX_POINT ( 'NONE', #10994 ) ;
#71834 = VECTOR ( 'NONE', #104088, 1000.000000000000000 ) ;
#71835 = ORIENTED_EDGE ( 'NONE', *, *, #63936, .T. ) ;
#71836 = DIRECTION ( 'NONE',  ( 0.6830127018922181881, 0.6830127018922202975, -0.2588190451025214056 ) ) ;
#71837 = CARTESIAN_POINT ( 'NONE',  ( 13.08100000000000307, 3.174999999999998046, 5.000000000000000000 ) ) ;
#71838 = VECTOR ( 'NONE', #78804, 1000.000000000000000 ) ;
#71839 = DIRECTION ( 'NONE',  ( 0.7071067811865487940, 0.7071067811865463515, 0.000000000000000000 ) ) ;
#71840 = ORIENTED_EDGE ( 'NONE', *, *, #98195, .T. ) ;
#71841 = AXIS2_PLACEMENT_3D ( 'NONE', #129849, #142177, #139334 ) ;
#71842 = DIRECTION ( 'NONE',  ( 0.3543493200069162685, -0.000000000000000000, -0.9351131265310288487 ) ) ;
#71843 = EDGE_CURVE ( 'NONE', #125467, #45614, #45829, .T. ) ;
#71844 = ORIENTED_EDGE ( 'NONE', *, *, #113248, .T. ) ;
#71845 = CARTESIAN_POINT ( 'NONE',  ( -19.49999999999986144, -17.94781430457064531, 5.000000000000000000 ) ) ;
#71846 = CARTESIAN_POINT ( 'NONE',  ( -29.99999999999977973, 17.58746187583906462, 4.000000000000000000 ) ) ;
#71847 = MECHANICAL_DESIGN_GEOMETRIC_PRESENTATION_REPRESENTATION (  '', ( #134345 ), #97239 ) ;
#71848 = EDGE_LOOP ( 'NONE', ( #117028, #116247, #58115, #29302 ) ) ;
#71850 = CARTESIAN_POINT ( 'NONE',  ( 3.328169399223500413, -21.74070752338406365, 4.000000000000000000 ) ) ;
#71849 = CARTESIAN_POINT ( 'NONE',  ( 102.5787635252314658, -7.482591942790327058E-16, 6.109999999999999432 ) ) ;
#71851 = DIRECTION ( 'NONE',  ( -0.6830127018922181881, 0.6830127018922202975, -0.2588190451025214056 ) ) ;
#71852 = EDGE_LOOP ( 'NONE', ( #73480, #47905, #3993, #81626 ) ) ;
#71853 = EDGE_CURVE ( 'NONE', #40909, #29037, #44411, .T. ) ;
#71854 = ORIENTED_EDGE ( 'NONE', *, *, #105326, .F. ) ;
#71855 = DIRECTION ( 'NONE',  ( 1.000000000000000000, 1.224606353822377258E-16, 0.000000000000000000 ) ) ;
#71856 = AXIS2_PLACEMENT_3D ( 'NONE', #106615, #95767, #29784 ) ;
#71857 = ORIENTED_EDGE ( 'NONE', *, *, #48234, .T. ) ;
#71858 = DIRECTION ( 'NONE',  ( 0.3543493200069162685, -0.000000000000000000, -0.9351131265310288487 ) ) ;
#71859 = DIRECTION ( 'NONE',  ( 0.7071067811865487940, 0.7071067811865463515, 0.000000000000000000 ) ) ;
#71860 = CARTESIAN_POINT ( 'NONE',  ( 53.41205288902393278, -48.51956544822605366, -36.87500513592858198 ) ) ;
#71861 = DIRECTION ( 'NONE',  ( 0.6830127018922181881, 0.6830127018922202975, -0.2588190451025214056 ) ) ;
#71862 = LINE ( 'NONE', #139258, #72680 ) ;
#71863 = ORIENTED_EDGE ( 'NONE', *, *, #64241, .F. ) ;
#71864 = EDGE_CURVE ( 'NONE', #31073, #117180, #79188, .T. ) ;
#71865 = CARTESIAN_POINT ( 'NONE',  ( 57.48921356237308800, -27.52281430457095368, 5.000000000000000000 ) ) ;
#71866 = EDGE_CURVE ( 'NONE', #142463, #98919, #68316, .T. ) ;
#71867 = FACE_OUTER_BOUND ( 'NONE', #22395, .T. ) ;
#71868 = CARTESIAN_POINT ( 'NONE',  ( 26.99999999999980815, 18.08204922493375477, 0.9627537363044238461 ) ) ;
#71869 = ORIENTED_EDGE ( 'NONE', *, *, #56184, .F. ) ;
#71870 = CARTESIAN_POINT ( 'NONE',  ( 7.122370700763592133, -39.92999999999999972, 19.06900128115122328 ) ) ;
#71871 = VECTOR ( 'NONE', #55795, 1000.000000000000000 ) ;
#71873 = EDGE_CURVE ( 'NONE', #139318, #4593, #125519, .T. ) ;
#71872 = CARTESIAN_POINT ( 'NONE',  ( 2.719980320105942262, 0.7592924766157069794, 14.27032725228009902 ) ) ;
#71874 = ORIENTED_EDGE ( 'NONE', *, *, #40070, .F. ) ;
#71876 = ORIENTED_EDGE ( 'NONE', *, *, #130605, .T. ) ;
#71875 = CARTESIAN_POINT ( 'NONE',  ( -10.49999999999992539, 8.319652575858375698, -8.582050562765852320 ) ) ;
#71877 = ORIENTED_EDGE ( 'NONE', *, *, #121267, .T. ) ;
#71878 = CARTESIAN_POINT ( 'NONE',  ( 25.82816939922334853, -8.240707523384203981, 4.000000000000000000 ) ) ;
#71879 = CARTESIAN_POINT ( 'NONE',  ( 29.99451991528749417, 28.92564299267958816, 4.000000000000000000 ) ) ;
#71881 = EDGE_LOOP ( 'NONE', ( #112609, #37162, #13699, #11142 ) ) ;
#71880 = VECTOR ( 'NONE', #51916, 1000.000000000000000 ) ;
#71882 = CARTESIAN_POINT ( 'NONE',  ( 14.99999999999990230, 8.587461875839158765, 4.000000000000000000 ) ) ;
#71883 = CLOSED_SHELL ( 'NONE', ( #107309, #29756, #49611, #3731 ) ) ;
#71884 = CARTESIAN_POINT ( 'NONE',  ( 63.18398860626900415, 28.73617430169831621, 5.000000000000000000 ) ) ;
#71885 = LINE ( 'NONE', #27622, #129413 ) ;
#71886 = ORIENTED_EDGE ( 'NONE', *, *, #5223, .F. ) ;
#71887 = EDGE_CURVE ( 'NONE', #69437, #75364, #61701, .T. ) ;
#71888 = DIRECTION ( 'NONE',  ( 0.7071067811865486830, -0.7071067811865464625, -0.000000000000000000 ) ) ;
#71889 = DIRECTION ( 'NONE',  ( -0.7071067811865486830, -0.7071067811865464625, 0.000000000000000000 ) ) ;
#71890 = DIRECTION ( 'NONE',  ( -0.7071067811865487940, 0.7071067811865463515, -0.000000000000000000 ) ) ;
#71891 = FACE_OUTER_BOUND ( 'NONE', #64093, .T. ) ;
#71892 = CARTESIAN_POINT ( 'NONE',  ( 25.39999999999999858, 0.000000000000000000, 0.000000000000000000 ) ) ;
#71893 = CARTESIAN_POINT ( 'NONE',  ( -28.82334089840009028, 5.259292476615665457, 15.86257073897104419 ) ) ;
#71894 = CARTESIAN_POINT ( 'NONE',  ( -19.49999999999985079, 10.46639925780215208, 5.000000000000000000 ) ) ;
#71896 = EDGE_CURVE ( 'NONE', #7006, #107344, #116036, .T. ) ;
#71895 = VECTOR ( 'NONE', #64359, 1000.000000000000227 ) ;
#71897 = DIRECTION ( 'NONE',  ( -0.7071067811865486830, 0.7071067811865464625, 0.000000000000000000 ) ) ;
#71898 = LINE ( 'NONE', #105200, #103257 ) ;
#71899 = EDGE_LOOP ( 'NONE', ( #68221, #110035, #38221, #67122, #69144, #56077, #2962, #69559 ) ) ;
#71900 = ORIENTED_EDGE ( 'NONE', *, *, #14229, .F. ) ;
#71901 = ORIENTED_EDGE ( 'NONE', *, *, #14355, .T. ) ;
#71902 = CARTESIAN_POINT ( 'NONE',  ( 117.9583333333333286, 3.974999999999997424, 6.884901960086288852 ) ) ;
#71903 = AXIS2_PLACEMENT_3D ( 'NONE', #52475, #96661, #132942 ) ;
#71904 = ORIENTED_EDGE ( 'NONE', *, *, #123998, .F. ) ;
#71905 = ORIENTED_EDGE ( 'NONE', *, *, #139422, .F. ) ;
#71906 = ORIENTED_EDGE ( 'NONE', *, *, #134000, .F. ) ;
#71907 = LINE ( 'NONE', #18165, #68772 ) ;
#71908 = CARTESIAN_POINT ( 'NONE',  ( -33.48921356237309510, -27.52281430457078670, 5.000000000000000000 ) ) ;
#71909 = AXIS2_PLACEMENT_3D ( 'NONE', #37599, #4904, #26707 ) ;
#71910 = VECTOR ( 'NONE', #136748, 1000.000000000000227 ) ;
#71911 = AXIS2_PLACEMENT_3D ( 'NONE', #26557, #91124, #114945 ) ;
#71912 = VECTOR ( 'NONE', #75492, 1000.000000000000000 ) ;
#71913 = ORIENTED_EDGE ( 'NONE', *, *, #98134, .F. ) ;
#71914 = CARTESIAN_POINT ( 'NONE',  ( 24.18398860626899705, 28.73617430169804265, 5.000000000000000000 ) ) ;
#71915 = VECTOR ( 'NONE', #64320, 1000.000000000000000 ) ;
#71916 = DIRECTION ( 'NONE',  ( 0.6830127018922180770, -0.6830127018922204085, -0.2588190451025213501 ) ) ;
#71917 = PLANE ( 'NONE',  #53241 ) ;
#71918 = FACE_OUTER_BOUND ( 'NONE', #103420, .T. ) ;
#71919 = CARTESIAN_POINT ( 'NONE',  ( 112.0004301918981042, -3.055000000000002380, 5.291415217122920289 ) ) ;
#71920 = ORIENTED_EDGE ( 'NONE', *, *, #127314, .T. ) ;
#71921 = CARTESIAN_POINT ( 'NONE',  ( 25.19159235450331735, 9.902892378096218942E-16, 0.000000000000000000 ) ) ;
#71922 = PLANE ( 'NONE',  #67880 ) ;
#71923 = CARTESIAN_POINT ( 'NONE',  ( -30.72281430457039875, -21.72499999999999432, 5.000000000000000000 ) ) ;
#71924 = VECTOR ( 'NONE', #95593, 1000.000000000000000 ) ;
#71925 = LINE ( 'NONE', #127713, #6045 ) ;
#71926 = DIRECTION ( 'NONE',  ( 0.000000000000000000, 0.000000000000000000, 1.000000000000000000 ) ) ;
#71927 = CARTESIAN_POINT ( 'NONE',  ( 36.97502705046289861, -5.819803920172572198, 5.819803920172572198 ) ) ;
#71928 = DIRECTION ( 'NONE',  ( -0.3543493200069162685, -0.000000000000000000, -0.9351131265310288487 ) ) ;
#71929 = EDGE_CURVE ( 'NONE', #58716, #77500, #47291, .T. ) ;
#71930 = ORIENTED_EDGE ( 'NONE', *, *, #48950, .T. ) ;
#71931 = ORIENTED_EDGE ( 'NONE', *, *, #140716, .T. ) ;
#71932 = CARTESIAN_POINT ( 'NONE',  ( 32.49999999999998579, 0.000000000000000000, -7.950000000000000178 ) ) ;
#71933 = VERTEX_POINT ( 'NONE', #93597 ) ;
#71934 = FACE_OUTER_BOUND ( 'NONE', #128272, .T. ) ;
#71935 = VECTOR ( 'NONE', #105040, 999.9999999999998863 ) ;
#71936 = DIRECTION ( 'NONE',  ( -0.000000000000000000, 0.3543493200069153248, 0.9351131265310292928 ) ) ;
#71937 = VERTEX_POINT ( 'NONE', #37060 ) ;
#71938 = CARTESIAN_POINT ( 'NONE',  ( 34.92499999999998295, -19.29806943317882784, 4.500000000000000888 ) ) ;
#71939 = FILL_AREA_STYLE_COLOUR ( '', #56187 ) ;
#71940 = LINE ( 'NONE', #48038, #139335 ) ;
#71941 = DIRECTION ( 'NONE',  ( -0.000000000000000000, -0.3543493200069152693, 0.9351131265310292928 ) ) ;
#71942 = AXIS2_PLACEMENT_3D ( 'NONE', #27686, #4443, #72688 ) ;
#71943 = AXIS2_PLACEMENT_3D ( 'NONE', #8784, #97240, #99386 ) ;
#71944 = CARTESIAN_POINT ( 'NONE',  ( 30.18793019189809357, 6.110000000000002984, -1.637169565754156730 ) ) ;
#71945 = VERTEX_POINT ( 'NONE', #25458 ) ;
#71946 = AXIS2_PLACEMENT_3D ( 'NONE', #47341, #91510, #135721 ) ;
#71947 = PLANE ( 'NONE',  #34056 ) ;
#71948 = ORIENTED_EDGE ( 'NONE', *, *, #17999, .T. ) ;
#71949 = SPHERICAL_SURFACE ( 'NONE', #40552, 0.5000000000000000000 ) ;
#71950 = AXIS2_PLACEMENT_3D ( 'NONE', #27097, #71338, #25667 ) ;
#71951 = PRESENTATION_STYLE_ASSIGNMENT (( #126992 ) ) ;
#71952 = CARTESIAN_POINT ( 'NONE',  ( 14.27718569542929572, -21.72500000000000142, 5.000000000000000000 ) ) ;
#71953 = CARTESIAN_POINT ( 'NONE',  ( 63.56249999999999289, -5.819803920172573086, -5.819803920172573974 ) ) ;
#71954 = VERTEX_POINT ( 'NONE', #28346 ) ;
#71955 = CARTESIAN_POINT ( 'NONE',  ( 55.12543019189811133, 5.291415217122919401, 3.055000000000002824 ) ) ;
#71956 = ORIENTED_EDGE ( 'NONE', *, *, #63275, .F. ) ;
#71957 = AXIS2_PLACEMENT_3D ( 'NONE', #4561, #129246, #59752 ) ;
#71958 = PLANE ( 'NONE',  #91042 ) ;
#71959 = DIRECTION ( 'NONE',  ( -0.000000000000000000, -0.3543493200069152693, 0.9351131265310292928 ) ) ;
#71960 = CARTESIAN_POINT ( 'NONE',  ( 8.999999999999937828, 12.83542986846997813, -1.025386466790390694 ) ) ;
#71961 = CARTESIAN_POINT ( 'NONE',  ( 32.24139925780183091, 21.72499999999999432, 5.000000000000000000 ) ) ;
#71962 = VECTOR ( 'NONE', #53300, 1000.000000000000000 ) ;
#71963 = CARTESIAN_POINT ( 'NONE',  ( 46.57876352523145158, -7.482591942790325086E-16, 6.109999999999998543 ) ) ;
#71964 = ORIENTED_EDGE ( 'NONE', *, *, #19738, .T. ) ;
#71965 = DIRECTION ( 'NONE',  ( -0.7071067811865486830, -0.7071067811865464625, 0.000000000000000000 ) ) ;
#71966 = CARTESIAN_POINT ( 'NONE',  ( -34.42500000000001137, 0.000000000000000000, 4.500000000000000888 ) ) ;
#71967 = VERTEX_POINT ( 'NONE', #116762 ) ;
#71968 = ORIENTED_EDGE ( 'NONE', *, *, #13671, .T. ) ;
#71969 = VECTOR ( 'NONE', #42845, 1000.000000000000000 ) ;
#71970 = CARTESIAN_POINT ( 'NONE',  ( 7.499999999999951150, -4.796895815301009947, -3.611700055028665535 ) ) ;
#71971 = VERTEX_POINT ( 'NONE', #17445 ) ;
#71972 = DIRECTION ( 'NONE',  ( 0.000000000000000000, 0.000000000000000000, 1.000000000000000000 ) ) ;
#71973 = ORIENTED_EDGE ( 'NONE', *, *, #71997, .T. ) ;
#71974 = CARTESIAN_POINT ( 'NONE',  ( 33.29974487139158867, -27.71228299555229313, 4.000000000000000000 ) ) ;
#71975 = EDGE_CURVE ( 'NONE', #115465, #34254, #62681, .T. ) ;
#71976 = FACE_BOUND ( 'NONE', #136467, .T. ) ;
#71977 = CARTESIAN_POINT ( 'NONE',  ( -34.42500000000001137, 5.977185695429358958, 5.000000000000000000 ) ) ;
#71978 = ADVANCED_FACE ( 'NONE', ( #113912 ), #115291, .F. ) ;
#71979 = ADVANCED_FACE ( 'NONE', ( #39216 ), #103719, .F. ) ;
#71980 = DIRECTION ( 'NONE',  ( -0.6830127018922180770, -0.6830127018922204085, -0.2588190451025213501 ) ) ;
#71981 = ORIENTED_EDGE ( 'NONE', *, *, #100272, .T. ) ;
#71982 = FACE_OUTER_BOUND ( 'NONE', #31866, .T. ) ;
#71984 = EDGE_LOOP ( 'NONE', ( #126679, #102989, #140184, #73881 ) ) ;
#71983 = CARTESIAN_POINT ( 'NONE',  ( 122.6835989386367345, -57.15000000000010516, 40.92499999999998295 ) ) ;
#71985 = EDGE_LOOP ( 'NONE', ( #86381, #40658, #52458, #26169 ) ) ;
#71986 = VECTOR ( 'NONE', #129267, 1000.000000000000227 ) ;
#71987 = VECTOR ( 'NONE', #107304, 999.9999999999998863 ) ;
#71988 = CARTESIAN_POINT ( 'NONE',  ( 11.15159235450332176, 9.902892378096218942E-16, 0.000000000000000000 ) ) ;
#71989 = VERTEX_POINT ( 'NONE', #137101 ) ;
#71990 = EDGE_CURVE ( 'NONE', #107902, #46199, #126902, .T. ) ;
#71991 = EDGE_CURVE ( 'NONE', #118884, #15218, #81310, .T. ) ;
#71992 = VERTEX_POINT ( 'NONE', #37805 ) ;
#71993 = CARTESIAN_POINT ( 'NONE',  ( 70.34959685856479439, 6.109999999999996767, 1.637169565754163836 ) ) ;
#71994 = ORIENTED_EDGE ( 'NONE', *, *, #90817, .T. ) ;
#71995 = DIRECTION ( 'NONE',  ( 0.6830127018922181881, 0.6830127018922202975, -0.2588190451025214056 ) ) ;
#71996 = CARTESIAN_POINT ( 'NONE',  ( -12.18398860626900060, 28.73617430169795739, 5.000000000000000000 ) ) ;
#71997 = EDGE_CURVE ( 'NONE', #91987, #57991, #4363, .T. ) ;
#71998 = ORIENTED_EDGE ( 'NONE', *, *, #134348, .F. ) ;
#71999 = DIRECTION ( 'NONE',  ( 0.7071067811865487940, -0.7071067811865463515, 0.000000000000000000 ) ) ;
#72000 = EDGE_CURVE ( 'NONE', #139988, #45425, #137826, .T. ) ;
#72001 = VECTOR ( 'NONE', #38521, 1000.000000000000000 ) ;
#72002 = VECTOR ( 'NONE', #59337, 1000.000000000000227 ) ;
#72003 = EDGE_CURVE ( 'NONE', #108960, #124077, #26902, .T. ) ;
#72004 = VECTOR ( 'NONE', #41086, 1000.000000000000000 ) ;
#72005 = CARTESIAN_POINT ( 'NONE',  ( 35.12499999999999289, -7.950000000000000178, -4.867971026610729436E-16 ) ) ;
#72006 = DIRECTION ( 'NONE',  ( 0.3543493200069162685, -0.000000000000000000, -0.9351131265310288487 ) ) ;
#72007 = CARTESIAN_POINT ( 'NONE',  ( 29.99451991528749417, 28.92564299267958816, 4.000000000000000000 ) ) ;
#72008 = LINE ( 'NONE', #114737, #132641 ) ;
#72009 = CARTESIAN_POINT ( 'NONE',  ( 10.49999999999993250, 5.696342897626511359, -7.587980461218374550 ) ) ;
#72010 = VERTEX_POINT ( 'NONE', #27603 ) ;
#72011 = AXIS2_PLACEMENT_3D ( 'NONE', #90761, #121208, #34220 ) ;
#72012 = AXIS2_PLACEMENT_3D ( 'NONE', #83672, #38709, #7483 ) ;
#72013 = VECTOR ( 'NONE', #61031, 1000.000000000000000 ) ;
#72014 = VERTEX_POINT ( 'NONE', #69731 ) ;
#72015 = PRESENTATION_LAYER_ASSIGNMENT (  '', '', ( #53452 ) ) ;
#72016 = CARTESIAN_POINT ( 'NONE',  ( 27.79289321881326202, 15.75929247661555443, 5.000000000000000000 ) ) ;
#72017 = DIRECTION ( 'NONE',  ( -0.7071067811865486830, -0.7071067811865464625, 0.000000000000000000 ) ) ;
#72018 = ORIENTED_EDGE ( 'NONE', *, *, #87630, .F. ) ;
#72019 = ADVANCED_FACE ( 'NONE', ( #71867 ), #124787, .F. ) ;
#72020 = ORIENTED_EDGE ( 'NONE', *, *, #65636, .F. ) ;
#72021 = EDGE_LOOP ( 'NONE', ( #105824, #28488, #117884, #91377 ) ) ;
#72022 = DIRECTION ( 'NONE',  ( -1.000000000000000000, -0.000000000000000000, -0.000000000000000000 ) ) ;
#72023 = FACE_OUTER_BOUND ( 'NONE', #10361, .T. ) ;
#72024 = ORIENTED_EDGE ( 'NONE', *, *, #54062, .F. ) ;
#72025 = VECTOR ( 'NONE', #97562, 1000.000000000000000 ) ;
#72026 = FACE_OUTER_BOUND ( 'NONE', #63967, .T. ) ;
#72027 = ADVANCED_FACE ( 'NONE', ( #8666 ), #19590, .F. ) ;
#72028 = LINE ( 'NONE', #116208, #9968 ) ;
#72029 = CARTESIAN_POINT ( 'NONE',  ( 12.02540314143521982, 2.126176841940962348, 7.934999999999989839 ) ) ;
#72030 = EDGE_LOOP ( 'NONE', ( #59211, #4198, #118447, #19332 ) ) ;
#72031 = AXIS2_PLACEMENT_3D ( 'NONE', #116867, #17541, #92978 ) ;
#72033 = B_SPLINE_CURVE_WITH_KNOTS ( 'NONE', 3,
 ( #136974, #125393, #37681, #81181, #4239, #102925, #92733, #14479, #60147, #24632, #25341, #58756, #81918, #113791, #126108, #26077, #26774, #104311, #35561, #60887, #124665, #137702, #102223, #71025, #3566, #115174, #135561, #47861, #27471, #48535, #4981, #79789, #49282, #5711, #71734, #93468, #114484, #15850, #38376, #69605, #82590, #92027, #105048, #136246, #126787 ),
 .UNSPECIFIED., .F., .F.,
 ( 4, 2, 2, 2, 2, 2, 2, 2, 1, 2, 2, 2, 2, 2, 2, 1, 2, 2, 2, 2, 1, 2, 2, 4 ),
 ( 6.981499371183832972E-15, 0.001511458381938139781, 0.002267187572903719191, 0.003022916763869298602, 0.004534375145800453519, 0.006045833527731608002, 0.007557291909662763353, 0.008313021100628342763, 0.009068750291593921306, 0.009824479482559499849, 0.01058020867352508013, 0.01209166705545623548, 0.01360312543738739256, 0.01511458381931854618, 0.01587031301028412125, 0.01662604220124970153, 0.01738177139221527834, 0.01813750058318085515, 0.01964895896511201223, 0.02040468815607758904, 0.02116041734704316932, 0.02191614653800874959, 0.02267187572897432640, 0.02418333411090548696 ),
 .UNSPECIFIED. ) ;
#72032 = DIRECTION ( 'NONE',  ( 0.7071067811865486830, -0.7071067811865464625, -0.000000000000000000 ) ) ;
#72034 = EDGE_CURVE ( 'NONE', #71967, #118712, #118161, .T. ) ;
#72035 = VECTOR ( 'NONE', #63517, 1000.000000000000000 ) ;
#72036 = DIRECTION ( 'NONE',  ( 0.7071067811865487940, 0.7071067811865463515, -0.000000000000000000 ) ) ;
#72038 = EDGE_LOOP ( 'NONE', ( #6807, #57536, #91534, #46311 ) ) ;
#72037 = DIRECTION ( 'NONE',  ( -0.7071067811865486830, -0.7071067811865464625, 0.000000000000000000 ) ) ;
#72039 = CARTESIAN_POINT ( 'NONE',  ( 17.99999999999987566, 20.70535890316562799, 1.956823837851874970 ) ) ;
#72040 = ORIENTED_EDGE ( 'NONE', *, *, #94496, .T. ) ;
#72041 = DIRECTION ( 'NONE',  ( -0.7071067811865487940, 0.7071067811865463515, -0.000000000000000000 ) ) ;
#72042 = DIRECTION ( 'NONE',  ( -0.7071067811865487940, 0.7071067811865463515, -0.000000000000000000 ) ) ;
#72043 = CYLINDRICAL_SURFACE ( 'NONE', #65632, 0.5000000000000004441 ) ;
#72044 = EDGE_LOOP ( 'NONE', ( #29023, #117700, #29994, #39352, #112385 ) ) ;
#72045 = AXIS2_PLACEMENT_3D ( 'NONE', #82468, #51812, #106869 ) ;
#72046 = EDGE_CURVE ( 'NONE', #14375, #143096, #85546, .T. ) ;
#72047 = VECTOR ( 'NONE', #100270, 1000.000000000000000 ) ;
#72048 = EDGE_CURVE ( 'NONE', #123737, #30060, #35062, .T. ) ;
#72050 = CARTESIAN_POINT ( 'NONE',  ( 20.51078643762690490, -27.52281430457041012, 5.000000000000000000 ) ) ;
#72049 = STYLED_ITEM ( 'NONE', ( #12930 ), #84438 ) ;
#72051 = DIRECTION ( 'NONE',  ( 0.6830127018922180770, -0.6830127018922204085, -0.2588190451025213501 ) ) ;
#72052 = LINE ( 'NONE', #16918, #23609 ) ;
#72053 = EDGE_LOOP ( 'NONE', ( #60632, #126347, #15224, #65902 ) ) ;
#72054 = FACE_OUTER_BOUND ( 'NONE', #121243, .T. ) ;
#72055 = VECTOR ( 'NONE', #101629, 1000.000000000000227 ) ;
#72056 = CARTESIAN_POINT ( 'NONE',  ( 18.18398860626898994, 28.73617430169800002, 5.000000000000000000 ) ) ;
#72057 = EDGE_CURVE ( 'NONE', #100524, #102057, #9390, .T. ) ;
#72059 = EDGE_CURVE ( 'NONE', #6489, #130351, #50805, .T. ) ;
#72058 = FACE_OUTER_BOUND ( 'NONE', #7989, .T. ) ;
#72060 = CARTESIAN_POINT ( 'NONE',  ( -14.20666063542142687, 21.75929247661549937, 4.998822639870708073 ) ) ;
#72061 = DIRECTION ( 'NONE',  ( -0.3543493200069162685, -0.000000000000000000, -0.9351131265310288487 ) ) ;
#72062 = ORIENTED_EDGE ( 'NONE', *, *, #131248, .F. ) ;
#72063 = VECTOR ( 'NONE', #16009, 1000.000000000000227 ) ;
#72064 = ORIENTED_EDGE ( 'NONE', *, *, #63155, .F. ) ;
#72065 = DIRECTION ( 'NONE',  ( -0.6830127018922181881, 0.6830127018922202975, -0.2588190451025214056 ) ) ;
#72066 = SURFACE_STYLE_FILL_AREA ( #103905 ) ;
#72067 = CARTESIAN_POINT ( 'NONE',  ( 4.353736474768552966, -5.808823158059035485, -5.808823158059033709 ) ) ;
#72068 = PLANE ( 'NONE',  #96817 ) ;
#72069 = VECTOR ( 'NONE', #138996, 1000.000000000000227 ) ;
#72070 = CARTESIAN_POINT ( 'NONE',  ( 156.1500000000000057, -57.14999999999999147, 49.92499999999997584 ) ) ;
#72071 = LINE ( 'NONE', #29930, #59900 ) ;
#72072 = DIRECTION ( 'NONE',  ( -0.7071067811865486830, 0.7071067811865464625, 0.000000000000000000 ) ) ;
#72073 = ORIENTED_EDGE ( 'NONE', *, *, #21095, .T. ) ;
#72074 = EDGE_CURVE ( 'NONE', #31974, #57153, #29048, .T. ) ;
#72075 = CARTESIAN_POINT ( 'NONE',  ( 25.49999999999982947, -2.568876922607784774, 4.000000000000000000 ) ) ;
#72076 = CARTESIAN_POINT ( 'NONE',  ( 34.75611968250419181, -6.187065745292550822, 4.955485411084886493 ) ) ;
#72077 = VECTOR ( 'NONE', #93290, 1000.000000000000000 ) ;
#72078 = DIRECTION ( 'NONE',  ( 0.6830127018922180770, -0.6830127018922204085, -0.2588190451025213501 ) ) ;
#72079 = CIRCLE ( 'NONE', #9496, 2.055000000000001048 ) ;
#72080 = FACE_OUTER_BOUND ( 'NONE', #89973, .T. ) ;
#72081 = CARTESIAN_POINT ( 'NONE',  ( 43.22459685856478728, -1.637169565754161171, 6.109999999999998543 ) ) ;
#72082 = DIRECTION ( 'NONE',  ( -0.6830127018922180770, -0.6830127018922204085, -0.2588190451025213501 ) ) ;
#72083 = EDGE_LOOP ( 'NONE', ( #56527, #140982, #89189, #53237 ) ) ;
#72084 = DIRECTION ( 'NONE',  ( 0.000000000000000000, 0.000000000000000000, -1.000000000000000000 ) ) ;
#72085 = VERTEX_POINT ( 'NONE', #76124 ) ;
#72086 = ORIENTED_EDGE ( 'NONE', *, *, #45662, .F. ) ;
#72087 = CIRCLE ( 'NONE', #4830, 2.500000000000000888 ) ;
#72088 = DIRECTION ( 'NONE',  ( 1.000000000000000000, 0.000000000000000000, 0.000000000000000000 ) ) ;
#72089 =( BOUNDED_CURVE ( )  B_SPLINE_CURVE ( 3, ( #71201, #79957, #103773, #115349 ),
 .UNSPECIFIED., .F., .F. ) 
 B_SPLINE_CURVE_WITH_KNOTS ( ( 4, 4 ),
 ( 5.143245962375976532, 6.645403452391245303 ),
 .UNSPECIFIED. ) 
 CURVE ( )  GEOMETRIC_REPRESENTATION_ITEM ( )  RATIONAL_B_SPLINE_CURVE ( ( 1.000000000000000000, 0.8206354192515270540, 0.8206354192515270540, 1.000000000000000000 ) ) 
 REPRESENTATION_ITEM ( '' )  );
#72090 = DIRECTION ( 'NONE',  ( 0.7071067811865487940, 0.7071067811865463515, 0.000000000000000000 ) ) ;
#72091 = DIRECTION ( 'NONE',  ( 1.000000000000000000, 0.000000000000000000, 0.000000000000000000 ) ) ;
#72092 = DIRECTION ( 'NONE',  ( -0.7071067811865486830, 0.7071067811865464625, 0.000000000000000000 ) ) ;
#72093 = EDGE_CURVE ( 'NONE', #74972, #96881, #86992, .T. ) ;
#72094 = CARTESIAN_POINT ( 'NONE',  ( 16.49999999999988987, 11.52377502935404685, -1.522421517564121363 ) ) ;
#72095 = CARTESIAN_POINT ( 'NONE',  ( 34.92499999999998295, 22.22500000000000142, 4.000000000000000000 ) ) ;
#72096 = VERTEX_POINT ( 'NONE', #63835 ) ;
#72097 = CARTESIAN_POINT ( 'NONE',  ( 10.49999999999993250, 7.087461875839178305, 4.000000000000000000 ) ) ;
#72098 = DIRECTION ( 'NONE',  ( 0.3543493200069162685, -0.000000000000000000, -0.9351131265310288487 ) ) ;
#72099 = UNCERTAINTY_MEASURE_WITH_UNIT (LENGTH_MEASURE( 1.000000000000000082E-05 ), #18386, 'distance_accuracy_value', 'NONE');
#72100 = VECTOR ( 'NONE', #87046, 1000.000000000000227 ) ;
#72101 = DIRECTION ( 'NONE',  ( 0.000000000000000000, -1.000000000000000000, 0.000000000000000000 ) ) ;
#72102 = DIRECTION ( 'NONE',  ( -0.7071067811865486830, -0.7071067811865464625, -0.000000000000000000 ) ) ;
#72103 = CARTESIAN_POINT ( 'NONE',  ( 36.18398860626899705, 28.73617430169812437, 5.000000000000000000 ) ) ;
#72104 = CARTESIAN_POINT ( 'NONE',  ( 68.91252705046288440, -7.949999999999998401, -4.867971026610728450E-16 ) ) ;
#72105 = DIRECTION ( 'NONE',  ( 0.7071067811865486830, -0.7071067811865464625, -0.000000000000000000 ) ) ;
#72106 = ORIENTED_EDGE ( 'NONE', *, *, #77951, .T. ) ;
#72107 = ORIENTED_EDGE ( 'NONE', *, *, #28274, .T. ) ;
#72108 = CARTESIAN_POINT ( 'NONE',  ( 67.50000000000000000, 0.000000000000000000, -7.950000000000000178 ) ) ;
#72109 = DIRECTION ( 'NONE',  ( -0.7071067811865486830, -0.7071067811865464625, 0.000000000000000000 ) ) ;
#72110 = FACE_OUTER_BOUND ( 'NONE', #62272, .T. ) ;
#72111 = ORIENTED_EDGE ( 'NONE', *, *, #12870, .F. ) ;
#72112 = EDGE_CURVE ( 'NONE', #28047, #81238, #52221, .T. ) ;
#72113 = DIRECTION ( 'NONE',  ( 0.7071067811865487940, 0.7071067811865463515, 0.000000000000000000 ) ) ;
#72114 = AXIS2_PLACEMENT_3D ( 'NONE', #33667, #98190, #12588 ) ;
#72115 = VECTOR ( 'NONE', #30779, 1000.000000000000227 ) ;
#72116 = EDGE_CURVE ( 'NONE', #133726, #22423, #84178, .T. ) ;
#72117 = CARTESIAN_POINT ( 'NONE',  ( -20.51078643762690490, -27.52281430457041012, 5.000000000000000000 ) ) ;
#72118 = CARTESIAN_POINT ( 'NONE',  ( 59.79209685856477563, -5.291415217122921177, 3.054999999999999272 ) ) ;
#72119 = PLANE ( 'NONE',  #48291 ) ;
#72120 = EDGE_LOOP ( 'NONE', ( #123721, #75477, #131423, #93646 ) ) ;
#72122 = VERTEX_POINT ( 'NONE', #97109 ) ;
#72121 = VECTOR ( 'NONE', #141372, 999.9999999999998863 ) ;
#72123 = VECTOR ( 'NONE', #24950, 1000.000000000000000 ) ;
#72124 = VECTOR ( 'NONE', #5679, 1000.000000000000114 ) ;
#72125 = VECTOR ( 'NONE', #96301, 999.9999999999998863 ) ;
#72126 = CARTESIAN_POINT ( 'NONE',  ( 5.865004262483735964, 3.759292476615671230, 15.36553568819724447 ) ) ;
#72128 = DIRECTION ( 'NONE',  ( -1.000000000000000000, -1.224606353822377258E-16, -0.000000000000000000 ) ) ;
#72127 = VECTOR ( 'NONE', #49566, 1000.000000000000227 ) ;
#72129 = DIRECTION ( 'NONE',  ( 0.6830127018922181881, 0.6830127018922202975, -0.2588190451025214056 ) ) ;
#72130 = CARTESIAN_POINT ( 'NONE',  ( -34.92500000000001137, -22.22500000000000142, 4.000000000000000000 ) ) ;
#72131 = EDGE_CURVE ( 'NONE', #81104, #98919, #96407, .T. ) ;
#72132 = CARTESIAN_POINT ( 'NONE',  ( 15.29974487139158867, -27.71228299555216879, 4.000000000000000000 ) ) ;
#72134 = VERTEX_POINT ( 'NONE', #30483 ) ;
#72133 = CARTESIAN_POINT ( 'NONE',  ( 11.93159235450332112, 9.902892378096218942E-16, 0.000000000000000000 ) ) ;
#72135 = CARTESIAN_POINT ( 'NONE',  ( -11.99999999999991296, 12.25461709320619796, -10.07315571508699747 ) ) ;
#72136 = DIRECTION ( 'NONE',  ( 0.7071067811865487940, 0.7071067811865463515, 0.000000000000000000 ) ) ;
#72137 = DIRECTION ( 'NONE',  ( 9.912705577010316675E-16, 0.000000000000000000, 1.000000000000000000 ) ) ;
#72138 = STYLED_ITEM ( 'NONE', ( #44670 ), #141443 ) ;
#72139 = CARTESIAN_POINT ( 'NONE',  ( 7.998069433178966570, -22.22500000000000142, 4.500000000000000888 ) ) ;
#72140 = ORIENTED_EDGE ( 'NONE', *, *, #85186, .T. ) ;
#72141 = ORIENTED_EDGE ( 'NONE', *, *, #138287, .T. ) ;
#72142 = AXIS2_PLACEMENT_3D ( 'NONE', #33652, #110442, #53217 ) ;
#72143 = FILL_AREA_STYLE_COLOUR ( '', #107762 ) ;
#72144 = CARTESIAN_POINT ( 'NONE',  ( 9.436801032208231632, -12.74070752338415247, 9.898150129686353438 ) ) ;
#72145 = LINE ( 'NONE', #138804, #105747 ) ;
#72146 = CARTESIAN_POINT ( 'NONE',  ( 110.6208603837962272, -6.884901960086286188, 3.974999999999997424 ) ) ;
#72147 = CARTESIAN_POINT ( 'NONE',  ( 5.999999999999956479, 10.93112307739207267, 4.000000000000000000 ) ) ;
#72148 = EDGE_LOOP ( 'NONE', ( #118369, #110479, #4226, #65037 ) ) ;
#72149 = ORIENTED_EDGE ( 'NONE', *, *, #48553, .F. ) ;
#72150 = FACE_OUTER_BOUND ( 'NONE', #66864, .T. ) ;
#72151 = SURFACE_STYLE_FILL_AREA ( #115563 ) ;
#72152 = ORIENTED_EDGE ( 'NONE', *, *, #15007, .F. ) ;
#72153 = VECTOR ( 'NONE', #78210, 1000.000000000000227 ) ;
#72154 = ORIENTED_EDGE ( 'NONE', *, *, #2078, .T. ) ;
#72155 = VECTOR ( 'NONE', #16440, 1000.000000000000000 ) ;
#72156 = FACE_OUTER_BOUND ( 'NONE', #108764, .T. ) ;
#72157 = VERTEX_POINT ( 'NONE', #86300 ) ;
#72158 = AXIS2_PLACEMENT_3D ( 'NONE', #71289, #137965, #116907 ) ;
#72159 = DIRECTION ( 'NONE',  ( 0.6830127018922180770, -0.6830127018922204085, -0.2588190451025213501 ) ) ;
#72160 = PLANE ( 'NONE',  #95624 ) ;
#72161 = VECTOR ( 'NONE', #78854, 1000.000000000000000 ) ;
#72162 = FACE_BOUND ( 'NONE', #15211, .T. ) ;
#72163 = VECTOR ( 'NONE', #36383, 1000.000000000000000 ) ;
#72164 = DIRECTION ( 'NONE',  ( 1.000000000000000000, 0.000000000000000000, 0.000000000000000000 ) ) ;
#72165 = EDGE_CURVE ( 'NONE', #88478, #57179, #142115, .T. ) ;
#72166 = DIRECTION ( 'NONE',  ( 0.000000000000000000, 0.000000000000000000, 1.000000000000000000 ) ) ;
#72168 = ORIENTED_EDGE ( 'NONE', *, *, #1438, .F. ) ;
#72167 = DIRECTION ( 'NONE',  ( 0.000000000000000000, 0.000000000000000000, 1.000000000000000000 ) ) ;
#72169 = CARTESIAN_POINT ( 'NONE',  ( 0.000000000000000000, 0.000000000000000000, 5.000000000000000000 ) ) ;
#72170 = SHAPE_DEFINITION_REPRESENTATION ( #10783, #428 ) ;
#72171 = VERTEX_POINT ( 'NONE', #120292 ) ;
#72172 = EDGE_CURVE ( 'NONE', #9288, #41067, #31904, .T. ) ;
#72173 = EDGE_CURVE ( 'NONE', #76506, #117516, #7257, .T. ) ;
#72174 = EDGE_LOOP ( 'NONE', ( #134577, #107922, #6015 ) ) ;
#72175 = CARTESIAN_POINT ( 'NONE',  ( 90.18293019189812298, -1.637169565754158951, -6.109999999999998543 ) ) ;
#72176 = ORIENTED_EDGE ( 'NONE', *, *, #44024, .F. ) ;
#72177 = ADVANCED_FACE ( 'NONE', ( #95725 ), #84853, .T. ) ;
#72178 = CARTESIAN_POINT ( 'NONE',  ( 29.99999999999980815, 20.58746187583903264, 4.000000000000000000 ) ) ;
#72179 = EDGE_CURVE ( 'NONE', #109420, #98043, #77574, .T. ) ;
#72180 = AXIS2_PLACEMENT_3D ( 'NONE', #139340, #97180, #40030 ) ;
#72181 = CARTESIAN_POINT ( 'NONE',  ( 53.99451991528749062, 28.92564299267975869, 4.000000000000000000 ) ) ;
#72182 = AXIS2_PLACEMENT_3D ( 'NONE', #109649, #10324, #54579 ) ;
#72183 = EDGE_CURVE ( 'NONE', #21250, #99801, #76869, .T. ) ;
#72184 = CARTESIAN_POINT ( 'NONE',  ( -8.758305415748079525, 0.7592924766157104211, 14.37146558664984752 ) ) ;
#72185 = VERTEX_POINT ( 'NONE', #89148 ) ;
#72186 = CARTESIAN_POINT ( 'NONE',  ( 34.42499999999998295, 21.72500000000000142, 0.4999999999999995559 ) ) ;
#72187 = EDGE_CURVE ( 'NONE', #78583, #29685, #79006, .T. ) ;
#72188 = PLANE ( 'NONE',  #54707 ) ;
#72189 = EDGE_CURVE ( 'NONE', #68842, #124916, #680, .T. ) ;
#72190 = CARTESIAN_POINT ( 'NONE',  ( 0.000000000000000000, 0.000000000000000000, 5.000000000000000000 ) ) ;
#72192 = PLANE ( 'NONE',  #38098 ) ;
#72191 = CARTESIAN_POINT ( 'NONE',  ( -14.99451991528749595, 28.92564299267948513, 4.000000000000000000 ) ) ;
#72193 = LINE ( 'NONE', #62716, #9867 ) ;
#72194 = CARTESIAN_POINT ( 'NONE',  ( -25.39999999999996305, 0.000000000000000000, 0.000000000000000000 ) ) ;
#72195 = CIRCLE ( 'NONE', #14183, 2.055000000000000604 ) ;
#72196 = DIRECTION ( 'NONE',  ( 0.3543493200069162685, -0.000000000000000000, -0.9351131265310288487 ) ) ;
#72197 = EDGE_LOOP ( 'NONE', ( #96348, #66401, #124324, #24919 ) ) ;
#72198 = FACE_OUTER_BOUND ( 'NONE', #39024, .T. ) ;
#72199 = DIRECTION ( 'NONE',  ( -0.6830127018922181881, 0.6830127018922202975, -0.2588190451025214056 ) ) ;
#72200 = ADVANCED_FACE ( 'NONE', ( #35512 ), #122458, .F. ) ;
#72201 = VERTEX_POINT ( 'NONE', #78275 ) ;
#72202 = ORIENTED_EDGE ( 'NONE', *, *, #109756, .T. ) ;
#72203 = EDGE_CURVE ( 'NONE', #102270, #51451, #24584, .T. ) ;
#72204 = ORIENTED_EDGE ( 'NONE', *, *, #56853, .T. ) ;
#72205 = CARTESIAN_POINT ( 'NONE',  ( 42.87543019189810423, -5.291415217122920289, -3.055000000000001492 ) ) ;
#72206 = VECTOR ( 'NONE', #137854, 1000.000000000000000 ) ;
#72207 = ORIENTED_EDGE ( 'NONE', *, *, #99006, .T. ) ;
#72208 = EDGE_CURVE ( 'NONE', #36106, #10226, #34769, .T. ) ;
#72209 = CARTESIAN_POINT ( 'NONE',  ( 14.92080628287044064, 3.047499999999997655, 5.278424836066143655 ) ) ;
#72210 =( BOUNDED_CURVE ( )  B_SPLINE_CURVE ( 3, ( #75191, #64288, #18603, #131688 ),
 .UNSPECIFIED., .F., .T. ) 
 B_SPLINE_CURVE_WITH_KNOTS ( ( 4, 4 ),
 ( 5.106027341939297415, 6.645403452391245303 ),
 .UNSPECIFIED. ) 
 CURVE ( )  GEOMETRIC_REPRESENTATION_ITEM ( )  RATIONAL_B_SPLINE_CURVE ( ( 1.000000000000000000, 0.8120851936182316155, 0.8120851936182316155, 1.000000000000000000 ) ) 
 REPRESENTATION_ITEM ( '' )  );
#72211 = EDGE_LOOP ( 'NONE', ( #29319, #70618, #119926, #133036, #74430, #127738 ) ) ;
#72212 = PLANE ( 'NONE',  #3293 ) ;
#72213 = VERTEX_POINT ( 'NONE', #100024 ) ;
#72214 = CARTESIAN_POINT ( 'NONE',  ( -34.42500000000001137, 0.000000000000000000, 4.500000000000000888 ) ) ;
#72215 = FACE_OUTER_BOUND ( 'NONE', #9572, .T. ) ;
#72216 = AXIS2_PLACEMENT_3D ( 'NONE', #93939, #138173, #27978 ) ;
#72217 = VECTOR ( 'NONE', #108683, 1000.000000000000000 ) ;
#72219 = VERTEX_POINT ( 'NONE', #87707 ) ;
#72218 = FACE_OUTER_BOUND ( 'NONE', #120328, .T. ) ;
#72220 = ORIENTED_EDGE ( 'NONE', *, *, #95420, .T. ) ;
#72221 = DIRECTION ( 'NONE',  ( 0.000000000000000000, -1.000000000000000000, 0.000000000000000000 ) ) ;
#72222 = DIRECTION ( 'NONE',  ( 0.3543493200069162685, -0.000000000000000000, -0.9351131265310288487 ) ) ;
#72223 = VECTOR ( 'NONE', #9172, 1000.000000000000114 ) ;
#72225 = ORIENTED_EDGE ( 'NONE', *, *, #77218, .T. ) ;
#72224 = MECHANICAL_DESIGN_GEOMETRIC_PRESENTATION_REPRESENTATION (  '', ( #93081 ), #62995 ) ;
#72226 = DIRECTION ( 'NONE',  ( -0.7071067811865487940, 0.7071067811865463515, -0.000000000000000000 ) ) ;
#72227 = VERTEX_POINT ( 'NONE', #110845 ) ;
#72228 = ORIENTED_EDGE ( 'NONE', *, *, #83163, .F. ) ;
#72229 = EDGE_LOOP ( 'NONE', ( #140291, #89220, #23968, #35319 ) ) ;
#72230 = ORIENTED_EDGE ( 'NONE', *, *, #107743, .T. ) ;
#72231 = EDGE_CURVE ( 'NONE', #16928, #120251, #133373, .T. ) ;
#72232 = DIRECTION ( 'NONE',  ( -0.000000000000000000, 0.000000000000000000, 1.000000000000000000 ) ) ;
#72233 = VECTOR ( 'NONE', #41902, 1000.000000000000000 ) ;
#72234 = AXIS2_PLACEMENT_3D ( 'NONE', #112525, #82580, #34259 ) ;
#72235 = AXIS2_PLACEMENT_3D ( 'NONE', #19324, #9865, #109900 ) ;
#72236 = CARTESIAN_POINT ( 'NONE',  ( -7.499999999999944045, 3.073033219394612825, -6.593910359670984711 ) ) ;
#72237 = CARTESIAN_POINT ( 'NONE',  ( 21.04658813629531267, 14.25929247661557042, 18.84478104361322792 ) ) ;
#72238 = LINE ( 'NONE', #126546, #71782 ) ;
#72239 = ORIENTED_EDGE ( 'NONE', *, *, #25090, .F. ) ;
#72240 = CARTESIAN_POINT ( 'NONE',  ( 66.04166666666667140, -3.975000000000002753, 6.884901960086286188 ) ) ;
#72242 = VERTEX_POINT ( 'NONE', #55091 ) ;
#72241 = VECTOR ( 'NONE', #85627, 1000.000000000000227 ) ;
#72243 = DIRECTION ( 'NONE',  ( -0.7071067811865486830, 0.7071067811865464625, 0.000000000000000000 ) ) ;
#72244 = EDGE_CURVE ( 'NONE', #99187, #69646, #68151, .T. ) ;
#72245 = CARTESIAN_POINT ( 'NONE',  ( 32.64540314143522437, -2.126176841940958351, -7.934999999999989839 ) ) ;
#72246 = LINE ( 'NONE', #128028, #90184 ) ;
#72247 = DIRECTION ( 'NONE',  ( 0.7071067811865487940, 0.7071067811865463515, 0.000000000000000000 ) ) ;
#72248 = PLANE ( 'NONE',  #39698 ) ;
#72249 = ORIENTED_EDGE ( 'NONE', *, *, #127156, .T. ) ;
#72250 = ORIENTED_EDGE ( 'NONE', *, *, #126223, .T. ) ;
#72251 = ADVANCED_FACE ( 'NONE', ( #43492 ), #11538, .F. ) ;
#72252 = ORIENTED_EDGE ( 'NONE', *, *, #56322, .F. ) ;
#72253 = LINE ( 'NONE', #138177, #51022 ) ;
#72254 = DIRECTION ( 'NONE',  ( 0.000000000000000000, -0.3543493200069153248, -0.9351131265310292928 ) ) ;
#72255 = CARTESIAN_POINT ( 'NONE',  ( 2.994519915287485734, 28.92564299267940342, 4.000000000000000000 ) ) ;
#72256 = PLANE ( 'NONE',  #114515 ) ;
#72257 = CARTESIAN_POINT ( 'NONE',  ( 0.07239000078343528488, -48.13855614193185772, -37.56434003616170969 ) ) ;
#72258 = CARTESIAN_POINT ( 'NONE',  ( 73.70376352523145158, 6.109999999999999432, 1.122388791418549108E-15 ) ) ;
#72259 = AXIS2_PLACEMENT_3D ( 'NONE', #122964, #111350, #92441 ) ;
#72260 = CARTESIAN_POINT ( 'NONE',  ( 74.30836038379624142, 7.949999999999996625, 2.130196079827431088 ) ) ;
#72261 = VECTOR ( 'NONE', #87275, 999.9999999999998863 ) ;
#72262 = CARTESIAN_POINT ( 'NONE',  ( -48.29974487139158867, -27.71228299555239971, 4.000000000000000000 ) ) ;
#72263 = CARTESIAN_POINT ( 'NONE',  ( 1.499999999999990896, 6.431123077392122411, 4.000000000000000000 ) ) ;
#72264 = ADVANCED_FACE ( 'NONE', ( #131944 ), #67411, .F. ) ;
#72265 = CARTESIAN_POINT ( 'NONE',  ( -27.29974487139158512, -27.71228299555225405, 4.000000000000000000 ) ) ;
#72266 = AXIS2_PLACEMENT_3D ( 'NONE', #103687, #103013, #58122 ) ;
#72267 = LINE ( 'NONE', #28729, #41892 ) ;
#72268 = ORIENTED_EDGE ( 'NONE', *, *, #37292, .F. ) ;
#72270 = VECTOR ( 'NONE', #124132, 1000.000000000000000 ) ;
#72269 = DIRECTION ( 'NONE',  ( -0.6830127018922181881, 0.6830127018922202975, -0.2588190451025214056 ) ) ;
#72271 = ORIENTED_EDGE ( 'NONE', *, *, #87199, .F. ) ;
#72272 = FACE_OUTER_BOUND ( 'NONE', #118842, .T. ) ;
#72274 = EDGE_LOOP ( 'NONE', ( #98650, #72596, #598, #11884 ) ) ;
#72273 = CARTESIAN_POINT ( 'NONE',  ( -5.994519915287488843, 28.92564299267942118, 4.000000000000000000 ) ) ;
#72275 = EDGE_CURVE ( 'NONE', #59858, #90775, #125340, .T. ) ;
#72276 = CARTESIAN_POINT ( 'NONE',  ( -6.489213562373093325, -27.52281430457059841, 5.000000000000000000 ) ) ;
#72277 = DIRECTION ( 'NONE',  ( -0.6830127018922180770, 0.6830127018922202975, -0.2588190451025213501 ) ) ;
#72278 = ORIENTED_EDGE ( 'NONE', *, *, #33834, .T. ) ;
#72279 = ORIENTED_EDGE ( 'NONE', *, *, #115391, .T. ) ;
#72280 = DIRECTION ( 'NONE',  ( -0.7071067811865486830, -0.7071067811865464625, 0.000000000000000000 ) ) ;
#72281 = ORIENTED_EDGE ( 'NONE', *, *, #83559, .T. ) ;
#72282 = AXIS2_PLACEMENT_3D ( 'NONE', #123524, #100320, #68437 ) ;
#72283 = CARTESIAN_POINT ( 'NONE',  ( 5.277185695429377432, -21.72500000000000853, 5.000000000000000000 ) ) ;
#72284 =( BOUNDED_CURVE ( )  B_SPLINE_CURVE ( 2, ( #3895, #37295, #3214, #4588, #91667, #82249, #79424, #125009, #92359, #71359, #16211, #134479, #81542 ),
 .UNSPECIFIED., .F., .T. ) 
 B_SPLINE_CURVE_WITH_KNOTS ( ( 3, 2, 2, 2, 2, 2, 3 ),
 ( 0.08333333333333341197, 0.08611111111111116601, 0.08888888888888893391, 0.09166666666666667407, 0.09444444444444442810, 0.09722222222222219601, 0.09999999999999995004 ),
 .UNSPECIFIED. ) 
 CURVE ( )  GEOMETRIC_REPRESENTATION_ITEM ( )  RATIONAL_B_SPLINE_CURVE ( ( 0.9999999999999990008, 0.9659258262890693114, 1.000000000000000000, 0.9659258262890683122, 1.000000000000000000, 0.9659258262890683122, 1.000000000000000000, 0.9659258262890683122, 1.000000000000000000, 0.9659258262890683122, 1.000000000000000000, 0.9659258262890689783, 0.9999999999999993339 ) ) 
 REPRESENTATION_ITEM ( '' )  );
#72285 = CARTESIAN_POINT ( 'NONE',  ( 96.91252705046289861, -7.949999999999998401, -4.867971026610728450E-16 ) ) ;
#72286 = CARTESIAN_POINT ( 'NONE',  ( 71.29166666666667140, 3.975000000000003642, -6.884901960086285300 ) ) ;
#72287 = DIRECTION ( 'NONE',  ( -1.000000000000000000, 0.000000000000000000, 0.000000000000000000 ) ) ;
#72288 = EDGE_LOOP ( 'NONE', ( #46359, #142973, #20455, #31990 ) ) ;
#72289 = CARTESIAN_POINT ( 'NONE',  ( -15.48921356237309510, -27.52281430457066236, 5.000000000000000000 ) ) ;
#72290 = CARTESIAN_POINT ( 'NONE',  ( -29.99999999999980105, -19.06887692260762179, 4.000000000000000000 ) ) ;
#72292 = VECTOR ( 'NONE', #1283, 1000.000000000000000 ) ;
#72291 = CARTESIAN_POINT ( 'NONE',  ( 27.41666666666666785, 5.278424836066147208, 3.047499999999990550 ) ) ;
#72293 = FACE_OUTER_BOUND ( 'NONE', #102696, .T. ) ;
#72295 = VECTOR ( 'NONE', #21596, 1000.000000000000000 ) ;
#72294 = LINE ( 'NONE', #94682, #51433 ) ;
#72296 = EDGE_LOOP ( 'NONE', ( #17483, #17420, #94275, #116542 ) ) ;
#72297 = CARTESIAN_POINT ( 'NONE',  ( 11.25346039003969523, -2.055000000000000160, 0.000000000000000000 ) ) ;
#72298 = EDGE_LOOP ( 'NONE', ( #31846, #77428, #28513, #119912 ) ) ;
#72299 = EDGE_CURVE ( 'NONE', #56571, #69864, #59396, .T. ) ;
#72300 = CARTESIAN_POINT ( 'NONE',  ( 82.54209685856478984, 5.291415217122923842, -3.054999999999996163 ) ) ;
#72301 = LINE ( 'NONE', #25887, #36157 ) ;
#72303 = AXIS2_PLACEMENT_3D ( 'NONE', #57418, #113183, #56001 ) ;
#72302 = LINE ( 'NONE', #38209, #100227 ) ;
#72304 = DIRECTION ( 'NONE',  ( -0.7071067811865486830, -0.7071067811865464625, 0.000000000000000000 ) ) ;
#72305 = EDGE_LOOP ( 'NONE', ( #36305, #85904 ) ) ;
#72306 = LINE ( 'NONE', #82424, #65126 ) ;
#72307 = CARTESIAN_POINT ( 'NONE',  ( -30.18398860626900060, 28.73617430169808173, 5.000000000000000000 ) ) ;
#72308 = DIRECTION ( 'NONE',  ( -0.7071067811865486830, -0.7071067811865464625, 0.000000000000000000 ) ) ;
#72309 = ADVANCED_FACE ( 'NONE', ( #81868 ), #39034, .F. ) ;
#72311 = ORIENTED_EDGE ( 'NONE', *, *, #2924, .F. ) ;
#72310 = DIRECTION ( 'NONE',  ( 0.7071067811865486830, -0.7071067811865464625, -0.000000000000000000 ) ) ;
#72312 = DIRECTION ( 'NONE',  ( 0.6830127018922180770, -0.6830127018922204085, -0.2588190451025213501 ) ) ;
#72313 = CARTESIAN_POINT ( 'NONE',  ( -15.18398860626900237, 28.73617430169797871, 5.000000000000000000 ) ) ;
#72314 = AXIS2_PLACEMENT_3D ( 'NONE', #4780, #38202, #5527 ) ;
#72315 = DIRECTION ( 'NONE',  ( 0.7071067811865487940, 0.7071067811865463515, 0.000000000000000000 ) ) ;
#72316 = CARTESIAN_POINT ( 'NONE',  ( 25.39999999999999858, -18.48000000000005372, -34.92499999999998295 ) ) ;
#72317 = ORIENTED_EDGE ( 'NONE', *, *, #97764, .F. ) ;
#72318 = ORIENTED_EDGE ( 'NONE', *, *, #70653, .F. ) ;
#72319 = CARTESIAN_POINT ( 'NONE',  ( 75.39626352523141861, 4.472830434245840259, -4.472830434245839371 ) ) ;
#72320 = ORIENTED_EDGE ( 'NONE', *, *, #20389, .F. ) ;
#72321 = DIRECTION ( 'NONE',  ( 0.6830127018922181881, 0.6830127018922202975, -0.2588190451025214056 ) ) ;
#72322 = CARTESIAN_POINT ( 'NONE',  ( 23.68342038867195853, -6.740707523384216415, 11.88629033278118641 ) ) ;
#72323 = CARTESIAN_POINT ( 'NONE',  ( 13.82816939922343202, 9.759292476615623713, 4.000000000000000000 ) ) ;
#72324 = ORIENTED_EDGE ( 'NONE', *, *, #87394, .F. ) ;
#72325 =( GEOMETRIC_REPRESENTATION_CONTEXT ( 3 ) GLOBAL_UNCERTAINTY_ASSIGNED_CONTEXT ( ( #130196 ) ) GLOBAL_UNIT_ASSIGNED_CONTEXT ( ( #96070, #46768, #12638 ) ) REPRESENTATION_CONTEXT ( 'NONE', 'WORKASPACE' ) );
#72326 = VECTOR ( 'NONE', #119238, 1000.000000000000000 ) ;
#72327 = VECTOR ( 'NONE', #128281, 1000.000000000000000 ) ;
#72328 = DIRECTION ( 'NONE',  ( 1.000000000000000000, 0.000000000000000000, 0.000000000000000000 ) ) ;
#72329 = LINE ( 'NONE', #115030, #69844 ) ;
#72330 = CONICAL_SURFACE ( 'NONE', #141729, 2.500000000000000444, 0.9599310885968830309 ) ;
#72331 = ORIENTED_EDGE ( 'NONE', *, *, #33834, .F. ) ;
#72332 = LINE ( 'NONE', #127367, #44300 ) ;
#72334 = CARTESIAN_POINT ( 'NONE',  ( 184.1500000000000057, -14.29000000000013593, -12.70000000000045404 ) ) ;
#72333 = VECTOR ( 'NONE', #112196, 1000.000000000000000 ) ;
#72335 = CARTESIAN_POINT ( 'NONE',  ( 72.29974487139158157, -27.71228299555256669, 4.000000000000000000 ) ) ;
#72336 = VECTOR ( 'NONE', #6743, 1000.000000000000227 ) ;
#72337 = VECTOR ( 'NONE', #59138, 1000.000000000000000 ) ;
#72338 = VERTEX_POINT ( 'NONE', #26027 ) ;
#72339 = EDGE_LOOP ( 'NONE', ( #66610, #13960, #85760, #50116 ) ) ;
#72340 = CARTESIAN_POINT ( 'NONE',  ( 0.000000000000000000, 0.000000000000000000, 10.00000000000000000 ) ) ;
#72342 = CARTESIAN_POINT ( 'NONE',  ( -5.999999999999954703, -19.22509904557637128, 1.855685503482163767 ) ) ;
#72341 = B_SPLINE_CURVE_WITH_KNOTS ( 'NONE', 3,
 ( #26270, #94361, #70533, #105245 ),
 .UNSPECIFIED., .F., .F.,
 ( 4, 4 ),
 ( 0.008519363277820955760, 0.008755597426397563471 ),
 .UNSPECIFIED. ) ;
#72343 = CARTESIAN_POINT ( 'NONE',  ( -31.17183060077625356, 12.75929247661558819, 4.000000000000000000 ) ) ;
#72344 = DIRECTION ( 'NONE',  ( -0.7071067811865486830, -0.7071067811865464625, -0.000000000000000000 ) ) ;
#72345 = FACE_OUTER_BOUND ( 'NONE', #58257, .T. ) ;
#72346 = CARTESIAN_POINT ( 'NONE',  ( -9.851816449618491234, 17.25929247661554200, 8.802941693769181342 ) ) ;
#72347 = ORIENTED_EDGE ( 'NONE', *, *, #127110, .F. ) ;
#72348 = EDGE_CURVE ( 'NONE', #53474, #53240, #36878, .T. ) ;
#72349 = VERTEX_POINT ( 'NONE', #115126 ) ;
#72350 = ORIENTED_EDGE ( 'NONE', *, *, #22362, .T. ) ;
#72351 = EDGE_CURVE ( 'NONE', #121175, #107840, #58712, .T. ) ;
#72352 = ORIENTED_EDGE ( 'NONE', *, *, #143117, .F. ) ;
#72353 = EDGE_CURVE ( 'NONE', #46724, #108692, #103554, .T. ) ;
#72354 = ADVANCED_FACE ( 'NONE', ( #102879 ), #127466, .F. ) ;
#72355 = FACE_OUTER_BOUND ( 'NONE', #114691, .T. ) ;
#72356 = EDGE_LOOP ( 'NONE', ( #113652, #118631, #26277, #10639 ) ) ;
#72357 = DIRECTION ( 'NONE',  ( 0.6830127018922180770, -0.6830127018922204085, -0.2588190451025213501 ) ) ;
#72358 = LINE ( 'NONE', #50556, #19382 ) ;
#72359 = AXIS2_PLACEMENT_3D ( 'NONE', #17770, #138162, #127263 ) ;
#72360 = PLANE ( 'NONE',  #15518 ) ;
#72361 = CARTESIAN_POINT ( 'NONE',  ( 34.49999999999975842, 13.56627193232217898, -10.57019076586060713 ) ) ;
#72362 = VECTOR ( 'NONE', #106629, 1000.000000000000000 ) ;
#72363 = CARTESIAN_POINT ( 'NONE',  ( 26.99999999999981881, -7.447814304570752775, 5.000000000000000000 ) ) ;
#72364 = ORIENTED_EDGE ( 'NONE', *, *, #9778, .T. ) ;
#72365 = DIRECTION ( 'NONE',  ( -1.000000000000000000, -1.224606353822377258E-16, -0.000000000000000000 ) ) ;
#72366 = FACE_OUTER_BOUND ( 'NONE', #134277, .T. ) ;
#72367 = EDGE_CURVE ( 'NONE', #129026, #73447, #48480, .T. ) ;
#72368 = EDGE_LOOP ( 'NONE', ( #56694, #34559, #123857, #55128 ) ) ;
#72369 = CARTESIAN_POINT ( 'NONE',  ( 31.49999999999978684, 15.05218569542901186, 5.000000000000000000 ) ) ;
#72370 = ORIENTED_EDGE ( 'NONE', *, *, #34211, .F. ) ;
#72371 = EDGE_CURVE ( 'NONE', #117002, #88966, #15114, .T. ) ;
#72372 = ORIENTED_EDGE ( 'NONE', *, *, #16222, .T. ) ;
#72373 = CARTESIAN_POINT ( 'NONE',  ( 4.969723521325230209, 4.202752102959690472E-16, 0.000000000000000000 ) ) ;
#72374 = ORIENTED_EDGE ( 'NONE', *, *, #64819, .T. ) ;
#72375 = ORIENTED_EDGE ( 'NONE', *, *, #9444, .T. ) ;
#72376 = CARTESIAN_POINT ( 'NONE',  ( 73.06293019189810423, 1.637169565754157174, 6.110000000000002984 ) ) ;
#72377 = ORIENTED_EDGE ( 'NONE', *, *, #76749, .F. ) ;
#72378 = EDGE_CURVE ( 'NONE', #129071, #56327, #113012, .T. ) ;
#72379 = DIRECTION ( 'NONE',  ( -0.3543493200069163240, 0.000000000000000000, 0.9351131265310288487 ) ) ;
#72380 = DIRECTION ( 'NONE',  ( -4.681814790819591790E-17, -0.3543493200069152693, 0.9351131265310292928 ) ) ;
#72381 = CARTESIAN_POINT ( 'NONE',  ( 109.3754301918981042, -5.291415217122920289, -3.055000000000001492 ) ) ;
#72382 = DIRECTION ( 'NONE',  ( 1.000000000000000000, 1.224606353822377258E-16, 0.000000000000000000 ) ) ;
#72384 = CARTESIAN_POINT ( 'NONE',  ( 5.671830600776426756, -21.74070752338406365, 4.000000000000000000 ) ) ;
#72383 = AXIS2_PLACEMENT_3D ( 'NONE', #138253, #127362, #72328 ) ;
#72385 = LINE ( 'NONE', #128163, #118091 ) ;
#72386 = EDGE_CURVE ( 'NONE', #47983, #90340, #71675, .T. ) ;
#72387 = PLANE ( 'NONE',  #29067 ) ;
#72388 = AXIS2_PLACEMENT_3D ( 'NONE', #12125, #101288, #1927 ) ;
#72389 = PLANE ( 'NONE',  #14558 ) ;
#72390 = DIRECTION ( 'NONE',  ( -0.7071067811865486830, -0.7071067811865464625, 0.000000000000000000 ) ) ;
#72391 = CARTESIAN_POINT ( 'NONE',  ( -9.183988606268997046, 28.73617430169793607, 5.000000000000000000 ) ) ;
#72392 = ORIENTED_EDGE ( 'NONE', *, *, #72351, .T. ) ;
#72393 = ORIENTED_EDGE ( 'NONE', *, *, #111713, .F. ) ;
#72394 = ORIENTED_EDGE ( 'NONE', *, *, #86610, .F. ) ;
#72395 = EDGE_CURVE ( 'NONE', #76403, #1315, #92683, .T. ) ;
#72396 = CARTESIAN_POINT ( 'NONE',  ( 114.4125270504628986, -7.949999999999998401, -4.867971026610728450E-16 ) ) ;
#72398 = ORIENTED_EDGE ( 'NONE', *, *, #130577, .F. ) ;
#72397 = CIRCLE ( 'NONE', #83974, 1.898649999999993065 ) ;
#72399 = CARTESIAN_POINT ( 'NONE',  ( -6.328169399223483538, 2.259292476615696099, 4.000000000000000000 ) ) ;
#72400 = DIRECTION ( 'NONE',  ( -0.000000000000000000, 0.000000000000000000, 1.000000000000000000 ) ) ;
#72401 = CARTESIAN_POINT ( 'NONE',  ( -34.92499999999997584, -6.270000000000012008, -37.00000000000000000 ) ) ;
#72402 = DIRECTION ( 'NONE',  ( 0.7071067811865486830, -0.7071067811865464625, -0.000000000000000000 ) ) ;
#72403 = ORIENTED_EDGE ( 'NONE', *, *, #30602, .T. ) ;
#72404 = CARTESIAN_POINT ( 'NONE',  ( 0.6686314397422480349, -52.14999999947626463, 41.03936837847535912 ) ) ;
#72405 = AXIS2_PLACEMENT_3D ( 'NONE', #131998, #89201, #64585 ) ;
#72406 = ORIENTED_EDGE ( 'NONE', *, *, #103086, .F. ) ;
#72407 = EDGE_CURVE ( 'NONE', #80487, #118264, #126062, .T. ) ;
#72408 = CARTESIAN_POINT ( 'NONE',  ( 4.937069808101886004, 2.126176841940952134, -7.934999999999993392 ) ) ;
#72409 = DIRECTION ( 'NONE',  ( -0.5735764363510503783, -0.8191520442889886899, 0.000000000000000000 ) ) ;
#72410 = CARTESIAN_POINT ( 'NONE',  ( 0.000000000000000000, 21.72500000000000142, 4.500000000000000888 ) ) ;
#72411 = CARTESIAN_POINT ( 'NONE',  ( 10.61499488414559700, -8.432637487761464712, 4.375000000000002665 ) ) ;
#72412 = VERTEX_POINT ( 'NONE', #136202 ) ;
#72413 = ORIENTED_EDGE ( 'NONE', *, *, #102624, .F. ) ;
#72414 = ORIENTED_EDGE ( 'NONE', *, *, #101343, .T. ) ;
#72415 = LINE ( 'NONE', #105679, #9259 ) ;
#72416 = CARTESIAN_POINT ( 'NONE',  ( -2.816011393730999401, 28.73617430169785436, 5.000000000000000000 ) ) ;
#72418 = LINE ( 'NONE', #120668, #17262 ) ;
#72417 = CIRCLE ( 'NONE', #19181, 2.500000000000000444 ) ;
#72419 = VECTOR ( 'NONE', #70563, 1000.000000000000000 ) ;
#72420 = CARTESIAN_POINT ( 'NONE',  ( -18.48921356237309510, -27.52281430457068367, 5.000000000000000000 ) ) ;
#72421 = CIRCLE ( 'NONE', #83905, 2.500000000000000444 ) ;
#72422 = CARTESIAN_POINT ( 'NONE',  ( 0.000000000000000000, 0.000000000000000000, 5.000000000000000000 ) ) ;
#72423 = COLOUR_RGB ( '', 0.66274510, 0.83137255, 0.94901961) ;
#72424 = CARTESIAN_POINT ( 'NONE',  ( 66.48921356237309510, -27.52281430457101763, 5.000000000000000000 ) ) ;
#72425 = EDGE_CURVE ( 'NONE', #41011, #141528, #14435, .T. ) ;
#72426 = CARTESIAN_POINT ( 'NONE',  ( 21.18398860626899349, 28.73617430169802134, 5.000000000000000000 ) ) ;
#72427 = CARTESIAN_POINT ( 'NONE',  ( 24.70710678118637205, -6.740707523384214639, 5.000000000000000000 ) ) ;
#72428 = ORIENTED_EDGE ( 'NONE', *, *, #100140, .F. ) ;
#72429 = DIRECTION ( 'NONE',  ( 0.000000000000000000, 0.7453559924999330066, 0.6666666666666630769 ) ) ;
#72430 = VECTOR ( 'NONE', #131283, 1000.000000000000227 ) ;
#72431 = VECTOR ( 'NONE', #121613, 1000.000000000000000 ) ;
#72432 = DIRECTION ( 'NONE',  ( 0.7071067811865487940, 0.7071067811865463515, 0.000000000000000000 ) ) ;
#72433 = ORIENTED_EDGE ( 'NONE', *, *, #103436, .F. ) ;
#72434 = CARTESIAN_POINT ( 'NONE',  ( -19.49999999999985079, 16.08746187583907528, 4.000000000000000000 ) ) ;
#72436 = ORIENTED_EDGE ( 'NONE', *, *, #127583, .T. ) ;
#72435 = CARTESIAN_POINT ( 'NONE',  ( 55.71344734891371075, -51.77943056867386673, -39.18578444878554734 ) ) ;
#72437 = ADVANCED_FACE ( 'NONE', ( #115842 ), #136919, .F. ) ;
#72438 = LINE ( 'NONE', #137666, #37615 ) ;
#72439 = CARTESIAN_POINT ( 'NONE',  ( 105.2708333333333428, -7.949999999999998401, -2.130196079827426203 ) ) ;
#72440 = VERTEX_POINT ( 'NONE', #2827 ) ;
#72441 =( NAMED_UNIT ( * ) SI_UNIT ( $, .STERADIAN. ) SOLID_ANGLE_UNIT ( ) );
#72442 = UNCERTAINTY_MEASURE_WITH_UNIT (LENGTH_MEASURE( 1.000000000000000082E-05 ), #34641, 'distance_accuracy_value', 'NONE');
#72443 = ORIENTED_EDGE ( 'NONE', *, *, #3721, .F. ) ;
#72444 = DIRECTION ( 'NONE',  ( -0.7071067811865486830, -0.7071067811865464625, 0.000000000000000000 ) ) ;
#72445 = CARTESIAN_POINT ( 'NONE',  ( 125.6416937171295700, -2.130196079827424871, -7.949999999999999289 ) ) ;
#72446 = FACE_OUTER_BOUND ( 'NONE', #126117, .T. ) ;
#72447 = VECTOR ( 'NONE', #133734, 1000.000000000000000 ) ;
#72448 = DIRECTION ( 'NONE',  ( 0.7071067811865486830, -0.7071067811865464625, -0.000000000000000000 ) ) ;
#72449 = LINE ( 'NONE', #6371, #51453 ) ;
#72450 = CARTESIAN_POINT ( 'NONE',  ( -1.499999999999982236, -1.912538124160737318, 4.000000000000000000 ) ) ;
#72451 = DIRECTION ( 'NONE',  ( 0.000000000000000000, -1.000000000000000000, 0.000000000000000000 ) ) ;
#72452 = CARTESIAN_POINT ( 'NONE',  ( 26.37456980810188867, 6.871911579029510442, -3.967499999999998916 ) ) ;
#72453 = CARTESIAN_POINT ( 'NONE',  ( 3.916236474768552522, -7.934999999999990727, 4.858786175617117713E-16 ) ) ;
#72454 = DIRECTION ( 'NONE',  ( 0.7071067811865486830, -0.7071067811865464625, -0.000000000000000000 ) ) ;
#72455 = CARTESIAN_POINT ( 'NONE',  ( -9.183988606268997046, 28.73617430169793607, 5.000000000000000000 ) ) ;
#72456 = CYLINDRICAL_SURFACE ( 'NONE', #38600, 2.500000000000000000 ) ;
#72457 = ORIENTED_EDGE ( 'NONE', *, *, #85182, .F. ) ;
#72458 = ORIENTED_EDGE ( 'NONE', *, *, #96662, .F. ) ;
#72459 = CARTESIAN_POINT ( 'NONE',  ( 80.77083333333331439, -7.949999999999999289, -2.130196079827426203 ) ) ;
#72460 = DIRECTION ( 'NONE',  ( 0.5735764363510451602, 0.8191520442889924647, 0.000000000000000000 ) ) ;
#72461 = ORIENTED_EDGE ( 'NONE', *, *, #115502, .F. ) ;
#72462 = PRODUCT ( '1.0 Base', '1.0 Base', '', ( #93870 ) ) ;
#72463 = EDGE_CURVE ( 'NONE', #43580, #142125, #93419, .T. ) ;
#72464 = MECHANICAL_DESIGN_GEOMETRIC_PRESENTATION_REPRESENTATION (  '', ( #58615 ), #14562 ) ;
#72465 = DIRECTION ( 'NONE',  ( -1.000000000000000000, 0.000000000000000000, 0.000000000000000000 ) ) ;
#72466 = CARTESIAN_POINT ( 'NONE',  ( 22.99806943317885199, -22.22500000000000142, 4.500000000000000888 ) ) ;
#72467 = VECTOR ( 'NONE', #110392, 1000.000000000000000 ) ;
#72468 = VECTOR ( 'NONE', #107729, 1000.000000000000000 ) ;
#72469 = CARTESIAN_POINT ( 'NONE',  ( 18.79289321881333308, -11.24070752338417023, 5.000000000000000000 ) ) ;
#72470 = ORIENTED_EDGE ( 'NONE', *, *, #93080, .T. ) ;
#72471 = CARTESIAN_POINT ( 'NONE',  ( -75.18398860626899705, 28.73617430169839793, 5.000000000000000000 ) ) ;
#72472 = LINE ( 'NONE', #116637, #37164 ) ;
#72473 = LINE ( 'NONE', #60886, #74170 ) ;
#72474 = CARTESIAN_POINT ( 'NONE',  ( 21.29974487139158512, -27.71228299555221142, 4.000000000000000000 ) ) ;
#72475 = EDGE_CURVE ( 'NONE', #13343, #103863, #5665, .T. ) ;
#72476 = EDGE_CURVE ( 'NONE', #88862, #22212, #135513, .T. ) ;
#72477 = CARTESIAN_POINT ( 'NONE',  ( -5.816011393731002066, 28.73617430169783304, 5.000000000000000000 ) ) ;
#72478 = CARTESIAN_POINT ( 'NONE',  ( 17.99451991528748351, 28.92564299267950645, 4.000000000000000000 ) ) ;
#72479 = DIRECTION ( 'NONE',  ( 0.6830127018922180770, -0.6830127018922204085, -0.2588190451025213501 ) ) ;
#72480 = CARTESIAN_POINT ( 'NONE',  ( -19.62823445044373116, -8.240707523384196875, 11.38925528200757142 ) ) ;
#72481 = LINE ( 'NONE', #48545, #112778 ) ;
#72482 = DIRECTION ( 'NONE',  ( -0.7071067811865486830, -0.7071067811865464625, 0.000000000000000000 ) ) ;
#72483 = CARTESIAN_POINT ( 'NONE',  ( 4.499999999999972466, -2.173586137069131841, -4.605770156576102003 ) ) ;
#72484 = VECTOR ( 'NONE', #89846, 1000.000000000000227 ) ;
#72485 = ORIENTED_EDGE ( 'NONE', *, *, #115359, .F. ) ;
#72486 = ORIENTED_EDGE ( 'NONE', *, *, #102732, .T. ) ;
#72487 = CARTESIAN_POINT ( 'NONE',  ( 102.0837635252314328, -6.110000000000001208, -3.741295971395164515E-16 ) ) ;
#72488 = ORIENTED_EDGE ( 'NONE', *, *, #79145, .F. ) ;
#72489 = VECTOR ( 'NONE', #124179, 1000.000000000000000 ) ;
#72490 = FACE_OUTER_BOUND ( 'NONE', #65067, .T. ) ;
#72491 = VECTOR ( 'NONE', #46443, 1000.000000000000227 ) ;
#72492 = DIRECTION ( 'NONE',  ( -0.3543493200069162685, -0.000000000000000000, -0.9351131265310288487 ) ) ;
#72493 = ORIENTED_EDGE ( 'NONE', *, *, #46465, .T. ) ;
#72494 = EDGE_CURVE ( 'NONE', #79059, #132154, #86834, .T. ) ;
#72495 = PLANE ( 'NONE',  #7425 ) ;
#72497 =( BOUNDED_CURVE ( )  B_SPLINE_CURVE ( 3, ( #10548, #384, #57677, #134509 ),
 .UNSPECIFIED., .F., .F. ) 
 B_SPLINE_CURVE_WITH_KNOTS ( ( 4, 4 ),
 ( 5.005968288816720069, 5.074607125596358514 ),
 .UNSPECIFIED. ) 
 CURVE ( )  GEOMETRIC_REPRESENTATION_ITEM ( )  RATIONAL_B_SPLINE_CURVE ( ( 1.000000000000000000, 0.9996074310407762065, 0.9996074310407762065, 1.000000000000000000 ) ) 
 REPRESENTATION_ITEM ( '' )  );
#72496 = FACE_OUTER_BOUND ( 'NONE', #85926, .T. ) ;
#72498 = CARTESIAN_POINT ( 'NONE',  ( 102.1412635252314232, 4.472830434245836706, 4.472830434245840259 ) ) ;
#72499 = ORIENTED_EDGE ( 'NONE', *, *, #87092, .T. ) ;
#72500 = DIRECTION ( 'NONE',  ( -0.7071067811865486830, -0.7071067811865464625, 0.000000000000000000 ) ) ;
#72501 = EDGE_LOOP ( 'NONE', ( #76811, #12310, #82550, #47161, #80945 ) ) ;
#72502 = CARTESIAN_POINT ( 'NONE',  ( 8.241399257801971245, 21.72500000000000142, 5.000000000000000000 ) ) ;
#72503 = VECTOR ( 'NONE', #109187, 1000.000000000000000 ) ;
#72504 = CARTESIAN_POINT ( 'NONE',  ( 22.49999999999984723, 15.05218569542901541, 5.000000000000000000 ) ) ;
#72505 = CARTESIAN_POINT ( 'NONE',  ( -45.29974487139158867, -27.71228299555237840, 4.000000000000000000 ) ) ;
#72506 =( BOUNDED_CURVE ( )  B_SPLINE_CURVE ( 3, ( #1924, #2669, #102006, #34610 ),
 .UNSPECIFIED., .F., .T. ) 
 B_SPLINE_CURVE_WITH_KNOTS ( ( 4, 4 ),
 ( 2.280733380739273564, 2.329266631601944137 ),
 .UNSPECIFIED. ) 
 CURVE ( )  GEOMETRIC_REPRESENTATION_ITEM ( )  RATIONAL_B_SPLINE_CURVE ( ( 1.000000000000000000, 0.9998037199289477872, 0.9998037199289477872, 1.000000000000000000 ) ) 
 REPRESENTATION_ITEM ( '' )  );
#72507 = LINE ( 'NONE', #113273, #22996 ) ;
#72508 = VERTEX_POINT ( 'NONE', #61540 ) ;
#72509 = ORIENTED_EDGE ( 'NONE', *, *, #83795, .T. ) ;
#72510 = ORIENTED_EDGE ( 'NONE', *, *, #116834, .F. ) ;
#72511 = CARTESIAN_POINT ( 'NONE',  ( -24.70057660522904897, 5.105512181938189009, 4.576947331497495774 ) ) ;
#72512 = CARTESIAN_POINT ( 'NONE',  ( 66.48921356237309510, -27.52281430457101763, 5.000000000000000000 ) ) ;
#72513 = CARTESIAN_POINT ( 'NONE',  ( 12.75456980810188767, -6.871911579029512218, 3.967499999999996252 ) ) ;
#72514 = VECTOR ( 'NONE', #89043, 1000.000000000000000 ) ;
#72515 = LINE ( 'NONE', #19503, #1586 ) ;
#72516 = ADVANCED_FACE ( 'NONE', ( #74541 ), #118725, .T. ) ;
#72517 = ORIENTED_EDGE ( 'NONE', *, *, #93795, .F. ) ;
#72518 = ORIENTED_EDGE ( 'NONE', *, *, #26560, .F. ) ;
#72519 = EDGE_CURVE ( 'NONE', #71568, #8795, #119419, .T. ) ;
#72520 = PLANE ( 'NONE',  #66529 ) ;
#72521 = EDGE_LOOP ( 'NONE', ( #100034, #114181, #40273, #28352 ) ) ;
#72522 = VERTEX_POINT ( 'NONE', #28164 ) ;
#72523 = VECTOR ( 'NONE', #31205, 999.9999999999998863 ) ;
#72524 = EDGE_CURVE ( 'NONE', #81146, #63415, #39778, .T. ) ;
#72526 = EDGE_CURVE ( 'NONE', #43949, #87685, #96939, .T. ) ;
#72525 = VECTOR ( 'NONE', #96567, 1000.000000000000000 ) ;
#72527 = CARTESIAN_POINT ( 'NONE',  ( 114.2454301918981230, -5.291415217122918513, -3.055000000000000160 ) ) ;
#72528 = VECTOR ( 'NONE', #115428, 1000.000000000000000 ) ;
#72529 = DIRECTION ( 'NONE',  ( -0.7071067811865487940, 0.7071067811865463515, -0.000000000000000000 ) ) ;
#72530 = DIRECTION ( 'NONE',  ( -0.6830127018922180770, -0.6830127018922204085, -0.2588190451025213501 ) ) ;
#72531 = ORIENTED_EDGE ( 'NONE', *, *, #118737, .F. ) ;
#72532 = DIRECTION ( 'NONE',  ( 0.7071067811865487940, 0.7071067811865463515, 0.000000000000000000 ) ) ;
#72534 = CARTESIAN_POINT ( 'NONE',  ( 2.510786437626908008, -27.52281430457053446, 5.000000000000000000 ) ) ;
#72533 = CONICAL_SURFACE ( 'NONE', #91038, 1.142820323027522456, 0.2617993877991512952 ) ;
#72535 = AXIS2_PLACEMENT_3D ( 'NONE', #124367, #25034, #12016 ) ;
#72536 = DIRECTION ( 'NONE',  ( -0.000000000000000000, 0.000000000000000000, 1.000000000000000000 ) ) ;
#72537 = CARTESIAN_POINT ( 'NONE',  ( 30.66846741159838530, -18.74070752338408852, 20.73178291233848469 ) ) ;
#72538 = EDGE_LOOP ( 'NONE', ( #79805, #140185, #53974, #120623 ) ) ;
#72539 = LINE ( 'NONE', #125449, #39500 ) ;
#72540 = CARTESIAN_POINT ( 'NONE',  ( 19.41999999999999815, 9.521314400968980422E-16, 0.000000000000000000 ) ) ;
#72541 = ADVANCED_FACE ( 'NONE', ( #41167 ), #105687, .F. ) ;
#72542 = ORIENTED_EDGE ( 'NONE', *, *, #47458, .F. ) ;
#72543 = CARTESIAN_POINT ( 'NONE',  ( 25.39999999999998792, -2.682872131610448907, -7.478867202222028610 ) ) ;
#72544 = CARTESIAN_POINT ( 'NONE',  ( 27.06011071044003202, -9.740707523384184441, 10.89222023123374505 ) ) ;
#72545 = LINE ( 'NONE', #36996, #7471 ) ;
#72546 = ADVANCED_FACE ( 'NONE', ( #7073 ), #129593, .F. ) ;
#72547 = ORIENTED_EDGE ( 'NONE', *, *, #53533, .T. ) ;
#72548 = CARTESIAN_POINT ( 'NONE',  ( -12.29974487139158512, -27.71228299555214747, 4.000000000000000000 ) ) ;
#72549 = VERTEX_POINT ( 'NONE', #62234 ) ;
#72550 = ORIENTED_EDGE ( 'NONE', *, *, #62155, .F. ) ;
#72551 = ORIENTED_EDGE ( 'NONE', *, *, #100523, .T. ) ;
#72552 = CARTESIAN_POINT ( 'NONE',  ( 32.87043019189811588, -3.055000000000001492, 5.291415217122917625 ) ) ;
#72553 = ORIENTED_EDGE ( 'NONE', *, *, #88229, .F. ) ;
#72554 = AXIS2_PLACEMENT_3D ( 'NONE', #89331, #21924, #45853 ) ;
#72555 = EDGE_CURVE ( 'NONE', #63684, #140803, #19419, .T. ) ;
#72556 = FACE_OUTER_BOUND ( 'NONE', #44964, .T. ) ;
#72557 = CARTESIAN_POINT ( 'NONE',  ( 8.000000000000007105, 1.465179874765178344E-16, -1.142820323027522456 ) ) ;
#72558 = CARTESIAN_POINT ( 'NONE',  ( -34.47516574401891631, -2.971932658884152367, 4.998110765256834398 ) ) ;
#72559 = CARTESIAN_POINT ( 'NONE',  ( -18.29974487139159223, -27.71228299555219010, 4.000000000000000000 ) ) ;
#72560 = DIRECTION ( 'NONE',  ( -0.6830127018922180770, -0.6830127018922204085, -0.2588190451025213501 ) ) ;
#72561 = CARTESIAN_POINT ( 'NONE',  ( -69.48921356237309510, -27.52281430457103895, 5.000000000000000000 ) ) ;
#72562 = EDGE_CURVE ( 'NONE', #6240, #82809, #140368, .T. ) ;
#72564 = CARTESIAN_POINT ( 'NONE',  ( -45.29974487139158867, -27.71228299555237840, 4.000000000000000000 ) ) ;
#72563 = VECTOR ( 'NONE', #90346, 1000.000000000000000 ) ;
#72565 = LINE ( 'NONE', #82001, #99202 ) ;
#72566 = DIRECTION ( 'NONE',  ( -0.3543493200069162685, -0.000000000000000000, -0.9351131265310288487 ) ) ;
#72567 = AXIS2_PLACEMENT_3D ( 'NONE', #39392, #126373, #83624 ) ;
#72568 = CARTESIAN_POINT ( 'NONE',  ( 0.4892135623730947680, -27.52281430457055578, 5.000000000000000000 ) ) ;
#72569 = ORIENTED_EDGE ( 'NONE', *, *, #54184, .F. ) ;
#72570 = ORIENTED_EDGE ( 'NONE', *, *, #111778, .T. ) ;
#72572 = ORIENTED_EDGE ( 'NONE', *, *, #53098, .T. ) ;
#72571 = ADVANCED_FACE ( 'NONE', ( #8497 ), #107135, .F. ) ;
#72573 = ORIENTED_EDGE ( 'NONE', *, *, #10159, .F. ) ;
#72574 = CARTESIAN_POINT ( 'NONE',  ( -1.055977286261792880, 0.8118917398807320440, 3.860134494607520672 ) ) ;
#72575 = ORIENTED_EDGE ( 'NONE', *, *, #65211, .F. ) ;
#72576 = VECTOR ( 'NONE', #69345, 1000.000000000000000 ) ;
#72577 = ORIENTED_EDGE ( 'NONE', *, *, #65335, .F. ) ;
#72578 = CARTESIAN_POINT ( 'NONE',  ( 26.99451991528749417, 28.92564299267956685, 4.000000000000000000 ) ) ;
#72579 = FACE_OUTER_BOUND ( 'NONE', #27797, .T. ) ;
#72580 = EDGE_CURVE ( 'NONE', #117925, #13143, #31033, .T. ) ;
#72581 = ORIENTED_EDGE ( 'NONE', *, *, #52881, .T. ) ;
#72582 = EDGE_CURVE ( 'NONE', #38491, #77870, #67974, .T. ) ;
#72583 = CARTESIAN_POINT ( 'NONE',  ( 21.71715331601274102, -2.164967620583693630, 5.000000000000000000 ) ) ;
#72584 = ORIENTED_EDGE ( 'NONE', *, *, #28800, .F. ) ;
#72586 = VECTOR ( 'NONE', #15564, 1000.000000000000000 ) ;
#72585 = CARTESIAN_POINT ( 'NONE',  ( -5.999999999999956479, -6.108550654416966097, -3.114665004254979941 ) ) ;
#72587 = EDGE_CURVE ( 'NONE', #32455, #75311, #143338, .T. ) ;
#72588 = DIRECTION ( 'NONE',  ( -0.5735764363510501562, 0.8191520442889890230, 1.003171929053521419E-16 ) ) ;
#72589 = AXIS2_PLACEMENT_3D ( 'NONE', #28706, #4726, #72243 ) ;
#72590 = CARTESIAN_POINT ( 'NONE',  ( 11.44206980810188767, 7.934999999999993392, 2.126176841940951689 ) ) ;
#72591 = ORIENTED_EDGE ( 'NONE', *, *, #36713, .T. ) ;
#72593 = FACE_OUTER_BOUND ( 'NONE', #46804, .T. ) ;
#72592 = CARTESIAN_POINT ( 'NONE',  ( 102.4329301918980946, 1.637169565754156730, 6.110000000000001208 ) ) ;
#72594 = CARTESIAN_POINT ( 'NONE',  ( 55.56056557994604361, -52.00875322212549179, -39.86617647058817937 ) ) ;
#72595 = DIRECTION ( 'NONE',  ( 0.6830127018922181881, 0.6830127018922202975, -0.2588190451025214056 ) ) ;
#72596 = ORIENTED_EDGE ( 'NONE', *, *, #48156, .T. ) ;
#72597 = VERTEX_POINT ( 'NONE', #21572 ) ;
#72598 = ORIENTED_EDGE ( 'NONE', *, *, #86707, .F. ) ;
#72600 = AXIS2_PLACEMENT_3D ( 'NONE', #99622, #90933, #11160 ) ;
#72599 = DIRECTION ( 'NONE',  ( -1.451651444332056451E-15, -1.000000000000000000, 0.000000000000000000 ) ) ;
#72601 = LINE ( 'NONE', #118894, #32537 ) ;
#72602 = CARTESIAN_POINT ( 'NONE',  ( -17.51078643762690845, -27.52281430457043143, 5.000000000000000000 ) ) ;
#72603 = EDGE_LOOP ( 'NONE', ( #88433, #107694, #49151, #73388 ) ) ;
#72604 = LINE ( 'NONE', #81308, #78397 ) ;
#72605 = DIRECTION ( 'NONE',  ( 0.7071067811865487940, 0.7071067811865463515, 0.000000000000000000 ) ) ;
#72606 = DIRECTION ( 'NONE',  ( -0.000000000000000000, -0.3543493200069152693, 0.9351131265310292928 ) ) ;
#72607 = ORIENTED_EDGE ( 'NONE', *, *, #3823, .F. ) ;
#72608 = DIRECTION ( 'NONE',  ( 0.7071067811865487940, 0.7071067811865463515, 0.000000000000000000 ) ) ;
#72609 = VECTOR ( 'NONE', #14220, 1000.000000000000000 ) ;
#72610 = LINE ( 'NONE', #129066, #42500 ) ;
#72611 = ORIENTED_EDGE ( 'NONE', *, *, #30142, .F. ) ;
#72613 = EDGE_LOOP ( 'NONE', ( #91496, #91970, #137815, #24477, #37439, #15542, #140428, #82744, #98829, #103726, #28938, #127828, #50703, #93394, #98748, #5768, #61138, #84119, #140034, #66672, #38794, #90584, #55638, #35642, #40840, #138011, #62668, #66079, #122174, #67619, #39570, #3976, #108341, #51077, #123764, #24008, #4296, #119714, #62885, #73417, #112170, #131466, #116999, #133301, #48987, #17656, #9735, #141501, #130854, #55042, #35781, #138112, #68261, #36232, #105890, #111404, #17663, #28969, #87096, #126259, #60113, #65701, #97276, #99669, #135307, #61760, #98723, #32485, #125865, #10335, #73605, #14398, #89827, #2091, #4866, #26914, #113579, #69512, #23015, #416, #89885, #1822, #53502, #87293, #28324, #24643, #56774, #124929, #98028, #36571, #103474, #102720, #133655, #89512, #127207, #24818, #97887, #125590, #29015, #35296, #104974, #126291, #27011, #50724, #45002, #55591, #140775, #142223, #105419, #76189, #68088, #35348, #86690, #123897, #108361, #26030, #37848, #30570, #119794, #138719, #51128, #31885, #136961, #104488, #69550, #11359, #31127, #83323, #134824, #55006, #27541, #29510, #130106, #11255, #85691, #83735, #54441, #131327, #42896, #2156, #126615, #48754, #96741, #35289, #97741, #22131, #127267, #47202, #94254, #100898, #58419, #79913, #89573, #59267, #6956, #72856, #84453, #61869, #103686, #7922, #23032, #115075, #96851, #85805, #88317, #140978, #117616, #81461, #18864, #4329, #34317, #5285, #117414, #18689, #57515, #122582, #27635, #92808, #93676, #99171, #32948, #33694, #88994, #41338, #139964, #25229, #95393, #87519, #138078, #1962, #140573, #66159, #57542, #14856, #104242, #95823, #109271, #1728, #142419, #134601, #26804, #128622, #115115, #63872, #59758, #32622, #96520, #41703, #92854, #91468, #119320, #68116, #7877, #91057, #53415, #59145, #70796, #28692, #80207, #1444, #81809, #30813, #117079, #99459, #108626, #19321, #110284, #118419, #8421, #42887, #136350, #134727, #36423, #120539, #137984, #117209, #65111, #88959, #23328, #50036, #79024, #23953, #5529, #90154, #5967, #125003, #65013, #57478, #64648, #38467, #61332, #118544, #12823, #98607, #98470, #65373, #84997, #17668, #71011, #136462, #30620, #53956, #132110, #62328, #82735, #36129, #78243, #41672, #52964, #103952, #20423, #97337, #123310, #67922, #128926, #65754, #87227, #54267, #109205, #13609, #122968, #105290, #84152, #131039, #79682, #127699, #139483, #106014, #7926, #30128, #36188, #105454, #138915, #91492, #93911, #71536, #1759, #75012, #116448, #40392, #73681, #104391, #3815, #48035, #110925, #7528, #141697, #72485, #135755, #60557, #121295, #139851, #1495, #115606, #57490, #92563, #16951, #76126, #48131, #124924, #129486, #120432, #78308, #6443, #92175, #138631, #80219, #44681, #78619, #2160, #107833, #135737, #104603, #130488, #87718, #141382, #92865, #93043, #106192, #11029, #119387, #134811, #77984, #104446, #63776, #32399, #5578, #46368, #132530, #69743, #47074, #92846, #64423, #83207, #99563, #41378, #66666, #127345, #107372, #115136, #127556, #57856, #140334, #131316, #11792, #113127, #11505, #34338, #18, #92576, #36165, #65398, #27817, #43134, #77469, #13779, #104701, #120843, #65805, #115459, #15044, #47552, #142434, #87276, #48731, #77136, #7448, #110798, #33719, #55032, #16324, #62222, #45201, #66662, #55805, #78341, #134954, #74076, #73972, #72638, #96947, #75851, #63492, #80181, #31808, #78091, #7161, #64269, #83772, #139980, #86053, #140448, #8444, #70436, #80157, #7079, #96, #83701, #121802, #114026, #57381, #25156, #116398, #86587, #12635, #39136, #56929, #109887, #107538, #133923, #25355, #21560, #94145, #59693, #9979, #47680, #105985, #121687, #112949, #89092, #42305, #124561, #91407, #760, #24691, #114119, #75399, #17736, #140116, #21108, #44895, #46169, #110143, #54773, #37014, #138174, #20928, #11022, #133241, #45165, #89463, #39112, #97572, #28377, #27614, #125729, #33691, #93854, #74082, #93922, #127091, #84658, #114648, #19203, #100223, #6717, #82534, #117923, #1555, #91701, #23273, #36457, #47577, #130267, #56528, #104838, #34803, #51187, #92109, #141107, #990, #23605, #67547, #133534, #39781, #142316, #113820, #45588, #69414, #68746, #51060, #106573, #106000, #88937, #51320, #84256, #128548, #143043, #5571, #107277, #92772, #85518, #88386, #41767, #110835, #45904, #68237, #84238, #120427, #36975, #50184, #83788, #88019, #41241, #10665, #65633, #41329, #95149, #25264, #52452, #62864, #129634, #53336, #100310, #140614, #92876, #8406, #54326, #40765, #35199, #8324, #76482, #131982, #9886, #73246, #111381, #57139, #14475, #121630, #84635, #39789, #111215, #43667, #74421, #40772, #45969, #56371, #124180, #35218, #139897, #5923, #71886, #93525, #82689, #40541, #103074, #102883, #40596, #76161, #130485, #28620, #73796, #102981, #2115, #80694, #41837, #133627, #11661, #20357, #18240, #53472, #4044, #10592, #59898, #111421, #60132, #24241, #103030, #103079, #62545, #42730, #57940, #89179, #96563, #32521, #4370, #17087, #132044, #136640, #63436, #70272, #57023, #95442, #67341 ) ) ;
#72612 = DIRECTION ( 'NONE',  ( 0.7071067811865487940, -0.7071067811865463515, 0.000000000000000000 ) ) ;
#72614 = ORIENTED_EDGE ( 'NONE', *, *, #142907, .T. ) ;
#72615 = VECTOR ( 'NONE', #113434, 1000.000000000000000 ) ;
#72616 = DIRECTION ( 'NONE',  ( 0.7071067811865487940, 0.7071067811865463515, -0.000000000000000000 ) ) ;
#72617 = ORIENTED_EDGE ( 'NONE', *, *, #15752, .T. ) ;
#72618 = DIRECTION ( 'NONE',  ( 0.7071067811865487940, 0.7071067811865463515, 0.000000000000000000 ) ) ;
#72619 = CARTESIAN_POINT ( 'NONE',  ( -53.99451991528749062, 28.92564299267975869, 4.000000000000000000 ) ) ;
#72621 = VECTOR ( 'NONE', #4880, 1000.000000000000000 ) ;
#72620 = DIRECTION ( 'NONE',  ( -1.000000000000000000, -1.224606353822377258E-16, -0.000000000000000000 ) ) ;
#72622 = VERTEX_POINT ( 'NONE', #44040 ) ;
#72623 = PLANE ( 'NONE',  #36932 ) ;
#72624 = LINE ( 'NONE', #137122, #28045 ) ;
#72625 = EDGE_CURVE ( 'NONE', #102057, #78692, #22246, .T. ) ;
#72626 = CARTESIAN_POINT ( 'NONE',  ( -0.7928932188134502068, -20.24070752338407431, 5.000000000000000000 ) ) ;
#72627 = CARTESIAN_POINT ( 'NONE',  ( -42.18398860626899705, 28.73617430169816700, 5.000000000000000000 ) ) ;
#72628 = FACE_OUTER_BOUND ( 'NONE', #18803, .T. ) ;
#72629 = CARTESIAN_POINT ( 'NONE',  ( 32.99999999999977973, 8.966399257802176948, 5.000000000000000000 ) ) ;
#72630 = CARTESIAN_POINT ( 'NONE',  ( 26.88558207307487891, 6.350000000000002309, 1.302735879833260446 ) ) ;
#72631 = CARTESIAN_POINT ( 'NONE',  ( -1.828169399223505964, 3.759292476615685441, 4.000000000000000000 ) ) ;
#72632 = DIRECTION ( 'NONE',  ( -0.6830127018922180770, -0.6830127018922204085, -0.2588190451025213501 ) ) ;
#72633 = EDGE_LOOP ( 'NONE', ( #14556, #138661, #135169, #98459 ) ) ;
#72634 = VECTOR ( 'NONE', #15243, 1000.000000000000000 ) ;
#72635 = ORIENTED_EDGE ( 'NONE', *, *, #117257, .F. ) ;
#72636 = ORIENTED_EDGE ( 'NONE', *, *, #115097, .F. ) ;
#72637 = CARTESIAN_POINT ( 'NONE',  ( 112.4166666666666714, -6.884901960086287076, -3.975000000000000977 ) ) ;
#72638 = ORIENTED_EDGE ( 'NONE', *, *, #20245, .F. ) ;
#72639 = ORIENTED_EDGE ( 'NONE', *, *, #7742, .F. ) ;
#72640 = VERTEX_POINT ( 'NONE', #57080 ) ;
#72641 =( NAMED_UNIT ( * ) PLANE_ANGLE_UNIT ( ) SI_UNIT ( $, .RADIAN. ) );
#72642 = DIRECTION ( 'NONE',  ( -0.7071067811865486830, 0.7071067811865463515, 0.000000000000000000 ) ) ;
#72643 = DIRECTION ( 'NONE',  ( -0.7071067811865486830, 0.7071067811865464625, 0.000000000000000000 ) ) ;
#72644 = ORIENTED_EDGE ( 'NONE', *, *, #18793, .F. ) ;
#72645 = DIRECTION ( 'NONE',  ( -0.7071067811865487940, 0.7071067811865463515, -0.000000000000000000 ) ) ;
#72646 = LINE ( 'NONE', #140690, #90344 ) ;
#72647 = DIRECTION ( 'NONE',  ( -0.7071067811865487940, 0.7071067811865463515, 0.000000000000000000 ) ) ;
#72648 = CARTESIAN_POINT ( 'NONE',  ( -18.48921356237309510, -27.52281430457068367, 5.000000000000000000 ) ) ;
#72649 = CARTESIAN_POINT ( 'NONE',  ( 101.7920968585647756, -5.291415217122921177, 3.054999999999999272 ) ) ;
#72650 = EDGE_CURVE ( 'NONE', #5966, #11091, #12100, .T. ) ;
#72651 = ORIENTED_EDGE ( 'NONE', *, *, #10204, .T. ) ;
#72653 = CARTESIAN_POINT ( 'NONE',  ( -9.900005234295676360, 9.518575983135214358, -29.22208412987195914 ) ) ;
#72652 = APPLICATION_CONTEXT ( 'automotive_design' ) ;
#72654 = CARTESIAN_POINT ( 'NONE',  ( -19.05499999999999261, 3.130000000000007887, 0.000000000000000000 ) ) ;
#72655 = EDGE_CURVE ( 'NONE', #14518, #63299, #133899, .T. ) ;
#72656 = CARTESIAN_POINT ( 'NONE',  ( -23.99451991528749062, 28.92564299267954908, 4.000000000000000000 ) ) ;
#72657 = LINE ( 'NONE', #40011, #9659 ) ;
#72659 = EDGE_CURVE ( 'NONE', #51451, #71767, #88262, .T. ) ;
#72658 = VECTOR ( 'NONE', #142918, 1000.000000000000227 ) ;
#72660 = DIRECTION ( 'NONE',  ( 0.6830127018922180770, -0.6830127018922204085, -0.2588190451025213501 ) ) ;
#72661 = EDGE_CURVE ( 'NONE', #39230, #129328, #54233, .T. ) ;
#72662 = CARTESIAN_POINT ( 'NONE',  ( 42.07919371712954870, 3.975000000000002753, -6.884901960086283523 ) ) ;
#72663 = CARTESIAN_POINT ( 'NONE',  ( 107.7500000000000000, -9.735942053221458872E-16, 7.950000000000000178 ) ) ;
#72665 = DIRECTION ( 'NONE',  ( -0.7071067811865486830, -0.7071067811865464625, 0.000000000000000000 ) ) ;
#72664 = VECTOR ( 'NONE', #2850, 1000.000000000000000 ) ;
#72666 = ORIENTED_EDGE ( 'NONE', *, *, #49930, .T. ) ;
#72667 = ORIENTED_EDGE ( 'NONE', *, *, #61545, .F. ) ;
#72668 = CARTESIAN_POINT ( 'NONE',  ( 127.3129301918980900, -1.637169565754159617, -6.110000000000001208 ) ) ;
#72669 = VERTEX_POINT ( 'NONE', #55634 ) ;
#72670 = ADVANCED_FACE ( 'NONE', ( #45494 ), #132512, .F. ) ;
#72671 = CARTESIAN_POINT ( 'NONE',  ( -34.92500000000001137, -22.22500000000000142, 4.000000000000000000 ) ) ;
#72672 = CARTESIAN_POINT ( 'NONE',  ( 69.48921356237309510, -27.52281430457103895, 5.000000000000000000 ) ) ;
#72673 = CARTESIAN_POINT ( 'NONE',  ( -1.171830600776451625, 12.75929247661558996, 4.000000000000000000 ) ) ;
#72674 = VECTOR ( 'NONE', #32801, 1000.000000000000000 ) ;
#72675 = LINE ( 'NONE', #117521, #7477 ) ;
#72676 = EDGE_CURVE ( 'NONE', #121862, #121313, #33197, .T. ) ;
#72677 = SURFACE_STYLE_USAGE ( .BOTH. , #50168 ) ;
#72678 = CARTESIAN_POINT ( 'NONE',  ( 22.17183060077631751, -20.24070752338407431, 4.000000000000000000 ) ) ;
#72679 = CARTESIAN_POINT ( 'NONE',  ( 128.6829301918981230, -1.637169565754158951, -6.109999999999998543 ) ) ;
#72680 = VECTOR ( 'NONE', #60271, 1000.000000000000000 ) ;
#72681 = ORIENTED_EDGE ( 'NONE', *, *, #83785, .T. ) ;
#72682 = DIRECTION ( 'NONE',  ( -0.7071067811865487940, 0.7071067811865463515, 0.000000000000000000 ) ) ;
#72683 = ORIENTED_EDGE ( 'NONE', *, *, #114850, .T. ) ;
#72684 = DIRECTION ( 'NONE',  ( -0.6830127018922181881, 0.6830127018922202975, -0.2588190451025214056 ) ) ;
#72685 = ADVANCED_FACE ( 'NONE', ( #34590 ), #65830, .F. ) ;
#72686 = PLANE ( 'NONE',  #49989 ) ;
#72687 = VECTOR ( 'NONE', #63061, 1000.000000000000000 ) ;
#72688 = DIRECTION ( 'NONE',  ( 1.000000000000000000, 0.000000000000000000, 0.000000000000000000 ) ) ;
#72689 = ORIENTED_EDGE ( 'NONE', *, *, #66779, .F. ) ;
#72690 = CARTESIAN_POINT ( 'NONE',  ( 57.75043019189809712, 3.055000000000002824, -5.291415217122919401 ) ) ;
#72691 = EDGE_LOOP ( 'NONE', ( #2858, #51841, #104076, #8041, #61747, #29700 ) ) ;
#72692 = DIRECTION ( 'NONE',  ( 0.000000000000000000, 0.000000000000000000, 1.000000000000000000 ) ) ;
#72693 = DIRECTION ( 'NONE',  ( 0.6830127018922181881, 0.6830127018922202975, -0.2588190451025214056 ) ) ;
#72694 = CARTESIAN_POINT ( 'NONE',  ( -25.82816939922335209, -2.240707523384255939, 4.000000000000000000 ) ) ;
#72695 = EDGE_CURVE ( 'NONE', #112409, #63022, #43327, .T. ) ;
#72696 = CARTESIAN_POINT ( 'NONE',  ( -26.67183060077628198, 20.25929247661550647, 4.000000000000000000 ) ) ;
#72697 =( BOUNDED_CURVE ( )  B_SPLINE_CURVE ( 3, ( #54609, #120522, #137508, #129466 ),
 .UNSPECIFIED., .F., .T. ) 
 B_SPLINE_CURVE_WITH_KNOTS ( ( 4, 4 ),
 ( 2.099584536334365925, 2.152415457235772323 ),
 .UNSPECIFIED. ) 
 CURVE ( )  GEOMETRIC_REPRESENTATION_ITEM ( )  RATIONAL_B_SPLINE_CURVE ( ( 1.000000000000000000, 0.9997674213408587196, 0.9997674213408587196, 1.000000000000000000 ) ) 
 REPRESENTATION_ITEM ( '' )  );
#72698 = AXIS2_PLACEMENT_3D ( 'NONE', #115077, #15749, #78957 ) ;
#72699 = VECTOR ( 'NONE', #66649, 999.9999999999998863 ) ;
#72700 = CARTESIAN_POINT ( 'NONE',  ( 51.39126352523145158, -4.472830434245839371, -4.472830434245839371 ) ) ;
#72701 = VERTEX_POINT ( 'NONE', #110675 ) ;
#72702 = LINE ( 'NONE', #82132, #51182 ) ;
#72703 = EDGE_CURVE ( 'NONE', #33545, #138262, #11357, .T. ) ;
#72704 = LINE ( 'NONE', #108092, #59507 ) ;
#72705 = VERTEX_POINT ( 'NONE', #131046 ) ;
#72706 = ORIENTED_EDGE ( 'NONE', *, *, #56068, .T. ) ;
#72707 = VECTOR ( 'NONE', #41022, 1000.000000000000000 ) ;
#72708 = DIRECTION ( 'NONE',  ( -0.000000000000000000, -1.000000000000000000, -0.000000000000000000 ) ) ;
#72709 = ORIENTED_EDGE ( 'NONE', *, *, #74468, .F. ) ;
#72710 = EDGE_CURVE ( 'NONE', #22968, #103695, #501, .T. ) ;
#72711 = EDGE_CURVE ( 'NONE', #94963, #136607, #120861, .T. ) ;
#72712 = CARTESIAN_POINT ( 'NONE',  ( 61.03752705046289151, -9.735942053221456900E-16, 7.949999999999998401 ) ) ;
#72713 = ORIENTED_EDGE ( 'NONE', *, *, #114830, .T. ) ;
#72714 = CARTESIAN_POINT ( 'NONE',  ( 17.82446237275610201, 9.017796866808286183, 4.672399651904014739 ) ) ;
#72715 = DIRECTION ( 'NONE',  ( -0.3543493200069162685, -0.000000000000000000, -0.9351131265310288487 ) ) ;
#72716 = CONICAL_SURFACE ( 'NONE', #10143, 2.055000000000001048, 0.9599310885968758145 ) ;
#72717 = EDGE_CURVE ( 'NONE', #47692, #26872, #75948, .T. ) ;
#72718 = CARTESIAN_POINT ( 'NONE',  ( -47.99451991528749062, 28.92564299267971251, 4.000000000000000000 ) ) ;
#72719 = FACE_BOUND ( 'NONE', #59221, .T. ) ;
#72720 = ADVANCED_FACE ( 'NONE', ( #32450 ), #76690, .T. ) ;
#72721 = FACE_OUTER_BOUND ( 'NONE', #54938, .T. ) ;
#72722 = CARTESIAN_POINT ( 'NONE',  ( 0.000000000000000000, 0.000000000000000000, 5.000000000000000000 ) ) ;
#72723 = CARTESIAN_POINT ( 'NONE',  ( 9.489213562373095101, -27.52281430457062328, 5.000000000000000000 ) ) ;
#72724 = EDGE_CURVE ( 'NONE', #96482, #59299, #70951, .T. ) ;
#72725 = VERTEX_POINT ( 'NONE', #22950 ) ;
#72726 = CARTESIAN_POINT ( 'NONE',  ( 128.5894344200537773, -57.14999999999999147, -39.86617647058817226 ) ) ;
#72728 = VERTEX_POINT ( 'NONE', #15636 ) ;
#72727 = CARTESIAN_POINT ( 'NONE',  ( 72.18398860626899705, 28.73617430169837661, 5.000000000000000000 ) ) ;
#72729 = VERTEX_POINT ( 'NONE', #3356 ) ;
#72730 = LINE ( 'NONE', #84294, #79592 ) ;
#72731 = ORIENTED_EDGE ( 'NONE', *, *, #68310, .F. ) ;
#72732 = CARTESIAN_POINT ( 'NONE',  ( 55.62043019189812298, 3.055000000000001936, -5.291415217122916737 ) ) ;
#72734 = VERTEX_POINT ( 'NONE', #37456 ) ;
#72733 = VECTOR ( 'NONE', #111571, 1000.000000000000000 ) ;
#72735 = EDGE_CURVE ( 'NONE', #34241, #43058, #4749, .T. ) ;
#72736 = PLANE ( 'NONE',  #76594 ) ;
#72737 = CARTESIAN_POINT ( 'NONE',  ( -25.82816939922335209, 0.7592924766157138627, 4.000000000000000000 ) ) ;
#72738 = ORIENTED_EDGE ( 'NONE', *, *, #84570, .F. ) ;
#72739 = LINE ( 'NONE', #95851, #120844 ) ;
#72740 = EDGE_CURVE ( 'NONE', #33461, #31488, #101981, .T. ) ;
#72741 = VECTOR ( 'NONE', #116527, 1000.000000000000000 ) ;
#72742 = DIRECTION ( 'NONE',  ( 0.7071067811865487940, -0.7071067811865463515, 0.000000000000000000 ) ) ;
#72743 = LINE ( 'NONE', #6658, #117670 ) ;
#72744 = DIRECTION ( 'NONE',  ( 0.7071067811865486830, -0.7071067811865464625, -0.000000000000000000 ) ) ;
#72745 = CARTESIAN_POINT ( 'NONE',  ( -56.99451991528749062, 28.92564299267978001, 4.000000000000000000 ) ) ;
#72746 = FACE_OUTER_BOUND ( 'NONE', #43727, .T. ) ;
#72747 = ORIENTED_EDGE ( 'NONE', *, *, #143188, .T. ) ;
#72748 = ORIENTED_EDGE ( 'NONE', *, *, #56255, .T. ) ;
#72749 = DIRECTION ( 'NONE',  ( -0.000000000000000000, 0.3543493200069153248, 0.9351131265310292928 ) ) ;
#72750 = LINE ( 'NONE', #5965, #106822 ) ;
#72751 = EDGE_LOOP ( 'NONE', ( #135553, #1513, #28199, #85607 ) ) ;
#72752 = ORIENTED_EDGE ( 'NONE', *, *, #20605, .F. ) ;
#72753 = ORIENTED_EDGE ( 'NONE', *, *, #119876, .T. ) ;
#72754 = CARTESIAN_POINT ( 'NONE',  ( 17.99999999999987210, -21.84840872380823029, 2.849755605029649974 ) ) ;
#72755 = DIRECTION ( 'NONE',  ( 0.6830127018922180770, -0.6830127018922204085, -0.2588190451025213501 ) ) ;
#72756 = ORIENTED_EDGE ( 'NONE', *, *, #70375, .T. ) ;
#72757 = CARTESIAN_POINT ( 'NONE',  ( -3.489213562373097322, -27.52281430457057709, 5.000000000000000000 ) ) ;
#72758 = VECTOR ( 'NONE', #96027, 1000.000000000000000 ) ;
#72759 = ADVANCED_FACE ( 'NONE', ( #16366 ), #80258, .F. ) ;
#72760 = DIRECTION ( 'NONE',  ( 0.000000000000000000, 0.000000000000000000, 1.000000000000000000 ) ) ;
#72761 = EDGE_CURVE ( 'NONE', #133481, #116655, #71508, .T. ) ;
#72762 = VECTOR ( 'NONE', #36742, 1000.000000000000000 ) ;
#72763 = CARTESIAN_POINT ( 'NONE',  ( 12.90040314143522160, -7.934999999999989839, 2.126176841940957907 ) ) ;
#72764 = DIRECTION ( 'NONE',  ( 1.000000000000000000, 0.000000000000000000, 0.000000000000000000 ) ) ;
#72765 = EDGE_LOOP ( 'NONE', ( #59282, #34049, #131221, #36822, #100739 ) ) ;
#72766 = DIRECTION ( 'NONE',  ( 0.7071067811865487940, -0.7071067811865463515, 0.000000000000000000 ) ) ;
#72767 = CARTESIAN_POINT ( 'NONE',  ( 26.99999999999980460, -10.06887692260771772, 4.000000000000000000 ) ) ;
#72768 = DIRECTION ( 'NONE',  ( 1.000000000000000000, 0.000000000000000000, 0.000000000000000000 ) ) ;
#72770 = ORIENTED_EDGE ( 'NONE', *, *, #108662, .F. ) ;
#72769 = PLANE ( 'NONE',  #33332 ) ;
#72771 = CARTESIAN_POINT ( 'NONE',  ( 9.962472949537104938, -7.464222240803106570E-16, -6.094999999999989981 ) ) ;
#72772 = VERTEX_POINT ( 'NONE', #48315 ) ;
#72773 = CARTESIAN_POINT ( 'NONE',  ( 44.99451991528749772, 28.92564299267969474, 4.000000000000000000 ) ) ;
#72774 = CARTESIAN_POINT ( 'NONE',  ( -31.49999999999977263, -14.70932175296478128, -11.46312253303829287 ) ) ;
#72775 = DIRECTION ( 'NONE',  ( 0.7071067811865487940, -0.7071067811865463515, 0.000000000000000000 ) ) ;
#72776 = VERTEX_POINT ( 'NONE', #46944 ) ;
#72777 = PLANE ( 'NONE',  #50320 ) ;
#72778 = VECTOR ( 'NONE', #128197, 1000.000000000000000 ) ;
#72779 = CARTESIAN_POINT ( 'NONE',  ( -32.99999999999976552, -4.068876922607779001, 4.000000000000000000 ) ) ;
#72780 = PLANE ( 'NONE',  #127547 ) ;
#72781 = PLANE ( 'NONE',  #106900 ) ;
#72782 = ORIENTED_EDGE ( 'NONE', *, *, #82850, .T. ) ;
#72783 = DIRECTION ( 'NONE',  ( 0.6830127018922181881, 0.6830127018922202975, -0.2588190451025214056 ) ) ;
#72784 = DIRECTION ( 'NONE',  ( 0.7071067811865486830, -0.7071067811865464625, -0.000000000000000000 ) ) ;
#72786 = VECTOR ( 'NONE', #141572, 1000.000000000000000 ) ;
#72785 = CARTESIAN_POINT ( 'NONE',  ( -27.18398860626900060, 28.73617430169806042, 5.000000000000000000 ) ) ;
#72787 = DIRECTION ( 'NONE',  ( -0.7071067811865486830, -0.7071067811865464625, 0.000000000000000000 ) ) ;
#72788 = DIRECTION ( 'NONE',  ( -1.000000000000000000, -1.224606353822377258E-16, -0.000000000000000000 ) ) ;
#72789 = AXIS2_PLACEMENT_3D ( 'NONE', #5819, #15265, #81299 ) ;
#72790 = ORIENTED_EDGE ( 'NONE', *, *, #136838, .T. ) ;
#72791 = ORIENTED_EDGE ( 'NONE', *, *, #30216, .F. ) ;
#72792 = CARTESIAN_POINT ( 'NONE',  ( 18.18398860626898994, 28.73617430169800002, 5.000000000000000000 ) ) ;
#72793 = VECTOR ( 'NONE', #136156, 1000.000000000000000 ) ;
#72794 = CARTESIAN_POINT ( 'NONE',  ( 2.312069808101886448, 7.934999999999993392, 2.126176841940951689 ) ) ;
#72795 = DIRECTION ( 'NONE',  ( -0.3543493200069162685, -0.000000000000000000, -0.9351131265310288487 ) ) ;
#72796 = VECTOR ( 'NONE', #22052, 1000.000000000000000 ) ;
#72797 = DIRECTION ( 'NONE',  ( -0.000000000000000000, 0.3543493200069153248, 0.9351131265310291818 ) ) ;
#72798 = CARTESIAN_POINT ( 'NONE',  ( -1.499999999999989120, 0.4311230773921797543, 4.000000000000000000 ) ) ;
#72799 = LINE ( 'NONE', #85744, #76860 ) ;
#72800 = ORIENTED_EDGE ( 'NONE', *, *, #19603, .T. ) ;
#72801 = DIRECTION ( 'NONE',  ( -0.7071067811865486830, 0.7071067811865464625, 0.000000000000000000 ) ) ;
#72802 = EDGE_CURVE ( 'NONE', #26788, #62844, #2647, .T. ) ;
#72803 = CARTESIAN_POINT ( 'NONE',  ( 34.49999999999975131, -5.945670655168991736, 4.994342998332164996 ) ) ;
#72804 = CARTESIAN_POINT ( 'NONE',  ( -1.499999999999992673, -15.29013452822854902, 0.3645803511610323233 ) ) ;
#72805 = CARTESIAN_POINT ( 'NONE',  ( 18.48921356237309510, -27.52281430457068367, 5.000000000000000000 ) ) ;
#72806 = CARTESIAN_POINT ( 'NONE',  ( 44.09959685856477307, -6.109999999999998543, -1.637169565754160727 ) ) ;
#72807 = CARTESIAN_POINT ( 'NONE',  ( -21.75860074219781382, 21.72500000000000142, 5.000000000000000000 ) ) ;
#72808 = VECTOR ( 'NONE', #33660, 1000.000000000000000 ) ;
#72810 = EDGE_CURVE ( 'NONE', #36267, #75381, #5500, .T. ) ;
#72809 = ORIENTED_EDGE ( 'NONE', *, *, #62846, .T. ) ;
#72811 = CARTESIAN_POINT ( 'NONE',  ( -29.99451991528749417, 28.92564299267958816, 4.000000000000000000 ) ) ;
#72812 = ORIENTED_EDGE ( 'NONE', *, *, #4991, .F. ) ;
#72813 = VERTEX_POINT ( 'NONE', #68664 ) ;
#72814 = VECTOR ( 'NONE', #8489, 1000.000000000000000 ) ;
#72815 = LINE ( 'NONE', #61228, #59362 ) ;
#72816 = CARTESIAN_POINT ( 'NONE',  ( -51.18398860626899705, 28.73617430169823095, 5.000000000000000000 ) ) ;
#72817 = LINE ( 'NONE', #116970, #219 ) ;
#72818 = EDGE_CURVE ( 'NONE', #83008, #116750, #4032, .T. ) ;
#72819 = PLANE ( 'NONE',  #2358 ) ;
#72820 = DIRECTION ( 'NONE',  ( 0.7071067811865486830, -0.7071067811865464625, -0.000000000000000000 ) ) ;
#72821 = CARTESIAN_POINT ( 'NONE',  ( 10.79166666666666785, -3.047499999999994547, 5.278424836066145431 ) ) ;
#72822 = ADVANCED_FACE ( 'NONE', ( #14254 ), #25113, .F. ) ;
#72823 = EDGE_CURVE ( 'NONE', #52532, #125922, #82390, .T. ) ;
#72824 = ORIENTED_EDGE ( 'NONE', *, *, #64101, .F. ) ;
#72825 = DIRECTION ( 'NONE',  ( 0.7071067811865486830, -0.7071067811865464625, -0.000000000000000000 ) ) ;
#72826 = PLANE ( 'NONE',  #81623 ) ;
#72827 = DIRECTION ( 'NONE',  ( -0.7071067811865486830, -0.7071067811865464625, -0.000000000000000000 ) ) ;
#72828 = PLANE ( 'NONE',  #14941 ) ;
#72829 = DIRECTION ( 'NONE',  ( -1.000000000000000000, -1.224606353822377258E-16, -0.000000000000000000 ) ) ;
#72830 = ADVANCED_FACE ( 'NONE', ( #13514 ), #70810, .T. ) ;
#72832 = EDGE_CURVE ( 'NONE', #109399, #18121, #114955, .T. ) ;
#72831 = CARTESIAN_POINT ( 'NONE',  ( 69.20419371712955581, -6.884901960086285300, -3.975000000000000089 ) ) ;
#72833 = PLANE ( 'NONE',  #85338 ) ;
#72834 = ORIENTED_EDGE ( 'NONE', *, *, #25432, .T. ) ;
#72835 = ORIENTED_EDGE ( 'NONE', *, *, #22362, .F. ) ;
#72836 = CARTESIAN_POINT ( 'NONE',  ( 66.62499999999998579, -7.950000000000000178, -4.867971026610729436E-16 ) ) ;
#72837 = LINE ( 'NONE', #6754, #95613 ) ;
#72838 = EDGE_CURVE ( 'NONE', #48106, #89121, #91807, .T. ) ;
#72839 = DIRECTION ( 'NONE',  ( 0.6830127018922180770, -0.6830127018922204085, -0.2588190451025213501 ) ) ;
#72840 = ORIENTED_EDGE ( 'NONE', *, *, #134515, .T. ) ;
#72841 = STYLED_ITEM ( 'NONE', ( #109578 ), #18383 ) ;
#72842 = CARTESIAN_POINT ( 'NONE',  ( 33.66666666666666430, 6.884901960086285300, 3.975000000000003642 ) ) ;
#72843 = EDGE_CURVE ( 'NONE', #110945, #97392, #60671, .T. ) ;
#72844 = LINE ( 'NONE', #116997, #104547 ) ;
#72845 = CARTESIAN_POINT ( 'NONE',  ( 58.18793019189811133, 6.110000000000002984, -1.637169565754156730 ) ) ;
#72846 = VERTEX_POINT ( 'NONE', #36715 ) ;
#72847 = LINE ( 'NONE', #8210, #29358 ) ;
#72848 = VERTEX_POINT ( 'NONE', #80958 ) ;
#72849 = ORIENTED_EDGE ( 'NONE', *, *, #48352, .T. ) ;
#72850 = FACE_OUTER_BOUND ( 'NONE', #129501, .T. ) ;
#72851 = DIRECTION ( 'NONE',  ( -0.000000000000000000, -1.000000000000000000, -0.000000000000000000 ) ) ;
#72852 = FACE_OUTER_BOUND ( 'NONE', #27633, .T. ) ;
#72853 = PLANE ( 'NONE',  #97214 ) ;
#72854 = CARTESIAN_POINT ( 'NONE',  ( 5.700255128608413102, -27.71228299555201957, 4.000000000000000000 ) ) ;
#72856 = ORIENTED_EDGE ( 'NONE', *, *, #30269, .F. ) ;
#72855 = CARTESIAN_POINT ( 'NONE',  ( 7.828169399223479985, 0.7592924766157104211, 4.000000000000000000 ) ) ;
#72857 = CARTESIAN_POINT ( 'NONE',  ( 27.04658813629527714, 14.25929247661557042, 18.84478104361321726 ) ) ;
#72858 = PLANE ( 'NONE',  #84832 ) ;
#72859 = DIRECTION ( 'NONE',  ( -0.7071067811865487940, 0.7071067811865463515, -0.000000000000000000 ) ) ;
#72861 = EDGE_CURVE ( 'NONE', #57345, #2265, #90387, .T. ) ;
#72860 = VECTOR ( 'NONE', #69880, 1000.000000000000000 ) ;
#72862 = DIRECTION ( 'NONE',  ( 0.7071067811865487940, 0.7071067811865463515, 0.000000000000000000 ) ) ;
#72863 = VERTEX_POINT ( 'NONE', #59236 ) ;
#72864 = VECTOR ( 'NONE', #140022, 1000.000000000000000 ) ;
#72865 = ORIENTED_EDGE ( 'NONE', *, *, #72034, .T. ) ;
#72866 = SURFACE_STYLE_FILL_AREA ( #116314 ) ;
#72867 = VECTOR ( 'NONE', #130009, 999.9999999999998863 ) ;
#72868 = DIRECTION ( 'NONE',  ( 0.6830127018922181881, 0.6830127018922202975, -0.2588190451025214056 ) ) ;
#72869 = DIRECTION ( 'NONE',  ( -1.000000000000000000, 0.000000000000000000, -0.000000000000000000 ) ) ;
#72870 = ADVANCED_FACE ( 'NONE', ( #134635 ), #35330, .F. ) ;
#72871 = DIRECTION ( 'NONE',  ( 0.6830127018922181881, 0.6830127018922202975, -0.2588190451025214056 ) ) ;
#72872 = CARTESIAN_POINT ( 'NONE',  ( 71.97502705046289861, -5.819803920172573086, 5.819803920172573086 ) ) ;
#72873 = EDGE_LOOP ( 'NONE', ( #7134, #18975, #34579, #68269 ) ) ;
#72874 = ORIENTED_EDGE ( 'NONE', *, *, #9550, .F. ) ;
#72875 = DIRECTION ( 'NONE',  ( -0.7071067811865486830, 0.7071067811865464625, 0.000000000000000000 ) ) ;
#72876 = ORIENTED_EDGE ( 'NONE', *, *, #12186, .F. ) ;
#72877 = EDGE_CURVE ( 'NONE', #56699, #92397, #62785, .T. ) ;
#72878 = EDGE_LOOP ( 'NONE', ( #134741, #76356, #126147, #92703 ) ) ;
#72879 = VECTOR ( 'NONE', #112841, 1000.000000000000000 ) ;
#72880 = CARTESIAN_POINT ( 'NONE',  ( 3.524001385854470314, 22.03583458319437582, 4.979811245910088502 ) ) ;
#72882 = EDGE_CURVE ( 'NONE', #64418, #119637, #127295, .T. ) ;
#72881 = VERTEX_POINT ( 'NONE', #52591 ) ;
#72883 = DIRECTION ( 'NONE',  ( -1.000000000000000000, -0.000000000000000000, -0.000000000000000000 ) ) ;
#72884 = CARTESIAN_POINT ( 'NONE',  ( -0.4892135623730947680, -27.52281430457055578, 5.000000000000000000 ) ) ;
#72885 = EDGE_CURVE ( 'NONE', #17540, #12905, #95384, .T. ) ;
#72886 = FACE_BOUND ( 'NONE', #59929, .T. ) ;
#72887 = DIRECTION ( 'NONE',  ( 0.000000000000000000, -1.000000000000000000, 0.000000000000000000 ) ) ;
#72888 = CARTESIAN_POINT ( 'NONE',  ( -18.48921356237309510, -27.52281430457068367, 5.000000000000000000 ) ) ;
#72890 = ORIENTED_EDGE ( 'NONE', *, *, #114260, .T. ) ;
#72889 = DIRECTION ( 'NONE',  ( 0.000000000000000000, 1.000000000000000000, 0.000000000000000000 ) ) ;
#72891 = VECTOR ( 'NONE', #41125, 1000.000000000000000 ) ;
#72892 = APPLICATION_PROTOCOL_DEFINITION ( 'draft international standard', 'automotive_design', 1998, #67989 ) ;
#72893 = VERTEX_POINT ( 'NONE', #63515 ) ;
#72894 = MECHANICAL_DESIGN_GEOMETRIC_PRESENTATION_REPRESENTATION (  '', ( #137743 ), #75241 ) ;
#72896 = ORIENTED_EDGE ( 'NONE', *, *, #27883, .F. ) ;
#72895 = AXIS2_PLACEMENT_3D ( 'NONE', #44223, #132678, #33369 ) ;
#72897 = CARTESIAN_POINT ( 'NONE',  ( 92.66209685856479439, -5.291415217122919401, 3.054999999999997939 ) ) ;
#72898 = ORIENTED_EDGE ( 'NONE', *, *, #8206, .T. ) ;
#72899 = COLOUR_RGB ( '', 0.40784314, 0.44705882, 0.49803922) ;
#72900 = EDGE_CURVE ( 'NONE', #49384, #10452, #75099, .T. ) ;
#72901 = DIRECTION ( 'NONE',  ( 0.000000000000000000, 0.000000000000000000, 1.000000000000000000 ) ) ;
#72902 = CYLINDRICAL_SURFACE ( 'NONE', #62937, 2.500000000000000000 ) ;
#72903 = CARTESIAN_POINT ( 'NONE',  ( -57.18398860626899705, 28.73617430169827358, 5.000000000000000000 ) ) ;
#72904 = VECTOR ( 'NONE', #27196, 1000.000000000000000 ) ;
#72905 = CARTESIAN_POINT ( 'NONE',  ( 19.17183060077633883, 21.75929247661549937, 4.000000000000000000 ) ) ;
#72906 = VERTEX_POINT ( 'NONE', #106968 ) ;
#72907 = DIRECTION ( 'NONE',  ( 0.7071067811865486830, -0.7071067811865464625, -0.000000000000000000 ) ) ;
#72908 = EDGE_CURVE ( 'NONE', #138159, #34174, #141022, .T. ) ;
#72909 = DIRECTION ( 'NONE',  ( -0.3543493200069162685, -0.000000000000000000, -0.9351131265310288487 ) ) ;
#72910 = DIRECTION ( 'NONE',  ( -0.6830127018922180770, -0.6830127018922204085, -0.2588190451025213501 ) ) ;
#72911 = CARTESIAN_POINT ( 'NONE',  ( 31.49999999999977973, 1.466399257802244893, 5.000000000000000000 ) ) ;
#72912 = PLANE ( 'NONE',  #109356 ) ;
#72913 = ORIENTED_EDGE ( 'NONE', *, *, #121267, .F. ) ;
#72914 = DIRECTION ( 'NONE',  ( 0.3543493200069162685, -0.000000000000000000, -0.9351131265310288487 ) ) ;
#72915 = LINE ( 'NONE', #9728, #141511 ) ;
#72916 = ORIENTED_EDGE ( 'NONE', *, *, #10173, .T. ) ;
#72917 = EDGE_CURVE ( 'NONE', #72171, #13889, #129434, .T. ) ;
#72918 = VERTEX_POINT ( 'NONE', #84538 ) ;
#72919 = VERTEX_POINT ( 'NONE', #19955 ) ;
#72920 = CARTESIAN_POINT ( 'NONE',  ( 45.20876352523143993, -7.482591942790329030E-16, 6.110000000000001208 ) ) ;
#72921 = ORIENTED_EDGE ( 'NONE', *, *, #25216, .F. ) ;
#72922 = EDGE_CURVE ( 'NONE', #135430, #21068, #50470, .T. ) ;
#72923 = CARTESIAN_POINT ( 'NONE',  ( 12.44163961620377101, -6.094999999999989093, 1.633150327867691765 ) ) ;
#72924 = ORIENTED_EDGE ( 'NONE', *, *, #117657, .T. ) ;
#72925 = ORIENTED_EDGE ( 'NONE', *, *, #60544, .F. ) ;
#72926 = CARTESIAN_POINT ( 'NONE',  ( 14.20710678118645021, -20.24070752338407786, 5.000000000000000000 ) ) ;
#72927 = CARTESIAN_POINT ( 'NONE',  ( -4.828169399223501301, 3.759292476615676559, 4.000000000000000000 ) ) ;
#72929 = ORIENTED_EDGE ( 'NONE', *, *, #142409, .T. ) ;
#72928 = DIRECTION ( 'NONE',  ( 0.000000000000000000, -1.000000000000000000, 0.000000000000000000 ) ) ;
#72930 = EDGE_LOOP ( 'NONE', ( #123411, #69797, #75450, #30884, #90105, #73072 ) ) ;
#72932 = EDGE_CURVE ( 'NONE', #112055, #24260, #41010, .T. ) ;
#72931 = AXIS2_PLACEMENT_3D ( 'NONE', #46341, #91934, #57211 ) ;
#72933 = FACE_OUTER_BOUND ( 'NONE', #133599, .T. ) ;
#72934 = CARTESIAN_POINT ( 'NONE',  ( 74.99451991528749772, 28.92564299267990435, 4.000000000000000000 ) ) ;
#72935 = ORIENTED_EDGE ( 'NONE', *, *, #25978, .F. ) ;
#72936 = EDGE_CURVE ( 'NONE', #43329, #2860, #18508, .T. ) ;
#72937 = PLANE ( 'NONE',  #20327 ) ;
#72938 = ORIENTED_EDGE ( 'NONE', *, *, #80818, .F. ) ;
#72939 = ORIENTED_EDGE ( 'NONE', *, *, #101437, .F. ) ;
#72940 = ORIENTED_EDGE ( 'NONE', *, *, #43658, .T. ) ;
#72941 = ORIENTED_EDGE ( 'NONE', *, *, #10382, .T. ) ;
#72942 = DIRECTION ( 'NONE',  ( -0.7071067811865486830, 0.7071067811865464625, 0.000000000000000000 ) ) ;
#72943 = LINE ( 'NONE', #130150, #65522 ) ;
#72944 = LINE ( 'NONE', #118534, #93424 ) ;
#72945 = DIRECTION ( 'NONE',  ( -0.000000000000000000, -0.3543493200069152693, 0.9351131265310292928 ) ) ;
#72946 = EDGE_CURVE ( 'NONE', #129515, #121901, #73644, .T. ) ;
#72947 = ORIENTED_EDGE ( 'NONE', *, *, #54584, .T. ) ;
#72948 = LINE ( 'NONE', #60645, #9394 ) ;
#72949 = ORIENTED_EDGE ( 'NONE', *, *, #19759, .T. ) ;
#72950 = CARTESIAN_POINT ( 'NONE',  ( -23.99999999999983302, 16.55218569542900298, 5.000000000000000000 ) ) ;
#72951 = AXIS2_PLACEMENT_3D ( 'NONE', #139129, #39834, #40529 ) ;
#72952 = CARTESIAN_POINT ( 'NONE',  ( 34.54123647476855297, 0.000000000000000000, 7.934999999999990727 ) ) ;
#72953 = DIRECTION ( 'NONE',  ( 1.000000000000000000, 0.000000000000000000, 0.000000000000000000 ) ) ;
#72954 = CARTESIAN_POINT ( 'NONE',  ( 18.00548008471250583, 28.92564299267925776, 4.000000000000000000 ) ) ;
#72955 = PLANE ( 'NONE',  #11923 ) ;
#72956 = ORIENTED_EDGE ( 'NONE', *, *, #131907, .F. ) ;
#72957 = VECTOR ( 'NONE', #139323, 1000.000000000000000 ) ;
#72958 = ORIENTED_EDGE ( 'NONE', *, *, #28515, .F. ) ;
#72959 = ORIENTED_EDGE ( 'NONE', *, *, #94726, .T. ) ;
#72960 = DIRECTION ( 'NONE',  ( 1.000000000000000000, 0.000000000000000000, 0.000000000000000000 ) ) ;
#72961 = CARTESIAN_POINT ( 'NONE',  ( 0.000000000000000000, 0.000000000000000000, 5.000000000000000000 ) ) ;
#72962 = CARTESIAN_POINT ( 'NONE',  ( 22.73493329717935652, 12.75929247661558996, 18.34774599283950991 ) ) ;
#72963 = FACE_OUTER_BOUND ( 'NONE', #99989, .T. ) ;
#72964 = CARTESIAN_POINT ( 'NONE',  ( -23.24139925780185223, 21.72500000000000853, 5.000000000000000000 ) ) ;
#72965 = CARTESIAN_POINT ( 'NONE',  ( 72.09959685856479439, -6.109999999999998543, -1.637169565754160727 ) ) ;
#72966 = DIRECTION ( 'NONE',  ( -0.7071067811865486830, -0.7071067811865464625, -0.000000000000000000 ) ) ;
#72967 = FACE_OUTER_BOUND ( 'NONE', #54745, .T. ) ;
#72968 = AXIS2_PLACEMENT_3D ( 'NONE', #26559, #80252, #136730 ) ;
#72969 = LINE ( 'NONE', #104830, #57152 ) ;
#72970 = CARTESIAN_POINT ( 'NONE',  ( 0.000000000000000000, 0.000000000000000000, 0.000000000000000000 ) ) ;
#72971 = DIRECTION ( 'NONE',  ( 0.3543493200069162685, -0.000000000000000000, -0.9351131265310288487 ) ) ;
#72972 = ORIENTED_EDGE ( 'NONE', *, *, #53003, .F. ) ;
#72973 = FACE_OUTER_BOUND ( 'NONE', #110120, .T. ) ;
#72974 = VERTEX_POINT ( 'NONE', #118558 ) ;
#72975 = DIRECTION ( 'NONE',  ( -0.7071067811865486830, -0.7071067811865464625, 0.000000000000000000 ) ) ;
#72977 = ORIENTED_EDGE ( 'NONE', *, *, #83646, .T. ) ;
#72976 = CARTESIAN_POINT ( 'NONE',  ( 26.20710678118636494, 0.7592924766157120864, 5.000000000000000000 ) ) ;
#72978 = FACE_OUTER_BOUND ( 'NONE', #44358, .T. ) ;
#72979 = PLANE ( 'NONE',  #56559 ) ;
#72980 = EDGE_CURVE ( 'NONE', #22872, #11920, #123116, .T. ) ;
#72981 = EDGE_LOOP ( 'NONE', ( #11501, #128860, #66474, #101073 ) ) ;
#72982 = ORIENTED_EDGE ( 'NONE', *, *, #3398, .T. ) ;
#72983 = CARTESIAN_POINT ( 'NONE',  ( 2.510786437626908008, -27.52281430457053446, 5.000000000000000000 ) ) ;
#72984 = CARTESIAN_POINT ( 'NONE',  ( 33.32816939922329880, -0.7407075233842753681, 4.000000000000000000 ) ) ;
#72985 = DIRECTION ( 'NONE',  ( -0.6830127018922181881, 0.6830127018922202975, -0.2588190451025214056 ) ) ;
#72986 = EDGE_CURVE ( 'NONE', #22682, #135194, #38872, .T. ) ;
#72988 = EDGE_CURVE ( 'NONE', #30838, #97296, #41726, .T. ) ;
#72987 = CARTESIAN_POINT ( 'NONE',  ( 94.28752705046289861, 0.000000000000000000, -7.949999999999998401 ) ) ;
#72990 = AXIS2_PLACEMENT_3D ( 'NONE', #74325, #143129, #109788 ) ;
#72989 = PLANE ( 'NONE',  #136549 ) ;
#72991 = VECTOR ( 'NONE', #128528, 1000.000000000000227 ) ;
#72992 = PLANE ( 'NONE',  #119992 ) ;
#72994 = EDGE_CURVE ( 'NONE', #25800, #103344, #49778, .T. ) ;
#72993 = ORIENTED_EDGE ( 'NONE', *, *, #89719, .T. ) ;
#72995 = AXIS2_PLACEMENT_3D ( 'NONE', #35610, #66775, #79837 ) ;
#72996 = CARTESIAN_POINT ( 'NONE',  ( 31.49999999999979039, 22.08746187583901843, 4.000000000000000000 ) ) ;
#72997 = EDGE_CURVE ( 'NONE', #48791, #131882, #83093, .T. ) ;
#72998 = CARTESIAN_POINT ( 'NONE',  ( -9.489213562373095101, -27.52281430457062328, 5.000000000000000000 ) ) ;
#72999 = CARTESIAN_POINT ( 'NONE',  ( 29.16666666666667140, -5.278424836066145431, -3.047499999999993658 ) ) ;
#73000 = FACE_OUTER_BOUND ( 'NONE', #15738, .T. ) ;
#73001 = EDGE_CURVE ( 'NONE', #47092, #89873, #105532, .T. ) ;
#73002 = VERTEX_POINT ( 'NONE', #96767 ) ;
#73003 = CARTESIAN_POINT ( 'NONE',  ( -11.99999999999991296, -16.06887692260766087, 4.000000000000000000 ) ) ;
#73005 = VERTEX_POINT ( 'NONE', #6904 ) ;
#73004 = ADVANCED_FACE ( 'NONE', ( #83839 ), #28728, .T. ) ;
#73006 = CARTESIAN_POINT ( 'NONE',  ( 85.31293019189811844, -1.637169565754159617, -6.110000000000001208 ) ) ;
#73007 = DIRECTION ( 'NONE',  ( -0.5735764363510499342, -0.8191520442889891340, 0.000000000000000000 ) ) ;
#73008 = LINE ( 'NONE', #62106, #65484 ) ;
#73009 = CARTESIAN_POINT ( 'NONE',  ( 21.70710678118639692, -9.740707523384179112, 5.000000000000000000 ) ) ;
#73010 = EDGE_LOOP ( 'NONE', ( #78393, #105678, #126279, #127886, #46675 ) ) ;
#73011 = CARTESIAN_POINT ( 'NONE',  ( -3.134995737516202308, 3.759292476615678336, 15.36553568819726934 ) ) ;
#73012 = EDGE_CURVE ( 'NONE', #108385, #33386, #32547, .T. ) ;
#73013 = LINE ( 'NONE', #117164, #65075 ) ;
#73014 = DIRECTION ( 'NONE',  ( 1.000000000000000000, 0.000000000000000000, 0.000000000000000000 ) ) ;
#73016 = ORIENTED_EDGE ( 'NONE', *, *, #44364, .T. ) ;
#73015 = DIRECTION ( 'NONE',  ( -0.7071067811865486830, 0.7071067811865464625, 0.000000000000000000 ) ) ;
#73017 = DIRECTION ( 'NONE',  ( 0.000000000000000000, 1.000000000000000000, 0.000000000000000000 ) ) ;
#73018 = LINE ( 'NONE', #62116, #124059 ) ;
#73019 = CARTESIAN_POINT ( 'NONE',  ( -19.49999999999986144, -5.568876922607759461, 4.000000000000000000 ) ) ;
#73020 = EDGE_CURVE ( 'NONE', #94372, #95699, #77246, .T. ) ;
#73021 = DIRECTION ( 'NONE',  ( -0.3543493200069162685, -0.000000000000000000, -0.9351131265310288487 ) ) ;
#73022 = ORIENTED_EDGE ( 'NONE', *, *, #27255, .F. ) ;
#73023 = EDGE_LOOP ( 'NONE', ( #87601, #6487, #57326, #104300 ) ) ;
#73024 = CARTESIAN_POINT ( 'NONE',  ( 74.08376352523143282, -6.110000000000001208, -3.741295971395164515E-16 ) ) ;
#73025 = ORIENTED_EDGE ( 'NONE', *, *, #31909, .T. ) ;
#73026 = CARTESIAN_POINT ( 'NONE',  ( 57.48921356237308800, -27.52281430457095368, 5.000000000000000000 ) ) ;
#73027 = CARTESIAN_POINT ( 'NONE',  ( 13.77149322861326652, 20.25929247661551358, 7.808871592221799496 ) ) ;
#73028 = CARTESIAN_POINT ( 'NONE',  ( -17.29289321881334018, 20.25929247661551003, 5.000000000000000000 ) ) ;
#73029 = EDGE_LOOP ( 'NONE', ( #6662, #8803, #118640, #92842 ) ) ;
#73030 = DIRECTION ( 'NONE',  ( -0.000000000000000000, -1.000000000000000000, -0.000000000000000000 ) ) ;
#73031 = LINE ( 'NONE', #117182, #118424 ) ;
#73032 = VERTEX_POINT ( 'NONE', #131595 ) ;
#73033 = CARTESIAN_POINT ( 'NONE',  ( 0.000000000000000000, 0.000000000000000000, 5.000000000000000000 ) ) ;
#73034 = EDGE_CURVE ( 'NONE', #82669, #58856, #78641, .T. ) ;
#73035 = DIRECTION ( 'NONE',  ( -0.6830127018922180770, -0.6830127018922204085, -0.2588190451025213501 ) ) ;
#73036 = DIRECTION ( 'NONE',  ( 0.000000000000000000, 0.000000000000000000, -1.000000000000000000 ) ) ;
#73037 = EDGE_CURVE ( 'NONE', #32044, #68720, #99656, .T. ) ;
#73038 = EDGE_LOOP ( 'NONE', ( #137660, #136815, #10720, #61690 ) ) ;
#73039 = EDGE_LOOP ( 'NONE', ( #57351, #26542, #88734, #28956, #102952 ) ) ;
#73040 = CARTESIAN_POINT ( 'NONE',  ( 38.34328999833763874, 3.759292476615685441, 13.27625715073274115 ) ) ;
#73041 = CARTESIAN_POINT ( 'NONE',  ( -39.48921356237310221, -27.52281430457082934, 5.000000000000000000 ) ) ;
#73042 = CARTESIAN_POINT ( 'NONE',  ( 5.816011393731002066, 28.73617430169783304, 5.000000000000000000 ) ) ;
#73043 = EDGE_CURVE ( 'NONE', #37329, #38295, #33029, .T. ) ;
#73044 = CARTESIAN_POINT ( 'NONE',  ( -21.48921356237309155, -27.52281430457070499, 5.000000000000000000 ) ) ;
#73045 =( NAMED_UNIT ( * ) SI_UNIT ( $, .STERADIAN. ) SOLID_ANGLE_UNIT ( ) );
#73047 = ORIENTED_EDGE ( 'NONE', *, *, #108895, .F. ) ;
#73046 = VECTOR ( 'NONE', #136615, 1000.000000000000000 ) ;
#73048 = ORIENTED_EDGE ( 'NONE', *, *, #79910, .F. ) ;
#73049 =( BOUNDED_CURVE ( )  B_SPLINE_CURVE ( 3, ( #479, #44773, #75235, #54211 ),
 .UNSPECIFIED., .F., .T. ) 
 B_SPLINE_CURVE_WITH_KNOTS ( ( 4, 4 ),
 ( 2.779374508378133601, 4.199602562396808736 ),
 .UNSPECIFIED. ) 
 CURVE ( )  GEOMETRIC_REPRESENTATION_ITEM ( )  RATIONAL_B_SPLINE_CURVE ( ( 1.000000000000000000, 0.8388583629366690442, 0.8388583629366690442, 1.000000000000000000 ) ) 
 REPRESENTATION_ITEM ( '' )  );
#73050 = VERTEX_POINT ( 'NONE', #32287 ) ;
#73051 = AXIS2_PLACEMENT_3D ( 'NONE', #70707, #14851, #117022 ) ;
#73052 = EDGE_CURVE ( 'NONE', #37692, #89916, #42472, .T. ) ;
#73053 = ORIENTED_EDGE ( 'NONE', *, *, #25702, .T. ) ;
#73054 = FACE_OUTER_BOUND ( 'NONE', #51012, .T. ) ;
#73055 = ORIENTED_EDGE ( 'NONE', *, *, #29446, .T. ) ;
#73056 = VECTOR ( 'NONE', #139095, 1000.000000000000000 ) ;
#73057 =( LENGTH_UNIT ( ) NAMED_UNIT ( * ) SI_UNIT ( .MILLI., .METRE. ) );
#73058 = PLANE ( 'NONE',  #105070 ) ;
#73059 = CARTESIAN_POINT ( 'NONE',  ( 34.92499999999998295, 22.22500000000000142, 4.500000000000000888 ) ) ;
#73060 = CARTESIAN_POINT ( 'NONE',  ( -29.01844734635652401, 18.75929247661553134, 20.33588619593449920 ) ) ;
#73061 = CARTESIAN_POINT ( 'NONE',  ( -1.499999999999989120, 1.466399257802246670, 5.000000000000000000 ) ) ;
#73062 = VERTEX_POINT ( 'NONE', #122853 ) ;
#73063 = DIRECTION ( 'NONE',  ( 0.3543493200069163240, -0.000000000000000000, 0.9351131265310288487 ) ) ;
#73064 = DIRECTION ( 'NONE',  ( 0.3543493200069162685, -0.000000000000000000, -0.9351131265310288487 ) ) ;
#73065 = ORIENTED_EDGE ( 'NONE', *, *, #107927, .T. ) ;
#73067 = EDGE_CURVE ( 'NONE', #141841, #65131, #121415, .T. ) ;
#73066 = LINE ( 'NONE', #139015, #96791 ) ;
#73068 = ORIENTED_EDGE ( 'NONE', *, *, #115112, .F. ) ;
#73069 = EDGE_CURVE ( 'NONE', #20671, #135734, #75794, .T. ) ;
#73070 = CARTESIAN_POINT ( 'NONE',  ( 13.31663961620377279, -1.633150327867691765, -6.094999999999989093 ) ) ;
#73071 = VERTEX_POINT ( 'NONE', #120688 ) ;
#73072 = ORIENTED_EDGE ( 'NONE', *, *, #82799, .F. ) ;
#73073 = CARTESIAN_POINT ( 'NONE',  ( 68.54209685856477563, 5.291415217122923842, -3.054999999999996163 ) ) ;
#73074 = VERTEX_POINT ( 'NONE', #9036 ) ;
#73075 = AXIS2_PLACEMENT_3D ( 'NONE', #14484, #124671, #24638 ) ;
#73076 = CONICAL_SURFACE ( 'NONE', #38282, 2.500000000000000444, 0.9599310885968830309 ) ;
#73077 = CARTESIAN_POINT ( 'NONE',  ( -32.29298673570672662, -21.74070752338405299, 4.999753212805210012 ) ) ;
#73078 = CARTESIAN_POINT ( 'NONE',  ( 110.9795968585647756, 6.109999999999999432, 1.637169565754164280 ) ) ;
#73079 = LINE ( 'NONE', #139761, #112017 ) ;
#73080 = VECTOR ( 'NONE', #84647, 1000.000000000000114 ) ;
#73081 = PLANE ( 'NONE',  #136648 ) ;
#73082 = DIRECTION ( 'NONE',  ( -0.6830127018922180770, -0.6830127018922204085, -0.2588190451025213501 ) ) ;
#73083 = EDGE_CURVE ( 'NONE', #136489, #133461, #11901, .T. ) ;
#73084 = CARTESIAN_POINT ( 'NONE',  ( 0.000000000000000000, -5.520864266206504263E-14, 0.000000000000000000 ) ) ;
#73085 = CARTESIAN_POINT ( 'NONE',  ( 0.000000000000000000, -14.29000000000013593, 12.69999999999954632 ) ) ;
#73086 = ORIENTED_EDGE ( 'NONE', *, *, #32196, .F. ) ;
#73087 = EDGE_CURVE ( 'NONE', #8692, #130004, #110520, .T. ) ;
#73088 = FACE_OUTER_BOUND ( 'NONE', #60747, .T. ) ;
#73089 = LINE ( 'NONE', #93381, #22019 ) ;
#73090 = VERTEX_POINT ( 'NONE', #11191 ) ;
#73091 = ORIENTED_EDGE ( 'NONE', *, *, #120707, .F. ) ;
#73092 = CARTESIAN_POINT ( 'NONE',  ( 78.18398860626899705, 28.73617430169841924, 5.000000000000000000 ) ) ;
#73093 = ORIENTED_EDGE ( 'NONE', *, *, #61221, .T. ) ;
#73094 = CARTESIAN_POINT ( 'NONE',  ( -63.48921356237309510, -27.52281430457099631, 5.000000000000000000 ) ) ;
#73095 = DIRECTION ( 'NONE',  ( -0.7071067811865486830, -0.7071067811865464625, 0.000000000000000000 ) ) ;
#73096 = DIRECTION ( 'NONE',  ( 0.7071067811865486830, -0.7071067811865464625, -0.000000000000000000 ) ) ;
#73097 = EDGE_CURVE ( 'NONE', #141006, #83058, #133741, .T. ) ;
#73098 = DIRECTION ( 'NONE',  ( 1.000000000000000000, 0.000000000000000000, 0.000000000000000000 ) ) ;
#73099 = ORIENTED_EDGE ( 'NONE', *, *, #57228, .T. ) ;
#73100 = PRESENTATION_STYLE_ASSIGNMENT (( #41879 ) ) ;
#73101 = ORIENTED_EDGE ( 'NONE', *, *, #123377, .F. ) ;
#73102 = CARTESIAN_POINT ( 'NONE',  ( 7.853736474768552966, -5.808823158059035485, -5.808823158059033709 ) ) ;
#73103 = CARTESIAN_POINT ( 'NONE',  ( -11.48334561358947070, 22.22500000000000142, 4.500000000000000888 ) ) ;
#73104 = FACE_OUTER_BOUND ( 'NONE', #41906, .T. ) ;
#73105 = CARTESIAN_POINT ( 'NONE',  ( 12.28062291172085274, -8.652526378290415821, 3.924136651621471295 ) ) ;
#73106 = VERTEX_POINT ( 'NONE', #1044 ) ;
#73107 = ORIENTED_EDGE ( 'NONE', *, *, #61428, .F. ) ;
#73108 = ORIENTED_EDGE ( 'NONE', *, *, #116243, .T. ) ;
#73109 = LINE ( 'NONE', #115831, #61227 ) ;
#73110 = PLANE ( 'NONE',  #39510 ) ;
#73111 = CARTESIAN_POINT ( 'NONE',  ( 0.000000000000000000, 0.000000000000000000, 5.000000000000000000 ) ) ;
#73112 = LINE ( 'NONE', #51348, #10205 ) ;
#73113 = CARTESIAN_POINT ( 'NONE',  ( -33.70710678118629744, -6.740707523384209310, 5.000000000000000000 ) ) ;
#73114 = FACE_OUTER_BOUND ( 'NONE', #26007, .T. ) ;
#73115 = LINE ( 'NONE', #110506, #97409 ) ;
#73116 = CARTESIAN_POINT ( 'NONE',  ( 12.82439460721831104, 4.202752102959690472E-16, 0.000000000000000000 ) ) ;
#73117 = CARTESIAN_POINT ( 'NONE',  ( 0.000000000000000000, 0.000000000000000000, 5.000000000000000000 ) ) ;
#73118 = CARTESIAN_POINT ( 'NONE',  ( 0.7933393645784738712, 21.75929247661549937, 4.998822639870705409 ) ) ;
#73120 = ORIENTED_EDGE ( 'NONE', *, *, #142151, .T. ) ;
#73119 = B_SPLINE_CURVE_WITH_KNOTS ( 'NONE', 3,
 ( #45926, #122014, #24155, #92240, #122744, #13961, #14704, #124182, #58264, #22681, #58981, #11821, #79299, #2362, #111883, #90113, #114014, #80004, #102453, #56105 ),
 .UNSPECIFIED., .F., .F.,
 ( 4, 2, 2, 2, 2, 2, 2, 2, 2, 4 ),
 ( 3.469446951953614189E-18, 0.002043365256125570517, 0.003065047884188353174, 0.004086730512251135830, 0.005108413140313918487, 0.006130095768376701143, 0.006640937082408094640, 0.007151778396439487269, 0.007662619710470881633, 0.008173461024502275130 ),
 .UNSPECIFIED. ) ;
#73121 = CARTESIAN_POINT ( 'NONE',  ( 73.77083333333332860, -7.949999999999998401, -2.130196079827426203 ) ) ;
#73122 = ADVANCED_FACE ( 'NONE', ( #97514 ), #55471, .F. ) ;
#73123 = CARTESIAN_POINT ( 'NONE',  ( 45.48921356237309510, -27.52281430457087197, 5.000000000000000000 ) ) ;
#73124 = ORIENTED_EDGE ( 'NONE', *, *, #80089, .T. ) ;
#73125 = DIRECTION ( 'NONE',  ( 0.3543493200069162685, -0.000000000000000000, -0.9351131265310288487 ) ) ;
#73127 = ORIENTED_EDGE ( 'NONE', *, *, #95009, .F. ) ;
#73126 = CARTESIAN_POINT ( 'NONE',  ( -25.49999999999982947, -15.29013452822856500, 0.3645803511609750913 ) ) ;
#73128 = DIRECTION ( 'NONE',  ( -1.000000000000000000, -1.224606353822377258E-16, -0.000000000000000000 ) ) ;
#73129 = DIRECTION ( 'NONE',  ( -0.000000000000000000, -0.3543493200069152693, 0.9351131265310292928 ) ) ;
#73130 = ORIENTED_EDGE ( 'NONE', *, *, #33517, .F. ) ;
#73131 = FACE_OUTER_BOUND ( 'NONE', #5511, .T. ) ;
#73132 = ORIENTED_EDGE ( 'NONE', *, *, #92748, .T. ) ;
#73133 = VECTOR ( 'NONE', #8566, 1000.000000000000000 ) ;
#73135 = EDGE_CURVE ( 'NONE', #56274, #42790, #88819, .T. ) ;
#73134 = CARTESIAN_POINT ( 'NONE',  ( 122.8708603837962272, 6.884901960086289741, -3.974999999999993427 ) ) ;
#73136 = DIRECTION ( 'NONE',  ( 0.7071067811865487940, -0.7071067811865463515, 0.000000000000000000 ) ) ;
#73137 = DIRECTION ( 'NONE',  ( 0.6830127018922180770, -0.6830127018922204085, -0.2588190451025213501 ) ) ;
#73138 = EDGE_CURVE ( 'NONE', #116824, #103756, #13988, .T. ) ;
#73139 = EDGE_CURVE ( 'NONE', #26770, #109240, #33732, .T. ) ;
#73140 = VECTOR ( 'NONE', #18774, 999.9999999999998863 ) ;
#73141 = PLANE ( 'NONE',  #106999 ) ;
#73142 = DIRECTION ( 'NONE',  ( -0.7071067811865486830, -0.7071067811865464625, 0.000000000000000000 ) ) ;
#73143 = EDGE_CURVE ( 'NONE', #131775, #62699, #98941, .T. ) ;
#73144 = DIRECTION ( 'NONE',  ( 0.000000000000000000, -1.000000000000000000, 0.000000000000000000 ) ) ;
#73145 = CARTESIAN_POINT ( 'NONE',  ( 25.64540314143522082, -2.126176841940958351, -7.934999999999989839 ) ) ;
#73146 = CARTESIAN_POINT ( 'NONE',  ( 5.957903141435219929, 6.871911579029515771, 3.967499999999989146 ) ) ;
#73147 = DIRECTION ( 'NONE',  ( -0.000000000000000000, -0.3543493200069152693, 0.9351131265310292928 ) ) ;
#73148 = CARTESIAN_POINT ( 'NONE',  ( -22.17183060077631396, -2.240707523384257716, 4.000000000000000000 ) ) ;
#73150 = EDGE_CURVE ( 'NONE', #13156, #19842, #94316, .T. ) ;
#73149 = DIRECTION ( 'NONE',  ( -1.000000000000000000, -0.000000000000000000, -0.000000000000000000 ) ) ;
#73151 = ORIENTED_EDGE ( 'NONE', *, *, #26899, .T. ) ;
#73152 = ORIENTED_EDGE ( 'NONE', *, *, #65780, .F. ) ;
#73153 = CARTESIAN_POINT ( 'NONE',  ( 82.95833333333332860, 3.974999999999997424, 6.884901960086288852 ) ) ;
#73154 = ORIENTED_EDGE ( 'NONE', *, *, #5812, .T. ) ;
#73155 = EDGE_CURVE ( 'NONE', #88478, #112059, #93620, .T. ) ;
#73156 = CARTESIAN_POINT ( 'NONE',  ( 92.10002705046288440, 5.819803920172570422, 5.819803920172575751 ) ) ;
#73157 = CARTESIAN_POINT ( 'NONE',  ( 8.999999999999944933, 17.96639925780208102, 5.000000000000000000 ) ) ;
#73158 = DIRECTION ( 'NONE',  ( -0.7071067811865487940, 0.7071067811865463515, 0.000000000000000000 ) ) ;
#73159 = VERTEX_POINT ( 'NONE', #90216 ) ;
#73160 = FACE_OUTER_BOUND ( 'NONE', #43268, .T. ) ;
#73161 = CARTESIAN_POINT ( 'NONE',  ( 24.70710678118637205, -9.740707523384187994, 5.000000000000000000 ) ) ;
#73162 = EDGE_CURVE ( 'NONE', #128274, #19220, #111995, .T. ) ;
#73163 = CARTESIAN_POINT ( 'NONE',  ( 11.81601139373100651, 28.73617430169779041, 5.000000000000000000 ) ) ;
#73164 = LINE ( 'NONE', #50671, #46660 ) ;
#73165 = EDGE_CURVE ( 'NONE', #111466, #118332, #24944, .T. ) ;
#73166 = DIRECTION ( 'NONE',  ( -0.000000000000000000, 0.000000000000000000, 1.000000000000000000 ) ) ;
#73167 = DIRECTION ( 'NONE',  ( -0.7071067811865486830, -0.7071067811865464625, -0.000000000000000000 ) ) ;
#73168 = DIRECTION ( 'NONE',  ( 0.7071067811865487940, 0.7071067811865463515, 0.000000000000000000 ) ) ;
#73169 = CARTESIAN_POINT ( 'NONE',  ( 10.49999999999992717, -20.53675388469229546, 2.352720554255917751 ) ) ;
#73170 = FACE_OUTER_BOUND ( 'NONE', #69426, .T. ) ;
#73171 = DIRECTION ( 'NONE',  ( 0.5735764363510448272, -0.8191520442889927978, 1.003171929053526103E-16 ) ) ;
#73172 = DIRECTION ( 'NONE',  ( -1.000000000000000000, 0.000000000000000000, 0.000000000000000000 ) ) ;
#73173 = EDGE_CURVE ( 'NONE', #33315, #23517, #82747, .T. ) ;
#73174 = VECTOR ( 'NONE', #12858, 1000.000000000000000 ) ;
#73175 = CARTESIAN_POINT ( 'NONE',  ( 53.41963127661843203, -48.51451318982864080, 38.21513923099880827 ) ) ;
#73176 = ORIENTED_EDGE ( 'NONE', *, *, #111786, .F. ) ;
#73177 = VERTEX_POINT ( 'NONE', #105194 ) ;
#73178 = AXIS2_PLACEMENT_3D ( 'NONE', #40888, #29990, #28594 ) ;
#73179 = CARTESIAN_POINT ( 'NONE',  ( 101.0629301918980900, 1.637169565754157174, 6.110000000000002984 ) ) ;
#73180 = ORIENTED_EDGE ( 'NONE', *, *, #6994, .T. ) ;
#73181 = CIRCLE ( 'NONE', #80122, 5.999999999999998224 ) ;
#73182 = VECTOR ( 'NONE', #121795, 999.9999999999998863 ) ;
#73183 = CARTESIAN_POINT ( 'NONE',  ( 8.604166666666669627, -1.633150327867691765, -6.094999999999989093 ) ) ;
